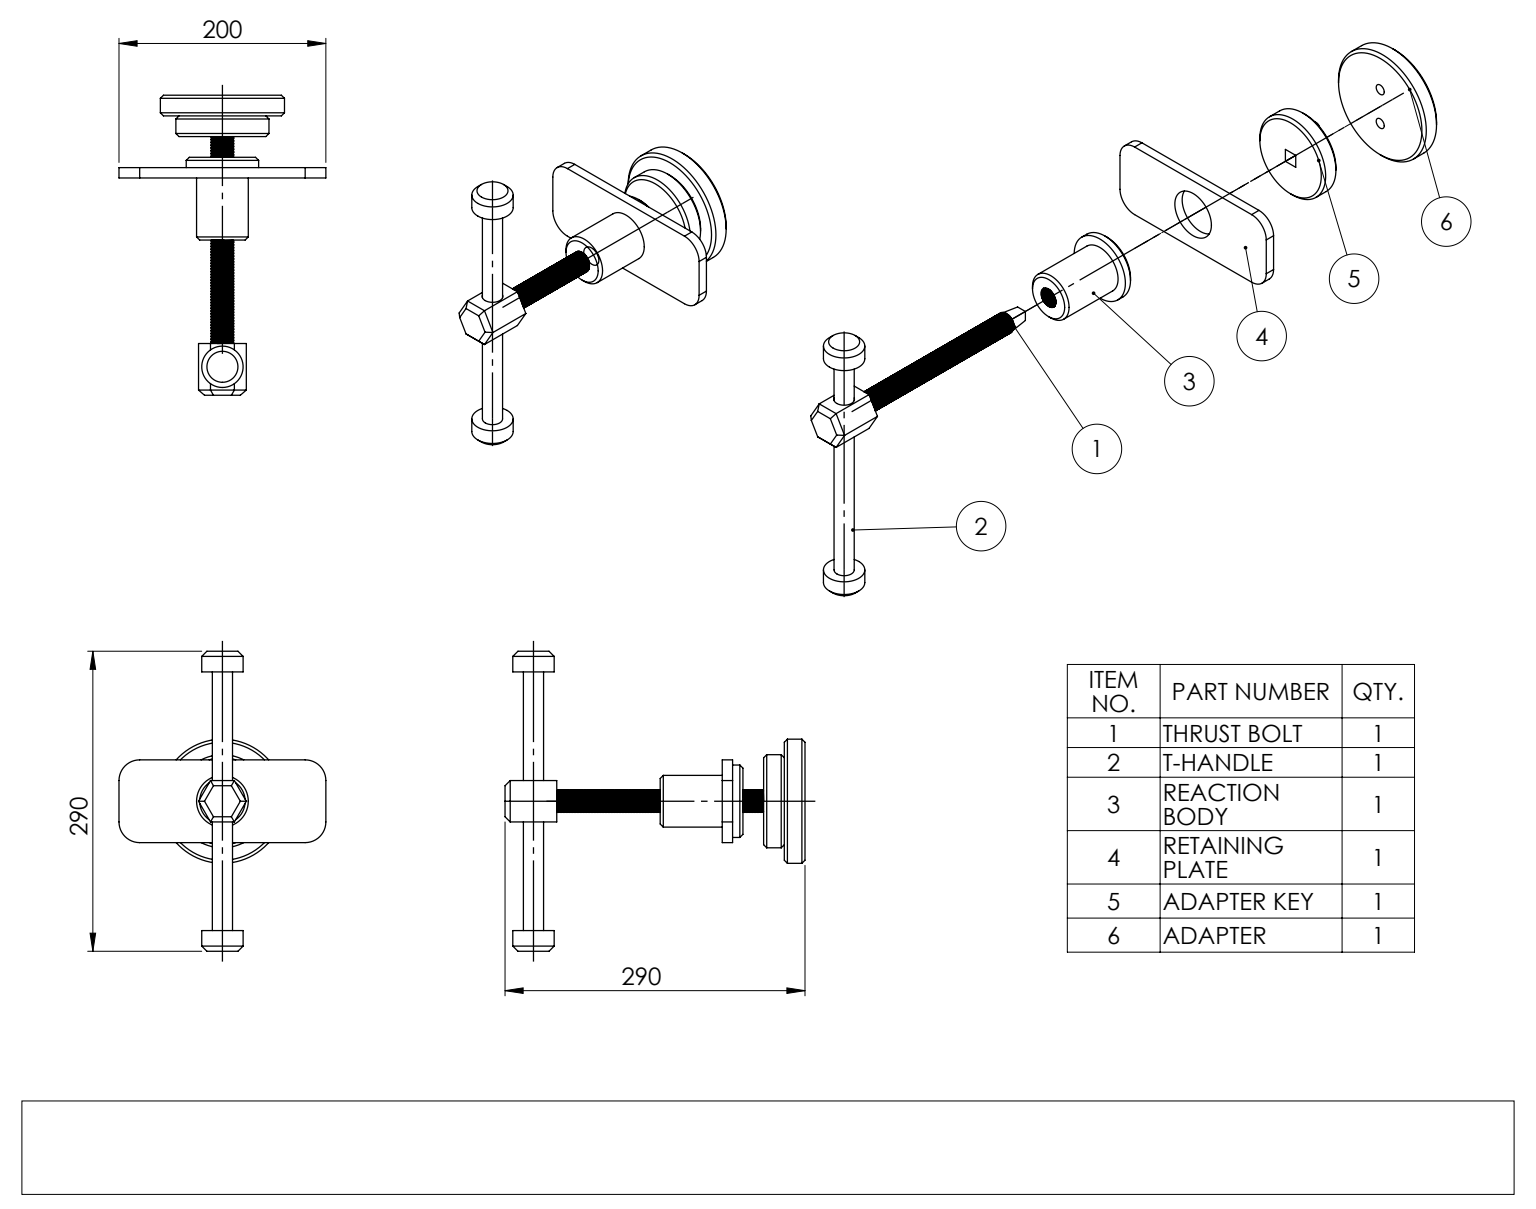
ISO-10303-21;
HEADER;
FILE_DESCRIPTION (('STEP AP203'),
    '1' );
FILE_NAME ('BR-597',
    '2026-09-28T05:57:06',
    ( '' ),
    ( '' ),
    'SwSTEP 2.0',
    'SolidWorks 2026',
    '' );
FILE_SCHEMA (( 'AUTOMOTIVE_DESIGN' ));
ENDSEC;

DATA;
#1 = ORIENTED_EDGE ( 'NONE', *, *, #11918, .T. ) ;
#2 = CARTESIAN_POINT ( 'NONE',  ( 10.81189881249999551, -6.242252689847874514, -42.15625000204836681 ) ) ;
#3 = CALENDAR_DATE ( 2026, 28, 9 ) ;
#4 = CARTESIAN_POINT ( 'NONE',  ( -10.81189881249999729, 1.324075727343319199E-15, -105.5937500020483810 ) ) ;
#5 = CARTESIAN_POINT ( 'NONE',  ( 10.81189881249999729, 6.242252689847867408, -121.4062500020483810 ) ) ;
#6 = VERTEX_POINT ( 'NONE', #18708 ) ;
#7 = DIRECTION ( 'NONE',  ( -0.000000000000000000, -0.000000000000000000, -1.000000000000000000 ) ) ;
#8 = CARTESIAN_POINT ( 'NONE',  ( -5.405949406249996869, 9.363379034771805109, -182.5312500020484094 ) ) ;
#9 = CARTESIAN_POINT ( 'NONE',  ( -5.000000000000003553, -8.660254037844383745, -26.49999999999996803 ) ) ;
#10 = DIRECTION ( 'NONE',  ( 0.000000000000000000, 0.000000000000000000, -1.000000000000000000 ) ) ;
#11 = AXIS2_PLACEMENT_3D ( 'NONE', #22333, #25786, #11966 ) ;
#12 = CARTESIAN_POINT ( 'NONE',  ( -2.293366432827344421E-15, -12.48450537969573659, -130.7187500020483810 ) ) ;
#13 = CARTESIAN_POINT ( 'NONE',  ( 10.81189881249999729, 0.000000000000000000, -100.3437500020483810 ) ) ;
#14 = CARTESIAN_POINT ( 'NONE',  ( -9.999999999999998224, 1.224646799147353059E-15, -200.0000000000000000 ) ) ;
#15 = CARTESIAN_POINT ( 'NONE',  ( 10.81189881249999551, -6.242252689847874514, -106.6562500020483952 ) ) ;
#16 = CARTESIAN_POINT ( 'NONE',  ( 5.000000000000000000, 8.660254037844385522, -194.1250000040967905 ) ) ;
#17 = CARTESIAN_POINT ( 'NONE',  ( -10.81189881249999729, 6.242252689847871849, -113.2187500020483810 ) ) ;
#18 = CARTESIAN_POINT ( 'NONE',  ( -2.293366432827344421E-15, -12.48450537969573659, -186.4062500020484094 ) ) ;
#19 = CARTESIAN_POINT ( 'NONE',  ( 9.999999999999998224, 0.000000000000000000, -46.99999999999998579 ) ) ;
#20 = CYLINDRICAL_SURFACE ( 'NONE', #32104, 9.999999999999998224 ) ;
#21 = CARTESIAN_POINT ( 'NONE',  ( 5.000000000000000000, 8.660254037844385522, -142.7500000000000000 ) ) ;
#22 = CARTESIAN_POINT ( 'NONE',  ( 4.999999999999992006, -8.660254037844389075, -2.249999999999974243 ) ) ;
#23 = CARTESIAN_POINT ( 'NONE',  ( 5.405949406249999534, 9.363379034771803333, -58.09375000204835970 ) ) ;
#24 = CARTESIAN_POINT ( 'NONE',  ( 7.644554776091147741E-16, 12.48450537969573659, -50.46875000204835970 ) ) ;
#25 = CARTESIAN_POINT ( 'NONE',  ( -9.999999999999998224, 5.773502691896259087, -178.7500000040967905 ) ) ;
#26 = CARTESIAN_POINT ( 'NONE',  ( 10.81189881249999551, -6.242252689847874514, -15.15625000204837036 ) ) ;
#27 = CARTESIAN_POINT ( 'NONE',  ( 10.81189881249999551, -6.242252689847874514, -29.96875000204834905 ) ) ;
#28 = CARTESIAN_POINT ( 'NONE',  ( 5.000000000000000000, 8.660254037844385522, -117.2500000000000000 ) ) ;
#29 = CARTESIAN_POINT ( 'NONE',  ( 5.405949406249992428, -9.363379034771808662, -141.0937500020483810 ) ) ;
#30 = CARTESIAN_POINT ( 'NONE',  ( 7.070501591499377789E-16, 11.54700538379251284, -105.1249999999999858 ) ) ;
#31 = CARTESIAN_POINT ( 'NONE',  ( -2.293366432827344421E-15, -12.48450537969573659, -37.90625000204836681 ) ) ;
#32 =( BOUNDED_CURVE ( )  B_SPLINE_CURVE ( 2, ( #493, #39950, #13606, #30683, #37364, #10382, #33502 ),
 .UNSPECIFIED., .F., .F. ) 
 B_SPLINE_CURVE_WITH_KNOTS ( ( 3, 2, 2, 3 ),
 ( 0.2462686567164180107, 0.2475124378109453960, 0.2487562189054727535, 0.2500000000000001110 ),
 .UNSPECIFIED. ) 
 CURVE ( )  GEOMETRIC_REPRESENTATION_ITEM ( )  RATIONAL_B_SPLINE_CURVE ( ( 0.9999999999999880096, 0.8660254037844506980, 1.000000000000000000, 0.8660254037844387076, 1.000000000000000000, 0.8660254037844267172, 1.000000000000011990 ) ) 
 REPRESENTATION_ITEM ( '' )  );
#33 = CARTESIAN_POINT ( 'NONE',  ( -5.000000000000003553, -8.660254037844383745, -27.99999999999996803 ) ) ;
#34 = CARTESIAN_POINT ( 'NONE',  ( 10.00000000000000000, 5.773502691896255534, -67.87500000000000000 ) ) ;
#35 = CARTESIAN_POINT ( 'NONE',  ( 10.81189881249999729, 0.000000000000000000, -133.5312500020484094 ) ) ;
#36 = CARTESIAN_POINT ( 'NONE',  ( 10.81189881249999729, 6.242252689847867408, -113.9062500020483952 ) ) ;
#37 = ORIENTED_EDGE ( 'NONE', *, *, #14781, .T. ) ;
#38 = CARTESIAN_POINT ( 'NONE',  ( -5.000000000000003553, -8.660254037844383745, -128.5000000000000000 ) ) ;
#39 = CARTESIAN_POINT ( 'NONE',  ( 10.00000000000000000, 5.773502691896255534, -105.7500000040967905 ) ) ;
#40 = DIRECTION ( 'NONE',  ( -0.000000000000000000, -0.000000000000000000, 1.000000000000000000 ) ) ;
#41 = CARTESIAN_POINT ( 'NONE',  ( -5.405949406250003975, -9.363379034771801557, -67.84375000204836681 ) ) ;
#42 = ORIENTED_EDGE ( 'NONE', *, *, #41503, .T. ) ;
#43 = CARTESIAN_POINT ( 'NONE',  ( 5.000000000000000000, 8.660254037844385522, -30.24999999999997158 ) ) ;
#44 = CARTESIAN_POINT ( 'NONE',  ( 5.000000000000000000, 8.660254037844385522, -18.62500000409675494 ) ) ;
#45 = CARTESIAN_POINT ( 'NONE',  ( -10.81189881249999729, 6.242252689847871849, -45.90625000204838102 ) ) ;
#46 = CARTESIAN_POINT ( 'NONE',  ( 5.000000000000000000, 8.660254037844385522, -111.6250000040967763 ) ) ;
#47 = CARTESIAN_POINT ( 'NONE',  ( 4.999999999999992006, -8.660254037844389075, -37.12500000409676915 ) ) ;
#48 = CARTESIAN_POINT ( 'NONE',  ( 0.000000000000000000, 0.000000000000000000, -200.0000000000000000 ) ) ;
#49 = CARTESIAN_POINT ( 'NONE',  ( -5.405949406250003975, -9.363379034771801557, -140.0312500020484094 ) ) ;
#50 = CARTESIAN_POINT ( 'NONE',  ( -5.405949406250003975, -9.363379034771801557, -140.0312500020484094 ) ) ;
#51 = CARTESIAN_POINT ( 'NONE',  ( -2.121150477449813534E-15, -11.54700538379251284, -123.8749999999999858 ) ) ;
#52 = EDGE_LOOP ( 'NONE', ( #2862, #11579, #9941, #38309 ) ) ;
#53 = ORIENTED_EDGE ( 'NONE', *, *, #4042, .F. ) ;
#54 = ADVANCED_FACE ( 'NONE', ( #19135 ), #5555, .T. ) ;
#55 = EDGE_LOOP ( 'NONE', ( #10881, #42328, #28621, #40784 ) ) ;
#56 = EDGE_CURVE ( 'NONE', #16041, #19819, #26737, .T. ) ;
#57 = DIRECTION ( 'NONE',  ( -0.000000000000000000, -0.000000000000000000, 1.000000000000000000 ) ) ;
#58 = CARTESIAN_POINT ( 'NONE',  ( -2.293366432827344421E-15, -12.48450537969573659, -177.2187500020484094 ) ) ;
#59 = CARTESIAN_POINT ( 'NONE',  ( -10.81189881249999729, 1.324075727343319199E-15, -23.09375000204835615 ) ) ;
#60 = CARTESIAN_POINT ( 'NONE',  ( -5.000000000000003553, -8.660254037844383745, -128.8750000040967905 ) ) ;
#61 = CARTESIAN_POINT ( 'NONE',  ( 5.405949406249992428, -9.363379034771808662, -157.5937500020483810 ) ) ;
#62 = CARTESIAN_POINT ( 'NONE',  ( 5.405949406249999534, 9.363379034771803333, -146.5937500020483810 ) ) ;
#63 = CARTESIAN_POINT ( 'NONE',  ( 9.999999999999998224, 0.000000000000000000, -173.3750000040968189 ) ) ;
#64 = CARTESIAN_POINT ( 'NONE',  ( -2.293366432827344421E-15, -12.48450537969573659, -127.7187500020483668 ) ) ;
#65 = CARTESIAN_POINT ( 'NONE',  ( -5.405949406249996869, 9.363379034771805109, -136.0312500020484094 ) ) ;
#66 = CARTESIAN_POINT ( 'NONE',  ( 5.405949406249999534, 9.363379034771803333, -16.09375000204835260 ) ) ;
#67 = CARTESIAN_POINT ( 'NONE',  ( -10.81189881249999729, -6.242252689847864744, -138.4687500020483810 ) ) ;
#68 = CARTESIAN_POINT ( 'NONE',  ( 9.877642915644548438, -4.410630136379726451, -179.9999999999999716 ) ) ;
#69 =( BOUNDED_CURVE ( )  B_SPLINE_CURVE ( 2, ( #4574, #21398, #14476, #34370, #4786, #36947, #20536 ),
 .UNSPECIFIED., .F., .F. ) 
 B_SPLINE_CURVE_WITH_KNOTS ( ( 3, 2, 2, 3 ),
 ( 0.1455223880597014963, 0.1467661691542288538, 0.1480099502487562391, 0.1492537313432835966 ),
 .UNSPECIFIED. ) 
 CURVE ( )  GEOMETRIC_REPRESENTATION_ITEM ( )  RATIONAL_B_SPLINE_CURVE ( ( 1.000000000000000000, 0.8660254037844387076, 1.000000000000000000, 0.8660254037844387076, 1.000000000000000000, 0.8660254037844357100, 1.000000000000003109 ) ) 
 REPRESENTATION_ITEM ( '' )  );
#70 = CARTESIAN_POINT ( 'NONE',  ( 10.00000000000051159, -5.773502691895965988, -102.6249999999999858 ) ) ;
#71 = CARTESIAN_POINT ( 'NONE',  ( 7.070501591499377789E-16, 11.54700538379251284, -165.1249999999999716 ) ) ;
#72 = CARTESIAN_POINT ( 'NONE',  ( -2.121150477449813534E-15, -11.54700538379251284, -17.37499999999997158 ) ) ;
#73 = CARTESIAN_POINT ( 'NONE',  ( -5.405949406249996869, 9.363379034771805109, -72.84375000204838102 ) ) ;
#74 = CARTESIAN_POINT ( 'NONE',  ( -5.405949406250003975, -9.363379034771801557, -39.53125000204838102 ) ) ;
#75 = CARTESIAN_POINT ( 'NONE',  ( 10.81189881249999551, -6.242252689847874514, -53.96875000204837391 ) ) ;
#76 = CARTESIAN_POINT ( 'NONE',  ( -2.121150477449813534E-15, -11.54700538379251284, -16.25000000409675849 ) ) ;
#77 = CARTESIAN_POINT ( 'NONE',  ( -2.293366432827344421E-15, -12.48450537969573659, -159.2187500020483810 ) ) ;
#78 = VECTOR ( 'NONE', #7244, 1000.000000000000000 ) ;
#79 = CARTESIAN_POINT ( 'NONE',  ( -5.000000000000003553, -8.660254037844383745, -130.0000000000000000 ) ) ;
#80 = CARTESIAN_POINT ( 'NONE',  ( 7.644554776091147741E-16, 12.48450537969573659, -137.6562500020484094 ) ) ;
#81 = CARTESIAN_POINT ( 'NONE',  ( 0.000000000000000000, 0.000000000000000000, -99.99999999999998579 ) ) ;
#82 = CARTESIAN_POINT ( 'NONE',  ( -4.999999999999996447, 8.660254037844387298, -112.8750000040967763 ) ) ;
#83 = CARTESIAN_POINT ( 'NONE',  ( 7.070501591499377789E-16, 11.54700538379251284, -90.12499999999997158 ) ) ;
#84 = ORIENTED_EDGE ( 'NONE', *, *, #34120, .T. ) ;
#85 =( BOUNDED_CURVE ( )  B_SPLINE_CURVE ( 2, ( #33505, #9757, #39954, #703, #26171, #36305, #278 ),
 .UNSPECIFIED., .F., .F. ) 
 B_SPLINE_CURVE_WITH_KNOTS ( ( 3, 2, 2, 3 ),
 ( 0.9440298507462689948, 0.9452736318407963800, 0.9465174129353237653, 0.9477611940298510396 ),
 .UNSPECIFIED. ) 
 CURVE ( )  GEOMETRIC_REPRESENTATION_ITEM ( )  RATIONAL_B_SPLINE_CURVE ( ( 0.9999999999999641398, 0.8660254037844745678, 1.000000000000000000, 0.8660254037844387076, 1.000000000000000000, 0.8660254037844028474, 1.000000000000035971 ) ) 
 REPRESENTATION_ITEM ( '' )  );
#86 = CARTESIAN_POINT ( 'NONE',  ( 5.405949406249992428, -9.363379034771808662, -112.7812500020483952 ) ) ;
#87 = CARTESIAN_POINT ( 'NONE',  ( 9.999999999999998224, 0.000000000000000000, -129.8750000040967905 ) ) ;
#88 = DIRECTION ( 'NONE',  ( -0.000000000000000000, -0.000000000000000000, -1.000000000000000000 ) ) ;
#89 = CARTESIAN_POINT ( 'NONE',  ( -10.81189881249999729, 1.324075727343319199E-15, -171.7812500020484094 ) ) ;
#90 = CARTESIAN_POINT ( 'NONE',  ( 5.000000000000000000, 8.660254037844385522, -42.62500000409677625 ) ) ;
#91 = CARTESIAN_POINT ( 'NONE',  ( -1.040834085586084257E-14, -125.0000000000000000, 12.74999999999998934 ) ) ;
#92 = CARTESIAN_POINT ( 'NONE',  ( -10.81189881249999729, 6.242252689847871849, -62.40625000204838813 ) ) ;
#93 = CARTESIAN_POINT ( 'NONE',  ( 7.070501591499376803E-16, 11.54700538379251284, -101.0000000040967905 ) ) ;
#94 = CARTESIAN_POINT ( 'NONE',  ( -10.81189881249999729, 1.324075727343319199E-15, -164.2812500020484094 ) ) ;
#95 = CARTESIAN_POINT ( 'NONE',  ( 5.405949406249999534, 9.363379034771803333, -134.5937500020483810 ) ) ;
#96 = DIRECTION ( 'NONE',  ( -0.000000000000000000, -0.000000000000000000, 1.000000000000000000 ) ) ;
#97 = CARTESIAN_POINT ( 'NONE',  ( -9.999999999999998224, 1.224646799147353059E-15, -196.2500000000000000 ) ) ;
#98 = ORIENTED_EDGE ( 'NONE', *, *, #19816, .T. ) ;
#99 = DIRECTION ( 'NONE',  ( -0.000000000000000000, -0.000000000000000000, -1.000000000000000000 ) ) ;
#100 = VECTOR ( 'NONE', #1628, 1000.000000000000000 ) ;
#101 = LOCAL_TIME ( 11, 57, 6.000000000000000000, #23512 ) ;
#103 = ORIENTED_EDGE ( 'NONE', *, *, #9830, .F. ) ;
#102 = CARTESIAN_POINT ( 'NONE',  ( 5.405949406249999534, 9.363379034771803333, -70.28125000204838102 ) ) ;
#104 =( NAMED_UNIT ( * ) PLANE_ANGLE_UNIT ( ) SI_UNIT ( $, .RADIAN. ) );
#105 = EDGE_CURVE ( 'NONE', #39394, #30784, #41849, .T. ) ;
#107 = VERTEX_POINT ( 'NONE', #25626 ) ;
#106 = CARTESIAN_POINT ( 'NONE',  ( -2.293366432827344421E-15, -12.48450537969573659, -121.7187500020483952 ) ) ;
#108 = ORIENTED_EDGE ( 'NONE', *, *, #20529, .T. ) ;
#109 = EDGE_CURVE ( 'NONE', #35866, #23028, #3547, .T. ) ;
#110 = CARTESIAN_POINT ( 'NONE',  ( 10.81189881249999551, -6.242252689847874514, -23.96875000204836681 ) ) ;
#111 = CARTESIAN_POINT ( 'NONE',  ( 10.81189881249999551, -6.242252689847874514, -197.9687500020484094 ) ) ;
#112 = AXIS2_PLACEMENT_3D ( 'NONE', #13766, #17434, #17222 ) ;
#114 = ADVANCED_FACE ( 'NONE', ( #26883 ), #29920, .T. ) ;
#113 = CARTESIAN_POINT ( 'NONE',  ( 10.81189881249999907, 6.242252689847868297, -50.71875000204835970 ) ) ;
#115 = FACE_OUTER_BOUND ( 'NONE', #1522, .T. ) ;
#116 = CARTESIAN_POINT ( 'NONE',  ( -9.999999999999998224, 1.224646799147353059E-15, -26.74999999999996803 ) ) ;
#117 = CARTESIAN_POINT ( 'NONE',  ( -5.405949406249996869, 9.363379034771805109, -182.3437500020483810 ) ) ;
#118 = CARTESIAN_POINT ( 'NONE',  ( 10.81189881249999729, 0.000000000000000000, -166.3437500020484094 ) ) ;
#119 = CC_DESIGN_PERSON_AND_ORGANIZATION_ASSIGNMENT ( #41852, #12290, ( #9061 ) ) ;
#120 = CARTESIAN_POINT ( 'NONE',  ( -10.81189881249999907, -6.242252689847864744, -147.4687500020484094 ) ) ;
#121 = CARTESIAN_POINT ( 'NONE',  ( -5.405949406249996869, 9.363379034771805109, -162.8437500020484094 ) ) ;
#122 = DIRECTION ( 'NONE',  ( -1.000000000000000000, 0.000000000000000000, 0.000000000000000000 ) ) ;
#123 = FACE_OUTER_BOUND ( 'NONE', #11010, .T. ) ;
#124 = CARTESIAN_POINT ( 'NONE',  ( -9.999999999999998224, 1.224646799147353059E-15, -188.7500000000000000 ) ) ;
#125 = CARTESIAN_POINT ( 'NONE',  ( 5.405949406249992428, -9.363379034771808662, -99.09375000204838102 ) ) ;
#126 = FACE_OUTER_BOUND ( 'NONE', #13645, .T. ) ;
#127 = CARTESIAN_POINT ( 'NONE',  ( -5.405949406250003975, -9.363379034771801557, -63.53125000204837391 ) ) ;
#128 = CARTESIAN_POINT ( 'NONE',  ( 10.81189881249999907, 6.242252689847868297, -184.2187500020483810 ) ) ;
#129 = CARTESIAN_POINT ( 'NONE',  ( 7.644554776091147741E-16, 12.48450537969573659, -164.6562500020484094 ) ) ;
#130 = CARTESIAN_POINT ( 'NONE',  ( 5.405949406249992428, -9.363379034771808662, -51.28125000204835970 ) ) ;
#131 = CARTESIAN_POINT ( 'NONE',  ( -9.999999999999998224, 1.224646799147353059E-15, -136.6250000040967620 ) ) ;
#132 = CARTESIAN_POINT ( 'NONE',  ( -9.999999999999998224, 1.224646799147353059E-15, -118.2500000000000000 ) ) ;
#133 = AXIS2_PLACEMENT_3D ( 'NONE', #27318, #14555, #30777 ) ;
#134 = VERTEX_POINT ( 'NONE', #10468 ) ;
#135 = CARTESIAN_POINT ( 'NONE',  ( -5.405949406249996869, 9.363379034771805109, -142.0312500020483810 ) ) ;
#136 = CARTESIAN_POINT ( 'NONE',  ( -10.81189881249999729, 6.242252689847871849, -152.4062500020483810 ) ) ;
#137 = ADVANCED_FACE ( 'NONE', ( #29707 ), #23658, .T. ) ;
#138 = SECURITY_CLASSIFICATION ( '', '', #9442 ) ;
#139 = CARTESIAN_POINT ( 'NONE',  ( -10.81189881249999729, 1.324075727343319199E-15, -195.7812500020484094 ) ) ;
#140 = LINE ( 'NONE', #33368, #22679 ) ;
#141 = CARTESIAN_POINT ( 'NONE',  ( -5.405949406249996869, 9.363379034771805109, -90.84375000204838102 ) ) ;
#142 = ORIENTED_EDGE ( 'NONE', *, *, #37948, .T. ) ;
#143 = CARTESIAN_POINT ( 'NONE',  ( -4.999999999999996447, 8.660254037844387298, -58.49999999999997158 ) ) ;
#144 = CARTESIAN_POINT ( 'NONE',  ( -10.81189881249999729, 1.324075727343319199E-15, -186.5937500020483810 ) ) ;
#145 = CARTESIAN_POINT ( 'NONE',  ( -5.000000000000003553, -8.660254037844383745, -62.87500000409676204 ) ) ;
#146 = CARTESIAN_POINT ( 'NONE',  ( 7.070501591499376803E-16, 11.54700538379251284, -102.1250000000000000 ) ) ;
#147 = CARTESIAN_POINT ( 'NONE',  ( 9.999999999999998224, 0.000000000000000000, -144.5000000000000000 ) ) ;
#148 = CARTESIAN_POINT ( 'NONE',  ( 10.81189881249999551, -6.242252689847874514, -81.15625000204839523 ) ) ;
#149 = CARTESIAN_POINT ( 'NONE',  ( -10.81189881249999729, -6.242252689847864744, -62.15625000204838813 ) ) ;
#150 = CARTESIAN_POINT ( 'NONE',  ( 5.000000000000000000, 8.660254037844385522, -57.62500000409676204 ) ) ;
#151 = CARTESIAN_POINT ( 'NONE',  ( -10.81189881249999729, 6.242252689847871849, -17.21875000204836681 ) ) ;
#152 = CARTESIAN_POINT ( 'NONE',  ( 9.999999999999998224, 0.000000000000000000, -200.0000000000000000 ) ) ;
#153 = CARTESIAN_POINT ( 'NONE',  ( -10.81189881249999907, -6.242252689847864744, -188.1562500020484094 ) ) ;
#154 = CARTESIAN_POINT ( 'NONE',  ( -10.81189881249999729, 6.242252689847871849, -11.40625000204836859 ) ) ;
#155 = CARTESIAN_POINT ( 'NONE',  ( 7.644554776091147741E-16, 12.48450537969573659, -0.9687500020483524876 ) ) ;
#156 = DIRECTION ( 'NONE',  ( -0.000000000000000000, -0.000000000000000000, -1.000000000000000000 ) ) ;
#157 =( BOUNDED_CURVE ( )  B_SPLINE_CURVE ( 2, ( #19226, #13579, #9933, #13155, #20069, #32416, #9303 ),
 .UNSPECIFIED., .F., .F. ) 
 B_SPLINE_CURVE_WITH_KNOTS ( ( 3, 2, 2, 3 ),
 ( 0.3955223880597015795, 0.3967661691542289648, 0.3980099502487563501, 0.3992537313432836799 ),
 .UNSPECIFIED. ) 
 CURVE ( )  GEOMETRIC_REPRESENTATION_ITEM ( )  RATIONAL_B_SPLINE_CURVE ( ( 0.9999999999999880096, 0.8660254037844506980, 1.000000000000000000, 0.8660254037844387076, 1.000000000000000000, 0.8660254037844267172, 1.000000000000011990 ) ) 
 REPRESENTATION_ITEM ( '' )  );
#158 = CARTESIAN_POINT ( 'NONE',  ( 9.999999999999998224, 1.224646799147353059E-15, -99.99999999999998579 ) ) ;
#159 = DIRECTION ( 'NONE',  ( -1.000000000000000000, 0.000000000000000000, 0.000000000000000000 ) ) ;
#160 = CARTESIAN_POINT ( 'NONE',  ( -10.00000000000000000, -5.773502691896251982, -167.6249999999999716 ) ) ;
#161 = CARTESIAN_POINT ( 'NONE',  ( 0.000000000000000000, 0.000000000000000000, -99.99999999999998579 ) ) ;
#163 = ORIENTED_EDGE ( 'NONE', *, *, #36914, .F. ) ;
#162 = CARTESIAN_POINT ( 'NONE',  ( -2.293366432827344421E-15, -12.48450537969573659, -94.90625000204838102 ) ) ;
#164 = CYLINDRICAL_SURFACE ( 'NONE', #41388, 9.999999999999998224 ) ;
#166 = ORIENTED_EDGE ( 'NONE', *, *, #11173, .F. ) ;
#165 = CARTESIAN_POINT ( 'NONE',  ( 10.81189881249999729, 6.242252689847867408, -101.7187500020483810 ) ) ;
#167 = ORIENTED_EDGE ( 'NONE', *, *, #19593, .F. ) ;
#168 = AXIS2_PLACEMENT_3D ( 'NONE', #1708, #40738, #1276 ) ;
#169 = CARTESIAN_POINT ( 'NONE',  ( 10.81189881249999729, 0.000000000000000000, -31.34375000204836681 ) ) ;
#170 = CARTESIAN_POINT ( 'NONE',  ( 10.81189881249999551, -6.242252689847874514, -22.65625000204837391 ) ) ;
#171 = CALENDAR_DATE ( 2026, 28, 9 ) ;
#172 = CARTESIAN_POINT ( 'NONE',  ( 5.405949406249999534, 9.363379034771803333, -71.59375000204836681 ) ) ;
#173 = CARTESIAN_POINT ( 'NONE',  ( 0.000000000000000000, 0.000000000000000000, -200.0000000000000000 ) ) ;
#174 = CARTESIAN_POINT ( 'NONE',  ( 5.405949406249992428, -9.363379034771808662, -192.0937500020484094 ) ) ;
#175 = CARTESIAN_POINT ( 'NONE',  ( -2.293366432827344421E-15, -12.48450537969573659, -150.2187500020483810 ) ) ;
#176 = CARTESIAN_POINT ( 'NONE',  ( 5.000000000000000000, 8.660254037844385522, -99.24999999999998579 ) ) ;
#177 = LINE ( 'NONE', #29948, #5403 ) ;
#178 = CARTESIAN_POINT ( 'NONE',  ( 5.405949406249999534, 9.363379034771803333, -149.7812500020483810 ) ) ;
#179 = CARTESIAN_POINT ( 'NONE',  ( -10.00000000000000000, -5.773502691896251982, -4.096743805827756695E-09 ) ) ;
#180 = VECTOR ( 'NONE', #38036, 1000.000000000000000 ) ;
#181 = CARTESIAN_POINT ( 'NONE',  ( -10.00000000000154188, 5.773502691895366468, -49.75000000409671230 ) ) ;
#182 = ADVANCED_FACE ( 'NONE', ( #33380 ), #3374, .T. ) ;
#183 = CARTESIAN_POINT ( 'NONE',  ( -10.81189881249999907, -6.242252689847864744, -123.4687500020483810 ) ) ;
#184 = DIRECTION ( 'NONE',  ( -0.000000000000000000, -0.000000000000000000, 1.000000000000000000 ) ) ;
#185 = CARTESIAN_POINT ( 'NONE',  ( 5.405949406249999534, 9.363379034771803333, -91.28125000204838102 ) ) ;
#186 = CARTESIAN_POINT ( 'NONE',  ( 5.405949406249999534, 9.363379034771803333, -106.0937500020483810 ) ) ;
#187 = CARTESIAN_POINT ( 'NONE',  ( 5.405949406249999534, 9.363379034771803333, -74.59375000204838102 ) ) ;
#188 = CARTESIAN_POINT ( 'NONE',  ( -10.81189881249999729, 1.324075727343319199E-15, -83.28125000204838102 ) ) ;
#189 = CARTESIAN_POINT ( 'NONE',  ( 10.00000000000000000, 5.773502691896255534, -161.2500000040967905 ) ) ;
#190 = CARTESIAN_POINT ( 'NONE',  ( -10.81189881249999729, -6.242252689847864744, -162.6562500020483810 ) ) ;
#191 = CARTESIAN_POINT ( 'NONE',  ( -5.405949406249996869, 9.363379034771805109, -181.0312500020483810 ) ) ;
#192 = CARTESIAN_POINT ( 'NONE',  ( -4.999999999999996447, 8.660254037844387298, -159.3750000040967905 ) ) ;
#193 = DIRECTION ( 'NONE',  ( -1.000000000000000000, 0.000000000000000000, 0.000000000000000000 ) ) ;
#194 = CARTESIAN_POINT ( 'NONE',  ( -5.405949406250003975, -9.363379034771801557, -9.343750002048345493 ) ) ;
#195 = FACE_OUTER_BOUND ( 'NONE', #14094, .T. ) ;
#196 = CARTESIAN_POINT ( 'NONE',  ( -10.81189881249999729, 1.324075727343319199E-15, -113.0937500020483810 ) ) ;
#197 = CARTESIAN_POINT ( 'NONE',  ( 10.00000000000000000, 5.773502691896255534, -81.37499999999998579 ) ) ;
#198 = CARTESIAN_POINT ( 'NONE',  ( 10.81189881249999729, 0.000000000000000000, -13.53125000204835615 ) ) ;
#199 = CARTESIAN_POINT ( 'NONE',  ( -9.999999999999998224, 5.773502691896259087, -91.75000000409677625 ) ) ;
#200 = CYLINDRICAL_SURFACE ( 'NONE', #38257, 25.00000000000000000 ) ;
#201 = CARTESIAN_POINT ( 'NONE',  ( 5.405949406249999534, 9.363379034771803333, -112.2812500020483952 ) ) ;
#202 = CARTESIAN_POINT ( 'NONE',  ( -2.293366432827344421E-15, -12.48450537969573659, -84.40625000204838102 ) ) ;
#203 = ORIENTED_EDGE ( 'NONE', *, *, #41316, .F. ) ;
#204 =( BOUNDED_CURVE ( )  B_SPLINE_CURVE ( 2, ( #13200, #12782, #19064, #9770, #9143, #32665, #29001 ),
 .UNSPECIFIED., .F., .F. ) 
 B_SPLINE_CURVE_WITH_KNOTS ( ( 3, 2, 2, 3 ),
 ( 0.5373134328358210032, 0.5385572139303483885, 0.5398009950248757738, 0.5410447761194030480 ),
 .UNSPECIFIED. ) 
 CURVE ( )  GEOMETRIC_REPRESENTATION_ITEM ( )  RATIONAL_B_SPLINE_CURVE ( ( 0.9999999999999880096, 0.8660254037844506980, 1.000000000000000000, 0.8660254037844387076, 1.000000000000000000, 0.8660254037844267172, 1.000000000000011990 ) ) 
 REPRESENTATION_ITEM ( '' )  );
#205 = CARTESIAN_POINT ( 'NONE',  ( 9.999999999999996447, -5.773502691896262640, -83.50000000409676204 ) ) ;
#206 = CARTESIAN_POINT ( 'NONE',  ( 9.999999999999742428, 5.773502691896404748, -134.2500000040967905 ) ) ;
#207 = CARTESIAN_POINT ( 'NONE',  ( -10.81189881249999729, 1.324075727343319199E-15, -44.09375000204837391 ) ) ;
#208 = ORIENTED_EDGE ( 'NONE', *, *, #27661, .F. ) ;
#209 = CARTESIAN_POINT ( 'NONE',  ( 5.000000000000000000, 8.660254037844385522, -7.749999999999978684 ) ) ;
#210 = CARTESIAN_POINT ( 'NONE',  ( -5.000000000000003553, -8.660254037844383745, -142.0000000000000000 ) ) ;
#211 = CARTESIAN_POINT ( 'NONE',  ( -9.999999999999998224, 1.224646799147353059E-15, -200.0000000000000000 ) ) ;
#212 = CARTESIAN_POINT ( 'NONE',  ( 9.999999999999996447, -5.773502691896262640, -10.00000000409676026 ) ) ;
#213 = VECTOR ( 'NONE', #33847, 1000.000000000000000 ) ;
#214 = CARTESIAN_POINT ( 'NONE',  ( 10.00000000000000000, 5.773502691896255534, -189.3750000000000000 ) ) ;
#215 = CARTESIAN_POINT ( 'NONE',  ( 9.999999999999998224, 0.000000000000000000, -123.5000000000000000 ) ) ;
#217 = ORIENTED_EDGE ( 'NONE', *, *, #1701, .T. ) ;
#216 = CARTESIAN_POINT ( 'NONE',  ( 5.405949406249992428, -9.363379034771808662, -115.7812500020483952 ) ) ;
#218 = ORIENTED_EDGE ( 'NONE', *, *, #5122, .T. ) ;
#219 = CARTESIAN_POINT ( 'NONE',  ( -5.405949406249996869, 9.363379034771805109, -47.53125000204838813 ) ) ;
#220 = PERSON_AND_ORGANIZATION_ROLE ( 'design_owner' ) ;
#221 = CARTESIAN_POINT ( 'NONE',  ( -10.81189881249999907, -6.242252689847864744, -91.96875000204838102 ) ) ;
#222 = CARTESIAN_POINT ( 'NONE',  ( -10.81189881249999729, -6.242252689847864744, -120.6562500020483810 ) ) ;
#223 = VERTEX_POINT ( 'NONE', #23443 ) ;
#224 = CARTESIAN_POINT ( 'NONE',  ( -9.999999999999998224, 1.224646799147353059E-15, -112.2499999999999858 ) ) ;
#225 = CARTESIAN_POINT ( 'NONE',  ( 4.999999999999992006, -8.660254037844389075, -116.2499999999999858 ) ) ;
#226 = CARTESIAN_POINT ( 'NONE',  ( 10.81189881249999907, 6.242252689847868297, -182.9062500020484094 ) ) ;
#227 = DIRECTION ( 'NONE',  ( 0.000000000000000000, -0.000000000000000000, 1.000000000000000000 ) ) ;
#228 = CARTESIAN_POINT ( 'NONE',  ( -10.81189881249999729, 6.242252689847871849, -129.7187500020483810 ) ) ;
#229 = CARTESIAN_POINT ( 'NONE',  ( -5.405949406250003975, -9.363379034771801557, -102.3437500020483810 ) ) ;
#230 = CYLINDRICAL_SURFACE ( 'NONE', #27006, 9.999999999999998224 ) ;
#231 = CARTESIAN_POINT ( 'NONE',  ( 10.81189881249999729, 0.000000000000000000, -105.0312500020483810 ) ) ;
#232 = CARTESIAN_POINT ( 'NONE',  ( 5.000000000000000000, 8.660254037844385522, -189.6250000040967905 ) ) ;
#233 = CARTESIAN_POINT ( 'NONE',  ( -5.405949406250003975, -9.363379034771801557, -115.8437500020483810 ) ) ;
#234 = CARTESIAN_POINT ( 'NONE',  ( -2.293366432827344421E-15, -12.48450537969573659, -189.4062500020484094 ) ) ;
#235 = CARTESIAN_POINT ( 'NONE',  ( 0.000000000000000000, 0.000000000000000000, -170.0000000000000000 ) ) ;
#236 = CARTESIAN_POINT ( 'NONE',  ( 57.00000000000002132, 7.164183775012018789E-15, -220.0000000000000000 ) ) ;
#237 = CARTESIAN_POINT ( 'NONE',  ( -9.999999999999998224, 1.224646799147353059E-15, -134.7499999999999716 ) ) ;
#238 = CARTESIAN_POINT ( 'NONE',  ( -4.999999999999996447, 8.660254037844387298, -7.499999999999978684 ) ) ;
#239 = CARTESIAN_POINT ( 'NONE',  ( 5.405949406249999534, 9.363379034771803333, -64.09375000204836681 ) ) ;
#240 = CARTESIAN_POINT ( 'NONE',  ( 5.405949406249992428, -9.363379034771808662, -51.09375000204835260 ) ) ;
#241 = CARTESIAN_POINT ( 'NONE',  ( -10.00000000000000000, -5.773502691896251982, -181.5000000040967905 ) ) ;
#242 = CARTESIAN_POINT ( 'NONE',  ( 10.81189881249999729, 0.000000000000000000, -18.03125000204835970 ) ) ;
#243 = CARTESIAN_POINT ( 'NONE',  ( 5.405949406249999534, 9.363379034771803333, -31.09375000204836326 ) ) ;
#244 = CARTESIAN_POINT ( 'NONE',  ( -5.000000000000003553, -8.660254037844383745, -124.3750000040967763 ) ) ;
#245 = CARTESIAN_POINT ( 'NONE',  ( 10.81189881249999907, 6.242252689847868297, -134.7187500020484094 ) ) ;
#246 = CARTESIAN_POINT ( 'NONE',  ( 9.999999999999998224, 0.000000000000000000, -108.4999999999999858 ) ) ;
#247 = CARTESIAN_POINT ( 'NONE',  ( 10.81189881249999729, 0.000000000000000000, -40.53125000204838102 ) ) ;
#248 = FACE_OUTER_BOUND ( 'NONE', #19771, .T. ) ;
#249 = CARTESIAN_POINT ( 'NONE',  ( 9.999999999999996447, -5.773502691896262640, -63.62499999999999289 ) ) ;
#250 = CARTESIAN_POINT ( 'NONE',  ( 5.405949406249999534, 9.363379034771803333, -136.2812500020483810 ) ) ;
#251 = CARTESIAN_POINT ( 'NONE',  ( 5.405949406249999534, 9.363379034771803333, -112.2812500020483952 ) ) ;
#252 = EDGE_CURVE ( 'NONE', #311, #38192, #33161, .T. ) ;
#253 = ORIENTED_EDGE ( 'NONE', *, *, #28926, .T. ) ;
#254 = CARTESIAN_POINT ( 'NONE',  ( -10.00000000000051337, 5.773502691895962435, -142.3750000000000000 ) ) ;
#255 = CARTESIAN_POINT ( 'NONE',  ( -9.999999999999998224, 5.773502691896259087, -105.2500000040967763 ) ) ;
#256 = CARTESIAN_POINT ( 'NONE',  ( -2.121150477449813534E-15, -11.54700538379251284, -146.3749999999999716 ) ) ;
#257 = CARTESIAN_POINT ( 'NONE',  ( 10.81189881249999551, -6.242252689847874514, -67.46875000204838102 ) ) ;
#258 = VERTEX_POINT ( 'NONE', #36387 ) ;
#259 = CARTESIAN_POINT ( 'NONE',  ( -4.999999999999996447, 8.660254037844387298, -35.99999999999997868 ) ) ;
#260 = CARTESIAN_POINT ( 'NONE',  ( -5.000000000000003553, -8.660254037844383745, -20.87500000409675494 ) ) ;
#261 = CARTESIAN_POINT ( 'NONE',  ( -10.81189881249999729, 6.242252689847871849, -39.90625000204835970 ) ) ;
#262 = CARTESIAN_POINT ( 'NONE',  ( 9.999999999999998224, 0.000000000000000000, -35.37500000409676915 ) ) ;
#263 = CARTESIAN_POINT ( 'NONE',  ( -10.00000000000000000, -5.773502691896251982, -39.00000000409676204 ) ) ;
#264 = LINE ( 'NONE', #16194, #5231 ) ;
#265 = CARTESIAN_POINT ( 'NONE',  ( 5.405949406249992428, -9.363379034771808662, -145.7812500020483810 ) ) ;
#266 = CARTESIAN_POINT ( 'NONE',  ( -2.121150477449813534E-15, -11.54700538379251284, -110.3749999999999858 ) ) ;
#267 = EDGE_LOOP ( 'NONE', ( #11226, #4653, #4074, #29262 ) ) ;
#268 = ORIENTED_EDGE ( 'NONE', *, *, #28886, .F. ) ;
#269 = EDGE_CURVE ( 'NONE', #8961, #22977, #32528, .T. ) ;
#270 = VERTEX_POINT ( 'NONE', #36591 ) ;
#271 = DIRECTION ( 'NONE',  ( -0.000000000000000000, -0.000000000000000000, 1.000000000000000000 ) ) ;
#272 = CARTESIAN_POINT ( 'NONE',  ( 7.644554776091147741E-16, 12.48450537969573659, -170.4687500020483810 ) ) ;
#273 = CARTESIAN_POINT ( 'NONE',  ( -10.81189881249999907, -6.242252689847864744, -21.46875000204836681 ) ) ;
#274 = CARTESIAN_POINT ( 'NONE',  ( 9.999999999999227285, 5.773502691896701400, -111.7500000040967478 ) ) ;
#275 = CARTESIAN_POINT ( 'NONE',  ( -10.81189881249999729, 1.324075727343319199E-15, -153.5937500020483810 ) ) ;
#276 = CARTESIAN_POINT ( 'NONE',  ( 10.81189881249999907, 6.242252689847868297, -143.7187500020483810 ) ) ;
#277 =( BOUNDED_CURVE ( )  B_SPLINE_CURVE ( 2, ( #35244, #34601, #35030, #41688, #5459, #14928, #5032 ),
 .UNSPECIFIED., .F., .F. ) 
 B_SPLINE_CURVE_WITH_KNOTS ( ( 3, 2, 2, 3 ),
 ( 0.4962686567164180107, 0.4975124378109453960, 0.4987562189054727257, 0.5000000000000001110 ),
 .UNSPECIFIED. ) 
 CURVE ( )  GEOMETRIC_REPRESENTATION_ITEM ( )  RATIONAL_B_SPLINE_CURVE ( ( 0.9999999999999880096, 0.8660254037844506980, 1.000000000000000000, 0.8660254037844387076, 1.000000000000000000, 0.8660254037844267172, 1.000000000000011990 ) ) 
 REPRESENTATION_ITEM ( '' )  );
#278 = CARTESIAN_POINT ( 'NONE',  ( 9.999999999999998224, 0.000000000000000000, -8.375000004096744277 ) ) ;
#279 = CARTESIAN_POINT ( 'NONE',  ( -10.81189881249999729, 6.242252689847871849, -125.2187500020483810 ) ) ;
#280 = CARTESIAN_POINT ( 'NONE',  ( 7.644554776091147741E-16, 12.48450537969573659, -128.6562500020483810 ) ) ;
#281 = CARTESIAN_POINT ( 'NONE',  ( -10.81189881249999729, 6.242252689847871849, -6.718750002048347270 ) ) ;
#282 = CARTESIAN_POINT ( 'NONE',  ( 10.81189881249999551, -6.242252689847874514, -139.4687500020483810 ) ) ;
#283 = CARTESIAN_POINT ( 'NONE',  ( 10.64016988090102700, -2.046480638857292256, -180.0000000000000000 ) ) ;
#284 = CARTESIAN_POINT ( 'NONE',  ( 7.070501591499376803E-16, 11.54700538379251284, -120.1249999999999858 ) ) ;
#285 = CARTESIAN_POINT ( 'NONE',  ( 7.070501591499377789E-16, 11.54700538379251284, -159.1250000000000000 ) ) ;
#286 = CARTESIAN_POINT ( 'NONE',  ( -10.81189881249999729, 1.324075727343319199E-15, -0.7812500020483725827 ) ) ;
#287 = CARTESIAN_POINT ( 'NONE',  ( -5.405949406250003975, -9.363379034771801557, -70.84375000204836681 ) ) ;
#288 = CARTESIAN_POINT ( 'NONE',  ( -10.81189881249999907, -6.242252689847864744, -44.15625000204838102 ) ) ;
#289 = CARTESIAN_POINT ( 'NONE',  ( -5.405949406249996869, 9.363379034771805109, -51.84375000204835260 ) ) ;
#290 = CARTESIAN_POINT ( 'NONE',  ( -1.040834085586084257E-14, -20.00000000000000355, 32.49999999999999289 ) ) ;
#291 = CARTESIAN_POINT ( 'NONE',  ( 10.81189881249999551, -6.242252689847874514, -158.9687500020484094 ) ) ;
#292 = CARTESIAN_POINT ( 'NONE',  ( 7.070501591499377789E-16, 11.54700538379251284, -127.6249999999999858 ) ) ;
#293 = CARTESIAN_POINT ( 'NONE',  ( -5.405949406250003975, -9.363379034771801557, -138.5312500020484094 ) ) ;
#294 = CARTESIAN_POINT ( 'NONE',  ( 9.999999999999998224, 0.000000000000000000, -150.5000000000000000 ) ) ;
#295 = CARTESIAN_POINT ( 'NONE',  ( 9.999999999999996447, -5.773502691896262640, -118.0000000040967905 ) ) ;
#296 = CARTESIAN_POINT ( 'NONE',  ( -9.999999999999998224, 5.773502691896259087, -92.87500000000000000 ) ) ;
#297 = ORIENTED_EDGE ( 'NONE', *, *, #13005, .T. ) ;
#298 = CARTESIAN_POINT ( 'NONE',  ( -2.293366432827344421E-15, -12.48450537969573659, -112.9062500020483952 ) ) ;
#299 = CARTESIAN_POINT ( 'NONE',  ( 10.00000000000000000, 5.773502691896255534, -128.2500000040967620 ) ) ;
#300 = LINE ( 'NONE', #39765, #14626 ) ;
#301 = CARTESIAN_POINT ( 'NONE',  ( -10.81189881249999729, 6.242252689847871849, -162.9062500020484094 ) ) ;
#302 = CARTESIAN_POINT ( 'NONE',  ( -10.00000000000000000, -5.773502691896251982, -45.00000000409676204 ) ) ;
#303 = EDGE_CURVE ( 'NONE', #6776, #24567, #9100, .T. ) ;
#304 = CARTESIAN_POINT ( 'NONE',  ( 9.999999999999998224, 0.000000000000000000, -155.3750000040967905 ) ) ;
#305 = CARTESIAN_POINT ( 'NONE',  ( 5.405949406249999534, 9.363379034771803333, -50.78125000204835970 ) ) ;
#306 = CARTESIAN_POINT ( 'NONE',  ( 9.999999999999479527, 5.773502691896553074, -73.87499999999994316 ) ) ;
#307 = CARTESIAN_POINT ( 'NONE',  ( -5.405949406249996869, 9.363379034771805109, -161.5312500020484094 ) ) ;
#308 = CARTESIAN_POINT ( 'NONE',  ( 5.405949406249992428, -9.363379034771808662, -136.5937500020483810 ) ) ;
#309 = CARTESIAN_POINT ( 'NONE',  ( -9.999999999999998224, 1.224646799147353059E-15, -100.2499999999999858 ) ) ;
#310 = CARTESIAN_POINT ( 'NONE',  ( -5.000000000000003553, -8.660254037844383745, -196.0000000000000000 ) ) ;
#311 = VERTEX_POINT ( 'NONE', #39824 ) ;
#312 = CARTESIAN_POINT ( 'NONE',  ( -4.999999999999996447, 8.660254037844387298, -130.8750000040967905 ) ) ;
#314 = ORIENTED_EDGE ( 'NONE', *, *, #31517, .F. ) ;
#313 = CARTESIAN_POINT ( 'NONE',  ( 5.405949406249992428, -9.363379034771808662, -70.78125000204838102 ) ) ;
#315 = PERSON_AND_ORGANIZATION ( #11915, #17965 ) ;
#317 = VERTEX_POINT ( 'NONE', #16084 ) ;
#316 = CARTESIAN_POINT ( 'NONE',  ( -5.405949406249996869, 9.363379034771805109, -117.8437500020483810 ) ) ;
#318 = VERTEX_POINT ( 'NONE', #29279 ) ;
#319 = CARTESIAN_POINT ( 'NONE',  ( 10.81189881249999551, -6.242252689847874514, -17.96875000204837036 ) ) ;
#320 =( BOUNDED_CURVE ( )  B_SPLINE_CURVE ( 2, ( #6511, #29389, #19660, #35453, #2432, #8903, #15567 ),
 .UNSPECIFIED., .F., .F. ) 
 B_SPLINE_CURVE_WITH_KNOTS ( ( 3, 2, 2, 3 ),
 ( 0.3955223880597015795, 0.3967661691542289648, 0.3980099502487563501, 0.3992537313432836799 ),
 .UNSPECIFIED. ) 
 CURVE ( )  GEOMETRIC_REPRESENTATION_ITEM ( )  RATIONAL_B_SPLINE_CURVE ( ( 0.9999999999999880096, 0.8660254037844506980, 1.000000000000000000, 0.8660254037844387076, 1.000000000000000000, 0.8660254037844267172, 1.000000000000011990 ) ) 
 REPRESENTATION_ITEM ( '' )  );
#321 = CARTESIAN_POINT ( 'NONE',  ( 5.405949406249999534, 9.363379034771803333, -196.0937500020484094 ) ) ;
#322 = CARTESIAN_POINT ( 'NONE',  ( -10.81189881249999907, -6.242252689847864744, -45.46875000204837391 ) ) ;
#323 = CARTESIAN_POINT ( 'NONE',  ( 0.000000000000000000, 0.000000000000000000, -200.0000000000000000 ) ) ;
#324 = DIRECTION ( 'NONE',  ( 1.000000000000000000, 0.000000000000000000, 0.000000000000000000 ) ) ;
#325 = CARTESIAN_POINT ( 'NONE',  ( -10.81189881249999729, -6.242252689847864744, -183.4687500020484094 ) ) ;
#326 = CARTESIAN_POINT ( 'NONE',  ( 10.81189881249999907, 6.242252689847868297, -170.7187500020483810 ) ) ;
#327 = CARTESIAN_POINT ( 'NONE',  ( -5.405949406249996869, 9.363379034771805109, -146.3437500020483810 ) ) ;
#328 = CARTESIAN_POINT ( 'NONE',  ( 5.405949406249999534, 9.363379034771803333, -163.0937500020484094 ) ) ;
#329 = CARTESIAN_POINT ( 'NONE',  ( -9.999999999999998224, 1.224646799147353059E-15, -105.1250000040967763 ) ) ;
#330 =( BOUNDED_CURVE ( )  B_SPLINE_CURVE ( 2, ( #4756, #1316, #14448, #8439, #17905, #11862, #34553 ),
 .UNSPECIFIED., .F., .F. ) 
 B_SPLINE_CURVE_WITH_KNOTS ( ( 3, 2, 2, 3 ),
 ( 0.1567164179104477695, 0.1579601990049751270, 0.1592039800995025123, 0.1604477611940298698 ),
 .UNSPECIFIED. ) 
 CURVE ( )  GEOMETRIC_REPRESENTATION_ITEM ( )  RATIONAL_B_SPLINE_CURVE ( ( 1.000000000000000000, 0.8660254037844387076, 1.000000000000000000, 0.8660254037844387076, 1.000000000000000000, 0.8660254037844357100, 1.000000000000003109 ) ) 
 REPRESENTATION_ITEM ( '' )  );
#331 = FACE_OUTER_BOUND ( 'NONE', #10477, .T. ) ;
#332 = CARTESIAN_POINT ( 'NONE',  ( -5.000000000000003553, -8.660254037844383745, -188.5000000000000000 ) ) ;
#333 = CARTESIAN_POINT ( 'NONE',  ( -10.81189881249999729, 6.242252689847871849, -96.71875000204838102 ) ) ;
#334 = CARTESIAN_POINT ( 'NONE',  ( -5.405949406250003975, -9.363379034771801557, -68.03125000204838102 ) ) ;
#335 = CYLINDRICAL_SURFACE ( 'NONE', #35072, 9.999999999999998224 ) ;
#336 = CARTESIAN_POINT ( 'NONE',  ( 7.644554776091147741E-16, 12.48450537969573659, -183.9687500020484094 ) ) ;
#337 = CARTESIAN_POINT ( 'NONE',  ( -10.81189881249999907, -6.242252689847864744, -119.1562500020484237 ) ) ;
#338 = CARTESIAN_POINT ( 'NONE',  ( 7.644554776091147741E-16, 12.48450537969573659, -163.1562500020483810 ) ) ;
#339 = CARTESIAN_POINT ( 'NONE',  ( 7.644554776091147741E-16, 12.48450537969573659, -50.65625000204837391 ) ) ;
#340 = CARTESIAN_POINT ( 'NONE',  ( 5.000000000000000000, 8.660254037844385522, -137.1250000040967620 ) ) ;
#341 = CARTESIAN_POINT ( 'NONE',  ( 5.000000000000000000, 8.660254037844385522, -112.7499999999999858 ) ) ;
#342 = VERTEX_POINT ( 'NONE', #10257 ) ;
#343 = AXIS2_PLACEMENT_3D ( 'NONE', #16719, #354, #20184 ) ;
#344 = CARTESIAN_POINT ( 'NONE',  ( 7.644554776091147741E-16, 12.48450537969573659, -137.6562500020484094 ) ) ;
#345 = CARTESIAN_POINT ( 'NONE',  ( -10.81189881249999729, 1.324075727343319199E-15, -152.2812500020484094 ) ) ;
#346 = CARTESIAN_POINT ( 'NONE',  ( -10.81189881249999729, 6.242252689847871849, -189.9062500020484379 ) ) ;
#347 = CARTESIAN_POINT ( 'NONE',  ( -9.999999999999998224, 1.224646799147353059E-15, -125.7499999999999716 ) ) ;
#348 = CARTESIAN_POINT ( 'NONE',  ( 10.81189881249999907, 6.242252689847868297, -82.21875000204836681 ) ) ;
#349 = ORIENTED_EDGE ( 'NONE', *, *, #20808, .F. ) ;
#350 = CARTESIAN_POINT ( 'NONE',  ( 9.999999999999998224, 0.000000000000000000, -57.49999999999996447 ) ) ;
#351 = CARTESIAN_POINT ( 'NONE',  ( -2.293366432827344421E-15, -12.48450537969573659, -181.7187500020484094 ) ) ;
#352 = CARTESIAN_POINT ( 'NONE',  ( -5.000000000000003553, -8.660254037844383745, -67.37500000409676204 ) ) ;
#353 = EDGE_CURVE ( 'NONE', #4966, #40396, #23982, .T. ) ;
#354 = DIRECTION ( 'NONE',  ( -0.000000000000000000, -0.000000000000000000, 1.000000000000000000 ) ) ;
#355 = CARTESIAN_POINT ( 'NONE',  ( 9.999999999999998224, 0.000000000000000000, -71.37500000409677625 ) ) ;
#356 = EDGE_CURVE ( 'NONE', #32390, #11765, #10047, .T. ) ;
#357 = CARTESIAN_POINT ( 'NONE',  ( -5.405949406250003975, -9.363379034771801557, -77.03125000204838102 ) ) ;
#358 = CARTESIAN_POINT ( 'NONE',  ( -5.405949406249996869, 9.363379034771805109, -61.03125000204837391 ) ) ;
#359 = ADVANCED_FACE ( 'NONE', ( #16509 ), #6406, .T. ) ;
#360 = CARTESIAN_POINT ( 'NONE',  ( -4.999999999999996447, 8.660254037844387298, -60.37500000409676204 ) ) ;
#361 = CARTESIAN_POINT ( 'NONE',  ( 10.81189881249999907, 6.242252689847868297, -8.718750002048359704 ) ) ;
#362 = DIRECTION ( 'NONE',  ( -0.000000000000000000, -0.000000000000000000, 1.000000000000000000 ) ) ;
#363 = CARTESIAN_POINT ( 'NONE',  ( 10.81189881249999729, 0.000000000000000000, -184.5312500020484094 ) ) ;
#364 = CARTESIAN_POINT ( 'NONE',  ( -10.81189881249999729, 6.242252689847871849, -9.906250002048366810 ) ) ;
#365 = CARTESIAN_POINT ( 'NONE',  ( 5.405949406249999534, 9.363379034771803333, -1.093750002048365921 ) ) ;
#366 = CARTESIAN_POINT ( 'NONE',  ( 9.999999999999998224, 0.000000000000000000, -147.8750000040967905 ) ) ;
#367 = CARTESIAN_POINT ( 'NONE',  ( 4.999999999999992006, -8.660254037844389075, -45.74999999999998579 ) ) ;
#368 = CC_DESIGN_PERSON_AND_ORGANIZATION_ASSIGNMENT ( #31056, #21758, ( #36620 ) ) ;
#369 = CARTESIAN_POINT ( 'NONE',  ( -5.000000000000003553, -8.660254037844383745, -134.8750000040967905 ) ) ;
#370 = CARTESIAN_POINT ( 'NONE',  ( 7.070501591499377789E-16, 11.54700538379251284, -168.1250000000000000 ) ) ;
#371 = CARTESIAN_POINT ( 'NONE',  ( -9.999999999999742428, -5.773502691896402084, -122.6249999999999858 ) ) ;
#373 = ORIENTED_EDGE ( 'NONE', *, *, #16628, .T. ) ;
#372 = CARTESIAN_POINT ( 'NONE',  ( 7.644554776091147741E-16, 12.48450537969573659, -92.65625000204839523 ) ) ;
#374 = CARTESIAN_POINT ( 'NONE',  ( -9.999999999999998224, 1.224646799147353059E-15, -160.6250000040967905 ) ) ;
#375 = EDGE_CURVE ( 'NONE', #30674, #33916, #10463, .T. ) ;
#377 = ORIENTED_EDGE ( 'NONE', *, *, #20105, .T. ) ;
#376 = CARTESIAN_POINT ( 'NONE',  ( -5.405949406250003975, -9.363379034771801557, -100.8437500020483810 ) ) ;
#378 = ORIENTED_EDGE ( 'NONE', *, *, #33115, .F. ) ;
#379 = CARTESIAN_POINT ( 'NONE',  ( -5.405949406250003975, -9.363379034771801557, -36.34375000204836681 ) ) ;
#380 = VECTOR ( 'NONE', #39658, 1000.000000000000000 ) ;
#381 = CARTESIAN_POINT ( 'NONE',  ( 10.81189881249999729, 0.000000000000000000, -24.03125000204836681 ) ) ;
#382 = EDGE_CURVE ( 'NONE', #28565, #29057, #16244, .T. ) ;
#383 = CARTESIAN_POINT ( 'NONE',  ( 10.81189881249999551, -6.242252689847874514, -70.46875000204840944 ) ) ;
#384 = LINE ( 'NONE', #32964, #19456 ) ;
#385 = EDGE_CURVE ( 'NONE', #1917, #4764, #24732, .T. ) ;
#386 = CARTESIAN_POINT ( 'NONE',  ( 10.81189881249999907, 6.242252689847868297, -193.2187500020484094 ) ) ;
#387 = CARTESIAN_POINT ( 'NONE',  ( 10.81189881249999729, 0.000000000000000000, -149.8437500020483810 ) ) ;
#388 = CARTESIAN_POINT ( 'NONE',  ( 5.000000000000000000, 8.660254037844385522, -132.6250000040967620 ) ) ;
#389 = DIRECTION ( 'NONE',  ( -0.000000000000000000, -0.000000000000000000, 1.000000000000000000 ) ) ;
#390 = CARTESIAN_POINT ( 'NONE',  ( 10.81189881249999729, 0.000000000000000000, -145.5312500020483810 ) ) ;
#391 = CARTESIAN_POINT ( 'NONE',  ( 7.070501591499377789E-16, 11.54700538379251284, -2.000000004096753159 ) ) ;
#392 = CARTESIAN_POINT ( 'NONE',  ( 5.405949406249992428, -9.363379034771808662, -124.5937500020483952 ) ) ;
#393 = FACE_OUTER_BOUND ( 'NONE', #36030, .T. ) ;
#394 = CARTESIAN_POINT ( 'NONE',  ( 10.81189881249999551, -6.242252689847874514, -93.15625000204838102 ) ) ;
#395 = CARTESIAN_POINT ( 'NONE',  ( 10.81189881249999729, 6.242252689847867408, -109.2187500020483810 ) ) ;
#396 = CARTESIAN_POINT ( 'NONE',  ( 10.81189881249999907, 6.242252689847868297, -73.21875000204836681 ) ) ;
#397 = CARTESIAN_POINT ( 'NONE',  ( -10.81189881249999729, 1.324075727343319199E-15, -75.78125000204838102 ) ) ;
#398 = CARTESIAN_POINT ( 'NONE',  ( 9.999999999999998224, 0.000000000000000000, -165.8750000040967905 ) ) ;
#399 = DIRECTION ( 'NONE',  ( -1.000000000000000000, 0.000000000000000000, 0.000000000000000000 ) ) ;
#400 = CARTESIAN_POINT ( 'NONE',  ( -10.81189881249999729, 1.324075727343319199E-15, -156.7812500020484094 ) ) ;
#401 = CARTESIAN_POINT ( 'NONE',  ( -2.293366432827344421E-15, -12.48450537969573659, -168.4062500020483810 ) ) ;
#402 = DIRECTION ( 'NONE',  ( -0.000000000000000000, -0.000000000000000000, -1.000000000000000000 ) ) ;
#403 = CARTESIAN_POINT ( 'NONE',  ( -10.81189881249999729, 6.242252689847871849, -0.7187500020483517105 ) ) ;
#404 = CARTESIAN_POINT ( 'NONE',  ( -5.000000000000003553, -8.660254037844383745, -108.9999999999999858 ) ) ;
#405 = CARTESIAN_POINT ( 'NONE',  ( 10.81189881249999551, -6.242252689847874514, -107.9687500020483810 ) ) ;
#406 = CARTESIAN_POINT ( 'NONE',  ( -5.000000000000003553, -8.660254037844383745, -84.99999999999997158 ) ) ;
#407 = CARTESIAN_POINT ( 'NONE',  ( 10.81189881249999907, 6.242252689847868297, -13.40625000204837036 ) ) ;
#408 = CARTESIAN_POINT ( 'NONE',  ( -4.999999999999996447, 8.660254037844387298, -90.37500000409677625 ) ) ;
#409 = VECTOR ( 'NONE', #32686, 1000.000000000000000 ) ;
#410 =( BOUNDED_CURVE ( )  B_SPLINE_CURVE ( 2, ( #7723, #30182, #3850, #7503, #30606, #17408, #620 ),
 .UNSPECIFIED., .F., .F. ) 
 B_SPLINE_CURVE_WITH_KNOTS ( ( 3, 2, 2, 3 ),
 ( 0.1529850746268656692, 0.1542288557213930267, 0.1554726368159203842, 0.1567164179104477695 ),
 .UNSPECIFIED. ) 
 CURVE ( )  GEOMETRIC_REPRESENTATION_ITEM ( )  RATIONAL_B_SPLINE_CURVE ( ( 1.000000000000000000, 0.8660254037844387076, 1.000000000000000000, 0.8660254037844387076, 1.000000000000000000, 0.8660254037844387076, 1.000000000000000000 ) ) 
 REPRESENTATION_ITEM ( '' )  );
#411 = CARTESIAN_POINT ( 'NONE',  ( -4.999999999999996447, 8.660254037844387298, -115.4999999999999858 ) ) ;
#412 = CARTESIAN_POINT ( 'NONE',  ( 10.81189881249999729, 0.000000000000000000, -109.5312500020483810 ) ) ;
#413 = CARTESIAN_POINT ( 'NONE',  ( -10.81189881249999729, 6.242252689847871849, -84.90625000204838102 ) ) ;
#414 = VERTEX_POINT ( 'NONE', #34229 ) ;
#415 = ADVANCED_FACE ( 'NONE', ( #31205 ), #992, .F. ) ;
#416 = CARTESIAN_POINT ( 'NONE',  ( -9.999999999999998224, 1.224646799147353059E-15, -87.12500000409677625 ) ) ;
#417 = CARTESIAN_POINT ( 'NONE',  ( 9.999999999999998224, 0.000000000000000000, -48.49999999999998579 ) ) ;
#418 = CARTESIAN_POINT ( 'NONE',  ( 10.81189881249999907, 6.242252689847868297, -41.71875000204835970 ) ) ;
#419 = VERTEX_POINT ( 'NONE', #17362 ) ;
#420 = CARTESIAN_POINT ( 'NONE',  ( 4.999999999999992006, -8.660254037844389075, -6.749999999999978684 ) ) ;
#421 = CARTESIAN_POINT ( 'NONE',  ( -2.121150477449813534E-15, -11.54700538379251284, -141.8750000000000000 ) ) ;
#422 = CARTESIAN_POINT ( 'NONE',  ( 9.999999999999998224, 0.000000000000000000, -140.0000000000000000 ) ) ;
#423 = CARTESIAN_POINT ( 'NONE',  ( 4.999999999999992006, -8.660254037844389075, -13.12500000409674783 ) ) ;
#424 = CARTESIAN_POINT ( 'NONE',  ( 4.999999999999992006, -8.660254037844389075, -194.2500000000000000 ) ) ;
#425 = CARTESIAN_POINT ( 'NONE',  ( 7.070501591499376803E-16, 11.54700538379251284, -96.12500000000000000 ) ) ;
#427 = ORIENTED_EDGE ( 'NONE', *, *, #34188, .T. ) ;
#426 = CARTESIAN_POINT ( 'NONE',  ( -5.405949406250003975, -9.363379034771801557, -117.5312500020483952 ) ) ;
#428 = CARTESIAN_POINT ( 'NONE',  ( 9.999999999999998224, 0.000000000000000000, -13.99999999999995737 ) ) ;
#429 = AXIS2_PLACEMENT_3D ( 'NONE', #40358, #23353, #23565 ) ;
#430 = ORIENTED_EDGE ( 'NONE', *, *, #34123, .T. ) ;
#431 = EDGE_CURVE ( 'NONE', #17742, #13704, #21254, .T. ) ;
#432 = AXIS2_PLACEMENT_3D ( 'NONE', #22811, #9638, #19552 ) ;
#433 = CARTESIAN_POINT ( 'NONE',  ( 7.644554776091147741E-16, 12.48450537969573659, -49.15625000204837391 ) ) ;
#434 = COORDINATED_UNIVERSAL_TIME_OFFSET ( 6, 0, .AHEAD. ) ;
#435 = CARTESIAN_POINT ( 'NONE',  ( -10.81189881249999729, 6.242252689847871849, -96.71875000204838102 ) ) ;
#436 = CARTESIAN_POINT ( 'NONE',  ( 5.405949406249992428, -9.363379034771808662, -121.7812500020483952 ) ) ;
#437 = VERTEX_POINT ( 'NONE', #1633 ) ;
#438 = AXIS2_PLACEMENT_3D ( 'NONE', #20570, #30100, #539 ) ;
#439 = CARTESIAN_POINT ( 'NONE',  ( -10.00000000000154188, 5.773502691895366468, -51.25000000409671941 ) ) ;
#440 = CARTESIAN_POINT ( 'NONE',  ( 4.999999999999992006, -8.660254037844389075, -125.6250000040967620 ) ) ;
#441 = CARTESIAN_POINT ( 'NONE',  ( -5.405949406250003975, -9.363379034771801557, -171.5312500020484094 ) ) ;
#442 = CARTESIAN_POINT ( 'NONE',  ( -10.00000000000038547, 5.773502691896036154, -154.7500000040967905 ) ) ;
#443 = CARTESIAN_POINT ( 'NONE',  ( -10.81189881249999729, 6.242252689847871849, -135.7187500020483810 ) ) ;
#444 = CARTESIAN_POINT ( 'NONE',  ( 5.405949406249999534, 9.363379034771803333, -92.59375000204838102 ) ) ;
#445 = CARTESIAN_POINT ( 'NONE',  ( -5.000000000000003553, -8.660254037844383745, -44.49999999999998579 ) ) ;
#446 = CARTESIAN_POINT ( 'NONE',  ( 10.81189881249999907, 6.242252689847868297, -103.4062500020483952 ) ) ;
#447 = CARTESIAN_POINT ( 'NONE',  ( -5.000000000000003553, -8.660254037844383745, -184.3750000040967905 ) ) ;
#448 = CARTESIAN_POINT ( 'NONE',  ( -10.81189881249999729, 6.242252689847871849, -116.2187500020483810 ) ) ;
#449 = CARTESIAN_POINT ( 'NONE',  ( -10.81189881249999729, -6.242252689847864744, -174.6562500020484094 ) ) ;
#450 =( BOUNDED_CURVE ( )  B_SPLINE_CURVE ( 2, ( #33037, #22265, #38870, #35646, #2628, #12315, #3257 ),
 .UNSPECIFIED., .F., .F. ) 
 B_SPLINE_CURVE_WITH_KNOTS ( ( 3, 2, 2, 3 ),
 ( 0.2462686567164180107, 0.2475124378109453960, 0.2487562189054727535, 0.2500000000000001110 ),
 .UNSPECIFIED. ) 
 CURVE ( )  GEOMETRIC_REPRESENTATION_ITEM ( )  RATIONAL_B_SPLINE_CURVE ( ( 0.9999999999999880096, 0.8660254037844506980, 1.000000000000000000, 0.8660254037844387076, 1.000000000000000000, 0.8660254037844267172, 1.000000000000011990 ) ) 
 REPRESENTATION_ITEM ( '' )  );
#451 = CARTESIAN_POINT ( 'NONE',  ( 5.000000000000000000, 8.660254037844385522, -3.249999999999975131 ) ) ;
#452 = CARTESIAN_POINT ( 'NONE',  ( 9.999999999999676703, 5.773502691896441164, -185.2500000040967620 ) ) ;
#453 = CARTESIAN_POINT ( 'NONE',  ( 5.000000000000000000, 8.660254037844385522, -7.749999999999978684 ) ) ;
#454 = CARTESIAN_POINT ( 'NONE',  ( 7.644554776091147741E-16, 12.48450537969573659, -59.46875000204837391 ) ) ;
#455 = CARTESIAN_POINT ( 'NONE',  ( 10.81189881249999729, 0.000000000000000000, -40.34375000204837391 ) ) ;
#456 = CARTESIAN_POINT ( 'NONE',  ( 10.00000000000000000, 5.773502691896255534, -180.7500000040968189 ) ) ;
#457 = CARTESIAN_POINT ( 'NONE',  ( 10.81189881249999729, 0.000000000000000000, -19.53125000204835970 ) ) ;
#458 = CARTESIAN_POINT ( 'NONE',  ( -5.405949406249996869, 9.363379034771805109, -30.84375000204836326 ) ) ;
#459 = DIRECTION ( 'NONE',  ( -0.000000000000000000, -0.000000000000000000, -1.000000000000000000 ) ) ;
#460 = CARTESIAN_POINT ( 'NONE',  ( 7.644554776091147741E-16, 12.48450537969573659, -140.4687500020483810 ) ) ;
#461 = CARTESIAN_POINT ( 'NONE',  ( 4.999999999999992006, -8.660254037844389075, -105.7499999999999858 ) ) ;
#462 = CARTESIAN_POINT ( 'NONE',  ( -5.405949406250003975, -9.363379034771801557, -38.03125000204838102 ) ) ;
#463 = CARTESIAN_POINT ( 'NONE',  ( -5.000000000000003553, -8.660254037844383745, -148.0000000000000000 ) ) ;
#464 = AXIS2_PLACEMENT_3D ( 'NONE', #4502, #8399, #24809 ) ;
#465 = CARTESIAN_POINT ( 'NONE',  ( 5.000000000000000000, 8.660254037844385522, -57.24999999999996447 ) ) ;
#466 = CARTESIAN_POINT ( 'NONE',  ( -10.81189881249999729, 6.242252689847871849, -128.4062500020484094 ) ) ;
#467 = CARTESIAN_POINT ( 'NONE',  ( 7.644554776091147741E-16, 12.48450537969573659, -110.6562500020483810 ) ) ;
#468 = VERTEX_POINT ( 'NONE', #30351 ) ;
#469 = FACE_OUTER_BOUND ( 'NONE', #25673, .T. ) ;
#470 = CARTESIAN_POINT ( 'NONE',  ( 7.070501591499377789E-16, 11.54700538379251284, -105.5000000040967763 ) ) ;
#471 = CARTESIAN_POINT ( 'NONE',  ( -1.040834085586084257E-14, -125.0000000000000000, 22.49999999999999289 ) ) ;
#472 = CARTESIAN_POINT ( 'NONE',  ( 5.405949406249999534, 9.363379034771803333, -70.09375000204836681 ) ) ;
#473 = ORIENTED_EDGE ( 'NONE', *, *, #25999, .F. ) ;
#474 = CARTESIAN_POINT ( 'NONE',  ( -9.999999999999998224, 1.224646799147353059E-15, -32.74999999999997158 ) ) ;
#475 = CARTESIAN_POINT ( 'NONE',  ( 7.070501591499377789E-16, 11.54700538379251284, -21.50000000409676559 ) ) ;
#476 = CARTESIAN_POINT ( 'NONE',  ( -2.293366432827344421E-15, -12.48450537969573659, -42.40625000204837391 ) ) ;
#477 = DIRECTION ( 'NONE',  ( -0.000000000000000000, -0.000000000000000000, 1.000000000000000000 ) ) ;
#478 = CARTESIAN_POINT ( 'NONE',  ( -4.999999999999996447, 8.660254037844387298, -37.87500000409676915 ) ) ;
#479 = CARTESIAN_POINT ( 'NONE',  ( 7.070501591499376803E-16, 11.54700538379251284, -57.50000000409677625 ) ) ;
#480 = EDGE_CURVE ( 'NONE', #37390, #31108, #781, .T. ) ;
#481 = CARTESIAN_POINT ( 'NONE',  ( -5.405949406249996869, 9.363379034771805109, -145.0312500020483810 ) ) ;
#482 = CARTESIAN_POINT ( 'NONE',  ( -2.121150477449813534E-15, -11.54700538379251284, -15.87499999999997868 ) ) ;
#483 = ORIENTED_EDGE ( 'NONE', *, *, #39890, .F. ) ;
#484 = ORIENTED_EDGE ( 'NONE', *, *, #2776, .T. ) ;
#485 = CARTESIAN_POINT ( 'NONE',  ( 9.999999999999998224, 0.000000000000000000, -114.4999999999999858 ) ) ;
#486 = EDGE_CURVE ( 'NONE', #18454, #8390, #35575, .T. ) ;
#487 = CYLINDRICAL_SURFACE ( 'NONE', #21478, 9.999999999999998224 ) ;
#488 = CARTESIAN_POINT ( 'NONE',  ( 10.81189881249999551, -6.242252689847874514, -176.9687500020483810 ) ) ;
#489 = APPROVAL_PERSON_ORGANIZATION ( #33603, #2230, #3391 ) ;
#490 = CARTESIAN_POINT ( 'NONE',  ( 7.644554776091147741E-16, 12.48450537969573659, -196.1562500020484379 ) ) ;
#491 = CARTESIAN_POINT ( 'NONE',  ( -5.405949406249996869, 9.363379034771805109, -26.34375000204835970 ) ) ;
#492 = CARTESIAN_POINT ( 'NONE',  ( 10.00000000000000000, 5.773502691896255534, -170.2500000040967905 ) ) ;
#493 = CARTESIAN_POINT ( 'NONE',  ( 9.999999999999998224, 0.000000000000000000, -150.5000000000000000 ) ) ;
#494 = CARTESIAN_POINT ( 'NONE',  ( -5.405949406249996869, 9.363379034771805109, -158.3437500020483810 ) ) ;
#495 = CARTESIAN_POINT ( 'NONE',  ( 10.81189881249999907, 6.242252689847868297, -133.2187500020483810 ) ) ;
#496 = CARTESIAN_POINT ( 'NONE',  ( -2.121150477449813534E-15, -11.54700538379251284, -88.25000000409677625 ) ) ;
#497 = CARTESIAN_POINT ( 'NONE',  ( 5.405949406249999534, 9.363379034771803333, -127.0937500020483668 ) ) ;
#498 = CARTESIAN_POINT ( 'NONE',  ( -10.00000000000000000, -5.773502691896251982, -193.5000000040967905 ) ) ;
#499 = CARTESIAN_POINT ( 'NONE',  ( 5.405949406249992428, -9.363379034771808662, -135.2812500020483810 ) ) ;
#500 = CARTESIAN_POINT ( 'NONE',  ( 5.405949406249999534, 9.363379034771803333, -10.09375000204834549 ) ) ;
#501 = CARTESIAN_POINT ( 'NONE',  ( -10.81189881249999729, 6.242252689847871849, -135.7187500020483810 ) ) ;
#502 = CARTESIAN_POINT ( 'NONE',  ( -2.121150477449813534E-15, -11.54700538379251284, -129.8750000000000000 ) ) ;
#503 = CARTESIAN_POINT ( 'NONE',  ( 10.00000000000051159, -5.773502691895965988, -178.0000000040967336 ) ) ;
#504 = CARTESIAN_POINT ( 'NONE',  ( 10.00000000000000000, 5.773502691896255534, -154.8750000000000000 ) ) ;
#505 = CARTESIAN_POINT ( 'NONE',  ( -10.81189881249999729, 1.324075727343319199E-15, -86.09375000204836681 ) ) ;
#506 = CARTESIAN_POINT ( 'NONE',  ( -5.405949406249996869, 9.363379034771805109, -74.34375000204838102 ) ) ;
#507 = CARTESIAN_POINT ( 'NONE',  ( -5.405949406250003975, -9.363379034771801557, -41.03125000204838102 ) ) ;
#508 = CARTESIAN_POINT ( 'NONE',  ( -5.405949406249996869, 9.363379034771805109, -56.34375000204835970 ) ) ;
#509 = CARTESIAN_POINT ( 'NONE',  ( -9.999999999999998224, 1.224646799147353059E-15, -142.2500000000000000 ) ) ;
#510 = CARTESIAN_POINT ( 'NONE',  ( -10.81189881249999729, 6.242252689847871849, -165.7187500020483810 ) ) ;
#511 = CARTESIAN_POINT ( 'NONE',  ( -10.00000000000000000, -5.773502691896251982, -130.1250000000000000 ) ) ;
#512 = CARTESIAN_POINT ( 'NONE',  ( 7.644554776091147741E-16, 12.48450537969573659, -140.6562500020484094 ) ) ;
#513 = CARTESIAN_POINT ( 'NONE',  ( 0.000000000000000000, 0.000000000000000000, -200.0000000000000000 ) ) ;
#514 = CARTESIAN_POINT ( 'NONE',  ( 5.000000000000000000, 8.660254037844385522, -87.24999999999998579 ) ) ;
#515 = CARTESIAN_POINT ( 'NONE',  ( 5.405949406249992428, -9.363379034771808662, -18.28125000204835970 ) ) ;
#516 = VERTEX_POINT ( 'NONE', #4861 ) ;
#517 = CARTESIAN_POINT ( 'NONE',  ( 5.405949406249992428, -9.363379034771808662, -111.2812500020483810 ) ) ;
#518 = CARTESIAN_POINT ( 'NONE',  ( 9.999999999999998224, 0.000000000000000000, -135.8750000040967905 ) ) ;
#519 = CARTESIAN_POINT ( 'NONE',  ( -10.00000000000019185, -5.773502691896140071, -178.1249999999999432 ) ) ;
#520 = CARTESIAN_POINT ( 'NONE',  ( -10.81189881249999907, -6.242252689847864744, -167.1562500020483810 ) ) ;
#521 = CARTESIAN_POINT ( 'NONE',  ( 7.070501591499377789E-16, 11.54700538379251284, -44.00000000409676204 ) ) ;
#522 = CARTESIAN_POINT ( 'NONE',  ( 7.644554776091147741E-16, 12.48450537969573659, -49.15625000204837391 ) ) ;
#523 = EDGE_CURVE ( 'NONE', #21106, #26311, #40206, .T. ) ;
#524 = CARTESIAN_POINT ( 'NONE',  ( 5.405949406249999534, 9.363379034771803333, -164.7812500020484094 ) ) ;
#525 = CARTESIAN_POINT ( 'NONE',  ( -2.293366432827344421E-15, -12.48450537969573659, -135.2187500020483810 ) ) ;
#526 = CARTESIAN_POINT ( 'NONE',  ( 0.000000000000000000, 5.321294541346989426, -219.9999999999999716 ) ) ;
#527 = EDGE_LOOP ( 'NONE', ( #24852, #22930, #27645, #38076 ) ) ;
#528 = CARTESIAN_POINT ( 'NONE',  ( 7.070501591499376803E-16, 11.54700538379251284, -131.0000000040967905 ) ) ;
#530 = VERTEX_POINT ( 'NONE', #27313 ) ;
#529 = CARTESIAN_POINT ( 'NONE',  ( -10.81189881249999907, -6.242252689847864744, -62.15625000204838102 ) ) ;
#532 = ORIENTED_EDGE ( 'NONE', *, *, #29928, .F. ) ;
#531 = CARTESIAN_POINT ( 'NONE',  ( 5.405949406249992428, -9.363379034771808662, -115.5937500020483810 ) ) ;
#533 =( BOUNDED_CURVE ( )  B_SPLINE_CURVE ( 2, ( #18878, #5294, #15199, #35083, #38941, #2694, #21690 ),
 .UNSPECIFIED., .F., .F. ) 
 B_SPLINE_CURVE_WITH_KNOTS ( ( 3, 2, 2, 3 ),
 ( 0.02611940298507465369, 0.02736318407960201815, 0.02860696517412938261, 0.02985074626865674360 ),
 .UNSPECIFIED. ) 
 CURVE ( )  GEOMETRIC_REPRESENTATION_ITEM ( )  RATIONAL_B_SPLINE_CURVE ( ( 0.9999999999999970024, 0.8660254037844417052, 1.000000000000000000, 0.8660254037844387076, 1.000000000000000000, 0.8660254037844357100, 1.000000000000003109 ) ) 
 REPRESENTATION_ITEM ( '' )  );
#534 = CARTESIAN_POINT ( 'NONE',  ( 5.405949406249999534, 9.363379034771803333, -25.09375000204835970 ) ) ;
#535 = CARTESIAN_POINT ( 'NONE',  ( -5.405949406250003975, -9.363379034771801557, -195.3437500020484094 ) ) ;
#536 = CARTESIAN_POINT ( 'NONE',  ( 10.81189881249999729, 0.000000000000000000, -49.34375000204838102 ) ) ;
#537 = DIRECTION ( 'NONE',  ( -0.000000000000000000, -0.000000000000000000, 1.000000000000000000 ) ) ;
#538 = EDGE_CURVE ( 'NONE', #35065, #39621, #32792, .T. ) ;
#539 = DIRECTION ( 'NONE',  ( -1.000000000000000000, 0.000000000000000000, 0.000000000000000000 ) ) ;
#540 = CARTESIAN_POINT ( 'NONE',  ( 7.644554776091147741E-16, 12.48450537969573659, -176.4687500020484094 ) ) ;
#541 = CARTESIAN_POINT ( 'NONE',  ( -2.293366432827344421E-15, -12.48450537969573659, -169.7187500020483810 ) ) ;
#542 = CARTESIAN_POINT ( 'NONE',  ( -10.81189881249999907, -6.242252689847864744, -153.4687500020484094 ) ) ;
#543 = CARTESIAN_POINT ( 'NONE',  ( 7.644554776091147741E-16, 12.48450537969573659, -164.4687500020483810 ) ) ;
#544 = CARTESIAN_POINT ( 'NONE',  ( -5.000000000000003553, -8.660254037844383745, -104.8750000040967763 ) ) ;
#545 = CARTESIAN_POINT ( 'NONE',  ( 9.999999999999998224, 0.000000000000000000, -188.3750000040967905 ) ) ;
#546 = CARTESIAN_POINT ( 'NONE',  ( -4.999999999999996447, 8.660254037844387298, -183.0000000000000000 ) ) ;
#547 = CARTESIAN_POINT ( 'NONE',  ( 5.405949406249992428, -9.363379034771808662, -97.59375000204838102 ) ) ;
#548 = CARTESIAN_POINT ( 'NONE',  ( 5.405949406249999534, 9.363379034771803333, -65.78125000204838102 ) ) ;
#549 = CARTESIAN_POINT ( 'NONE',  ( 9.999999999999998224, 0.000000000000000000, -168.8750000040967905 ) ) ;
#550 = CARTESIAN_POINT ( 'NONE',  ( -10.81189881249999729, 6.242252689847871849, -188.2187500020483810 ) ) ;
#551 = CARTESIAN_POINT ( 'NONE',  ( -5.405949406250003975, -9.363379034771801557, -125.0312500020483952 ) ) ;
#552 = CARTESIAN_POINT ( 'NONE',  ( -2.293366432827344421E-15, -12.48450537969573659, -159.4062500020483810 ) ) ;
#553 = CARTESIAN_POINT ( 'NONE',  ( -10.81189881249999729, 6.242252689847871849, -51.90625000204837391 ) ) ;
#554 = CARTESIAN_POINT ( 'NONE',  ( 9.999999999999998224, 0.000000000000000000, -138.8750000040968189 ) ) ;
#555 = CARTESIAN_POINT ( 'NONE',  ( -2.121150477449813534E-15, -11.54700538379251284, -114.8749999999999716 ) ) ;
#556 = ORIENTED_EDGE ( 'NONE', *, *, #24143, .F. ) ;
#557 = CARTESIAN_POINT ( 'NONE',  ( 10.81189881249999551, -6.242252689847874514, -136.6562500020484094 ) ) ;
#558 = CARTESIAN_POINT ( 'NONE',  ( -5.405949406250003975, -9.363379034771801557, -144.5312500020483810 ) ) ;
#559 = CARTESIAN_POINT ( 'NONE',  ( -10.81189881249999729, 1.324075727343319199E-15, -188.2812500020484094 ) ) ;
#560 = CARTESIAN_POINT ( 'NONE',  ( -10.81189881249999729, 1.324075727343319199E-15, -80.09375000204838102 ) ) ;
#561 = AXIS2_PLACEMENT_3D ( 'NONE', #36619, #6430, #2984 ) ;
#562 = ORIENTED_EDGE ( 'NONE', *, *, #35604, .T. ) ;
#563 = CARTESIAN_POINT ( 'NONE',  ( -9.999999999999998224, 5.773502691896259087, -53.87499999999996447 ) ) ;
#564 = CARTESIAN_POINT ( 'NONE',  ( 5.405949406249992428, -9.363379034771808662, -181.5937500020483810 ) ) ;
#565 = CARTESIAN_POINT ( 'NONE',  ( 7.070501591499377789E-16, 11.54700538379251284, -68.00000000409679046 ) ) ;
#566 = CIRCLE ( 'NONE', #35714, 20.00000000000000000 ) ;
#567 = CARTESIAN_POINT ( 'NONE',  ( 7.070501591499376803E-16, 11.54700538379251284, -179.0000000040967905 ) ) ;
#568 = CARTESIAN_POINT ( 'NONE',  ( -5.405949406249996869, 9.363379034771805109, -77.53125000204838102 ) ) ;
#569 = CARTESIAN_POINT ( 'NONE',  ( 5.405949406249992428, -9.363379034771808662, -58.78125000204836681 ) ) ;
#570 =( BOUNDED_CURVE ( )  B_SPLINE_CURVE ( 2, ( #24153, #28024, #1483, #40729, #41154, #21541, #1270 ),
 .UNSPECIFIED., .F., .F. ) 
 B_SPLINE_CURVE_WITH_KNOTS ( ( 3, 2, 2, 3 ),
 ( 0.2201492537313433639, 0.2213930348258707215, 0.2226368159203980790, 0.2238805970149254365 ),
 .UNSPECIFIED. ) 
 CURVE ( )  GEOMETRIC_REPRESENTATION_ITEM ( )  RATIONAL_B_SPLINE_CURVE ( ( 0.9999999999999910072, 0.8660254037844477004, 1.000000000000000000, 0.8660254037844387076, 1.000000000000000000, 0.8660254037844327124, 1.000000000000005995 ) ) 
 REPRESENTATION_ITEM ( '' )  );
#571 = CARTESIAN_POINT ( 'NONE',  ( -9.999999999999998224, 5.773502691896259087, -49.75000000409676915 ) ) ;
#572 = CARTESIAN_POINT ( 'NONE',  ( 10.81189881249999551, -6.242252689847874514, -8.968750002048359704 ) ) ;
#573 = DIRECTION ( 'NONE',  ( 1.000000000000000000, 0.000000000000000000, 0.000000000000000000 ) ) ;
#574 = CARTESIAN_POINT ( 'NONE',  ( -5.405949406250003975, -9.363379034771801557, -182.0312500020483810 ) ) ;
#575 = CARTESIAN_POINT ( 'NONE',  ( 10.81189881249999729, 0.000000000000000000, -4.531250002048375691 ) ) ;
#576 = CARTESIAN_POINT ( 'NONE',  ( 5.000000000000000000, 8.660254037844385522, -85.74999999999998579 ) ) ;
#577 = CARTESIAN_POINT ( 'NONE',  ( 7.320508151741852210, -7.320508031779506375, -100.0669873003032393 ) ) ;
#578 = CARTESIAN_POINT ( 'NONE',  ( -9.999999999999227285, -5.773502691896698735, -103.5000000040967336 ) ) ;
#579 = DIRECTION ( 'NONE',  ( -0.000000000000000000, -0.000000000000000000, 1.000000000000000000 ) ) ;
#580 =( BOUNDED_CURVE ( )  B_SPLINE_CURVE ( 2, ( #41162, #856, #11601, #23943, #21549, #20896, #11392 ),
 .UNSPECIFIED., .F., .F. ) 
 B_SPLINE_CURVE_WITH_KNOTS ( ( 3, 2, 2, 3 ),
 ( 0.4253731343283583266, 0.4266169154228856564, 0.4278606965174130417, 0.4291044776119404269 ),
 .UNSPECIFIED. ) 
 CURVE ( )  GEOMETRIC_REPRESENTATION_ITEM ( )  RATIONAL_B_SPLINE_CURVE ( ( 0.9999999999999880096, 0.8660254037844506980, 1.000000000000000000, 0.8660254037844387076, 1.000000000000000000, 0.8660254037844267172, 1.000000000000011990 ) ) 
 REPRESENTATION_ITEM ( '' )  );
#581 = CARTESIAN_POINT ( 'NONE',  ( -9.999999999999998224, 1.224646799147353059E-15, -146.7500000000000000 ) ) ;
#583 = ORIENTED_EDGE ( 'NONE', *, *, #23598, .F. ) ;
#582 = CARTESIAN_POINT ( 'NONE',  ( -10.81189881249999729, 6.242252689847871849, -92.40625000204838102 ) ) ;
#584 = CARTESIAN_POINT ( 'NONE',  ( -4.999999999999996447, 8.660254037844387298, -24.37500000409675849 ) ) ;
#586 = ORIENTED_EDGE ( 'NONE', *, *, #41768, .F. ) ;
#585 = CARTESIAN_POINT ( 'NONE',  ( 3.516324526667281347, 10.45435446766629894, -100.0500568239963002 ) ) ;
#587 = VERTEX_POINT ( 'NONE', #37224 ) ;
#588 = CARTESIAN_POINT ( 'NONE',  ( -10.81189881249999729, 6.242252689847871849, -23.21875000204836326 ) ) ;
#589 = CARTESIAN_POINT ( 'NONE',  ( -10.81189881249999729, 6.242252689847871849, -21.90625000204837036 ) ) ;
#590 =( BOUNDED_CURVE ( )  B_SPLINE_CURVE ( 2, ( #31404, #18430, #8519, #21672, #31619, #26918, #41073 ),
 .UNSPECIFIED., .F., .F. ) 
 B_SPLINE_CURVE_WITH_KNOTS ( ( 3, 2, 2, 3 ),
 ( 0.02985074626865674360, 0.03109452736318411153, 0.03233830845771147600, 0.03358208955223884046 ),
 .UNSPECIFIED. ) 
 CURVE ( )  GEOMETRIC_REPRESENTATION_ITEM ( )  RATIONAL_B_SPLINE_CURVE ( ( 0.9999999999999970024, 0.8660254037844417052, 1.000000000000000000, 0.8660254037844387076, 1.000000000000000000, 0.8660254037844349329, 1.000000000000003775 ) ) 
 REPRESENTATION_ITEM ( '' )  );
#591 = DATE_TIME_ROLE ( 'classification_date' ) ;
#592 = CARTESIAN_POINT ( 'NONE',  ( -10.81189881249999907, -6.242252689847864744, -70.96875000204840944 ) ) ;
#593 = CARTESIAN_POINT ( 'NONE',  ( -10.00000000000012790, -5.773502691896178263, -174.0000000040968473 ) ) ;
#594 = ADVANCED_FACE ( 'NONE', ( #20609 ), #33795, .T. ) ;
#595 = CARTESIAN_POINT ( 'NONE',  ( 4.999999999999992006, -8.660254037844389075, -45.74999999999998579 ) ) ;
#596 = CARTESIAN_POINT ( 'NONE',  ( 5.405949406249999534, 9.363379034771803333, -196.0937500020484094 ) ) ;
#597 = CARTESIAN_POINT ( 'NONE',  ( 5.405949406249999534, 9.363379034771803333, -148.0937500020483810 ) ) ;
#598 = EDGE_CURVE ( 'NONE', #33430, #41855, #8103, .T. ) ;
#599 = CARTESIAN_POINT ( 'NONE',  ( -10.00000000000076916, 5.773502691895813221, -132.2500000040967620 ) ) ;
#600 = FACE_OUTER_BOUND ( 'NONE', #38499, .T. ) ;
#601 = CARTESIAN_POINT ( 'NONE',  ( 7.644554776091147741E-16, 12.48450537969573659, -149.6562500020484094 ) ) ;
#602 = CARTESIAN_POINT ( 'NONE',  ( -2.121150477449813534E-15, -11.54700538379251284, -2.750000004096756712 ) ) ;
#603 = LINE ( 'NONE', #13718, #29480 ) ;
#604 = CARTESIAN_POINT ( 'NONE',  ( 5.405949406249999534, 9.363379034771803333, -124.0937500020483952 ) ) ;
#605 = DIRECTION ( 'NONE',  ( -0.000000000000000000, -0.000000000000000000, 1.000000000000000000 ) ) ;
#606 = CARTESIAN_POINT ( 'NONE',  ( 5.405949406249999534, 9.363379034771803333, -94.28125000204838102 ) ) ;
#607 = CARTESIAN_POINT ( 'NONE',  ( 10.81189881249999729, 6.242252689847867408, -100.2187500020483810 ) ) ;
#608 = CARTESIAN_POINT ( 'NONE',  ( -10.81189881249999729, 6.242252689847871849, -72.71875000204835260 ) ) ;
#609 = CARTESIAN_POINT ( 'NONE',  ( -5.405949406249996869, 9.363379034771805109, -73.03125000204838102 ) ) ;
#610 = CARTESIAN_POINT ( 'NONE',  ( 10.00000000000000000, 5.773502691896255534, -165.7500000040967905 ) ) ;
#611 = CARTESIAN_POINT ( 'NONE',  ( 5.405949406249992428, -9.363379034771808662, -159.2812500020484094 ) ) ;
#612 = CARTESIAN_POINT ( 'NONE',  ( 5.405949406249999534, 9.363379034771803333, -170.7812500020484094 ) ) ;
#613 = DIRECTION ( 'NONE',  ( -0.000000000000000000, -0.000000000000000000, 1.000000000000000000 ) ) ;
#614 = DIRECTION ( 'NONE',  ( -0.000000000000000000, -0.000000000000000000, -1.000000000000000000 ) ) ;
#615 = CARTESIAN_POINT ( 'NONE',  ( -2.121150477449813534E-15, -11.54700538379251284, -149.3750000000000000 ) ) ;
#616 = CARTESIAN_POINT ( 'NONE',  ( 10.81189881249999729, 0.000000000000000000, -107.8437500020483810 ) ) ;
#617 = CARTESIAN_POINT ( 'NONE',  ( -4.999999999999996447, 8.660254037844387298, -79.49999999999998579 ) ) ;
#618 = CARTESIAN_POINT ( 'NONE',  ( -10.81189881249999729, 1.324075727343319199E-15, -8.281250002048350822 ) ) ;
#619 = CARTESIAN_POINT ( 'NONE',  ( 9.999999999999998224, 0.000000000000000000, -93.87500000409677625 ) ) ;
#620 = CARTESIAN_POINT ( 'NONE',  ( 9.999999999999998224, 0.000000000000000000, -168.5000000000000000 ) ) ;
#621 = CARTESIAN_POINT ( 'NONE',  ( 10.81189881249999729, 0.000000000000000000, -99.03125000204839523 ) ) ;
#622 = CARTESIAN_POINT ( 'NONE',  ( 7.644554776091147741E-16, 12.48450537969573659, -83.65625000204838102 ) ) ;
#623 = CARTESIAN_POINT ( 'NONE',  ( 7.070501591499377789E-16, 11.54700538379251284, -75.50000000409677625 ) ) ;
#624 = CARTESIAN_POINT ( 'NONE',  ( 9.999999999999998224, 0.000000000000000000, -146.3750000040967905 ) ) ;
#625 = CARTESIAN_POINT ( 'NONE',  ( 10.81189881249999907, 6.242252689847868297, -32.71875000204835260 ) ) ;
#626 = EDGE_LOOP ( 'NONE', ( #27970, #9734, #5629, #32320 ) ) ;
#627 = CARTESIAN_POINT ( 'NONE',  ( -9.999999999999998224, 5.773502691896259087, -10.37499999999995381 ) ) ;
#628 = CARTESIAN_POINT ( 'NONE',  ( 5.405949406249999534, 9.363379034771803333, -31.28125000204837036 ) ) ;
#629 = CARTESIAN_POINT ( 'NONE',  ( -4.999999999999996447, 8.660254037844387298, -147.0000000000000000 ) ) ;
#630 = CARTESIAN_POINT ( 'NONE',  ( -9.999999999999998224, 1.224646799147353059E-15, -139.2499999999999716 ) ) ;
#631 = EDGE_CURVE ( 'NONE', #26632, #15830, #7962, .T. ) ;
#632 = VECTOR ( 'NONE', #19479, 1000.000000000000000 ) ;
#633 = CARTESIAN_POINT ( 'NONE',  ( -9.999999999999998224, 1.224646799147353059E-15, -13.62500000409674961 ) ) ;
#634 = CARTESIAN_POINT ( 'NONE',  ( -9.999999999999998224, 5.773502691896259087, -188.8750000000000568 ) ) ;
#635 = CARTESIAN_POINT ( 'NONE',  ( 7.070501591499376803E-16, 11.54700538379251284, -123.1249999999999858 ) ) ;
#637 = ORIENTED_EDGE ( 'NONE', *, *, #8821, .T. ) ;
#636 = CARTESIAN_POINT ( 'NONE',  ( -5.405949406249996869, 9.363379034771805109, -118.0312500020483952 ) ) ;
#638 = CARTESIAN_POINT ( 'NONE',  ( 4.999999999999992006, -8.660254037844389075, -74.62500000409677625 ) ) ;
#639 = ORIENTED_EDGE ( 'NONE', *, *, #8724, .T. ) ;
#640 = ORIENTED_EDGE ( 'NONE', *, *, #901, .F. ) ;
#641 = CARTESIAN_POINT ( 'NONE',  ( 7.644554776091147741E-16, 12.48450537969573659, -43.15625000204838102 ) ) ;
#642 = SHAPE_DEFINITION_REPRESENTATION ( #7327, #6779 ) ;
#643 = CARTESIAN_POINT ( 'NONE',  ( -10.81189881249999907, -6.242252689847864744, -94.96875000204838102 ) ) ;
#644 = CARTESIAN_POINT ( 'NONE',  ( 10.81189881249999729, 0.000000000000000000, -120.0312500020483952 ) ) ;
#646 = ORIENTED_EDGE ( 'NONE', *, *, #5501, .F. ) ;
#645 = EDGE_CURVE ( 'NONE', #15029, #36871, #9699, .T. ) ;
#647 = CARTESIAN_POINT ( 'NONE',  ( -9.999999999999998224, 1.224646799147353059E-15, -133.2499999999999716 ) ) ;
#648 = CARTESIAN_POINT ( 'NONE',  ( 10.81189881249999729, 0.000000000000000000, -193.3437500020484094 ) ) ;
#649 = ADVANCED_FACE ( 'NONE', ( #25782 ), #8323, .T. ) ;
#650 = CARTESIAN_POINT ( 'NONE',  ( 7.644554776091147741E-16, 12.48450537969573659, -169.1562500020484094 ) ) ;
#651 = EDGE_CURVE ( 'NONE', #26892, #19714, #35826, .T. ) ;
#652 = CARTESIAN_POINT ( 'NONE',  ( -5.405949406249996869, 9.363379034771805109, -129.8437500020484094 ) ) ;
#653 =( BOUNDED_CURVE ( )  B_SPLINE_CURVE ( 2, ( #37800, #31773, #34793, #28743, #41870, #5213, #18149 ),
 .UNSPECIFIED., .F., .F. ) 
 B_SPLINE_CURVE_WITH_KNOTS ( ( 3, 2, 2, 3 ),
 ( 0.9328358208955226383, 0.9340796019900500236, 0.9353233830845774088, 0.9365671641791047941 ),
 .UNSPECIFIED. ) 
 CURVE ( )  GEOMETRIC_REPRESENTATION_ITEM ( )  RATIONAL_B_SPLINE_CURVE ( ( 0.9999999999999761302, 0.8660254037844625774, 1.000000000000000000, 0.8660254037844387076, 1.000000000000000000, 0.8660254037844028474, 1.000000000000035971 ) ) 
 REPRESENTATION_ITEM ( '' )  );
#654 = CC_DESIGN_DATE_AND_TIME_ASSIGNMENT ( #34558, #4987, ( #8303 ) ) ;
#655 = CARTESIAN_POINT ( 'NONE',  ( 5.405949406249992428, -9.363379034771808662, -93.09375000204838102 ) ) ;
#656 = CARTESIAN_POINT ( 'NONE',  ( -4.999999999999996447, 8.660254037844387298, -154.5000000000000000 ) ) ;
#657 = CARTESIAN_POINT ( 'NONE',  ( -5.405949406250003975, -9.363379034771801557, -98.03125000204839523 ) ) ;
#658 = CARTESIAN_POINT ( 'NONE',  ( 4.999999999999992006, -8.660254037844389075, -187.1250000040967905 ) ) ;
#659 = CARTESIAN_POINT ( 'NONE',  ( 5.405949406249999534, 9.363379034771803333, -110.5937500020483810 ) ) ;
#660 = CARTESIAN_POINT ( 'NONE',  ( -2.293366432827344421E-15, -12.48450537969573659, -178.9062500020484379 ) ) ;
#661 = CARTESIAN_POINT ( 'NONE',  ( 9.999999999999998224, 0.000000000000000000, -200.0000000000000000 ) ) ;
#662 = CARTESIAN_POINT ( 'NONE',  ( 10.81189881249999729, 0.000000000000000000, -178.5312500020483810 ) ) ;
#663 = CARTESIAN_POINT ( 'NONE',  ( 7.644554776091147741E-16, 12.48450537969573659, -196.1562500020484379 ) ) ;
#664 = CARTESIAN_POINT ( 'NONE',  ( -5.405949406249996869, 9.363379034771805109, -63.84375000204836681 ) ) ;
#665 = VECTOR ( 'NONE', #4017, 1000.000000000000000 ) ;
#666 = CARTESIAN_POINT ( 'NONE',  ( 10.81189881249999551, -6.242252689847874514, -44.96875000204836681 ) ) ;
#667 = CARTESIAN_POINT ( 'NONE',  ( 9.999999999999998224, 0.000000000000000000, -173.3750000040968189 ) ) ;
#668 = CARTESIAN_POINT ( 'NONE',  ( 5.405949406249999534, 9.363379034771803333, -19.28125000204835970 ) ) ;
#669 = CARTESIAN_POINT ( 'NONE',  ( -5.405949406249996869, 9.363379034771805109, -21.84375000204835615 ) ) ;
#670 = DIRECTION ( 'NONE',  ( 1.000000000000000000, 0.000000000000000000, 0.000000000000000000 ) ) ;
#671 = CARTESIAN_POINT ( 'NONE',  ( -2.293366432827344421E-15, -12.48450537969573659, -126.2187500020483952 ) ) ;
#672 = CARTESIAN_POINT ( 'NONE',  ( 4.999999999999992006, -8.660254037844389075, -107.2499999999999858 ) ) ;
#673 = CARTESIAN_POINT ( 'NONE',  ( -10.81189881249999729, 6.242252689847871849, -29.40625000204835260 ) ) ;
#674 = CARTESIAN_POINT ( 'NONE',  ( 6.964452268037472749, 6.964452268037473637, -201.2186212422413689 ) ) ;
#675 = CARTESIAN_POINT ( 'NONE',  ( 7.070501591499377789E-16, 11.54700538379251284, -55.62499999999998579 ) ) ;
#676 = CARTESIAN_POINT ( 'NONE',  ( -5.405949406250003975, -9.363379034771801557, -123.5312500020483952 ) ) ;
#677 = CARTESIAN_POINT ( 'NONE',  ( -5.405949406249996869, 9.363379034771805109, -109.0312500020483810 ) ) ;
#678 = ADVANCED_FACE ( 'NONE', ( #5078 ), #28601, .T. ) ;
#679 = ORIENTED_EDGE ( 'NONE', *, *, #9216, .T. ) ;
#680 = CARTESIAN_POINT ( 'NONE',  ( -4.999999999999996447, 8.660254037844387298, -160.5000000000000000 ) ) ;
#681 = CARTESIAN_POINT ( 'NONE',  ( 4.999999999999992006, -8.660254037844389075, -104.6250000040967763 ) ) ;
#682 = CARTESIAN_POINT ( 'NONE',  ( 9.999999999999872102, 5.773502691896329253, -162.3750000000000000 ) ) ;
#683 = CARTESIAN_POINT ( 'NONE',  ( -5.405949406250003975, -9.363379034771801557, -60.34375000204835970 ) ) ;
#684 = VERTEX_POINT ( 'NONE', #25360 ) ;
#685 = CARTESIAN_POINT ( 'NONE',  ( -5.000000000000003553, -8.660254037844383745, -32.49999999999997158 ) ) ;
#686 = CARTESIAN_POINT ( 'NONE',  ( 5.405949406249992428, -9.363379034771808662, -36.28125000204837391 ) ) ;
#687 = CARTESIAN_POINT ( 'NONE',  ( 4.999999999999992006, -8.660254037844389075, -38.62500000409676915 ) ) ;
#688 = CARTESIAN_POINT ( 'NONE',  ( -10.00000000000102496, 5.773502691895664007, -57.25000000409674072 ) ) ;
#689 = CARTESIAN_POINT ( 'NONE',  ( -10.81189881249999729, 6.242252689847871849, -144.9062500020484094 ) ) ;
#690 = CARTESIAN_POINT ( 'NONE',  ( -4.999999999999996447, 8.660254037844387298, -166.8750000040967905 ) ) ;
#691 = EDGE_LOOP ( 'NONE', ( #4059, #17804, #37681, #25112 ) ) ;
#692 = VECTOR ( 'NONE', #41320, 1000.000000000000227 ) ;
#693 = ORIENTED_EDGE ( 'NONE', *, *, #35509, .F. ) ;
#694 = DIRECTION ( 'NONE',  ( -0.000000000000000000, -0.000000000000000000, -1.000000000000000000 ) ) ;
#695 = CYLINDRICAL_SURFACE ( 'NONE', #38038, 9.999999999999998224 ) ;
#696 =( BOUNDED_CURVE ( )  B_SPLINE_CURVE ( 2, ( #32919, #42190, #13037, #42399, #26231, #3352, #25810 ),
 .UNSPECIFIED., .F., .F. ) 
 B_SPLINE_CURVE_WITH_KNOTS ( ( 3, 2, 2, 3 ),
 ( 0.3320895522388061516, 0.3333333333333334259, 0.3345771144278607556, 0.3358208955223880854 ),
 .UNSPECIFIED. ) 
 CURVE ( )  GEOMETRIC_REPRESENTATION_ITEM ( )  RATIONAL_B_SPLINE_CURVE ( ( 0.9999999999999820144, 0.8660254037844566932, 1.000000000000000000, 0.8660254037844387076, 1.000000000000000000, 0.8660254037844387076, 1.000000000000000000 ) ) 
 REPRESENTATION_ITEM ( '' )  );
#697 = CARTESIAN_POINT ( 'NONE',  ( -10.81189881249999729, 6.242252689847871849, -164.2187500020483810 ) ) ;
#698 = CARTESIAN_POINT ( 'NONE',  ( 10.81189881249999729, 0.000000000000000000, -198.0312500020484094 ) ) ;
#699 = CARTESIAN_POINT ( 'NONE',  ( 5.405949406249999534, 9.363379034771803333, -16.09375000204835260 ) ) ;
#700 = CARTESIAN_POINT ( 'NONE',  ( -12.99038105676667598, 7.500000000000051514, 49.99999999999998579 ) ) ;
#701 = CARTESIAN_POINT ( 'NONE',  ( -10.81189881249999729, 6.242252689847871849, -158.2187500020483810 ) ) ;
#702 = CARTESIAN_POINT ( 'NONE',  ( -5.405949406249996869, 9.363379034771805109, -138.8437500020484094 ) ) ;
#703 = CARTESIAN_POINT ( 'NONE',  ( -2.121150477449813534E-15, -11.54700538379251284, -8.750000004096753159 ) ) ;
#704 = CARTESIAN_POINT ( 'NONE',  ( 10.81189881249999551, -6.242252689847874514, -115.4687500020483810 ) ) ;
#705 = CARTESIAN_POINT ( 'NONE',  ( 9.999999999999998224, 0.000000000000000000, -192.8750000040967905 ) ) ;
#706 = CARTESIAN_POINT ( 'NONE',  ( -5.405949406249996869, 9.363379034771805109, -127.0312500020483952 ) ) ;
#707 = CARTESIAN_POINT ( 'NONE',  ( -5.405949406250003975, -9.363379034771801557, -12.34375000204834905 ) ) ;
#708 = CARTESIAN_POINT ( 'NONE',  ( 10.81189881249999729, 6.242252689847867408, -136.2187500020483810 ) ) ;
#709 = CARTESIAN_POINT ( 'NONE',  ( 5.000000000000000000, 8.660254037844385522, -163.7500000000000000 ) ) ;
#710 = CARTESIAN_POINT ( 'NONE',  ( -9.999999999999998224, 1.224646799147353059E-15, -178.6250000040968189 ) ) ;
#711 = CARTESIAN_POINT ( 'NONE',  ( -4.999999999999996447, 8.660254037844387298, -151.5000000000000000 ) ) ;
#712 = CARTESIAN_POINT ( 'NONE',  ( -9.999999999999998224, 1.224646799147353059E-15, -19.24999999999996092 ) ) ;
#713 = EDGE_CURVE ( 'NONE', #35715, #25539, #16503, .T. ) ;
#714 = CARTESIAN_POINT ( 'NONE',  ( 10.81189881249999729, 0.000000000000000000, -82.34375000204836681 ) ) ;
#715 = CARTESIAN_POINT ( 'NONE',  ( -5.405949406250003975, -9.363379034771801557, -63.34375000204836681 ) ) ;
#716 = CARTESIAN_POINT ( 'NONE',  ( -9.999999999999998224, 1.224646799147353059E-15, -35.74999999999997868 ) ) ;
#717 = CARTESIAN_POINT ( 'NONE',  ( -5.405949406249996869, 9.363379034771805109, -44.53125000204838102 ) ) ;
#718 = CARTESIAN_POINT ( 'NONE',  ( 10.81189881249999729, 0.000000000000000000, -44.84375000204837391 ) ) ;
#719 = CYLINDRICAL_SURFACE ( 'NONE', #31650, 9.999999999999998224 ) ;
#720 = CARTESIAN_POINT ( 'NONE',  ( -10.81189881249999729, 1.324075727343319199E-15, -156.5937500020483810 ) ) ;
#721 = CARTESIAN_POINT ( 'NONE',  ( -10.00000000000000000, -5.773502691896251982, -131.6250000000000000 ) ) ;
#722 = CARTESIAN_POINT ( 'NONE',  ( 10.81189881249999729, 0.000000000000000000, -138.0312500020484094 ) ) ;
#723 = FACE_OUTER_BOUND ( 'NONE', #41523, .T. ) ;
#724 = CARTESIAN_POINT ( 'NONE',  ( 4.999999999999992006, -8.660254037844389075, -84.74999999999997158 ) ) ;
#725 = CARTESIAN_POINT ( 'NONE',  ( 5.405949406249999534, 9.363379034771803333, -17.78125000204835970 ) ) ;
#726 = ORIENTED_EDGE ( 'NONE', *, *, #22094, .T. ) ;
#727 = CARTESIAN_POINT ( 'NONE',  ( 5.405949406249992428, -9.363379034771808662, -108.2812500020483810 ) ) ;
#728 = CARTESIAN_POINT ( 'NONE',  ( 5.000000000000000000, 8.660254037844385522, -134.1250000040967620 ) ) ;
#729 = CARTESIAN_POINT ( 'NONE',  ( -9.999999999999998224, 1.224646799147353059E-15, -115.6250000040967905 ) ) ;
#730 = AXIS2_PLACEMENT_3D ( 'NONE', #35139, #34718, #14823 ) ;
#731 = CARTESIAN_POINT ( 'NONE',  ( 9.999999999999996447, -5.773502691896262640, -44.50000000409676915 ) ) ;
#732 = DIRECTION ( 'NONE',  ( -0.000000000000000000, -0.000000000000000000, -1.000000000000000000 ) ) ;
#733 = CARTESIAN_POINT ( 'NONE',  ( -2.293366432827344421E-15, -12.48450537969573659, -49.90625000204838102 ) ) ;
#734 = CARTESIAN_POINT ( 'NONE',  ( -10.81189881249999907, -6.242252689847864744, -152.1562500020484094 ) ) ;
#735 = CARTESIAN_POINT ( 'NONE',  ( -5.405949406250003975, -9.363379034771801557, -133.8437500020484094 ) ) ;
#736 = CARTESIAN_POINT ( 'NONE',  ( 9.999999999999479527, 5.773502691896553074, -150.3750000000000000 ) ) ;
#737 = ORIENTED_EDGE ( 'NONE', *, *, #16143, .T. ) ;
#738 = LINE ( 'NONE', #34393, #39657 ) ;
#740 = VERTEX_POINT ( 'NONE', #18224 ) ;
#739 = CARTESIAN_POINT ( 'NONE',  ( -2.293366432827344421E-15, -12.48450537969573659, -63.40625000204838102 ) ) ;
#741 = PERSON_AND_ORGANIZATION ( #11915, #17965 ) ;
#743 = ORIENTED_EDGE ( 'NONE', *, *, #17051, .T. ) ;
#742 = CARTESIAN_POINT ( 'NONE',  ( 7.644554776091147741E-16, 12.48450537969573659, -114.9687500020483668 ) ) ;
#744 = CARTESIAN_POINT ( 'NONE',  ( 7.644554776091147741E-16, 12.48450537969573659, -18.96875000204837391 ) ) ;
#745 = CARTESIAN_POINT ( 'NONE',  ( 5.405949406249999534, 9.363379034771803333, -188.5937500020483810 ) ) ;
#746 = CARTESIAN_POINT ( 'NONE',  ( 5.405949406249999534, 9.363379034771803333, -46.09375000204838102 ) ) ;
#747 = CARTESIAN_POINT ( 'NONE',  ( 9.999999999998456346, 5.773502691897149042, -62.25000000409676204 ) ) ;
#748 = FACE_OUTER_BOUND ( 'NONE', #30201, .T. ) ;
#749 = AXIS2_PLACEMENT_3D ( 'NONE', #21637, #18173, #15569 ) ;
#750 = CARTESIAN_POINT ( 'NONE',  ( -10.81189881249999729, -6.242252689847864744, -180.4687500020484094 ) ) ;
#751 = CARTESIAN_POINT ( 'NONE',  ( -5.405949406250003975, -9.363379034771801557, -163.8437500020484094 ) ) ;
#752 = CARTESIAN_POINT ( 'NONE',  ( 7.644554776091147741E-16, 12.48450537969573659, -143.4687500020483810 ) ) ;
#753 = CARTESIAN_POINT ( 'NONE',  ( 5.405949406249992428, -9.363379034771808662, -163.5937500020484094 ) ) ;
#754 = CYLINDRICAL_SURFACE ( 'NONE', #21930, 9.999999999999998224 ) ;
#755 = DIRECTION ( 'NONE',  ( -0.000000000000000000, -0.000000000000000000, -1.000000000000000000 ) ) ;
#756 = CARTESIAN_POINT ( 'NONE',  ( -5.000000000000003553, -8.660254037844383745, -182.5000000000000000 ) ) ;
#757 = CARTESIAN_POINT ( 'NONE',  ( -10.81189881249999729, 1.324075727343319199E-15, -92.09375000204838102 ) ) ;
#758 = CARTESIAN_POINT ( 'NONE',  ( -2.293366432827344421E-15, -12.48450537969573659, -69.40625000204838102 ) ) ;
#759 = CARTESIAN_POINT ( 'NONE',  ( -10.81189881249999907, -6.242252689847864744, -175.9687500020483526 ) ) ;
#760 = CARTESIAN_POINT ( 'NONE',  ( -5.405949406250003975, -9.363379034771801557, -122.0312500020483952 ) ) ;
#761 = CARTESIAN_POINT ( 'NONE',  ( 10.81189881249999551, -6.242252689847874514, -162.1562500020484094 ) ) ;
#762 = CARTESIAN_POINT ( 'NONE',  ( 10.81189881249999907, 6.242252689847868297, -52.40625000204838102 ) ) ;
#763 = CARTESIAN_POINT ( 'NONE',  ( -9.999999999999998224, 5.773502691896259087, -136.7500000040967905 ) ) ;
#764 = CARTESIAN_POINT ( 'NONE',  ( -5.000000000000003553, -8.660254037844383745, -104.4999999999999858 ) ) ;
#765 = ORIENTED_EDGE ( 'NONE', *, *, #1965, .F. ) ;
#766 = CARTESIAN_POINT ( 'NONE',  ( 5.405949406249992428, -9.363379034771808662, -138.2812500020483810 ) ) ;
#767 = CARTESIAN_POINT ( 'NONE',  ( -10.81189881249999907, -6.242252689847864744, -150.6562500020484094 ) ) ;
#768 = CARTESIAN_POINT ( 'NONE',  ( -5.405949406250003975, -9.363379034771801557, -188.0312500020484094 ) ) ;
#769 = CARTESIAN_POINT ( 'NONE',  ( -10.81189881249999729, 6.242252689847871849, -84.71875000204836681 ) ) ;
#770 = ORIENTED_EDGE ( 'NONE', *, *, #21485, .F. ) ;
#771 = CARTESIAN_POINT ( 'NONE',  ( -9.999999999999998224, 1.224646799147353059E-15, -52.24999999999996447 ) ) ;
#772 = CARTESIAN_POINT ( 'NONE',  ( -5.405949406250003975, -9.363379034771801557, -181.8437500020483810 ) ) ;
#773 = CARTESIAN_POINT ( 'NONE',  ( 9.999999999999996447, -5.773502691896262640, -62.50000000409677625 ) ) ;
#774 = DIRECTION ( 'NONE',  ( 1.000000000000000000, 0.000000000000000000, 0.000000000000000000 ) ) ;
#775 = CARTESIAN_POINT ( 'NONE',  ( 5.000000000000000000, 8.660254037844385522, -179.1250000040968189 ) ) ;
#776 = CARTESIAN_POINT ( 'NONE',  ( 7.644554776091147741E-16, 12.48450537969573659, -76.15625000204839523 ) ) ;
#777 = CARTESIAN_POINT ( 'NONE',  ( 7.644554776091147741E-16, 12.48450537969573659, -56.65625000204837391 ) ) ;
#778 = ADVANCED_FACE ( 'NONE', ( #8529 ), #41731, .T. ) ;
#779 = CARTESIAN_POINT ( 'NONE',  ( 10.00000000000000000, 5.773502691896255534, -51.75000000409676204 ) ) ;
#780 = CARTESIAN_POINT ( 'NONE',  ( -10.81189881249999729, 1.324075727343319199E-15, -8.093750002048343717 ) ) ;
#781 = LINE ( 'NONE', #14330, #22809 ) ;
#782 = CARTESIAN_POINT ( 'NONE',  ( -2.293366432827344421E-15, -12.48450537969573659, -174.4062500020483810 ) ) ;
#783 = APPROVAL_PERSON_ORGANIZATION ( #33118, #10370, #6361 ) ;
#784 = CARTESIAN_POINT ( 'NONE',  ( -10.81189881249999907, -6.242252689847864744, -6.656250002048364145 ) ) ;
#785 = DIRECTION ( 'NONE',  ( -0.000000000000000000, -0.000000000000000000, 1.000000000000000000 ) ) ;
#786 = DIRECTION ( 'NONE',  ( 1.000000000000000000, 4.506943796211477094E-16, 0.000000000000000000 ) ) ;
#787 = CARTESIAN_POINT ( 'NONE',  ( 9.999999999999998224, 0.000000000000000000, -102.8750000040967763 ) ) ;
#788 = FACE_OUTER_BOUND ( 'NONE', #14986, .T. ) ;
#789 = LINE ( 'NONE', #29930, #38601 ) ;
#791 = ORIENTED_EDGE ( 'NONE', *, *, #21137, .T. ) ;
#790 = CARTESIAN_POINT ( 'NONE',  ( 5.405949406249992428, -9.363379034771808662, -85.78125000204838102 ) ) ;
#792 = CYLINDRICAL_SURFACE ( 'NONE', #42070, 9.999999999999998224 ) ;
#794 = ORIENTED_EDGE ( 'NONE', *, *, #33571, .F. ) ;
#793 = DIRECTION ( 'NONE',  ( 0.000000000000000000, 0.000000000000000000, -1.000000000000000000 ) ) ;
#795 = VERTEX_POINT ( 'NONE', #5721 ) ;
#796 = CARTESIAN_POINT ( 'NONE',  ( 10.81189881249999551, -6.242252689847874514, -26.96875000204837747 ) ) ;
#797 = CARTESIAN_POINT ( 'NONE',  ( 5.405949406249999534, 9.363379034771803333, -20.78125000204836326 ) ) ;
#798 = APPROVAL_ROLE ( '' ) ;
#799 = CARTESIAN_POINT ( 'NONE',  ( -10.81189881249999729, 6.242252689847871849, -69.71875000204838102 ) ) ;
#800 = CARTESIAN_POINT ( 'NONE',  ( -9.999999999999742428, -5.773502691896402084, -122.6249999999999858 ) ) ;
#801 = CARTESIAN_POINT ( 'NONE',  ( 7.070501591499377789E-16, 11.54700538379251284, -43.62499999999996447 ) ) ;
#802 = CARTESIAN_POINT ( 'NONE',  ( -10.81189881249999729, 1.324075727343319199E-15, -183.5937500020483810 ) ) ;
#803 = AXIS2_PLACEMENT_3D ( 'NONE', #35661, #19239, #32428 ) ;
#804 = CARTESIAN_POINT ( 'NONE',  ( -9.999999999999998224, 1.224646799147353059E-15, -178.6250000040968189 ) ) ;
#805 = CARTESIAN_POINT ( 'NONE',  ( -10.00000000000051337, 5.773502691895962435, -98.87499999999997158 ) ) ;
#806 = CARTESIAN_POINT ( 'NONE',  ( -9.999999999999998224, 1.224646799147353059E-15, -95.74999999999998579 ) ) ;
#807 = CARTESIAN_POINT ( 'NONE',  ( 9.999999999999996447, -5.773502691896262640, -1.000000004096748496 ) ) ;
#808 = LINE ( 'NONE', #1232, #21898 ) ;
#809 = CC_DESIGN_APPROVAL ( #26222, ( #22864 ) ) ;
#810 = CARTESIAN_POINT ( 'NONE',  ( 5.405949406249999534, 9.363379034771803333, -118.0937500020483810 ) ) ;
#811 = CARTESIAN_POINT ( 'NONE',  ( -9.999999999999998224, 1.224646799147353059E-15, -109.2499999999999858 ) ) ;
#812 = CARTESIAN_POINT ( 'NONE',  ( 5.405949406249999534, 9.363379034771803333, -89.78125000204838102 ) ) ;
#813 = CARTESIAN_POINT ( 'NONE',  ( 5.405949406249992428, -9.363379034771808662, -97.59375000204838102 ) ) ;
#814 = CARTESIAN_POINT ( 'NONE',  ( -2.293366432827344421E-15, -12.48450537969573659, -66.21875000204838102 ) ) ;
#815 = CARTESIAN_POINT ( 'NONE',  ( -2.293366432827344421E-15, -12.48450537969573659, -78.40625000204838102 ) ) ;
#816 = CARTESIAN_POINT ( 'NONE',  ( 9.999999999999998224, 0.000000000000000000, -159.8750000040967905 ) ) ;
#817 =( BOUNDED_CURVE ( )  B_SPLINE_CURVE ( 2, ( #10105, #39880, #23929, #23502, #17205, #20245, #37073 ),
 .UNSPECIFIED., .F., .F. ) 
 B_SPLINE_CURVE_WITH_KNOTS ( ( 3, 2, 2, 3 ),
 ( 0.9141791044776121922, 0.9154228855721395774, 0.9166666666666669627, 0.9179104477611943480 ),
 .UNSPECIFIED. ) 
 CURVE ( )  GEOMETRIC_REPRESENTATION_ITEM ( )  RATIONAL_B_SPLINE_CURVE ( ( 0.9999999999999761302, 0.8660254037844625774, 1.000000000000000000, 0.8660254037844387076, 1.000000000000000000, 0.8660254037844028474, 1.000000000000035971 ) ) 
 REPRESENTATION_ITEM ( '' )  );
#818 = CARTESIAN_POINT ( 'NONE',  ( -10.81189881249999729, -6.242252689847864744, -158.1562500020484094 ) ) ;
#819 = CARTESIAN_POINT ( 'NONE',  ( -10.81189881249999729, 6.242252689847871849, -170.4062500020484094 ) ) ;
#820 = VECTOR ( 'NONE', #41436, 1000.000000000000000 ) ;
#821 = PLANE ( 'NONE',  #20595 ) ;
#822 = CARTESIAN_POINT ( 'NONE',  ( -9.999999999999998224, 1.224646799147353059E-15, -149.7500000000000000 ) ) ;
#823 = CARTESIAN_POINT ( 'NONE',  ( -5.405949406249996869, 9.363379034771805109, -102.8437500020483810 ) ) ;
#824 = DIRECTION ( 'NONE',  ( -0.000000000000000000, -0.000000000000000000, -1.000000000000000000 ) ) ;
#825 = CARTESIAN_POINT ( 'NONE',  ( -5.000000000000003553, -8.660254037844383745, -77.49999999999998579 ) ) ;
#826 = CARTESIAN_POINT ( 'NONE',  ( -5.405949406250003975, -9.363379034771801557, -3.531250002048374803 ) ) ;
#827 = CARTESIAN_POINT ( 'NONE',  ( -9.999999999999998224, 1.224646799147353059E-15, -93.12500000409677625 ) ) ;
#828 = CARTESIAN_POINT ( 'NONE',  ( 10.81189881249999551, -6.242252689847874514, -100.6562500020483952 ) ) ;
#829 = CARTESIAN_POINT ( 'NONE',  ( 5.405949406249999534, 9.363379034771803333, -86.78125000204838102 ) ) ;
#830 =( BOUNDED_CURVE ( )  B_SPLINE_CURVE ( 2, ( #36833, #13512, #36415, #10287, #3833, #30164, #23686 ),
 .UNSPECIFIED., .F., .F. ) 
 B_SPLINE_CURVE_WITH_KNOTS ( ( 3, 2, 2, 3 ),
 ( 0.2910447761194031036, 0.2922885572139304333, 0.2935323383084578186, 0.2947761194029852039 ),
 .UNSPECIFIED. ) 
 CURVE ( )  GEOMETRIC_REPRESENTATION_ITEM ( )  RATIONAL_B_SPLINE_CURVE ( ( 0.9999999999999880096, 0.8660254037844506980, 1.000000000000000000, 0.8660254037844387076, 1.000000000000000000, 0.8660254037844267172, 1.000000000000011990 ) ) 
 REPRESENTATION_ITEM ( '' )  );
#831 = CARTESIAN_POINT ( 'NONE',  ( -5.000000000000003553, -8.660254037844383745, -77.87500000409677625 ) ) ;
#832 = CARTESIAN_POINT ( 'NONE',  ( 10.81189881249999907, 6.242252689847868297, -37.21875000204835260 ) ) ;
#833 = ORIENTED_EDGE ( 'NONE', *, *, #26459, .F. ) ;
#834 = CARTESIAN_POINT ( 'NONE',  ( 9.999999999999996447, -5.773502691896262640, -11.12499999999995737 ) ) ;
#835 = CARTESIAN_POINT ( 'NONE',  ( 10.81189881249999907, 6.242252689847868297, -25.40625000204838102 ) ) ;
#836 = EDGE_CURVE ( 'NONE', #16464, #23854, #11860, .T. ) ;
#837 = CARTESIAN_POINT ( 'NONE',  ( 9.999999999999996447, -5.773502691896262640, -147.6250000000000000 ) ) ;
#838 = CARTESIAN_POINT ( 'NONE',  ( 9.999999999999998224, 0.000000000000000000, -200.0000000000000000 ) ) ;
#839 = CARTESIAN_POINT ( 'NONE',  ( 9.999999999999996447, -5.773502691896262640, -5.500000004096755823 ) ) ;
#840 = CARTESIAN_POINT ( 'NONE',  ( 7.644554776091147741E-16, 12.48450537969573659, -134.6562500020483810 ) ) ;
#841 = AXIS2_PLACEMENT_3D ( 'NONE', #9008, #5137, #34714 ) ;
#842 = CARTESIAN_POINT ( 'NONE',  ( -2.121150477449813534E-15, -11.54700538379251284, -188.3750000000000284 ) ) ;
#843 = DIRECTION ( 'NONE',  ( -1.000000000000000000, -4.506943796211477094E-16, 0.000000000000000000 ) ) ;
#844 = APPLICATION_CONTEXT ( 'configuration controlled 3d designs of mechanical parts and assemblies' ) ;
#846 = EDGE_LOOP ( 'NONE', ( #39244, #16924, #7522, #35832 ) ) ;
#845 = CARTESIAN_POINT ( 'NONE',  ( 10.81189881249999907, 6.242252689847868297, -113.9062500020483952 ) ) ;
#847 = CARTESIAN_POINT ( 'NONE',  ( -4.999999999999996447, 8.660254037844387298, -36.37500000409676915 ) ) ;
#848 = VERTEX_POINT ( 'NONE', #12170 ) ;
#849 = ORIENTED_EDGE ( 'NONE', *, *, #18345, .F. ) ;
#850 = CARTESIAN_POINT ( 'NONE',  ( 5.405949406249999534, 9.363379034771803333, -49.28125000204838813 ) ) ;
#851 = MECHANICAL_CONTEXT ( 'NONE', #29772, 'mechanical' ) ;
#852 = VECTOR ( 'NONE', #22630, 1000.000000000000000 ) ;
#853 = CARTESIAN_POINT ( 'NONE',  ( -5.405949406250003975, -9.363379034771801557, -93.34375000204838102 ) ) ;
#854 = CARTESIAN_POINT ( 'NONE',  ( 10.81189881249999729, 6.242252689847867408, -122.9062500020483810 ) ) ;
#855 = ORIENTED_EDGE ( 'NONE', *, *, #34933, .F. ) ;
#856 = CARTESIAN_POINT ( 'NONE',  ( 9.999999999999479527, 5.773502691896553074, -114.3749999999999716 ) ) ;
#857 = CARTESIAN_POINT ( 'NONE',  ( 5.405949406249999534, 9.363379034771803333, -194.5937500020484094 ) ) ;
#858 = CARTESIAN_POINT ( 'NONE',  ( -5.405949406250003975, -9.363379034771801557, -176.0312500020483810 ) ) ;
#859 = CARTESIAN_POINT ( 'NONE',  ( -2.121150477449813534E-15, -11.54700538379251284, -68.37499999999998579 ) ) ;
#860 = CARTESIAN_POINT ( 'NONE',  ( -10.81189881249999729, 1.324075727343319199E-15, -128.0937500020483810 ) ) ;
#861 = CARTESIAN_POINT ( 'NONE',  ( 10.81189881249999907, 6.242252689847868297, -92.71875000204836681 ) ) ;
#862 = CYLINDRICAL_SURFACE ( 'NONE', #31845, 9.999999999999998224 ) ;
#863 = CARTESIAN_POINT ( 'NONE',  ( 5.405949406249992428, -9.363379034771808662, -102.2812500020483952 ) ) ;
#864 = CARTESIAN_POINT ( 'NONE',  ( 7.070501591499377789E-16, 11.54700538379251284, -188.0000000040967905 ) ) ;
#865 = CARTESIAN_POINT ( 'NONE',  ( 10.81189881249999551, -6.242252689847874514, -109.4687500020483952 ) ) ;
#866 = CARTESIAN_POINT ( 'NONE',  ( 5.405949406249992428, -9.363379034771808662, -180.2812500020484094 ) ) ;
#867 = CARTESIAN_POINT ( 'NONE',  ( 80.00000000000002842, 19.99999999999999289, -160.0000000000000000 ) ) ;
#868 = DIRECTION ( 'NONE',  ( 0.000000000000000000, 0.000000000000000000, -1.000000000000000000 ) ) ;
#869 = CARTESIAN_POINT ( 'NONE',  ( 5.405949406249992428, -9.363379034771808662, -193.7812500020484094 ) ) ;
#870 = CARTESIAN_POINT ( 'NONE',  ( -10.81189881249999729, 1.324075727343319199E-15, -50.09375000204835260 ) ) ;
#871 = CARTESIAN_POINT ( 'NONE',  ( 10.81189881249999551, -6.242252689847874514, -41.96875000204835970 ) ) ;
#872 = CARTESIAN_POINT ( 'NONE',  ( -2.121150477449813534E-15, -11.54700538379251284, -173.7500000040968189 ) ) ;
#873 = CARTESIAN_POINT ( 'NONE',  ( 10.81189881249999729, 0.000000000000000000, -12.03125000204835438 ) ) ;
#874 = CARTESIAN_POINT ( 'NONE',  ( -5.405949406250003975, -9.363379034771801557, -19.84375000204835615 ) ) ;
#875 = FACE_OUTER_BOUND ( 'NONE', #15728, .T. ) ;
#876 = CARTESIAN_POINT ( 'NONE',  ( -10.81189881249999907, -6.242252689847864744, -133.9687500020483810 ) ) ;
#877 = CARTESIAN_POINT ( 'NONE',  ( 4.999999999999992006, -8.660254037844389075, -102.7500000000000000 ) ) ;
#878 = CARTESIAN_POINT ( 'NONE',  ( -10.81189881249999729, 1.324075727343319199E-15, -32.28125000204837391 ) ) ;
#879 = CARTESIAN_POINT ( 'NONE',  ( -5.000000000000003553, -8.660254037844383745, -57.99999999999997158 ) ) ;
#880 = CARTESIAN_POINT ( 'NONE',  ( -10.81189881249999907, -6.242252689847864744, -123.6562500020484094 ) ) ;
#881 = CARTESIAN_POINT ( 'NONE',  ( -5.405949406249996869, 9.363379034771805109, -106.0312500020483810 ) ) ;
#882 = ORIENTED_EDGE ( 'NONE', *, *, #22628, .F. ) ;
#883 = CARTESIAN_POINT ( 'NONE',  ( 4.999999999999992006, -8.660254037844389075, -6.749999999999978684 ) ) ;
#884 = CARTESIAN_POINT ( 'NONE',  ( 7.070501591499377789E-16, 11.54700538379251284, -104.0000000040967763 ) ) ;
#885 = CARTESIAN_POINT ( 'NONE',  ( 10.00000000000011013, -5.773502691896197803, -194.5000000040968189 ) ) ;
#886 = CARTESIAN_POINT ( 'NONE',  ( -2.293366432827344421E-15, -12.48450537969573659, -61.71875000204837391 ) ) ;
#887 = ORIENTED_EDGE ( 'NONE', *, *, #16169, .T. ) ;
#888 = CARTESIAN_POINT ( 'NONE',  ( -9.999999999999998224, 5.773502691896259087, -29.87499999999994671 ) ) ;
#889 = EDGE_CURVE ( 'NONE', #21756, #21702, #32549, .T. ) ;
#890 = CARTESIAN_POINT ( 'NONE',  ( 7.644554776091147741E-16, 12.48450537969573659, -35.65625000204835260 ) ) ;
#891 = CARTESIAN_POINT ( 'NONE',  ( -2.121150477449813534E-15, -11.54700538379251284, -90.87500000000000000 ) ) ;
#892 = CARTESIAN_POINT ( 'NONE',  ( 7.070501591499377789E-16, 11.54700538379251284, -30.50000000409674783 ) ) ;
#893 = ADVANCED_FACE ( 'NONE', ( #38728 ), #31847, .F. ) ;
#894 = ADVANCED_FACE ( 'NONE', ( #15403, #36540 ), #12798, .F. ) ;
#895 = CYLINDRICAL_SURFACE ( 'NONE', #29343, 9.999999999999998224 ) ;
#896 = CARTESIAN_POINT ( 'NONE',  ( -5.405949406250003975, -9.363379034771801557, -138.5312500020484094 ) ) ;
#897 = CC_DESIGN_DATE_AND_TIME_ASSIGNMENT ( #7744, #24158, ( #18005 ) ) ;
#898 = CARTESIAN_POINT ( 'NONE',  ( -4.999999999999996447, 8.660254037844387298, -174.3750000040968189 ) ) ;
#899 = ORIENTED_EDGE ( 'NONE', *, *, #28328, .T. ) ;
#900 = VERTEX_POINT ( 'NONE', #13639 ) ;
#901 = EDGE_CURVE ( 'NONE', #35538, #22217, #21188, .T. ) ;
#902 =( BOUNDED_CURVE ( )  B_SPLINE_CURVE ( 2, ( #15846, #28631, #22560, #29046, #28420, #31441, #38756 ),
 .UNSPECIFIED., .F., .F. ) 
 B_SPLINE_CURVE_WITH_KNOTS ( ( 3, 2, 2, 3 ),
 ( 0.3619402985074628432, 0.3631840796019901729, 0.3644278606965175027, 0.3656716417910448325 ),
 .UNSPECIFIED. ) 
 CURVE ( )  GEOMETRIC_REPRESENTATION_ITEM ( )  RATIONAL_B_SPLINE_CURVE ( ( 0.9999999999999820144, 0.8660254037844566932, 1.000000000000000000, 0.8660254037844387076, 1.000000000000000000, 0.8660254037844327124, 1.000000000000005995 ) ) 
 REPRESENTATION_ITEM ( '' )  );
#903 = CARTESIAN_POINT ( 'NONE',  ( 9.999999999999998224, 0.000000000000000000, -105.8750000040967763 ) ) ;
#904 = CARTESIAN_POINT ( 'NONE',  ( -10.81189881249999907, -6.242252689847864744, -163.9687500020484094 ) ) ;
#905 = ADVANCED_FACE ( 'NONE', ( #38935 ), #13216, .T. ) ;
#906 = CARTESIAN_POINT ( 'NONE',  ( 5.405949406249992428, -9.363379034771808662, -198.2812500020484094 ) ) ;
#907 = CARTESIAN_POINT ( 'NONE',  ( -2.293366432827344421E-15, -12.48450537969573659, -16.71875000204836326 ) ) ;
#908 = DIRECTION ( 'NONE',  ( 1.000000000000000000, 0.000000000000000000, 0.000000000000000000 ) ) ;
#909 = CARTESIAN_POINT ( 'NONE',  ( -5.405949406250003975, -9.363379034771801557, -144.3437500020483810 ) ) ;
#910 = CARTESIAN_POINT ( 'NONE',  ( 5.405949406249992428, -9.363379034771808662, -141.0937500020483810 ) ) ;
#911 = CARTESIAN_POINT ( 'NONE',  ( 10.81189881249999729, 0.000000000000000000, -109.5312500020483810 ) ) ;
#912 = CARTESIAN_POINT ( 'NONE',  ( 10.81189881249999551, -6.242252689847874514, -118.4687500020483810 ) ) ;
#913 = CARTESIAN_POINT ( 'NONE',  ( 5.000000000000000000, 8.660254037844385522, -195.6250000040967905 ) ) ;
#914 = CARTESIAN_POINT ( 'NONE',  ( 10.81189881249999907, 6.242252689847868297, -121.4062500020483810 ) ) ;
#915 = CARTESIAN_POINT ( 'NONE',  ( -10.81189881249999907, -6.242252689847864744, -13.96875000204836681 ) ) ;
#916 = CARTESIAN_POINT ( 'NONE',  ( 5.405949406249999534, 9.363379034771803333, -131.5937500020483810 ) ) ;
#917 = DIRECTION ( 'NONE',  ( 0.000000000000000000, 0.000000000000000000, -1.000000000000000000 ) ) ;
#918 = CARTESIAN_POINT ( 'NONE',  ( 10.00000000000051159, -5.773502691895965988, -96.62499999999998579 ) ) ;
#919 = CARTESIAN_POINT ( 'NONE',  ( 5.000000000000000000, 8.660254037844385522, -154.7500000000000000 ) ) ;
#920 = CARTESIAN_POINT ( 'NONE',  ( 7.070501591499377789E-16, 11.54700538379251284, -19.62499999999997513 ) ) ;
#921 = CARTESIAN_POINT ( 'NONE',  ( -10.81189881249999729, -6.242252689847864744, -84.46875000204836681 ) ) ;
#922 = CARTESIAN_POINT ( 'NONE',  ( 10.81189881249999551, -6.242252689847874514, -64.46875000204838102 ) ) ;
#923 = CARTESIAN_POINT ( 'NONE',  ( 10.81189881249999907, 6.242252689847868297, -37.40625000204836681 ) ) ;
#924 = CARTESIAN_POINT ( 'NONE',  ( -10.81189881249999907, -6.242252689847864744, -43.96875000204835970 ) ) ;
#925 = DIRECTION ( 'NONE',  ( 1.000000000000000000, 0.000000000000000000, 0.000000000000000000 ) ) ;
#926 = CARTESIAN_POINT ( 'NONE',  ( -10.81189881249999729, 6.242252689847871849, -153.7187500020483526 ) ) ;
#927 = CARTESIAN_POINT ( 'NONE',  ( -2.121150477449813534E-15, -11.54700538379251284, -128.3750000000000000 ) ) ;
#928 = CARTESIAN_POINT ( 'NONE',  ( 5.405949406249992428, -9.363379034771808662, -127.7812500020483810 ) ) ;
#929 = EDGE_CURVE ( 'NONE', #29237, #40403, #1924, .T. ) ;
#930 = CARTESIAN_POINT ( 'NONE',  ( 6.220436543609608293, 8.439850853362262484, -179.9999999999998863 ) ) ;
#931 = CARTESIAN_POINT ( 'NONE',  ( 4.999999999999992006, -8.660254037844389075, -86.24999999999998579 ) ) ;
#932 = CARTESIAN_POINT ( 'NONE',  ( -5.405949406249996869, 9.363379034771805109, -22.03125000204836326 ) ) ;
#933 = VERTEX_POINT ( 'NONE', #36122 ) ;
#934 = CARTESIAN_POINT ( 'NONE',  ( -10.81189881249999729, 6.242252689847871849, -110.4062500020483810 ) ) ;
#935 = CARTESIAN_POINT ( 'NONE',  ( 10.00000000000000000, 5.773502691896255534, -125.2500000040967905 ) ) ;
#936 = CARTESIAN_POINT ( 'NONE',  ( -4.999999999999996447, 8.660254037844387298, -38.99999999999997868 ) ) ;
#937 = CARTESIAN_POINT ( 'NONE',  ( -10.00000000000000000, -5.773502691896251982, -33.00000000409676204 ) ) ;
#938 = CARTESIAN_POINT ( 'NONE',  ( 9.999999999999998224, 0.000000000000000000, -129.8750000040967905 ) ) ;
#939 = CARTESIAN_POINT ( 'NONE',  ( -2.293366432827344421E-15, -12.48450537969573659, -55.90625000204838102 ) ) ;
#940 = CARTESIAN_POINT ( 'NONE',  ( 9.999999999999998224, 0.000000000000000000, -146.0000000000000000 ) ) ;
#941 = CARTESIAN_POINT ( 'NONE',  ( -2.293366432827344421E-15, -12.48450537969573659, -151.9062500020483810 ) ) ;
#942 = CARTESIAN_POINT ( 'NONE',  ( -5.405949406250003975, -9.363379034771801557, -136.8437500020484094 ) ) ;
#943 = CARTESIAN_POINT ( 'NONE',  ( -9.999999999999998224, 1.224646799147353059E-15, -199.2500000000000000 ) ) ;
#944 = ORIENTED_EDGE ( 'NONE', *, *, #33581, .T. ) ;
#945 = CYLINDRICAL_SURFACE ( 'NONE', #32114, 9.999999999999998224 ) ;
#946 = ORIENTED_EDGE ( 'NONE', *, *, #37567, .T. ) ;
#947 =( BOUNDED_CURVE ( )  B_SPLINE_CURVE ( 2, ( #24537, #27764, #27336, #11550, #27982, #24759, #4887 ),
 .UNSPECIFIED., .F., .F. ) 
 B_SPLINE_CURVE_WITH_KNOTS ( ( 3, 2, 2, 3 ),
 ( 0.07835820895522395413, 0.07960199004975131165, 0.08084577114427868305, 0.08208955223880604057 ),
 .UNSPECIFIED. ) 
 CURVE ( )  GEOMETRIC_REPRESENTATION_ITEM ( )  RATIONAL_B_SPLINE_CURVE ( ( 0.9999999999999924505, 0.8660254037844461461, 1.000000000000000000, 0.8660254037844387076, 1.000000000000000000, 0.8660254037844312691, 1.000000000000007550 ) ) 
 REPRESENTATION_ITEM ( '' )  );
#948 = EDGE_CURVE ( 'NONE', #41544, #2239, #13723, .T. ) ;
#949 = ORIENTED_EDGE ( 'NONE', *, *, #14043, .F. ) ;
#950 = COORDINATED_UNIVERSAL_TIME_OFFSET ( 6, 0, .AHEAD. ) ;
#952 = ORIENTED_EDGE ( 'NONE', *, *, #12475, .F. ) ;
#951 = CARTESIAN_POINT ( 'NONE',  ( -2.293366432827344421E-15, -12.48450537969573659, -109.7187500020483668 ) ) ;
#953 = CARTESIAN_POINT ( 'NONE',  ( -5.000000000000002665, 20.00000000000000000, -235.0000000000000000 ) ) ;
#954 = CARTESIAN_POINT ( 'NONE',  ( 10.81189881249999729, 0.000000000000000000, -193.3437500020484094 ) ) ;
#955 = CARTESIAN_POINT ( 'NONE',  ( 10.81189881249999907, 6.242252689847868297, -35.71875000204835970 ) ) ;
#956 = FACE_OUTER_BOUND ( 'NONE', #6211, .T. ) ;
#957 = CARTESIAN_POINT ( 'NONE',  ( -9.999999999998456346, -5.773502691897145489, -10.50000000409672296 ) ) ;
#958 = CARTESIAN_POINT ( 'NONE',  ( -5.405949406249996869, 9.363379034771805109, -183.8437500020483810 ) ) ;
#959 = CARTESIAN_POINT ( 'NONE',  ( 10.81189881249999551, -6.242252689847874514, -158.9687500020484094 ) ) ;
#960 = LINE ( 'NONE', #1170, #21072 ) ;
#961 = CARTESIAN_POINT ( 'NONE',  ( -2.293366432827344421E-15, -12.48450537969573659, -142.7187500020484094 ) ) ;
#962 = CARTESIAN_POINT ( 'NONE',  ( -10.81189881249999729, 1.324075727343319199E-15, -150.5937500020483810 ) ) ;
#963 = CARTESIAN_POINT ( 'NONE',  ( -4.999999999999996447, 8.660254037844387298, -86.99999999999998579 ) ) ;
#964 = DIRECTION ( 'NONE',  ( -0.000000000000000000, -0.000000000000000000, 1.000000000000000000 ) ) ;
#965 = CARTESIAN_POINT ( 'NONE',  ( -4.999999999999996447, 8.660254037844387298, -181.5000000000000000 ) ) ;
#966 = CARTESIAN_POINT ( 'NONE',  ( 7.644554776091147741E-16, 12.48450537969573659, -87.96875000204838102 ) ) ;
#967 = CARTESIAN_POINT ( 'NONE',  ( -2.275517850991317657E-15, -20.00000000000000000, -235.0000000000000000 ) ) ;
#968 = CARTESIAN_POINT ( 'NONE',  ( -2.293366432827344421E-15, -12.48450537969573659, -66.40625000204838102 ) ) ;
#969 = CARTESIAN_POINT ( 'NONE',  ( 7.070501591499376803E-16, 11.54700538379251284, -168.5000000040967620 ) ) ;
#970 = CARTESIAN_POINT ( 'NONE',  ( -10.81189881249999729, 1.324075727343319199E-15, -182.0937500020483810 ) ) ;
#971 = CARTESIAN_POINT ( 'NONE',  ( 7.644554776091147741E-16, 12.48450537969573659, -121.1562500020483952 ) ) ;
#972 = CARTESIAN_POINT ( 'NONE',  ( -10.81189881249999729, 6.242252689847871849, -158.4062500020483810 ) ) ;
#973 = CARTESIAN_POINT ( 'NONE',  ( 10.81189881249999729, 0.000000000000000000, -49.53125000204838813 ) ) ;
#974 = CARTESIAN_POINT ( 'NONE',  ( -9.999999999999998224, 5.773502691896259087, -132.2500000040967905 ) ) ;
#975 = CARTESIAN_POINT ( 'NONE',  ( -10.00000000000000000, -5.773502691896251982, -110.6249999999999858 ) ) ;
#976 = ORIENTED_EDGE ( 'NONE', *, *, #7502, .F. ) ;
#977 = CARTESIAN_POINT ( 'NONE',  ( -10.81189881249999729, 6.242252689847871849, -132.9062500020483810 ) ) ;
#978 = CARTESIAN_POINT ( 'NONE',  ( 7.070501591499377789E-16, 11.54700538379251284, -146.0000000040967905 ) ) ;
#979 = CARTESIAN_POINT ( 'NONE',  ( -10.81189881249999729, 6.242252689847871849, -147.9062500020483810 ) ) ;
#980 = CARTESIAN_POINT ( 'NONE',  ( -2.293366432827344421E-15, -12.48450537969573659, -184.9062500020484094 ) ) ;
#981 = CARTESIAN_POINT ( 'NONE',  ( 5.405949406249992428, -9.363379034771808662, -85.59375000204836681 ) ) ;
#982 = VERTEX_POINT ( 'NONE', #26410 ) ;
#983 = CARTESIAN_POINT ( 'NONE',  ( 5.000000000000000000, 8.660254037844385522, -48.24999999999998579 ) ) ;
#984 = CARTESIAN_POINT ( 'NONE',  ( -10.81189881249999729, 6.242252689847871849, -180.7187500020483810 ) ) ;
#985 = CARTESIAN_POINT ( 'NONE',  ( 9.999999999999998224, 0.000000000000000000, -56.37500000409676204 ) ) ;
#986 = CARTESIAN_POINT ( 'NONE',  ( -5.000000000000003553, -8.660254037844383745, -179.5000000000000000 ) ) ;
#987 = CARTESIAN_POINT ( 'NONE',  ( -5.000000000000003553, -8.660254037844383745, -158.5000000000000000 ) ) ;
#988 = CARTESIAN_POINT ( 'NONE',  ( 7.644554776091147741E-16, 12.48450537969573659, -74.65625000204838102 ) ) ;
#989 = CARTESIAN_POINT ( 'NONE',  ( 7.644554776091147741E-16, 12.48450537969573659, -62.65625000204838813 ) ) ;
#990 = CARTESIAN_POINT ( 'NONE',  ( 5.000000000000000000, 8.660254037844385522, -51.62500000409675494 ) ) ;
#991 = CARTESIAN_POINT ( 'NONE',  ( -10.81189881249999729, 6.242252689847871849, -12.71875000204836326 ) ) ;
#992 = CYLINDRICAL_SURFACE ( 'NONE', #29713, 9.999999999999998224 ) ;
#993 = CARTESIAN_POINT ( 'NONE',  ( 10.81189881249999551, -6.242252689847874514, -177.1562500020484094 ) ) ;
#994 = CARTESIAN_POINT ( 'NONE',  ( -10.81189881249999729, 1.324075727343319199E-15, -6.781250002048377468 ) ) ;
#995 = LINE ( 'NONE', #11531, #18049 ) ;
#996 = DIRECTION ( 'NONE',  ( 0.000000000000000000, -0.08715574274765837404, -0.9961946980917455452 ) ) ;
#997 = CARTESIAN_POINT ( 'NONE',  ( 5.000000000000000000, 8.660254037844385522, -154.7500000000000000 ) ) ;
#998 = CYLINDRICAL_SURFACE ( 'NONE', #23130, 24.99999999999999645 ) ;
#999 = CARTESIAN_POINT ( 'NONE',  ( -5.000000000000003553, -8.660254037844383745, -122.5000000000000000 ) ) ;
#1000 = EDGE_CURVE ( 'NONE', #28982, #14499, #28136, .T. ) ;
#1002 = VERTEX_POINT ( 'NONE', #35708 ) ;
#1001 = CARTESIAN_POINT ( 'NONE',  ( 5.405949406249992428, -9.363379034771808662, -84.28125000204838102 ) ) ;
#1003 =( LENGTH_UNIT ( ) NAMED_UNIT ( * ) SI_UNIT ( .MILLI., .METRE. ) );
#1005 = EDGE_LOOP ( 'NONE', ( #25428, #30555, #16181, #13108 ) ) ;
#1004 = CARTESIAN_POINT ( 'NONE',  ( -4.999999999999996447, 8.660254037844387298, -80.99999999999998579 ) ) ;
#1006 = ORIENTED_EDGE ( 'NONE', *, *, #30835, .F. ) ;
#1007 = CARTESIAN_POINT ( 'NONE',  ( 5.405949406249992428, -9.363379034771808662, -34.59375000204836681 ) ) ;
#1008 = CARTESIAN_POINT ( 'NONE',  ( -10.81189881249999729, 1.324075727343319199E-15, -27.59375000204836326 ) ) ;
#1009 = CARTESIAN_POINT ( 'NONE',  ( -5.405949406249996869, 9.363379034771805109, -13.03125000204835615 ) ) ;
#1010 = CARTESIAN_POINT ( 'NONE',  ( -2.293366432827344421E-15, -12.48450537969573659, -63.21875000204839523 ) ) ;
#1011 = CARTESIAN_POINT ( 'NONE',  ( 9.999999999999996447, -5.773502691896262640, -42.62499999999997158 ) ) ;
#1012 = CARTESIAN_POINT ( 'NONE',  ( -5.405949406249996869, 9.363379034771805109, -183.8437500020483810 ) ) ;
#1013 = CARTESIAN_POINT ( 'NONE',  ( 10.81189881249999551, -6.242252689847874514, -163.4687500020483810 ) ) ;
#1014 = EDGE_CURVE ( 'NONE', #18719, #21484, #32476, .T. ) ;
#1015 = CARTESIAN_POINT ( 'NONE',  ( 7.070501591499376803E-16, 11.54700538379251284, -175.6250000000000000 ) ) ;
#1016 = CARTESIAN_POINT ( 'NONE',  ( 9.999999999999998224, 0.000000000000000000, -200.0000000000000000 ) ) ;
#1017 = CARTESIAN_POINT ( 'NONE',  ( 4.999999999999992006, -8.660254037844389075, -20.62500000409675494 ) ) ;
#1018 = CARTESIAN_POINT ( 'NONE',  ( 9.999999999999998224, 0.000000000000000000, -200.0000000000000000 ) ) ;
#1019 = CARTESIAN_POINT ( 'NONE',  ( 10.81189881249999729, 0.000000000000000000, -116.8437500020483810 ) ) ;
#1020 = CARTESIAN_POINT ( 'NONE',  ( 0.000000000000000000, 0.000000000000000000, -200.0000000000000000 ) ) ;
#1021 = CARTESIAN_POINT ( 'NONE',  ( 10.81189881249999551, -6.242252689847874514, -88.65625000204838102 ) ) ;
#1022 = CARTESIAN_POINT ( 'NONE',  ( -5.405949406249996869, 9.363379034771805109, -99.84375000204838102 ) ) ;
#1023 = CARTESIAN_POINT ( 'NONE',  ( -10.81189881249999907, -6.242252689847864744, -70.96875000204838102 ) ) ;
#1024 = CARTESIAN_POINT ( 'NONE',  ( -10.81189881249999907, -6.242252689847864744, -80.15625000204839523 ) ) ;
#1025 = CARTESIAN_POINT ( 'NONE',  ( -9.999999999999998224, 1.224646799147353059E-15, -156.1250000040967905 ) ) ;
#1026 = CARTESIAN_POINT ( 'NONE',  ( -10.00000000000000000, -5.773502691896251982, -133.1250000000000000 ) ) ;
#1027 = CARTESIAN_POINT ( 'NONE',  ( -5.405949406250003975, -9.363379034771801557, -156.5312500020484094 ) ) ;
#1028 = CARTESIAN_POINT ( 'NONE',  ( -10.81189881249999907, -6.242252689847864744, -174.6562500020483810 ) ) ;
#1029 = CYLINDRICAL_SURFACE ( 'NONE', #35783, 9.999999999999998224 ) ;
#1030 = CARTESIAN_POINT ( 'NONE',  ( -5.405949406249996869, 9.363379034771805109, -105.8437500020483810 ) ) ;
#1031 = CARTESIAN_POINT ( 'NONE',  ( 9.999999999999998224, 0.000000000000000000, -146.0000000000000000 ) ) ;
#1032 = CARTESIAN_POINT ( 'NONE',  ( 9.999999999999996447, -5.773502691896262640, -75.62499999999998579 ) ) ;
#1033 = CARTESIAN_POINT ( 'NONE',  ( -2.293366432827344421E-15, -12.48450537969573659, -4.906250002048362369 ) ) ;
#1034 = CARTESIAN_POINT ( 'NONE',  ( 5.000000000000000000, 8.660254037844385522, -87.62500000409677625 ) ) ;
#1035 = CARTESIAN_POINT ( 'NONE',  ( 10.81189881249999729, 0.000000000000000000, -100.5312500020483952 ) ) ;
#1036 = CARTESIAN_POINT ( 'NONE',  ( -2.293366432827344421E-15, -12.48450537969573659, -79.90625000204838102 ) ) ;
#1037 = CARTESIAN_POINT ( 'NONE',  ( 7.070501591499377789E-16, 11.54700538379251284, -72.50000000409676204 ) ) ;
#1038 = CARTESIAN_POINT ( 'NONE',  ( -9.999999999999998224, 1.224646799147353059E-15, -200.0000000000000000 ) ) ;
#1039 = CARTESIAN_POINT ( 'NONE',  ( 10.81189881249999907, 6.242252689847868297, -31.21875000204835260 ) ) ;
#1040 = ORIENTED_EDGE ( 'NONE', *, *, #22283, .F. ) ;
#1041 = CARTESIAN_POINT ( 'NONE',  ( -2.121150477449813534E-15, -11.54700538379251284, -3.874999999999953815 ) ) ;
#1042 = CARTESIAN_POINT ( 'NONE',  ( -10.81189881249999729, 6.242252689847871849, -29.40625000204835260 ) ) ;
#1043 = CARTESIAN_POINT ( 'NONE',  ( -10.81189881249999729, 6.242252689847871849, -12.71875000204837569 ) ) ;
#1044 = CYLINDRICAL_SURFACE ( 'NONE', #33100, 9.999999999999998224 ) ;
#1045 = CARTESIAN_POINT ( 'NONE',  ( 5.000000000000000000, 8.660254037844385522, -0.6250000040967651493 ) ) ;
#1046 = CARTESIAN_POINT ( 'NONE',  ( -5.405949406250003975, -9.363379034771801557, -128.0312500020484094 ) ) ;
#1047 = EDGE_CURVE ( 'NONE', #8327, #13549, #2902, .T. ) ;
#1048 = CARTESIAN_POINT ( 'NONE',  ( 10.00000000000000000, 5.773502691896255534, -183.3750000000000000 ) ) ;
#1049 = DIRECTION ( 'NONE',  ( -1.000000000000000000, 0.000000000000000000, 0.000000000000000000 ) ) ;
#1051 = ORIENTED_EDGE ( 'NONE', *, *, #12971, .T. ) ;
#1050 = CARTESIAN_POINT ( 'NONE',  ( 7.644554776091147741E-16, 12.48450537969573659, -113.6562500020483952 ) ) ;
#1052 = CARTESIAN_POINT ( 'NONE',  ( 0.000000000000000000, 0.000000000000000000, -180.0000000000000000 ) ) ;
#1053 = VERTEX_POINT ( 'NONE', #42366 ) ;
#1054 = VERTEX_POINT ( 'NONE', #16453 ) ;
#1055 = CARTESIAN_POINT ( 'NONE',  ( -10.81189881249999729, 6.242252689847871849, -39.90625000204835970 ) ) ;
#1056 = PERSON_AND_ORGANIZATION_ROLE ( 'design_supplier' ) ;
#1057 = CARTESIAN_POINT ( 'NONE',  ( -2.293366432827344421E-15, -12.48450537969573659, -91.71875000204838102 ) ) ;
#1058 = CARTESIAN_POINT ( 'NONE',  ( 0.000000000000000000, 0.000000000000000000, -200.0000000000000000 ) ) ;
#1059 = CARTESIAN_POINT ( 'NONE',  ( -9.999999999999998224, 1.224646799147353059E-15, -200.0000000000000000 ) ) ;
#1060 = VECTOR ( 'NONE', #37117, 1000.000000000000000 ) ;
#1061 = FACE_OUTER_BOUND ( 'NONE', #23770, .T. ) ;
#1062 =( BOUNDED_SURFACE ( )  B_SPLINE_SURFACE ( 1, 2, ( 
 ( #28852, #5971, #23214, #2527, #42619, #26242, #6592, #13048, #16280, #39391, #22790, #19749, #42199, #35952, #29477, #23005, #15652, #16072, #32515, #9618, #12840, #18911, #3151, #2729, #16495, #26446, #41988, #32929, #3362, #29693, #139, #13260, #19534, #39598, #29061, #12417, #6393, #25611, #32094, #32718, #9195, #38974, #22365, #12625, #19122, #9410, #22574, #25819, #35753, #10032, #6181, #32307, #15861, #19320, #2944, #1193, #7660, #39810, #37213, #40026, #10665, #19962, #27300, #20177, #10242, #3787, #20381, #20596, #4206, #33572, #16712, #16921, #3994, #7442, #33999, #24072, #20813, #346, #17138, #30122, #30339, #27516, #4420, #36793, #36578, #17560, #30760, #26660, #24293, #13468, #559, #26871, #768, #14316, #23430, #11090, #10456, #13680, #33367, #23647, #17349, #40436, #7231, #40648, #13894, #27087, #40230, #6807, #33148, #7025, #3578, #23859, #37007, #29907, #10879, #33783, #30553, #980, #14098, #8520, #34856, #21457, #4634, #4850, #8312, #38079, #21890, #11952, #8736, #30977, #34641, #34430, #5067, #15398, #35069, #24721, #24500, #5496, #18646, #14536, #12164, #1406, #17993, #14752, #18215, #31840, #40866, #41726, #27947, #31193, #21244, #41074, #5278, #27730, #28595, #31405, #11737, #15184, #17780, #1623, #2054, #2277, #21028, #11519, #37437, #21673, #37867, #1840, #28381, #7880, #41522, #34218, #11307, #25143, #14966, #37653, #8093, #28164, #41299, #24936, #18431, #31620, #38290, #8947, #6347, #32677, #12997, #19491, #22744, #3106, #29222, #26194, #5924, #42361, #35910, #16234, #22110, #22531, #38930, #32472, #19276, #25356, #9570, #9155, #22961, #32886, #35284, #29434, #42576, #39342, #9781, #36116, #25987, #6549, #35498, #5717, #12794, #18869, #29646, #16026, #32049, #2683, #89, #19075, #28809, #15818, #29014, #32256, #42153, #2896, #38504, #19703, #22323, #3316, #16448, #2478, #15607, #41941, #12374, #25570, #38722, #39138, #12584, #25777, #9362, #35704, #6133, #18116, #4535, #19913, #33319, #31311, #36536, #16662, #3744, #16874, #23386, #30079, #34330, #520, #37767, #37341, #14219, #10200, #8212, #14659, #3526, #1526, #27419, #17677, #26405, #4748, #26617, #29863, #6977, #40555, #27632, #11212, #10999, #23165, #20131, #24193, #14440, #40981, #31093, #27848, #6759, #7787, #20931, #34113, #34544, #11424, #30872, #301, #24619, #21361, #33102, #13211, #13421, #1307, #40771, #24412, #4970, #39766, #39555, #37553, #7991, #21144, #17894, #9986, #36328, #18975, #2169, #25261, #15507, #41192, #1954, #2380, #38617, #14869, #15080, #35396, #8848, #28280, #41417, #28712, #25472, #41838, #9054, #22221, #12276, #5398, #24838, #37985, #8429, #18336, #38195, #11633, #34760, #2590, #28066, #18762, #5820, #32160, #31951, #35181, #15719, #12067, #1743, #18550, #21582, #5182, #31525, #8639, #11853, #25052, #21794, #34974, #31740, #15304, #28501, #41631, #38406, #22006, #5607, #12960, #19453, #25741, #35246, #42536, #22924, #19244, #5461, #18611, #9322, #32221, #2647, #9116, #15360, #35666, #31804, #2235, #12549, #38894, #25320, #28558, #35875, #32011, #26156, #19037, #22287, #22491, #22072, #12334, #6307, #38682, #12129, #41901, #15571, #35458, #5883, #15779, #32643, #9535, #6097, #5678, #15990, #42115, #28977, #2859, #3070, #25533, #41690, #32434, #39306, #2436, #29187, #22706, #16196, #18827, #38466, #29396, #42326, #28772, #8908, #9743, #12752, #25948, #39097, #36498, #265, #23765, #16623, #33060, #3487, #23560, #481, #689, #10578, #10795, #26788, #6723, #29826, #32852, #36079, #26999, #26578, #39728, #6934, #13808, #20089, #10163, #29606, #33697, #36294, #7146, #7362, #13386, #39937, #16835, #16407, #23346, #36920, #10369, #36707, #30036, #33281, #14013, #17052, #20299, #19664, #26368, #13175, #3706, #40150, #3916, #50, #17264, #3280, #4123, #23129, #13596, #33490, #30251, #20511, #39521, #27207, #30468, #896, #40352, #9950, #6515, #19876, #37994, #7572, #34126, #5191, #24632, #4546, #20941, #31321, #8440, #1753, #21591, #34770, #14881, #37562, #17477, #30672, #1102, #24202, #27641, #33915, #40563, #28288, #20726, #4981, #28076, #11645, #18125, #21370, #41205, #27858, #24847, #17687, #40991, #34554, #18347, #4334, #21153, #8004, #31103, #17906, #23984, #8221, #7797, #31534, #1963, #14227, #15092, #41427, #37126, #27429, #11008, #37777, #37351, #30882, #1317, #11434, #14449, #40782, #14670, #11223, #24422, #34340, #4757, #1535, #31959, #2388, #22018, #15516, #32381, #28721, #35823, #35404, #41846, #8859, #6254, #12286, #25481, #28509, #25891, #15727, #25061, #2806, #25270, #15313, #35189, #38627, #25686, #9267, #9063, #21804, #5620, #22232, #12494, #39045, #29135, #9482, #5410, #5829, #18771, #18983, #32591, #22651, #32170, #41640, #19401, #3016, #31750, #29339, #18560, #2599, #28927, #42064, #16139, #12075, #11863, #38839, #22435, #38416, #35614, #2179, #38203, #6042, #19192, #15937, #42270, #12696, #8648, #34983, #39467, #9901, #29984, #6882, #7098, #17001, #17210, #33228, #13118, #23077, #39257, #42481, #33439, #33006, #3435, #36235, #16783, #10320, #3866, #26103, #39674, #13335, #20034, #36448, #12907, #26732, #26317, #40099, #7308, #9690, #30200, #636, #20250, #13752, #23506, #426, #36656, #6667, #22866, #3657, #36029, #4071, #13548, #6466, #19818, #19608, #16571, #3227, #29773, #216, #26525, #10110, #26942, #23286, #23714, #39886, #10531, #36867, #20459, #33647, #32788, #16350, #29550, #31849, #845, #8169, #1050, #33858, #27375, #1268, #1481, #27806, #14393, #40300, #40510, #27589, #31050, #14824, #4926, #1698, #23934, #40727, #10955, #11170, #8388, #28022, #17636, #17424, #41152, #11590, #7521, #5143, #37077, #24151, #7738, #24367, #24798, #4283, #34719, #20885, #37292, #14174, #34071, #40937, #20672, #21539, #37509, #4703, #21317, #10743, #4493, #37726, #37943, #13964, #30830, #30412, #14617, #7952, #21102, #30621, #27159, #34289, #11380, #17854, #24578, #34506, #18076, #31270, #21960, #28238, #5781, #18291, #35775, #25427, #38571, #38154, #41373, #5994, #2128, #38997, #31912, #35140, #9013, #34930, #25220, #19143, #8803, #25012, #12026, #28460, #5565, #18718, #15468, #32331, #22388, #22181, #5351, #28878, #12234, #2339, #15677, #2757, #38365, #31478, #28669, #9433, #15260, #42011, #35566, #15882, #18506, #11809, #29084, #41798, #31696, #8597, #25841, #35352, #12440, #41593, #18935, #32119, #42221, #2550, #25634, #38793, #9219, #12650, #22598, #1911, #15041, #21751, #19555, #3178, #2966, #6207, #6617, #19983, #16093, #22816, #13494, #19770, #39417, #42432, #3811, #6415, #33172, #20199, #16304, #39620, #29718, #29287, #29500, #23453, #23236, #10058, #162, #9850, #26891, #29932, #36396, #32538, #39206, #26055, #32953, #26682, #16733, #12861, #30143, #9643, #16945, #35977, #16520, #3604, #372, #23027, #582, #32740, #42642, #13070, #36179, #26265, #13285, #26471, #13699, #33388, #6827, #39834, #3383, #10267, #36601, #7048, #40045, #10476, #23667, #19351, #41094, #20406, #17800, #1426, #24521, #30997, #17158, #4015, #11326, #10687, #17370, #11110, #4652, #27749, #33594, #34018, #7681, #1214, #30780, #36815, #21046, #20616, #34450, #1641, #30359, #40884, #37672, #14559, #8112, #21264, #37456, #4869, #4229, #790, #40670, #13913, #11535, #27537, #27108, #14119, #7255, #30571, #40251, #27321, #40456, #1001, #10903, #18017, #24092, #31215, #17581, #37233, #33805, #14769, #20833, #4440, #23880, #27965, #24313, #37030, #7467, #14339, #7899, #34238, #38308, #38516, #22124, #8750, #34662, #34873, #21905, #25370, #9165, #41953, #38735, #18232, #35085, #21692, #5510, #2696, #22335, #11967, #11754, #35511, #5938, #1859, #42166, #31422, #5296, #2072, #18660, #19086, #28183, #29027, #15203, #18451, #8540, #28402, #35299, #14985, #15829, #31858, #41743, #2492, #5086, #31638, #32061, #32272, #8332, #41540, #24741, #8960, #25163, #2290, #15620, #37887, #28823, #21479, #41317, #15413, #28609, #12178, #5729, #18881, #12386, #25582, #24955, #38097, #23179, #6561, #3118, #9998, #13432, #6359, #30092, #19503, #3756, #39152, #36339, #29874, #16676, #42373, #22543, #23397, #32688, #26000, #6149, #20146, #39356, #6771, #9582, #13015, #16247, #313, #35921, #22758, #29447, #102, #19717, #19928, #26628, #12595, #3330, #42589, #26205, #9376, #25787, #9795, #26415, #35716, #29233, #33116, #22973, #36129, #19290, #10212, #12807, #39566, #39778, #32897, #16463, #29660, #32483, #13227, #36547, #3541, #6992, #33330, #16888, #38943, #2909, #16040, #26839, #33540, #20351, #27862, #8444, #11650, #36761, #25065, #39990, #11867, #30304, #11439, #41210, #37999, #17910, #38208, #23616, #17104, #3964, #31107, #739, #8225, #24636, #8654, #15096, #21373, #13861, #21807, #18566, #14886, #529, #13648, #4986, #40995, #37781, #4761, #10423, #31325, #7195, #27057, #34557, #18129, #40201, #10632, #31539, #23817, #34988, #14675, #1540, #1757, #36974, #8010, #1970, #34344, #21157, #28082, #5416, #24850, #21595, #34774, #5195, #18351, #28292, #41431, #15317, #41851, #12912, #32385, #12289, #28725, #39049, #3020, #9488, #29344, #16146, #22655, #2603, #25275, #38421, #8863, #31965, #35408, #41645, #5625, #36033, #28513, #12700, #35828, #19405, #25896, #12081, #22025, #6258, #18776, #25485, #6046, #42277, #32596, #35196, #28932, #15731, #38844, #25693, #31754, #15941, #15521, #42485, #39261, #2392, #26108, #9694, #22871, #6470, #2183, #2810, #38633, #9069, #22236, #35618, #5833, #18988, #22440, #32174, #42068, #12498, #9271, #19196, #29138, #10114, #29778, #23294, #40104, #39680, #850, #433, #36452, #16576, #13969, #6886, #20038, #36241, #33654, #23511, #32797, #10535, #33010, #23081, #219, #33233, #33444, #17008, #3660, #29555, #13339, #16788, #20256, #4077, #36872, #17215, #13122, #29987, #26531, #13552, #40306, #30420, #26739, #6674, #27164, #10748, #39471, #37083, #26321, #39893, #10324, #36660, #23939, #19825, #19612, #7102, #3871, #3439, #30205, #641, #13760, #26947, #23721, #7314, #3231, #20465, #16356, #2, #9905, #7527, #34511, #34076, #5148, #15047, #4290, #11597, #24804, #28030, #37949, #31276, #8175, #18081, #17642, #33863, #11388, #1055, #11815, #40942, #14181, #27594, #25017, #30836, #10959, #40734, #11176, #1273, #24372, #41157, #37516, #31484, #31055, #7957, #4498, #1918, #21107, #34294, #24157, #21544, #24584, #20678, #8394, #20892, #37299, #14400, #4710, #21323, #4931, #17860, #17430, #1486, #14624, #1705, #34724, #18297, #28244, #27380, #27812, #37731, #14829, #41378, #30626, #40516, #7743, #6213, #9440, #15266, #12867, #2133, #18725, #15473, #35358, #19358, #41598, #42440, #28674, #31916, #21965, #41803, #35572, #28466, #16100, #18941, #12445, #15888, #5357, #35147, #2762, #22605, #21757, #5571, #32544, #38798, #2346, #12239, #29090, #35781, #42230, #2972, #29293, #12656, #9020, #31702, #12031, #25224, #38370, #25434, #18514, #8809, #38159, #34936, #19148, #25850, #39004, #32337, #38577, #22185, #8603, #5786, #32124, #2556, #15682, #28884, #42018, #25642, #9225, #22394, #5999, #32749, #6625, #3390, #23243, #36821, #29507, #30367, #16527, #19777, #9858, #29725, #23461, #3185, #4021, #6835, #381, #3819, #35986, #23034, #33395, #40053, #9650, #36188, #7262, #26689, #32962, #170, #16953, #10484, #30151, #23674, #20414, #589, #39626, #19562, #16312, #42650, #26272, #13292, #6422, #13077, #797, #22823, #7056, #13707, #26898, #20206, #39425, #26479, #33602, #10065, #36402, #13501, #36608, #17165, #19989, #33180, #3611, #16740, #29940, #26062, #10274, #39842, #39213, #21489, #10694, #18026, #31221, #34457, #1648, #37679, #14567, #24529, #24102, #40257, #17809, #7473, #18240, #4659, #20622, #34026, #31430, #37241, #17378, #4448, #17589, #7688, #30788, #4878, #1222, #37895, #37464, #14347, #10911, #8339, #27545, #40679, #30578, #27974, #31005, #27115, #14778, #27329, #1009, #20843, #11118, #27756, #11335, #24320, #23889, #7907, #21055, #40892, #41101, #11543, #24749, #33812, #34245, #1434, #8119, #34671, #21271, #5094, #13921, #37037, #4236, #14128, #40463, #15835, #22343, #15422, #38105, #8549, #21700, #2079, #5517, #11763, #18458, #6156, #28191, #25588, #9172, #32279, #38743, #24964, #34882, #19096, #31646, #25172, #18889, #12394, #35519, #41325, #41751, #28619, #8966, #38524, #1867, #28830, #28409, #42174, #9386, #5305, #5948, #2704, #29035, #12601, #25795, #2503, #38951, #11977, #15210, #5736, #41547, #19297, #35306, #38316, #21912, #14993, #8757, #35092, #18668, #31865, #2297, #12186, #22551, #25377, #35726, #22131, #32069, #15627, #41961, #6568, #32904, #6367, #3762, #36347, #2918, #10218, #3126, #35927, #29454, #3338, #3550, #29881, #16470, #42383, #42597, #29668, #33123, #16895, #6999 ),
 ( #7204, #13022, #19510, #9801, #22980, #26214, #36136, #23404, #19724, #13654, #13234, #111, #39364, #26845, #26422, #39573, #32695, #30097, #6778, #16048, #36553, #16254, #10006, #23186, #19935, #16685, #321, #13440, #12815, #26635, #39785, #20151, #535, #33341, #39997, #26008, #10430, #23622, #36767, #32491, #29240, #39159, #9590, #22765, #34398, #40208, #37839, #27063, #954, #40407, #17532, #31164, #23828, #24693, #10852, #14072, #4179, #24043, #17748, #10638, #41046, #1163, #37410, #40839, #30311, #17323, #27700, #4818, #3971, #30526, #1595, #21000, #27267, #37184, #11278, #17964, #24473, #14723, #27915, #37622, #33973, #13867, #36981, #7417, #20567, #7631, #745, #33758, #20357, #17111, #1377, #8065, #21214, #14506, #20784, #4392, #11489, #30733, #14287, #7852, #30944, #33546, #27487, #40622, #11062, #24263, #34190, #4608, #35253, #34827, #5890, #15788, #5040, #12342, #25541, #28780, #38690, #32018, #8917, #18185, #5251, #15579, #22295, #34614, #18403, #32229, #22080, #31592, #2024, #41911, #35467, #9123, #19047, #2655, #28985, #21862, #1811, #14938, #28138, #8493, #11924, #31377, #24904, #12555, #41270, #2446, #42123, #25749, #8280, #11708, #38053, #21428, #21646, #15154, #25329, #18838, #28352, #41488, #5468, #35042, #15367, #2247, #25117, #5688, #38261, #8708, #18617, #31814, #28568, #41698, #12136, #38474, #19884, #39527, #6730, #6315, #22500, #58, #32441, #488, #29613, #2867, #16202, #13602, #19462, #42332, #29403, #42545, #32648, #12968, #16632, #26165, #20096, #19671, #39313, #35881, #33290, #9751, #22932, #12763, #10170, #13182, #9332, #29834, #9542, #25957, #3076, #36086, #9958, #36300, #6521, #6105, #32858, #3287, #23136, #23355, #13393, #36506, #15998, #16417, #26375, #33068, #16843, #6944, #3493, #39103, #3715, #30042, #29193, #38903, #22715, #272, #26585, #39735, #35675, #19250, #31112, #17271, #20517, #10585, #4130, #24211, #3923, #4767, #7582, #1110, #4556, #30679, #39946, #17696, #40156, #30258, #23773, #40360, #40573, #37361, #10801, #36713, #36927, #23991, #27437, #11231, #1327, #40790, #20306, #37134, #7370, #20735, #17916, #24430, #14020, #13816, #37573, #8016, #17060, #1546, #33498, #33705, #30476, #33922, #21162, #697, #26796, #904, #27212, #4346, #17486, #7804, #27008, #10377, #14236, #11016, #30890, #7154, #20952, #34135, #34349, #23567, #14458, #27649, #15324, #24855, #11656, #22032, #28732, #35204, #12296, #41859, #5634, #28300, #8231, #21381, #34564, #14892, #18357, #24643, #31332, #18997, #41000, #38428, #18783, #2399, #8870, #37787, #4993, #31971, #1762, #38006, #31762, #25283, #15529, #11444, #11875, #41437, #21814, #8661, #14679, #41652, #41217, #25493, #22244, #18136, #38641, #9077, #35415, #5840, #32181, #28522, #27866, #8451, #28090, #18575, #21601, #34781, #5423, #5201, #31546, #1978, #15103, #25071, #38215, #34995, #2191, #12089, #3825, #26485, #23679, #33185, #39631, #3395, #36826, #10071, #23248, #35626, #26903, #7268, #4027, #10279, #2609, #15739, #39846, #3617, #16744, #36408, #25701, #23466, #28939, #42076, #26694, #36613, #6053, #22449, #10490, #175, #12506, #29944, #387, #7061, #29729, #6841, #20421, #19994, #32968, #13505, #20211, #33400, #16961, #30157, #33609, #38851, #597, #13296, #13714, #40059, #9278, #19204, #16532, #34925, #16456, #5346, #32892, #25007, #9577, #16240, #3113, #28233, #8382, #9789, #18501, #11805, #34713, #6555, #25216, #39146, #38149, #41588, #31690, #29441, #21745, #8592, #2123, #29229, #6141, #6353, #42582, #41146, #32478, #15253, #28454, #37937, #11584, #12020, #12800, #21532, #15035, #19498, #38937, #9368, #5136, #39348, #41368, #25995, #13007, #22538, #2904, #35710, #18283, #19284, #26200, #16033, #42368, #22751, #35917, #19711, #32683, #22968, #24791, #31472, #1905, #36124, #3322, #40196, #23171, #10839, #26412, #40394, #16670, #39985, #27052, #23813, #3749, #24034, #9992, #3534, #33110, #16883, #29867, #36755, #10416, #37173, #942, #7190, #308, #20139, #39772, #33325, #7409, #6983, #7621, #23609, #30086, #26624, #20774, #525, #13641, #13427, #14061, #33537, #95, #20556, #10206, #23392, #36542, #26833, #735, #10626, #20345, #39561, #3959, #17098, #30298, #27254, #4167, #33963, #36334, #13855, #36966, #33746, #4384, #29654, #17312, #30516, #13218, #6765, #19921, #35032, #24250, #40827, #37612, #14715, #28342, #20991, #21853, #8056, #11269, #1366, #21203, #14930, #37400, #38254, #41038, #34603, #38044, #27475, #14497, #24895, #31583, #1151, #27690, #41480, #18176, #24465, #34389, #8486, #2015, #21639, #15146, #11913, #34819, #31154, #11054, #7843, #34178, #17736, #4807, #40611, #4597, #17523, #14274, #41259, #5242, #18395, #11699, #30930, #17955, #25107, #1587, #27904, #5034, #28128, #8700, #11481, #24683, #37829, #8272, #21418, #30724, #1802, #31368, #26003, #19931, #36764, #39359, #39569, #19720, #7200, #39780, #3544, #42376, #6362, #35923, #106, #23400, #26631, #9585, #39993, #12810, #26842, #3121, #26418, #13435, #13017, #16680, #23182, #36550, #33334, #33543, #6774, #29450, #26209, #39154, #16043, #16466, #29877, #22761, #32691, #6995, #29662, #6563, #19506, #13651, #16250, #316, #30094, #9797, #33119, #10001, #42592, #22976, #10215, #20354, #36132, #36342, #32900, #29236, #20148, #3759, #3333, #13230, #16891, #531, #10426, #23619, #40204, #28515, #742, #15319, #33754, #14282, #1374, #40835, #20781, #41647, #27060, #20564, #7414, #33969, #4176, #11059, #27484, #12083, #18569, #24258, #17320, #25278, #22027, #17744, #3968, #17107, #7849, #30731, #1160, #7627, #13864, #34184, #30307, #10635, #37407, #20997, #23821, #36977, #34990, #30523, #38423, #17529, #4389, #4605, #951, #10849, #5418, #37180, #14069, #40402, #27262, #40619, #30938, #14503, #31756, #8657, #27697, #24041, #11869, #25067, #38210, #21809, #2186, #8865, #9907, #42071, #26323, #18990, #3022, #9696, #39263, #22238, #2394, #3233, #28934, #5835, #28727, #4, #19198, #32598, #32176, #35620, #12501, #22875, #15734, #2605, #38636, #9273, #9071, #42279, #2812, #13125, #6472, #12702, #35410, #29557, #35198, #6262, #5628, #18778, #39051, #32388, #15944, #38846, #15523, #22657, #31967, #41854, #25898, #9490, #12291, #25487, #36035, #25695, #39474, #6048, #22442, #35830, #29140, #19408, #19614, #16148, #29346, #42487, #12914, #26110, #32799, #16358, #10750, #27166, #30207, #39682, #33656, #17010, #13554, #20468, #23941, #16790, #40518, #29990, #14183, #6888, #4079, #40308, #37086, #10116, #33012, #33866, #435, #36454, #16578, #30628, #7104, #17217, #20041, #23514, #26741, #7529, #3662, #33236, #39895, #10537, #643, #30422, #20680, #23083, #13762, #10326, #36663, #19827, #36243, #20259, #36874, #3441, #23296, #853, #33446, #3874, #29781, #4292, #26950, #7316, #17432, #40106, #23723, #13971, #221, #13342, #1057, #27382, #6676, #26533, #14627, #31704, #34727, #41159, #37302, #1275, #30838, #37733, #18299, #21547, #4500, #34938, #7746, #21760, #40737, #21325, #8397, #5150, #27814, #5359, #34078, #27597, #34513, #18516, #25019, #31278, #11179, #2135, #28469, #24806, #10962, #24159, #14831, #8177, #4934, #40944, #20894, #11599, #17644, #14402, #18084, #1707, #24374, #37518, #41380, #7959, #15269, #24586, #11390, #28032, #21109, #17862, #11818, #1491, #34296, #4712, #31057, #37951, #31486, #1920, #38161, #15049, #28246, #8606, #9443, #35573, #32126, #39006, #42442, #35361, #16313, #5788, #32750, #25436, #22607, #16102, #2975, #28676, #8811, #9652, #18942, #12242, #35149, #6424, #25643, #35784, #38578, #42020, #2559, #29295, #22188, #9022, #15684, #29093, #6002, #6215, #12869, #41599, #32339, #28887, #12447, #38373, #12033, #38800, #12658, #21967, #15475, #19361, #9227, #22396, #5573, #39215, #41806, #25852, #26064, #19150, #2765, #15890, #18727, #31919, #42232, #19565, #32546, #22825, #35989, #3186, #25226, #2348, #13078, #19779, #6628, #13502, #36822, #40055, #23035, #10696, #26274, #40259, #16529, #39843, #26899, #23675, #3614, #23890, #9861, #3392, #32963, #16742, #29726, #36609, #26482, #16956, #7057, #7264, #4023, #4237, #20207, #172, #39628, #39427, #29509, #29941, #592, #36190, #13293, #20416, #383, #19991, #10067, #27117, #23245, #13710, #799, #36404, #33396, #10276, #6838, #33182, #3820, #7474, #26690, #23462, #30153, #20625, #10486, #33604, #17167, #30369, #13923, #37038, #33813, #42653, #10912, #41326, #14129, #28193, #4449, #27757, #14779, #11544, #34247, #11764, #40464, #34027, #20844, #4660, #17590, #24530, #40893, #24965, #31431, #37680, #30789, #38106, #34883, #31223, #17379, #30579, #21272, #1435, #14568, #21056, #27330, #4879, #1010, #24104, #8120, #34459, #37243, #7689, #5095, #1223, #8550, #31006, #17810, #18027, #14348, #24321, #18241, #7908, #27547, #11119, #40680, #11336, #1649, #27975, #1868, #21490, #41102, #37465, #24750, #37897, #8340, #34672, #14994, #21701, #22766, #12187, #39160, #31866, #15837, #22552, #9387, #35093, #15211, #16050, #41752, #18669, #41548, #12817, #32070, #2705, #2298, #5737, #25378, #35727, #28620, #15423, #25589, #5519, #42384, #5306, #19098, #18459, #31647, #9173, #2504, #15628, #8967, #28410, #35520, #2081, #11978, #12395, #38744, #25174, #38317, #6157, #38525, #26009, #18890, #22133, #22344, #21913, #35307, #19298, #28831, #8758, #41962, #5949, #32280, #29036, #42175, #32492, #2919, #12602, #25796, #38952, #29241, #9591, #33342, #36768, #29670, #10639, #113, #27064, #19725, #3763, #10432, #39999, #22981, #3127, #3972, #13235, #39786, #536, #7205, #13655, #33547, #20358, #26846, #6780, #29455, #42598, #13024, #36137, #39574, #16255, #9802, #40209, #19511, #16896, #23623, #17112, #30098, #26216, #39365, #30312, #6569, #16471, #10219, #746, #13868, #32696, #33125, #19936, #322, #29882, #35928, #20152, #32905, #3339, #6368, #13441, #26423, #10008, #23187, #36348, #3552, #36554, #16686, #26636, #23405, #7001, #17325, #28139, #14508, #30527, #1164, #41272, #4393, #27269, #14288, #27488, #33974, #40623, #1596, #11064, #5041, #4609, #24265, #20786, #18186, #37411, #7853, #21001, #21215, #24694, #17533, #23830, #30734, #14939, #7633, #34399, #41047, #27916, #10853, #33759, #34191, #37185, #1812, #17749, #31378, #30945, #4819, #1378, #27702, #40840, #11490, #11279, #24474, #37624, #8066, #17966, #31166, #37840, #36982, #14724, #8281, #21430, #20568, #7418, #34615, #4180, #955, #40408, #14073, #24044, #2249, #5252, #9333, #11925, #25542, #25750, #21863, #2447, #35255, #34828, #21647, #15580, #32442, #35043, #5690, #15368, #2869, #35468, #41912, #38054, #2025, #31593, #38475, #19048, #22296, #18404, #35676, #8494, #22501, #41490, #22081, #9125, #5891, #28569, #6106, #15155, #28353, #25118, #41699, #38262, #18839, #32019, #19252, #38904, #28781, #8709, #15999, #29194, #38692, #11709, #24906, #12343, #8919, #32230, #12137, #5470, #2656, #18618, #31816, #15790, #28986, #25330, #42125, #12557, #26167, #20308, #13184, #16418, #33069, #16203, #6522, #491, #32859, #6317, #36087, #9753, #29615, #3289, #39528, #30044, #3717, #6731, #29406, #10171, #36301, #39314, #22934, #29836, #19886, #6945, #16846, #17062, #3494, #12969, #19672, #39104, #42333, #59, #13394, #9543, #42546, #20098, #26377, #9959, #35882, #39948, #23137, #26586, #13604, #16634, #273, #39737, #22717, #19464, #23356, #33501, #36508, #33291, #26798, #3925, #10380, #23569, #25958, #32649, #3077, #36716, #7156, #12764, #23776, #11446, #27011, #41002, #17273, #40576, #27651, #24432, #4348, #24646, #10588, #4132, #33707, #17489, #30478, #37363, #11019, #37789, #1548, #7806, #907, #8233, #4997, #1329, #30260, #699, #34139, #14238, #27439, #33924, #40158, #17698, #13818, #36929, #20954, #4558, #7373, #20519, #17918, #14022, #21383, #1112, #30682, #30892, #27216, #37136, #31115, #20737, #40362, #23994, #10803, #24212, #14461, #40792, #14681, #34351, #11233, #7584, #37575, #8020, #21164, #4769, #27868, #34566, #35629, #25073, #9280, #1981, #28734, #35417, #22246, #5204, #28092, #21816, #31548, #38853, #5425, #25703, #2193, #15531, #15105, #18577, #38218, #5842, #41439, #12509, #18138, #31973, #31334, #1765, #22034, #15326, #28524, #34997, #41219, #5636, #14894, #11658, #25285, #38430, #38008, #24857, #18999, #28302, #22451, #31764, #41655, #8872, #34783, #8663, #32183, #12092, #8453, #11877, #35206, #18785, #2401, #41861, #2611, #15741, #12298, #18359, #25495, #38645, #9079, #28941, #42078, #21604, #24110, #12919, #40469, #32605, #17174, #23896, #10701, #35835, #15950, #9703, #19415, #27335, #36041, #14135, #32807, #4028, #3029, #6477, #26114, #37043, #29353, #16156, #42492, #36827, #13133, #13927, #7481, #6055, #39480, #39268, #22882, #2818 ) ),
 .UNSPECIFIED., .F., .F., .F. ) 
 B_SPLINE_SURFACE_WITH_KNOTS ( ( 2, 2 ),
 ( 3, 2, 2, 2, 2, 2, 2, 2, 2, 2, 2, 2, 2, 2, 2, 2, 2, 2, 2, 2, 2, 2, 2, 2, 2, 2, 2, 2, 2, 2, 2, 2, 2, 2, 2, 2, 2, 2, 2, 2, 2, 2, 2, 2, 2, 2, 2, 2, 2, 2, 2, 2, 2, 2, 2, 2, 2, 2, 2, 2, 2, 2, 2, 2, 2, 2, 2, 2, 2, 2, 2, 2, 2, 2, 2, 2, 2, 2, 2, 2, 2, 2, 2, 2, 2, 2, 2, 2, 2, 2, 2, 2, 2, 2, 2, 2, 2, 2, 2, 2, 2, 2, 2, 2, 2, 2, 2, 2, 2, 2, 2, 2, 2, 2, 2, 2, 2, 2, 2, 2, 2, 2, 2, 2, 2, 2, 2, 2, 2, 2, 2, 2, 2, 2, 2, 2, 2, 2, 2, 2, 2, 2, 2, 2, 2, 2, 2, 2, 2, 2, 2, 2, 2, 2, 2, 2, 2, 2, 2, 2, 2, 2, 2, 2, 2, 2, 2, 2, 2, 2, 2, 2, 2, 2, 2, 2, 2, 2, 2, 2, 2, 2, 2, 2, 2, 2, 2, 2, 2, 2, 2, 2, 2, 2, 2, 2, 2, 2, 2, 2, 2, 2, 2, 2, 2, 2, 2, 2, 2, 2, 2, 2, 2, 2, 2, 2, 2, 2, 2, 2, 2, 2, 2, 2, 2, 2, 2, 2, 2, 2, 2, 2, 2, 2, 2, 2, 2, 2, 2, 2, 2, 2, 2, 2, 2, 2, 2, 2, 2, 2, 2, 2, 2, 2, 2, 2, 2, 2, 2, 2, 2, 2, 2, 2, 2, 2, 2, 2, 2, 2, 2, 2, 2, 2, 2, 2, 2, 2, 2, 2, 2, 2, 2, 2, 2, 2, 2, 2, 2, 2, 2, 2, 2, 2, 2, 2, 2, 2, 2, 2, 2, 2, 2, 2, 2, 2, 2, 2, 2, 2, 2, 2, 2, 2, 2, 2, 2, 2, 2, 2, 2, 2, 2, 2, 2, 2, 2, 2, 2, 2, 2, 2, 2, 2, 2, 2, 2, 2, 2, 2, 2, 2, 2, 2, 2, 2, 2, 2, 2, 2, 2, 2, 2, 2, 2, 2, 2, 2, 2, 2, 2, 2, 2, 2, 2, 2, 2, 2, 2, 2, 2, 2, 2, 2, 2, 2, 2, 2, 2, 2, 2, 2, 2, 2, 2, 2, 2, 2, 2, 2, 2, 2, 2, 2, 2, 2, 2, 2, 2, 2, 2, 2, 2, 2, 2, 2, 2, 2, 2, 2, 2, 2, 2, 2, 2, 2, 2, 2, 2, 2, 2, 2, 2, 2, 2, 2, 2, 2, 2, 2, 2, 2, 2, 2, 2, 2, 2, 2, 2, 2, 2, 2, 2, 2, 2, 2, 2, 2, 2, 2, 2, 2, 2, 2, 2, 2, 2, 2, 2, 2, 2, 2, 2, 2, 2, 2, 2, 2, 2, 2, 2, 2, 2, 2, 2, 2, 2, 2, 2, 2, 2, 2, 2, 2, 2, 2, 2, 2, 2, 2, 2, 2, 2, 2, 2, 2, 2, 2, 2, 2, 2, 2, 2, 2, 2, 2, 2, 2, 2, 2, 2, 2, 2, 2, 2, 2, 2, 2, 2, 2, 2, 2, 2, 2, 2, 2, 2, 2, 2, 2, 2, 2, 2, 2, 2, 2, 2, 2, 2, 2, 2, 2, 2, 2, 2, 2, 2, 2, 2, 2, 2, 2, 2, 2, 2, 2, 2, 2, 2, 2, 2, 2, 2, 2, 2, 2, 2, 2, 2, 2, 2, 2, 2, 2, 2, 2, 2, 2, 2, 2, 2, 2, 2, 2, 2, 2, 2, 2, 2, 2, 2, 2, 2, 2, 2, 2, 2, 2, 2, 2, 2, 2, 2, 2, 2, 2, 2, 2, 2, 2, 2, 2, 2, 2, 2, 2, 2, 2, 2, 2, 2, 2, 2, 2, 2, 2, 2, 2, 2, 2, 2, 2, 2, 2, 2, 2, 2, 2, 2, 2, 2, 2, 2, 2, 2, 2, 2, 2, 2, 2, 2, 2, 2, 2, 2, 2, 2, 2, 2, 2, 2, 2, 2, 2, 2, 2, 2, 2, 2, 2, 2, 2, 2, 2, 2, 2, 2, 2, 2, 2, 2, 2, 2, 2, 2, 2, 2, 2, 2, 2, 2, 2, 2, 2, 2, 2, 2, 2, 2, 2, 2, 2, 2, 2, 2, 2, 2, 2, 2, 2, 2, 2, 2, 2, 2, 2, 2, 2, 2, 2, 2, 2, 2, 2, 2, 2, 2, 2, 2, 2, 2, 2, 2, 2, 2, 2, 2, 2, 2, 2, 2, 2, 2, 2, 2, 2, 2, 2, 2, 2, 2, 2, 2, 2, 2, 2, 2, 2, 2, 2, 2, 2, 2, 2, 2, 2, 2, 2, 2, 2, 2, 2, 2, 2, 2, 2, 2, 2, 2, 2, 2, 2, 2, 2, 2, 2, 2, 2, 2, 2, 2, 2, 2, 2, 2, 2, 2, 2, 2, 2, 3 ),
 ( 0.000000000000000000, 1.000000000000000000 ),
 ( 0.000000000000000000, 0.001243781094527363160, 0.002487562189054726321, 0.003731343283582089481, 0.004975124378109452641, 0.006218905472636816235, 0.007462686567164178962, 0.008706467661691542556, 0.009950248756218905283, 0.01119402985074626801, 0.01243781094527363247, 0.01368159203980099520, 0.01492537313432835792, 0.01616915422885572065, 0.01741293532338308511, 0.01865671641791044610, 0.01990049751243781057, 0.02114427860696517503, 0.02238805970149253602, 0.02363184079601990048, 0.02487562189054726494, 0.02611940298507462593, 0.02736318407960199039, 0.02860696517412935486, 0.02985074626865671585, 0.03109452736318408031, 0.03233830845771144130, 0.03358208955223880576, 0.03482587064676617022, 0.03606965174129353469, 0.03731343283582089221, 0.03855721393034825667, 0.03980099502487562113, 0.04104477611940298559, 0.04228855721393035005, 0.04353233830845771452, 0.04477611940298507204, 0.04601990049751243650, 0.04726368159203980096, 0.04850746268656716542, 0.04975124378109452988, 0.05099502487562188741, 0.05223880597014925187, 0.05348258706467661633, 0.05472636815920398079, 0.05597014925373134525, 0.05721393034825870971, 0.05845771144278606724, 0.05970149253731343170, 0.06094527363184079616, 0.06218905472636816062, 0.06343283582089552508, 0.06467661691542288260, 0.06592039800995025400, 0.06716417910447761153, 0.06840796019900496905, 0.06965174129353234045, 0.07089552238805969797, 0.07213930348258706937, 0.07338308457711442689, 0.07462686567164178442, 0.07587064676616915582, 0.07711442786069651334, 0.07835820895522388474, 0.07960199004975124226, 0.08084577114427861366, 0.08208955223880597118, 0.08333333333333332871, 0.08457711442786070011, 0.08582089552238805763, 0.08706467661691542903, 0.08830845771144278655, 0.08955223880597014408, 0.09079601990049751548, 0.09203980099502487300, 0.09328358208955224440, 0.09452736318407960192, 0.09577114427860695944, 0.09701492537313433084, 0.09825870646766168837, 0.09950248756218905977, 0.1007462686567164173, 0.1019900497512437748, 0.1032338308457711462, 0.1044776119402985037, 0.1057213930348258751, 0.1069651741293532327, 0.1082089552238805902, 0.1094527363184079616, 0.1106965174129353191, 0.1119402985074626905, 0.1131840796019900480, 0.1144278606965174194, 0.1156716417910447769, 0.1169154228855721345, 0.1181592039800995059, 0.1194029850746268634, 0.1206467661691542348, 0.1218905472636815923, 0.1231343283582089498, 0.1243781094527363212, 0.1256218905472636926, 0.1268656716417910502, 0.1281094527363184077, 0.1293532338308457652, 0.1305970149253731227, 0.1318407960199005080, 0.1330845771144278655, 0.1343283582089552231, 0.1355721393034825806, 0.1368159203980099381, 0.1380597014925373234, 0.1393034825870646809, 0.1405472636815920384, 0.1417910447761193959, 0.1430348258706467535, 0.1442786069651741387, 0.1455223880597014963, 0.1467661691542288538, 0.1480099502487562113, 0.1492537313432835688, 0.1504975124378109541, 0.1517412935323383116, 0.1529850746268656692, 0.1542288557213930267, 0.1554726368159203842, 0.1567164179104477695, 0.1579601990049751270, 0.1592039800995024845, 0.1604477611940298420, 0.1616915422885572273, 0.1629353233830845848, 0.1641791044776119424, 0.1654228855721392999, 0.1666666666666666574, 0.1679104477611940427, 0.1691542288557214002, 0.1703980099502487577, 0.1716417910447761153, 0.1728855721393034728, 0.1741293532338308581, 0.1753731343283582156, 0.1766169154228855731, 0.1778606965174129306, 0.1791044776119402882, 0.1803482587064676734, 0.1815920398009950310, 0.1828358208955223885, 0.1840796019900497460, 0.1853233830845771035, 0.1865671641791044888, 0.1878109452736318463, 0.1890547263681592038, 0.1902985074626865614, 0.1915422885572139189, 0.1927860696517413042, 0.1940298507462686617, 0.1952736318407960192, 0.1965174129353233767, 0.1977611940298507343, 0.1990049751243781195, 0.2002487562189054771, 0.2014925373134328346, 0.2027363184079601921, 0.2039800995024875496, 0.2052238805970149349, 0.2064676616915422924, 0.2077114427860696499, 0.2089552238805970075, 0.2101990049751243650, 0.2114427860696517503, 0.2126865671641791078, 0.2139303482587064653, 0.2151741293532338228, 0.2164179104477611804, 0.2176616915422885656, 0.2189054726368159232, 0.2201492537313432807, 0.2213930348258706382, 0.2226368159203980235, 0.2238805970149253810, 0.2251243781094527385, 0.2263681592039800961, 0.2276119402985074536, 0.2288557213930348389, 0.2300995024875621964, 0.2313432835820895539, 0.2325870646766169114, 0.2338308457711442689, 0.2350746268656716542, 0.2363184079601990117, 0.2375621890547263693, 0.2388059701492537268, 0.2400497512437810843, 0.2412935323383084696, 0.2425373134328358271, 0.2437810945273631846, 0.2450248756218905422, 0.2462686567164178997, 0.2475124378109452850, 0.2487562189054726425, 0.2500000000000000000, 0.2512437810945273853, 0.2524875621890547150, 0.2537313432835821003, 0.2549751243781094301, 0.2562189054726368154, 0.2574626865671642006, 0.2587064676616915304, 0.2599502487562189157, 0.2611940298507462455, 0.2624378109452736307, 0.2636815920398010160, 0.2649253731343283458, 0.2661691542288557311, 0.2674129353233830608, 0.2686567164179104461, 0.2699004975124378314, 0.2711442786069651611, 0.2723880597014925464, 0.2736318407960198762, 0.2748756218905472615, 0.2761194029850746468, 0.2773631840796019765, 0.2786069651741293618, 0.2798507462686566916, 0.2810945273631840768, 0.2823383084577114621, 0.2835820895522387919, 0.2848258706467661772, 0.2860696517412935069, 0.2873134328358208922, 0.2885572139303482775, 0.2898009950248756073, 0.2910447761194029925, 0.2922885572139303223, 0.2935323383084577076, 0.2947761194029850929, 0.2960199004975124226, 0.2972636815920398079, 0.2985074626865671377, 0.2997512437810945229, 0.3009950248756219082, 0.3022388059701492380, 0.3034825870646766233, 0.3047263681592039530, 0.3059701492537313383, 0.3072139303482587236, 0.3084577114427860534, 0.3097014925373134386, 0.3109452736318407684, 0.3121890547263681537, 0.3134328358208955390, 0.3146766169154228687, 0.3159203980099502540, 0.3171641791044776393, 0.3184079601990049690, 0.3196517412935323543, 0.3208955223880596841, 0.3221393034825870694, 0.3233830845771144546, 0.3246268656716417844, 0.3258706467661691697, 0.3271144278606964995, 0.3283582089552238847, 0.3296019900497512700, 0.3308457711442785998, 0.3320895522388059851, 0.3333333333333333148, 0.3345771144278607001, 0.3358208955223880854, 0.3370646766169154152, 0.3383084577114428004, 0.3395522388059701302, 0.3407960199004975155, 0.3420398009950249008, 0.3432835820895522305, 0.3445273631840796158, 0.3457711442786069456, 0.3470149253731343308, 0.3482587064676617161, 0.3495024875621890459, 0.3507462686567164312, 0.3519900497512437609, 0.3532338308457711462, 0.3544776119402985315, 0.3557213930348258613, 0.3569651741293532465, 0.3582089552238805763, 0.3594527363184079616, 0.3606965174129353469, 0.3619402985074626766, 0.3631840796019900619, 0.3644278606965173917, 0.3656716417910447769, 0.3669154228855721622, 0.3681592039800994920, 0.3694029850746268773, 0.3706467661691542070, 0.3718905472636815923, 0.3731343283582089776, 0.3743781094527363074, 0.3756218905472636926, 0.3768656716417910224, 0.3781094527363184077, 0.3793532338308457930, 0.3805970149253731227, 0.3818407960199005080, 0.3830845771144278378, 0.3843283582089552231, 0.3855721393034826083, 0.3868159203980099381, 0.3880597014925373234, 0.3893034825870646531, 0.3905472636815920384, 0.3917910447761194237, 0.3930348258706467535, 0.3942786069651741387, 0.3955223880597014685, 0.3967661691542288538, 0.3980099502487562391, 0.3992537313432835688, 0.4004975124378109541, 0.4017412935323382839, 0.4029850746268656692, 0.4042288557213930544, 0.4054726368159203842, 0.4067164179104477695, 0.4079601990049750992, 0.4092039800995024845, 0.4104477611940298698, 0.4116915422885571996, 0.4129353233830845848, 0.4141791044776119146, 0.4154228855721392999, 0.4166666666666666852, 0.4179104477611940149, 0.4191542288557214002, 0.4203980099502487300, 0.4216417910447761153, 0.4228855721393035005, 0.4241293532338308303, 0.4253731343283582156, 0.4266169154228855454, 0.4278606965174129306, 0.4291044776119403159, 0.4303482587064676457, 0.4315920398009950310, 0.4328358208955223607, 0.4340796019900497460, 0.4353233830845771313, 0.4365671641791044610, 0.4378109452736318463, 0.4390547263681592316, 0.4402985074626865614, 0.4415422885572139466, 0.4427860696517412764, 0.4440298507462686617, 0.4452736318407960470, 0.4465174129353233767, 0.4477611940298507620, 0.4490049751243780918, 0.4502487562189054771, 0.4514925373134328623, 0.4527363184079601921, 0.4539800995024875774, 0.4552238805970149071, 0.4564676616915422924, 0.4577114427860696777, 0.4589552238805970075, 0.4601990049751243927, 0.4614427860696517225, 0.4626865671641791078, 0.4639303482587064931, 0.4651741293532338228, 0.4664179104477612081, 0.4676616915422885379, 0.4689054726368159232, 0.4701492537313433084, 0.4713930348258706382, 0.4726368159203980235, 0.4738805970149253532, 0.4751243781094527385, 0.4763681592039801238, 0.4776119402985074536, 0.4788557213930348389, 0.4800995024875621686, 0.4813432835820895539, 0.4825870646766169392, 0.4838308457711442689, 0.4850746268656716542, 0.4863184079601989840, 0.4875621890547263693, 0.4888059701492537545, 0.4900497512437810843, 0.4912935323383084696, 0.4925373134328357994, 0.4937810945273631846, 0.4950248756218905699, 0.4962686567164178997, 0.4975124378109452850, 0.4987562189054726147, 0.5000000000000000000, 0.5012437810945273853, 0.5024875621890547706, 0.5037313432835820448, 0.5049751243781094301, 0.5062189054726368154, 0.5074626865671642006, 0.5087064676616915859, 0.5099502487562188602, 0.5111940298507462455, 0.5124378109452736307, 0.5136815920398010160, 0.5149253731343284013, 0.5161691542288556755, 0.5174129353233830608, 0.5186567164179104461, 0.5199004975124378314, 0.5211442786069652167, 0.5223880597014924909, 0.5236318407960198762, 0.5248756218905472615, 0.5261194029850746468, 0.5273631840796020320, 0.5286069651741293063, 0.5298507462686566916, 0.5310945273631840768, 0.5323383084577114621, 0.5335820895522388474, 0.5348258706467661217, 0.5360696517412935069, 0.5373134328358208922, 0.5385572139303482775, 0.5398009950248756628, 0.5410447761194029370, 0.5422885572139303223, 0.5435323383084577076, 0.5447761194029850929, 0.5460199004975124781, 0.5472636815920397524, 0.5485074626865671377, 0.5497512437810945229, 0.5509950248756219082, 0.5522388059701492935, 0.5534825870646765678, 0.5547263681592039530, 0.5559701492537313383, 0.5572139303482587236, 0.5584577114427861089, 0.5597014925373133831, 0.5609452736318407684, 0.5621890547263681537, 0.5634328358208955390, 0.5646766169154229242, 0.5659203980099501985, 0.5671641791044775838, 0.5684079601990049690, 0.5696517412935323543, 0.5708955223880597396, 0.5721393034825870139, 0.5733830845771143991, 0.5746268656716417844, 0.5758706467661691697, 0.5771144278606965550, 0.5783582089552238292, 0.5796019900497512145, 0.5808457711442785998, 0.5820895522388059851, 0.5833333333333333703, 0.5845771144278606446, 0.5858208955223880299, 0.5870646766169154152, 0.5883084577114428004, 0.5895522388059701857, 0.5907960199004974600, 0.5920398009950248452, 0.5932835820895522305, 0.5945273631840796158, 0.5957711442786070011, 0.5970149253731342753, 0.5982587064676616606, 0.5995024875621890459, 0.6007462686567164312, 0.6019900497512438164, 0.6032338308457710907, 0.6044776119402984760, 0.6057213930348258613, 0.6069651741293532465, 0.6082089552238806318, 0.6094527363184079061, 0.6106965174129352913, 0.6119402985074626766, 0.6131840796019900619, 0.6144278606965174472, 0.6156716417910447214, 0.6169154228855721067, 0.6181592039800994920, 0.6194029850746268773, 0.6206467661691542625, 0.6218905472636815368, 0.6231343283582089221, 0.6243781094527363074, 0.6256218905472636926, 0.6268656716417910779, 0.6281094527363184632, 0.6293532338308457375, 0.6305970149253731227, 0.6318407960199005080, 0.6330845771144278933, 0.6343283582089552786, 0.6355721393034825528, 0.6368159203980099381, 0.6380597014925373234, 0.6393034825870647087, 0.6405472636815920939, 0.6417910447761193682, 0.6430348258706467535, 0.6442786069651741387, 0.6455223880597015240, 0.6467661691542289093, 0.6480099502487561836, 0.6492537313432835688, 0.6504975124378109541, 0.6517412935323383394, 0.6529850746268657247, 0.6542288557213929989, 0.6554726368159203842, 0.6567164179104477695, 0.6579601990049751548, 0.6592039800995025400, 0.6604477611940298143, 0.6616915422885571996, 0.6629353233830845848, 0.6641791044776119701, 0.6654228855721393554, 0.6666666666666666297, 0.6679104477611940149, 0.6691542288557214002, 0.6703980099502487855, 0.6716417910447761708, 0.6728855721393034450, 0.6741293532338308303, 0.6753731343283582156, 0.6766169154228856009, 0.6778606965174129861, 0.6791044776119402604, 0.6803482587064676457, 0.6815920398009950310, 0.6828358208955224162, 0.6840796019900498015, 0.6853233830845770758, 0.6865671641791044610, 0.6878109452736318463, 0.6890547263681592316, 0.6902985074626866169, 0.6915422885572138911, 0.6927860696517412764, 0.6940298507462686617, 0.6952736318407960470, 0.6965174129353234322, 0.6977611940298507065, 0.6990049751243780918, 0.7002487562189054771, 0.7014925373134328623, 0.7027363184079602476, 0.7039800995024875219, 0.7052238805970149071, 0.7064676616915422924, 0.7077114427860696777, 0.7089552238805970630, 0.7101990049751243372, 0.7114427860696517225, 0.7126865671641791078, 0.7139303482587064931, 0.7151741293532338783, 0.7164179104477611526, 0.7176616915422885379, 0.7189054726368159232, 0.7201492537313433084, 0.7213930348258706937, 0.7226368159203979680, 0.7238805970149253532, 0.7251243781094527385, 0.7263681592039801238, 0.7276119402985075091, 0.7288557213930347833, 0.7300995024875621686, 0.7313432835820895539, 0.7325870646766169392, 0.7338308457711443245, 0.7350746268656715987, 0.7363184079601989840, 0.7375621890547263693, 0.7388059701492537545, 0.7400497512437811398, 0.7412935323383084141, 0.7425373134328357994, 0.7437810945273631846, 0.7450248756218905699, 0.7462686567164179552, 0.7475124378109452294, 0.7487562189054726147, 0.7500000000000000000, 0.7512437810945273853, 0.7524875621890547706, 0.7537313432835820448, 0.7549751243781094301, 0.7562189054726368154, 0.7574626865671642006, 0.7587064676616915859, 0.7599502487562188602, 0.7611940298507462455, 0.7624378109452736307, 0.7636815920398010160, 0.7649253731343284013, 0.7661691542288556755, 0.7674129353233830608, 0.7686567164179104461, 0.7699004975124378314, 0.7711442786069652167, 0.7723880597014924909, 0.7736318407960198762, 0.7748756218905472615, 0.7761194029850746468, 0.7773631840796020320, 0.7786069651741293063, 0.7798507462686566916, 0.7810945273631840768, 0.7823383084577114621, 0.7835820895522388474, 0.7848258706467661217, 0.7860696517412935069, 0.7873134328358208922, 0.7885572139303482775, 0.7898009950248756628, 0.7910447761194029370, 0.7922885572139303223, 0.7935323383084577076, 0.7947761194029850929, 0.7960199004975124781, 0.7972636815920397524, 0.7985074626865671377, 0.7997512437810945229, 0.8009950248756219082, 0.8022388059701492935, 0.8034825870646765678, 0.8047263681592039530, 0.8059701492537313383, 0.8072139303482587236, 0.8084577114427861089, 0.8097014925373133831, 0.8109452736318407684, 0.8121890547263681537, 0.8134328358208955390, 0.8146766169154229242, 0.8159203980099501985, 0.8171641791044775838, 0.8184079601990049690, 0.8196517412935323543, 0.8208955223880597396, 0.8221393034825870139, 0.8233830845771143991, 0.8246268656716417844, 0.8258706467661691697, 0.8271144278606965550, 0.8283582089552238292, 0.8296019900497512145, 0.8308457711442785998, 0.8320895522388059851, 0.8333333333333333703, 0.8345771144278606446, 0.8358208955223880299, 0.8370646766169154152, 0.8383084577114428004, 0.8395522388059701857, 0.8407960199004974600, 0.8420398009950248452, 0.8432835820895522305, 0.8445273631840796158, 0.8457711442786070011, 0.8470149253731342753, 0.8482587064676616606, 0.8495024875621890459, 0.8507462686567164312, 0.8519900497512438164, 0.8532338308457710907, 0.8544776119402984760, 0.8557213930348258613, 0.8569651741293532465, 0.8582089552238806318, 0.8594527363184079061, 0.8606965174129352913, 0.8619402985074626766, 0.8631840796019900619, 0.8644278606965174472, 0.8656716417910447214, 0.8669154228855721067, 0.8681592039800994920, 0.8694029850746268773, 0.8706467661691542625, 0.8718905472636815368, 0.8731343283582089221, 0.8743781094527363074, 0.8756218905472636926, 0.8768656716417910779, 0.8781094527363184632, 0.8793532338308457375, 0.8805970149253731227, 0.8818407960199005080, 0.8830845771144278933, 0.8843283582089552786, 0.8855721393034825528, 0.8868159203980099381, 0.8880597014925373234, 0.8893034825870647087, 0.8905472636815920939, 0.8917910447761193682, 0.8930348258706467535, 0.8942786069651741387, 0.8955223880597015240, 0.8967661691542289093, 0.8980099502487561836, 0.8992537313432835688, 0.9004975124378109541, 0.9017412935323383394, 0.9029850746268657247, 0.9042288557213929989, 0.9054726368159203842, 0.9067164179104477695, 0.9079601990049751548, 0.9092039800995025400, 0.9104477611940298143, 0.9116915422885571996, 0.9129353233830845848, 0.9141791044776119701, 0.9154228855721393554, 0.9166666666666666297, 0.9179104477611940149, 0.9191542288557214002, 0.9203980099502487855, 0.9216417910447761708, 0.9228855721393034450, 0.9241293532338308303, 0.9253731343283582156, 0.9266169154228856009, 0.9278606965174129861, 0.9291044776119402604, 0.9303482587064676457, 0.9315920398009950310, 0.9328358208955224162, 0.9340796019900498015, 0.9353233830845770758, 0.9365671641791044610, 0.9378109452736318463, 0.9390547263681592316, 0.9402985074626866169, 0.9415422885572138911, 0.9427860696517412764, 0.9440298507462686617, 0.9452736318407960470, 0.9465174129353234322, 0.9477611940298507065, 0.9490049751243780918, 0.9502487562189054771, 0.9514925373134328623, 0.9527363184079602476, 0.9539800995024875219, 0.9552238805970149071, 0.9564676616915422924, 0.9577114427860696777, 0.9589552238805970630, 0.9601990049751243372, 0.9614427860696517225, 0.9626865671641791078, 0.9639303482587064931, 0.9651741293532338783, 0.9664179104477611526, 0.9676616915422885379, 0.9689054726368159232, 0.9701492537313433084, 0.9713930348258706937, 0.9726368159203979680, 0.9738805970149253532, 0.9751243781094527385, 0.9763681592039801238, 0.9776119402985075091, 0.9788557213930347833, 0.9800995024875621686, 0.9813432835820895539, 0.9825870646766169392, 0.9838308457711443245, 0.9850746268656715987, 0.9863184079601989840, 0.9875621890547263693, 0.9888059701492537545, 0.9900497512437811398, 0.9912935323383084141, 0.9925373134328357994, 0.9937810945273631846, 0.9950248756218905699 ),
 .UNSPECIFIED. ) 
 GEOMETRIC_REPRESENTATION_ITEM ( )  RATIONAL_B_SPLINE_SURFACE ( (
 ( 1.000000000000000000, 0.8660254037844387076, 1.000000000000000000, 0.8660254037844387076, 1.000000000000000000, 0.8660254037844387076, 1.000000000000000000, 0.8660254037844387076, 1.000000000000000000, 0.8660254037844387076, 1.000000000000000000, 0.8660254037844387076, 1.000000000000000000, 0.8660254037844387076, 1.000000000000000000, 0.8660254037844387076, 1.000000000000000000, 0.8660254037844387076, 1.000000000000000000, 0.8660254037844387076, 1.000000000000000000, 0.8660254037844387076, 1.000000000000000000, 0.8660254037844387076, 1.000000000000000000, 0.8660254037844387076, 1.000000000000000000, 0.8660254037844387076, 1.000000000000000000, 0.8660254037844387076, 1.000000000000000000, 0.8660254037844387076, 1.000000000000000000, 0.8660254037844387076, 1.000000000000000000, 0.8660254037844387076, 1.000000000000000000, 0.8660254037844387076, 1.000000000000000000, 0.8660254037844387076, 1.000000000000000000, 0.8660254037844387076, 1.000000000000000000, 0.8660254037844387076, 1.000000000000000000, 0.8660254037844387076, 1.000000000000000000, 0.8660254037844387076, 1.000000000000000000, 0.8660254037844387076, 1.000000000000000000, 0.8660254037844387076, 1.000000000000000000, 0.8660254037844387076, 1.000000000000000000, 0.8660254037844387076, 1.000000000000000000, 0.8660254037844387076, 1.000000000000000000, 0.8660254037844387076, 1.000000000000000000, 0.8660254037844387076, 1.000000000000000000, 0.8660254037844387076, 1.000000000000000000, 0.8660254037844387076, 1.000000000000000000, 0.8660254037844387076, 1.000000000000000000, 0.8660254037844387076, 1.000000000000000000, 0.8660254037844387076, 1.000000000000000000, 0.8660254037844387076, 1.000000000000000000, 0.8660254037844387076, 1.000000000000000000, 0.8660254037844387076, 1.000000000000000000, 0.8660254037844387076, 1.000000000000000000, 0.8660254037844387076, 1.000000000000000000, 0.8660254037844387076, 1.000000000000000000, 0.8660254037844387076, 1.000000000000000000, 0.8660254037844387076, 1.000000000000000000, 0.8660254037844387076, 1.000000000000000000, 0.8660254037844387076, 1.000000000000000000, 0.8660254037844387076, 1.000000000000000000, 0.8660254037844387076, 1.000000000000000000, 0.8660254037844387076, 1.000000000000000000, 0.8660254037844387076, 1.000000000000000000, 0.8660254037844387076, 1.000000000000000000, 0.8660254037844387076, 1.000000000000000000, 0.8660254037844387076, 1.000000000000000000, 0.8660254037844387076, 1.000000000000000000, 0.8660254037844387076, 1.000000000000000000, 0.8660254037844387076, 1.000000000000000000, 0.8660254037844387076, 1.000000000000000000, 0.8660254037844387076, 1.000000000000000000, 0.8660254037844387076, 1.000000000000000000, 0.8660254037844387076, 1.000000000000000000, 0.8660254037844387076, 1.000000000000000000, 0.8660254037844387076, 1.000000000000000000, 0.8660254037844387076, 1.000000000000000000, 0.8660254037844387076, 1.000000000000000000, 0.8660254037844387076, 1.000000000000000000, 0.8660254037844387076, 1.000000000000000000, 0.8660254037844387076, 1.000000000000000000, 0.8660254037844387076, 1.000000000000000000, 0.8660254037844387076, 1.000000000000000000, 0.8660254037844387076, 1.000000000000000000, 0.8660254037844387076, 1.000000000000000000, 0.8660254037844387076, 1.000000000000000000, 0.8660254037844387076, 1.000000000000000000, 0.8660254037844387076, 1.000000000000000000, 0.8660254037844387076, 1.000000000000000000, 0.8660254037844387076, 1.000000000000000000, 0.8660254037844387076, 1.000000000000000000, 0.8660254037844387076, 1.000000000000000000, 0.8660254037844387076, 1.000000000000000000, 0.8660254037844387076, 1.000000000000000000, 0.8660254037844387076, 1.000000000000000000, 0.8660254037844387076, 1.000000000000000000, 0.8660254037844387076, 1.000000000000000000, 0.8660254037844387076, 1.000000000000000000, 0.8660254037844387076, 1.000000000000000000, 0.8660254037844387076, 1.000000000000000000, 0.8660254037844387076, 1.000000000000000000, 0.8660254037844387076, 1.000000000000000000, 0.8660254037844387076, 1.000000000000000000, 0.8660254037844387076, 1.000000000000000000, 0.8660254037844387076, 1.000000000000000000, 0.8660254037844387076, 1.000000000000000000, 0.8660254037844387076, 1.000000000000000000, 0.8660254037844387076, 1.000000000000000000, 0.8660254037844387076, 1.000000000000000000, 0.8660254037844387076, 1.000000000000000000, 0.8660254037844387076, 1.000000000000000000, 0.8660254037844387076, 1.000000000000000000, 0.8660254037844387076, 1.000000000000000000, 0.8660254037844387076, 1.000000000000000000, 0.8660254037844387076, 1.000000000000000000, 0.8660254037844387076, 1.000000000000000000, 0.8660254037844387076, 1.000000000000000000, 0.8660254037844387076, 1.000000000000000000, 0.8660254037844387076, 1.000000000000000000, 0.8660254037844387076, 1.000000000000000000, 0.8660254037844387076, 1.000000000000000000, 0.8660254037844387076, 1.000000000000000000, 0.8660254037844387076, 1.000000000000000000, 0.8660254037844387076, 1.000000000000000000, 0.8660254037844387076, 1.000000000000000000, 0.8660254037844387076, 1.000000000000000000, 0.8660254037844387076, 1.000000000000000000, 0.8660254037844387076, 1.000000000000000000, 0.8660254037844387076, 1.000000000000000000, 0.8660254037844387076, 1.000000000000000000, 0.8660254037844387076, 1.000000000000000000, 0.8660254037844387076, 1.000000000000000000, 0.8660254037844387076, 1.000000000000000000, 0.8660254037844387076, 1.000000000000000000, 0.8660254037844387076, 1.000000000000000000, 0.8660254037844387076, 1.000000000000000000, 0.8660254037844387076, 1.000000000000000000, 0.8660254037844387076, 1.000000000000000000, 0.8660254037844387076, 1.000000000000000000, 0.8660254037844387076, 1.000000000000000000, 0.8660254037844387076, 1.000000000000000000, 0.8660254037844387076, 1.000000000000000000, 0.8660254037844387076, 1.000000000000000000, 0.8660254037844387076, 1.000000000000000000, 0.8660254037844387076, 1.000000000000000000, 0.8660254037844387076, 1.000000000000000000, 0.8660254037844387076, 1.000000000000000000, 0.8660254037844387076, 1.000000000000000000, 0.8660254037844387076, 1.000000000000000000, 0.8660254037844387076, 1.000000000000000000, 0.8660254037844387076, 1.000000000000000000, 0.8660254037844387076, 1.000000000000000000, 0.8660254037844387076, 1.000000000000000000, 0.8660254037844387076, 1.000000000000000000, 0.8660254037844387076, 1.000000000000000000, 0.8660254037844387076, 1.000000000000000000, 0.8660254037844387076, 1.000000000000000000, 0.8660254037844387076, 1.000000000000000000, 0.8660254037844387076, 1.000000000000000000, 0.8660254037844387076, 1.000000000000000000, 0.8660254037844387076, 1.000000000000000000, 0.8660254037844387076, 1.000000000000000000, 0.8660254037844387076, 1.000000000000000000, 0.8660254037844387076, 1.000000000000000000, 0.8660254037844387076, 1.000000000000000000, 0.8660254037844387076, 1.000000000000000000, 0.8660254037844387076, 1.000000000000000000, 0.8660254037844387076, 1.000000000000000000, 0.8660254037844387076, 1.000000000000000000, 0.8660254037844387076, 1.000000000000000000, 0.8660254037844387076, 1.000000000000000000, 0.8660254037844387076, 1.000000000000000000, 0.8660254037844387076, 1.000000000000000000, 0.8660254037844387076, 1.000000000000000000, 0.8660254037844387076, 1.000000000000000000, 0.8660254037844387076, 1.000000000000000000, 0.8660254037844387076, 1.000000000000000000, 0.8660254037844387076, 1.000000000000000000, 0.8660254037844387076, 1.000000000000000000, 0.8660254037844387076, 1.000000000000000000, 0.8660254037844387076, 1.000000000000000000, 0.8660254037844387076, 1.000000000000000000, 0.8660254037844387076, 1.000000000000000000, 0.8660254037844387076, 1.000000000000000000, 0.8660254037844387076, 1.000000000000000000, 0.8660254037844387076, 1.000000000000000000, 0.8660254037844387076, 1.000000000000000000, 0.8660254037844387076, 1.000000000000000000, 0.8660254037844387076, 1.000000000000000000, 0.8660254037844387076, 1.000000000000000000, 0.8660254037844387076, 1.000000000000000000, 0.8660254037844387076, 1.000000000000000000, 0.8660254037844387076, 1.000000000000000000, 0.8660254037844387076, 1.000000000000000000, 0.8660254037844387076, 1.000000000000000000, 0.8660254037844387076, 1.000000000000000000, 0.8660254037844387076, 1.000000000000000000, 0.8660254037844387076, 1.000000000000000000, 0.8660254037844387076, 1.000000000000000000, 0.8660254037844387076, 1.000000000000000000, 0.8660254037844387076, 1.000000000000000000, 0.8660254037844387076, 1.000000000000000000, 0.8660254037844387076, 1.000000000000000000, 0.8660254037844387076, 1.000000000000000000, 0.8660254037844387076, 1.000000000000000000, 0.8660254037844387076, 1.000000000000000000, 0.8660254037844387076, 1.000000000000000000, 0.8660254037844387076, 1.000000000000000000, 0.8660254037844387076, 1.000000000000000000, 0.8660254037844387076, 1.000000000000000000, 0.8660254037844387076, 1.000000000000000000, 0.8660254037844387076, 1.000000000000000000, 0.8660254037844387076, 1.000000000000000000, 0.8660254037844387076, 1.000000000000000000, 0.8660254037844387076, 1.000000000000000000, 0.8660254037844387076, 1.000000000000000000, 0.8660254037844387076, 1.000000000000000000, 0.8660254037844387076, 1.000000000000000000, 0.8660254037844387076, 1.000000000000000000, 0.8660254037844387076, 1.000000000000000000, 0.8660254037844387076, 1.000000000000000000, 0.8660254037844387076, 1.000000000000000000, 0.8660254037844387076, 1.000000000000000000, 0.8660254037844387076, 1.000000000000000000, 0.8660254037844387076, 1.000000000000000000, 0.8660254037844387076, 1.000000000000000000, 0.8660254037844387076, 1.000000000000000000, 0.8660254037844387076, 1.000000000000000000, 0.8660254037844387076, 1.000000000000000000, 0.8660254037844387076, 1.000000000000000000, 0.8660254037844387076, 1.000000000000000000, 0.8660254037844387076, 1.000000000000000000, 0.8660254037844387076, 1.000000000000000000, 0.8660254037844387076, 1.000000000000000000, 0.8660254037844387076, 1.000000000000000000, 0.8660254037844387076, 1.000000000000000000, 0.8660254037844387076, 1.000000000000000000, 0.8660254037844387076, 1.000000000000000000, 0.8660254037844387076, 1.000000000000000000, 0.8660254037844387076, 1.000000000000000000, 0.8660254037844387076, 1.000000000000000000, 0.8660254037844387076, 1.000000000000000000, 0.8660254037844387076, 1.000000000000000000, 0.8660254037844387076, 1.000000000000000000, 0.8660254037844387076, 1.000000000000000000, 0.8660254037844387076, 1.000000000000000000, 0.8660254037844387076, 1.000000000000000000, 0.8660254037844387076, 1.000000000000000000, 0.8660254037844387076, 1.000000000000000000, 0.8660254037844387076, 1.000000000000000000, 0.8660254037844387076, 1.000000000000000000, 0.8660254037844387076, 1.000000000000000000, 0.8660254037844387076, 1.000000000000000000, 0.8660254037844387076, 1.000000000000000000, 0.8660254037844387076, 1.000000000000000000, 0.8660254037844387076, 1.000000000000000000, 0.8660254037844387076, 1.000000000000000000, 0.8660254037844387076, 1.000000000000000000, 0.8660254037844387076, 1.000000000000000000, 0.8660254037844387076, 1.000000000000000000, 0.8660254037844387076, 1.000000000000000000, 0.8660254037844387076, 1.000000000000000000, 0.8660254037844387076, 1.000000000000000000, 0.8660254037844387076, 1.000000000000000000, 0.8660254037844387076, 1.000000000000000000, 0.8660254037844387076, 1.000000000000000000, 0.8660254037844387076, 1.000000000000000000, 0.8660254037844387076, 1.000000000000000000, 0.8660254037844387076, 1.000000000000000000, 0.8660254037844387076, 1.000000000000000000, 0.8660254037844387076, 1.000000000000000000, 0.8660254037844387076, 1.000000000000000000, 0.8660254037844387076, 1.000000000000000000, 0.8660254037844387076, 1.000000000000000000, 0.8660254037844387076, 1.000000000000000000, 0.8660254037844387076, 1.000000000000000000, 0.8660254037844387076, 1.000000000000000000, 0.8660254037844387076, 1.000000000000000000, 0.8660254037844387076, 1.000000000000000000, 0.8660254037844387076, 1.000000000000000000, 0.8660254037844387076, 1.000000000000000000, 0.8660254037844387076, 1.000000000000000000, 0.8660254037844387076, 1.000000000000000000, 0.8660254037844387076, 1.000000000000000000, 0.8660254037844387076, 1.000000000000000000, 0.8660254037844387076, 1.000000000000000000, 0.8660254037844387076, 1.000000000000000000, 0.8660254037844387076, 1.000000000000000000, 0.8660254037844387076, 1.000000000000000000, 0.8660254037844387076, 1.000000000000000000, 0.8660254037844387076, 1.000000000000000000, 0.8660254037844387076, 1.000000000000000000, 0.8660254037844387076, 1.000000000000000000, 0.8660254037844387076, 1.000000000000000000, 0.8660254037844387076, 1.000000000000000000, 0.8660254037844387076, 1.000000000000000000, 0.8660254037844387076, 1.000000000000000000, 0.8660254037844387076, 1.000000000000000000, 0.8660254037844387076, 1.000000000000000000, 0.8660254037844387076, 1.000000000000000000, 0.8660254037844387076, 1.000000000000000000, 0.8660254037844387076, 1.000000000000000000, 0.8660254037844387076, 1.000000000000000000, 0.8660254037844387076, 1.000000000000000000, 0.8660254037844387076, 1.000000000000000000, 0.8660254037844387076, 1.000000000000000000, 0.8660254037844387076, 1.000000000000000000, 0.8660254037844387076, 1.000000000000000000, 0.8660254037844387076, 1.000000000000000000, 0.8660254037844387076, 1.000000000000000000, 0.8660254037844387076, 1.000000000000000000, 0.8660254037844387076, 1.000000000000000000, 0.8660254037844387076, 1.000000000000000000, 0.8660254037844387076, 1.000000000000000000, 0.8660254037844387076, 1.000000000000000000, 0.8660254037844387076, 1.000000000000000000, 0.8660254037844387076, 1.000000000000000000, 0.8660254037844387076, 1.000000000000000000, 0.8660254037844387076, 1.000000000000000000, 0.8660254037844387076, 1.000000000000000000, 0.8660254037844387076, 1.000000000000000000, 0.8660254037844387076, 1.000000000000000000, 0.8660254037844387076, 1.000000000000000000, 0.8660254037844387076, 1.000000000000000000, 0.8660254037844387076, 1.000000000000000000, 0.8660254037844387076, 1.000000000000000000, 0.8660254037844387076, 1.000000000000000000, 0.8660254037844387076, 1.000000000000000000, 0.8660254037844387076, 1.000000000000000000, 0.8660254037844387076, 1.000000000000000000, 0.8660254037844387076, 1.000000000000000000, 0.8660254037844387076, 1.000000000000000000, 0.8660254037844387076, 1.000000000000000000, 0.8660254037844387076, 1.000000000000000000, 0.8660254037844387076, 1.000000000000000000, 0.8660254037844387076, 1.000000000000000000, 0.8660254037844387076, 1.000000000000000000, 0.8660254037844387076, 1.000000000000000000, 0.8660254037844387076, 1.000000000000000000, 0.8660254037844387076, 1.000000000000000000, 0.8660254037844387076, 1.000000000000000000, 0.8660254037844387076, 1.000000000000000000, 0.8660254037844387076, 1.000000000000000000, 0.8660254037844387076, 1.000000000000000000, 0.8660254037844387076, 1.000000000000000000, 0.8660254037844387076, 1.000000000000000000, 0.8660254037844387076, 1.000000000000000000, 0.8660254037844387076, 1.000000000000000000, 0.8660254037844387076, 1.000000000000000000, 0.8660254037844387076, 1.000000000000000000, 0.8660254037844387076, 1.000000000000000000, 0.8660254037844387076, 1.000000000000000000, 0.8660254037844387076, 1.000000000000000000, 0.8660254037844387076, 1.000000000000000000, 0.8660254037844387076, 1.000000000000000000, 0.8660254037844387076, 1.000000000000000000, 0.8660254037844387076, 1.000000000000000000, 0.8660254037844387076, 1.000000000000000000, 0.8660254037844387076, 1.000000000000000000, 0.8660254037844387076, 1.000000000000000000, 0.8660254037844387076, 1.000000000000000000, 0.8660254037844387076, 1.000000000000000000, 0.8660254037844387076, 1.000000000000000000, 0.8660254037844387076, 1.000000000000000000, 0.8660254037844387076, 1.000000000000000000, 0.8660254037844387076, 1.000000000000000000, 0.8660254037844387076, 1.000000000000000000, 0.8660254037844387076, 1.000000000000000000, 0.8660254037844387076, 1.000000000000000000, 0.8660254037844387076, 1.000000000000000000, 0.8660254037844387076, 1.000000000000000000, 0.8660254037844387076, 1.000000000000000000, 0.8660254037844387076, 1.000000000000000000, 0.8660254037844387076, 1.000000000000000000, 0.8660254037844387076, 1.000000000000000000, 0.8660254037844387076, 1.000000000000000000, 0.8660254037844387076, 1.000000000000000000, 0.8660254037844387076, 1.000000000000000000, 0.8660254037844387076, 1.000000000000000000, 0.8660254037844387076, 1.000000000000000000, 0.8660254037844387076, 1.000000000000000000, 0.8660254037844387076, 1.000000000000000000, 0.8660254037844387076, 1.000000000000000000, 0.8660254037844387076, 1.000000000000000000, 0.8660254037844387076, 1.000000000000000000, 0.8660254037844387076, 1.000000000000000000, 0.8660254037844387076, 1.000000000000000000, 0.8660254037844387076, 1.000000000000000000, 0.8660254037844387076, 1.000000000000000000, 0.8660254037844387076, 1.000000000000000000, 0.8660254037844387076, 1.000000000000000000, 0.8660254037844387076, 1.000000000000000000, 0.8660254037844387076, 1.000000000000000000, 0.8660254037844387076, 1.000000000000000000, 0.8660254037844387076, 1.000000000000000000, 0.8660254037844387076, 1.000000000000000000, 0.8660254037844387076, 1.000000000000000000, 0.8660254037844387076, 1.000000000000000000, 0.8660254037844387076, 1.000000000000000000, 0.8660254037844387076, 1.000000000000000000, 0.8660254037844387076, 1.000000000000000000, 0.8660254037844387076, 1.000000000000000000, 0.8660254037844387076, 1.000000000000000000, 0.8660254037844387076, 1.000000000000000000, 0.8660254037844387076, 1.000000000000000000, 0.8660254037844387076, 1.000000000000000000, 0.8660254037844387076, 1.000000000000000000, 0.8660254037844387076, 1.000000000000000000, 0.8660254037844387076, 1.000000000000000000, 0.8660254037844387076, 1.000000000000000000, 0.8660254037844387076, 1.000000000000000000, 0.8660254037844387076, 1.000000000000000000, 0.8660254037844387076, 1.000000000000000000, 0.8660254037844387076, 1.000000000000000000, 0.8660254037844387076, 1.000000000000000000, 0.8660254037844387076, 1.000000000000000000, 0.8660254037844387076, 1.000000000000000000, 0.8660254037844387076, 1.000000000000000000, 0.8660254037844387076, 1.000000000000000000, 0.8660254037844387076, 1.000000000000000000, 0.8660254037844387076, 1.000000000000000000, 0.8660254037844387076, 1.000000000000000000, 0.8660254037844387076, 1.000000000000000000, 0.8660254037844387076, 1.000000000000000000, 0.8660254037844387076, 1.000000000000000000, 0.8660254037844387076, 1.000000000000000000, 0.8660254037844387076, 1.000000000000000000, 0.8660254037844387076, 1.000000000000000000, 0.8660254037844387076, 1.000000000000000000, 0.8660254037844387076, 1.000000000000000000, 0.8660254037844387076, 1.000000000000000000, 0.8660254037844387076, 1.000000000000000000, 0.8660254037844387076, 1.000000000000000000, 0.8660254037844387076, 1.000000000000000000, 0.8660254037844387076, 1.000000000000000000, 0.8660254037844387076, 1.000000000000000000, 0.8660254037844387076, 1.000000000000000000, 0.8660254037844387076, 1.000000000000000000, 0.8660254037844387076, 1.000000000000000000, 0.8660254037844387076, 1.000000000000000000, 0.8660254037844387076, 1.000000000000000000, 0.8660254037844387076, 1.000000000000000000, 0.8660254037844387076, 1.000000000000000000, 0.8660254037844387076, 1.000000000000000000, 0.8660254037844387076, 1.000000000000000000, 0.8660254037844387076, 1.000000000000000000, 0.8660254037844387076, 1.000000000000000000, 0.8660254037844387076, 1.000000000000000000, 0.8660254037844387076, 1.000000000000000000, 0.8660254037844387076, 1.000000000000000000, 0.8660254037844387076, 1.000000000000000000, 0.8660254037844387076, 1.000000000000000000, 0.8660254037844387076, 1.000000000000000000, 0.8660254037844387076, 1.000000000000000000, 0.8660254037844387076, 1.000000000000000000, 0.8660254037844387076, 1.000000000000000000, 0.8660254037844387076, 1.000000000000000000, 0.8660254037844387076, 1.000000000000000000, 0.8660254037844387076, 1.000000000000000000, 0.8660254037844387076, 1.000000000000000000, 0.8660254037844387076, 1.000000000000000000, 0.8660254037844387076, 1.000000000000000000, 0.8660254037844387076, 1.000000000000000000, 0.8660254037844387076, 1.000000000000000000, 0.8660254037844387076, 1.000000000000000000, 0.8660254037844387076, 1.000000000000000000, 0.8660254037844387076, 1.000000000000000000, 0.8660254037844387076, 1.000000000000000000, 0.8660254037844387076, 1.000000000000000000, 0.8660254037844387076, 1.000000000000000000, 0.8660254037844387076, 1.000000000000000000, 0.8660254037844387076, 1.000000000000000000, 0.8660254037844387076, 1.000000000000000000, 0.8660254037844387076, 1.000000000000000000, 0.8660254037844387076, 1.000000000000000000, 0.8660254037844387076, 1.000000000000000000, 0.8660254037844387076, 1.000000000000000000, 0.8660254037844387076, 1.000000000000000000, 0.8660254037844387076, 1.000000000000000000, 0.8660254037844387076, 1.000000000000000000, 0.8660254037844387076, 1.000000000000000000, 0.8660254037844387076, 1.000000000000000000, 0.8660254037844387076, 1.000000000000000000, 0.8660254037844387076, 1.000000000000000000, 0.8660254037844387076, 1.000000000000000000, 0.8660254037844387076, 1.000000000000000000, 0.8660254037844387076, 1.000000000000000000, 0.8660254037844387076, 1.000000000000000000, 0.8660254037844387076, 1.000000000000000000, 0.8660254037844387076, 1.000000000000000000, 0.8660254037844387076, 1.000000000000000000, 0.8660254037844387076, 1.000000000000000000, 0.8660254037844387076, 1.000000000000000000, 0.8660254037844387076, 1.000000000000000000, 0.8660254037844387076, 1.000000000000000000, 0.8660254037844387076, 1.000000000000000000, 0.8660254037844387076, 1.000000000000000000, 0.8660254037844387076, 1.000000000000000000, 0.8660254037844387076, 1.000000000000000000, 0.8660254037844387076, 1.000000000000000000, 0.8660254037844387076, 1.000000000000000000, 0.8660254037844387076, 1.000000000000000000, 0.8660254037844387076, 1.000000000000000000, 0.8660254037844387076, 1.000000000000000000, 0.8660254037844387076, 1.000000000000000000, 0.8660254037844387076, 1.000000000000000000, 0.8660254037844387076, 1.000000000000000000, 0.8660254037844387076, 1.000000000000000000, 0.8660254037844387076, 1.000000000000000000, 0.8660254037844387076, 1.000000000000000000, 0.8660254037844387076, 1.000000000000000000, 0.8660254037844387076, 1.000000000000000000, 0.8660254037844387076, 1.000000000000000000, 0.8660254037844387076, 1.000000000000000000, 0.8660254037844387076, 1.000000000000000000, 0.8660254037844387076, 1.000000000000000000, 0.8660254037844387076, 1.000000000000000000, 0.8660254037844387076, 1.000000000000000000, 0.8660254037844387076, 1.000000000000000000, 0.8660254037844387076, 1.000000000000000000, 0.8660254037844387076, 1.000000000000000000, 0.8660254037844387076, 1.000000000000000000, 0.8660254037844387076, 1.000000000000000000, 0.8660254037844387076, 1.000000000000000000, 0.8660254037844387076, 1.000000000000000000, 0.8660254037844387076, 1.000000000000000000, 0.8660254037844387076, 1.000000000000000000, 0.8660254037844387076, 1.000000000000000000, 0.8660254037844387076, 1.000000000000000000, 0.8660254037844387076, 1.000000000000000000, 0.8660254037844387076, 1.000000000000000000, 0.8660254037844387076, 1.000000000000000000, 0.8660254037844387076, 1.000000000000000000, 0.8660254037844387076, 1.000000000000000000, 0.8660254037844387076, 1.000000000000000000, 0.8660254037844387076, 1.000000000000000000, 0.8660254037844387076, 1.000000000000000000, 0.8660254037844387076, 1.000000000000000000, 0.8660254037844387076, 1.000000000000000000, 0.8660254037844387076, 1.000000000000000000, 0.8660254037844387076, 1.000000000000000000, 0.8660254037844387076, 1.000000000000000000, 0.8660254037844387076, 1.000000000000000000, 0.8660254037844387076, 1.000000000000000000, 0.8660254037844387076, 1.000000000000000000, 0.8660254037844387076, 1.000000000000000000, 0.8660254037844387076, 1.000000000000000000, 0.8660254037844387076, 1.000000000000000000, 0.8660254037844387076, 1.000000000000000000, 0.8660254037844387076, 1.000000000000000000, 0.8660254037844387076, 1.000000000000000000, 0.8660254037844387076, 1.000000000000000000, 0.8660254037844387076, 1.000000000000000000, 0.8660254037844387076, 1.000000000000000000, 0.8660254037844387076, 1.000000000000000000, 0.8660254037844387076, 1.000000000000000000, 0.8660254037844387076, 1.000000000000000000, 0.8660254037844387076, 1.000000000000000000, 0.8660254037844387076, 1.000000000000000000, 0.8660254037844387076, 1.000000000000000000, 0.8660254037844387076, 1.000000000000000000, 0.8660254037844387076, 1.000000000000000000, 0.8660254037844387076, 1.000000000000000000, 0.8660254037844387076, 1.000000000000000000, 0.8660254037844387076, 1.000000000000000000, 0.8660254037844387076, 1.000000000000000000, 0.8660254037844387076, 1.000000000000000000, 0.8660254037844387076, 1.000000000000000000, 0.8660254037844387076, 1.000000000000000000, 0.8660254037844387076, 1.000000000000000000, 0.8660254037844387076, 1.000000000000000000, 0.8660254037844387076, 1.000000000000000000, 0.8660254037844387076, 1.000000000000000000, 0.8660254037844387076, 1.000000000000000000, 0.8660254037844387076, 1.000000000000000000, 0.8660254037844387076, 1.000000000000000000, 0.8660254037844387076, 1.000000000000000000, 0.8660254037844387076, 1.000000000000000000, 0.8660254037844387076, 1.000000000000000000, 0.8660254037844387076, 1.000000000000000000, 0.8660254037844387076, 1.000000000000000000, 0.8660254037844387076, 1.000000000000000000, 0.8660254037844387076, 1.000000000000000000, 0.8660254037844387076, 1.000000000000000000, 0.8660254037844387076, 1.000000000000000000, 0.8660254037844387076, 1.000000000000000000, 0.8660254037844387076, 1.000000000000000000, 0.8660254037844387076, 1.000000000000000000, 0.8660254037844387076, 1.000000000000000000, 0.8660254037844387076, 1.000000000000000000, 0.8660254037844387076, 1.000000000000000000, 0.8660254037844387076, 1.000000000000000000, 0.8660254037844387076, 1.000000000000000000, 0.8660254037844387076, 1.000000000000000000, 0.8660254037844387076, 1.000000000000000000, 0.8660254037844387076, 1.000000000000000000, 0.8660254037844387076, 1.000000000000000000, 0.8660254037844387076, 1.000000000000000000, 0.8660254037844387076, 1.000000000000000000, 0.8660254037844387076, 1.000000000000000000, 0.8660254037844387076, 1.000000000000000000, 0.8660254037844387076, 1.000000000000000000, 0.8660254037844387076, 1.000000000000000000, 0.8660254037844387076, 1.000000000000000000, 0.8660254037844387076, 1.000000000000000000, 0.8660254037844387076, 1.000000000000000000, 0.8660254037844387076, 1.000000000000000000, 0.8660254037844387076, 1.000000000000000000, 0.8660254037844387076, 1.000000000000000000, 0.8660254037844387076, 1.000000000000000000, 0.8660254037844387076, 1.000000000000000000, 0.8660254037844387076, 1.000000000000000000, 0.8660254037844387076, 1.000000000000000000, 0.8660254037844387076, 1.000000000000000000, 0.8660254037844387076, 1.000000000000000000, 0.8660254037844387076, 1.000000000000000000, 0.8660254037844387076, 1.000000000000000000, 0.8660254037844387076, 1.000000000000000000, 0.8660254037844387076, 1.000000000000000000, 0.8660254037844387076, 1.000000000000000000, 0.8660254037844387076, 1.000000000000000000, 0.8660254037844387076, 1.000000000000000000, 0.8660254037844387076, 1.000000000000000000, 0.8660254037844387076, 1.000000000000000000, 0.8660254037844387076, 1.000000000000000000, 0.8660254037844387076, 1.000000000000000000, 0.8660254037844387076, 1.000000000000000000, 0.8660254037844387076, 1.000000000000000000, 0.8660254037844387076, 1.000000000000000000, 0.8660254037844387076, 1.000000000000000000, 0.8660254037844387076, 1.000000000000000000, 0.8660254037844387076, 1.000000000000000000, 0.8660254037844387076, 1.000000000000000000, 0.8660254037844387076, 1.000000000000000000, 0.8660254037844387076, 1.000000000000000000, 0.8660254037844387076, 1.000000000000000000, 0.8660254037844387076, 1.000000000000000000, 0.8660254037844387076, 1.000000000000000000, 0.8660254037844387076, 1.000000000000000000, 0.8660254037844387076, 1.000000000000000000, 0.8660254037844387076, 1.000000000000000000, 0.8660254037844387076, 1.000000000000000000, 0.8660254037844387076, 1.000000000000000000, 0.8660254037844387076, 1.000000000000000000, 0.8660254037844387076, 1.000000000000000000, 0.8660254037844387076, 1.000000000000000000, 0.8660254037844387076, 1.000000000000000000, 0.8660254037844387076, 1.000000000000000000, 0.8660254037844387076, 1.000000000000000000, 0.8660254037844387076, 1.000000000000000000, 0.8660254037844387076, 1.000000000000000000, 0.8660254037844387076, 1.000000000000000000, 0.8660254037844387076, 1.000000000000000000, 0.8660254037844387076, 1.000000000000000000, 0.8660254037844387076, 1.000000000000000000, 0.8660254037844387076, 1.000000000000000000, 0.8660254037844387076, 1.000000000000000000, 0.8660254037844387076, 1.000000000000000000, 0.8660254037844387076, 1.000000000000000000, 0.8660254037844387076, 1.000000000000000000, 0.8660254037844387076, 1.000000000000000000, 0.8660254037844387076, 1.000000000000000000, 0.8660254037844387076, 1.000000000000000000, 0.8660254037844387076, 1.000000000000000000, 0.8660254037844387076, 1.000000000000000000, 0.8660254037844387076, 1.000000000000000000, 0.8660254037844387076, 1.000000000000000000, 0.8660254037844387076, 1.000000000000000000, 0.8660254037844387076, 1.000000000000000000, 0.8660254037844387076, 1.000000000000000000, 0.8660254037844387076, 1.000000000000000000, 0.8660254037844387076, 1.000000000000000000, 0.8660254037844387076, 1.000000000000000000, 0.8660254037844387076, 1.000000000000000000, 0.8660254037844387076, 1.000000000000000000, 0.8660254037844387076, 1.000000000000000000, 0.8660254037844387076, 1.000000000000000000, 0.8660254037844387076, 1.000000000000000000, 0.8660254037844387076, 1.000000000000000000, 0.8660254037844387076, 1.000000000000000000, 0.8660254037844387076, 1.000000000000000000, 0.8660254037844387076, 1.000000000000000000, 0.8660254037844387076, 1.000000000000000000, 0.8660254037844387076, 1.000000000000000000, 0.8660254037844387076, 1.000000000000000000, 0.8660254037844387076, 1.000000000000000000, 0.8660254037844387076, 1.000000000000000000, 0.8660254037844387076, 1.000000000000000000, 0.8660254037844387076, 1.000000000000000000, 0.8660254037844387076, 1.000000000000000000, 0.8660254037844387076, 1.000000000000000000, 0.8660254037844387076, 1.000000000000000000, 0.8660254037844387076, 1.000000000000000000, 0.8660254037844387076, 1.000000000000000000, 0.8660254037844387076, 1.000000000000000000, 0.8660254037844387076, 1.000000000000000000, 0.8660254037844387076, 1.000000000000000000, 0.8660254037844387076, 1.000000000000000000, 0.8660254037844387076, 1.000000000000000000, 0.8660254037844387076, 1.000000000000000000, 0.8660254037844387076, 1.000000000000000000, 0.8660254037844387076, 1.000000000000000000, 0.8660254037844387076, 1.000000000000000000, 0.8660254037844387076, 1.000000000000000000, 0.8660254037844387076, 1.000000000000000000, 0.8660254037844387076, 1.000000000000000000, 0.8660254037844387076, 1.000000000000000000, 0.8660254037844387076, 1.000000000000000000, 0.8660254037844387076, 1.000000000000000000, 0.8660254037844387076, 1.000000000000000000, 0.8660254037844387076, 1.000000000000000000, 0.8660254037844387076, 1.000000000000000000, 0.8660254037844387076, 1.000000000000000000, 0.8660254037844387076, 1.000000000000000000, 0.8660254037844387076, 1.000000000000000000, 0.8660254037844387076, 1.000000000000000000, 0.8660254037844387076, 1.000000000000000000, 0.8660254037844387076, 1.000000000000000000, 0.8660254037844387076, 1.000000000000000000, 0.8660254037844387076, 1.000000000000000000, 0.8660254037844387076, 1.000000000000000000, 0.8660254037844387076, 1.000000000000000000, 0.8660254037844387076, 1.000000000000000000, 0.8660254037844387076, 1.000000000000000000, 0.8660254037844387076, 1.000000000000000000, 0.8660254037844387076, 1.000000000000000000, 0.8660254037844387076, 1.000000000000000000, 0.8660254037844387076, 1.000000000000000000, 0.8660254037844387076, 1.000000000000000000, 0.8660254037844387076, 1.000000000000000000, 0.8660254037844387076, 1.000000000000000000, 0.8660254037844387076, 1.000000000000000000, 0.8660254037844387076, 1.000000000000000000, 0.8660254037844387076, 1.000000000000000000, 0.8660254037844387076, 1.000000000000000000, 0.8660254037844387076, 1.000000000000000000, 0.8660254037844387076, 1.000000000000000000, 0.8660254037844387076, 1.000000000000000000, 0.8660254037844387076, 1.000000000000000000, 0.8660254037844387076, 1.000000000000000000, 0.8660254037844387076, 1.000000000000000000, 0.8660254037844387076, 1.000000000000000000, 0.8660254037844387076, 1.000000000000000000, 0.8660254037844387076, 1.000000000000000000, 0.8660254037844387076, 1.000000000000000000, 0.8660254037844387076, 1.000000000000000000, 0.8660254037844387076, 1.000000000000000000, 0.8660254037844387076, 1.000000000000000000, 0.8660254037844387076, 1.000000000000000000, 0.8660254037844387076, 1.000000000000000000, 0.8660254037844387076, 1.000000000000000000, 0.8660254037844387076, 1.000000000000000000, 0.8660254037844387076, 1.000000000000000000, 0.8660254037844387076, 1.000000000000000000, 0.8660254037844387076, 1.000000000000000000, 0.8660254037844387076, 1.000000000000000000, 0.8660254037844387076, 1.000000000000000000, 0.8660254037844387076, 1.000000000000000000, 0.8660254037844387076, 1.000000000000000000, 0.8660254037844387076, 1.000000000000000000, 0.8660254037844387076, 1.000000000000000000, 0.8660254037844387076, 1.000000000000000000, 0.8660254037844387076, 1.000000000000000000, 0.8660254037844387076, 1.000000000000000000, 0.8660254037844387076, 1.000000000000000000, 0.8660254037844387076, 1.000000000000000000, 0.8660254037844387076, 1.000000000000000000, 0.8660254037844387076, 1.000000000000000000, 0.8660254037844387076, 1.000000000000000000, 0.8660254037844387076, 1.000000000000000000, 0.8660254037844387076, 1.000000000000000000, 0.8660254037844387076, 1.000000000000000000, 0.8660254037844387076, 1.000000000000000000, 0.8660254037844387076, 1.000000000000000000, 0.8660254037844387076, 1.000000000000000000, 0.8660254037844387076, 1.000000000000000000, 0.8660254037844387076, 1.000000000000000000, 0.8660254037844387076, 1.000000000000000000, 0.8660254037844387076, 1.000000000000000000, 0.8660254037844387076, 1.000000000000000000, 0.8660254037844387076, 1.000000000000000000, 0.8660254037844387076, 1.000000000000000000, 0.8660254037844387076, 1.000000000000000000, 0.8660254037844387076, 1.000000000000000000, 0.8660254037844387076, 1.000000000000000000, 0.8660254037844387076, 1.000000000000000000, 0.8660254037844387076, 1.000000000000000000, 0.8660254037844387076, 1.000000000000000000, 0.8660254037844387076, 1.000000000000000000, 0.8660254037844387076, 1.000000000000000000, 0.8660254037844387076, 1.000000000000000000, 0.8660254037844387076, 1.000000000000000000, 0.8660254037844387076, 1.000000000000000000, 0.8660254037844387076, 1.000000000000000000, 0.8660254037844387076, 1.000000000000000000, 0.8660254037844387076, 1.000000000000000000, 0.8660254037844387076, 1.000000000000000000, 0.8660254037844387076, 1.000000000000000000, 0.8660254037844387076, 1.000000000000000000, 0.8660254037844387076, 1.000000000000000000, 0.8660254037844387076, 1.000000000000000000, 0.8660254037844387076, 1.000000000000000000, 0.8660254037844387076, 1.000000000000000000, 0.8660254037844387076, 1.000000000000000000, 0.8660254037844387076, 1.000000000000000000, 0.8660254037844387076, 1.000000000000000000, 0.8660254037844387076, 1.000000000000000000, 0.8660254037844387076, 1.000000000000000000, 0.8660254037844387076, 1.000000000000000000, 0.8660254037844387076, 1.000000000000000000, 0.8660254037844387076, 1.000000000000000000, 0.8660254037844387076, 1.000000000000000000, 0.8660254037844387076, 1.000000000000000000, 0.8660254037844387076, 1.000000000000000000),
 ( 1.000000000000000000, 0.8660254037844387076, 1.000000000000000000, 0.8660254037844387076, 1.000000000000000000, 0.8660254037844387076, 1.000000000000000000, 0.8660254037844387076, 1.000000000000000000, 0.8660254037844387076, 1.000000000000000000, 0.8660254037844387076, 1.000000000000000000, 0.8660254037844387076, 1.000000000000000000, 0.8660254037844387076, 1.000000000000000000, 0.8660254037844387076, 1.000000000000000000, 0.8660254037844387076, 1.000000000000000000, 0.8660254037844387076, 1.000000000000000000, 0.8660254037844387076, 1.000000000000000000, 0.8660254037844387076, 1.000000000000000000, 0.8660254037844387076, 1.000000000000000000, 0.8660254037844387076, 1.000000000000000000, 0.8660254037844387076, 1.000000000000000000, 0.8660254037844387076, 1.000000000000000000, 0.8660254037844387076, 1.000000000000000000, 0.8660254037844387076, 1.000000000000000000, 0.8660254037844387076, 1.000000000000000000, 0.8660254037844387076, 1.000000000000000000, 0.8660254037844387076, 1.000000000000000000, 0.8660254037844387076, 1.000000000000000000, 0.8660254037844387076, 1.000000000000000000, 0.8660254037844387076, 1.000000000000000000, 0.8660254037844387076, 1.000000000000000000, 0.8660254037844387076, 1.000000000000000000, 0.8660254037844387076, 1.000000000000000000, 0.8660254037844387076, 1.000000000000000000, 0.8660254037844387076, 1.000000000000000000, 0.8660254037844387076, 1.000000000000000000, 0.8660254037844387076, 1.000000000000000000, 0.8660254037844387076, 1.000000000000000000, 0.8660254037844387076, 1.000000000000000000, 0.8660254037844387076, 1.000000000000000000, 0.8660254037844387076, 1.000000000000000000, 0.8660254037844387076, 1.000000000000000000, 0.8660254037844387076, 1.000000000000000000, 0.8660254037844387076, 1.000000000000000000, 0.8660254037844387076, 1.000000000000000000, 0.8660254037844387076, 1.000000000000000000, 0.8660254037844387076, 1.000000000000000000, 0.8660254037844387076, 1.000000000000000000, 0.8660254037844387076, 1.000000000000000000, 0.8660254037844387076, 1.000000000000000000, 0.8660254037844387076, 1.000000000000000000, 0.8660254037844387076, 1.000000000000000000, 0.8660254037844387076, 1.000000000000000000, 0.8660254037844387076, 1.000000000000000000, 0.8660254037844387076, 1.000000000000000000, 0.8660254037844387076, 1.000000000000000000, 0.8660254037844387076, 1.000000000000000000, 0.8660254037844387076, 1.000000000000000000, 0.8660254037844387076, 1.000000000000000000, 0.8660254037844387076, 1.000000000000000000, 0.8660254037844387076, 1.000000000000000000, 0.8660254037844387076, 1.000000000000000000, 0.8660254037844387076, 1.000000000000000000, 0.8660254037844387076, 1.000000000000000000, 0.8660254037844387076, 1.000000000000000000, 0.8660254037844387076, 1.000000000000000000, 0.8660254037844387076, 1.000000000000000000, 0.8660254037844387076, 1.000000000000000000, 0.8660254037844387076, 1.000000000000000000, 0.8660254037844387076, 1.000000000000000000, 0.8660254037844387076, 1.000000000000000000, 0.8660254037844387076, 1.000000000000000000, 0.8660254037844387076, 1.000000000000000000, 0.8660254037844387076, 1.000000000000000000, 0.8660254037844387076, 1.000000000000000000, 0.8660254037844387076, 1.000000000000000000, 0.8660254037844387076, 1.000000000000000000, 0.8660254037844387076, 1.000000000000000000, 0.8660254037844387076, 1.000000000000000000, 0.8660254037844387076, 1.000000000000000000, 0.8660254037844387076, 1.000000000000000000, 0.8660254037844387076, 1.000000000000000000, 0.8660254037844387076, 1.000000000000000000, 0.8660254037844387076, 1.000000000000000000, 0.8660254037844387076, 1.000000000000000000, 0.8660254037844387076, 1.000000000000000000, 0.8660254037844387076, 1.000000000000000000, 0.8660254037844387076, 1.000000000000000000, 0.8660254037844387076, 1.000000000000000000, 0.8660254037844387076, 1.000000000000000000, 0.8660254037844387076, 1.000000000000000000, 0.8660254037844387076, 1.000000000000000000, 0.8660254037844387076, 1.000000000000000000, 0.8660254037844387076, 1.000000000000000000, 0.8660254037844387076, 1.000000000000000000, 0.8660254037844387076, 1.000000000000000000, 0.8660254037844387076, 1.000000000000000000, 0.8660254037844387076, 1.000000000000000000, 0.8660254037844387076, 1.000000000000000000, 0.8660254037844387076, 1.000000000000000000, 0.8660254037844387076, 1.000000000000000000, 0.8660254037844387076, 1.000000000000000000, 0.8660254037844387076, 1.000000000000000000, 0.8660254037844387076, 1.000000000000000000, 0.8660254037844387076, 1.000000000000000000, 0.8660254037844387076, 1.000000000000000000, 0.8660254037844387076, 1.000000000000000000, 0.8660254037844387076, 1.000000000000000000, 0.8660254037844387076, 1.000000000000000000, 0.8660254037844387076, 1.000000000000000000, 0.8660254037844387076, 1.000000000000000000, 0.8660254037844387076, 1.000000000000000000, 0.8660254037844387076, 1.000000000000000000, 0.8660254037844387076, 1.000000000000000000, 0.8660254037844387076, 1.000000000000000000, 0.8660254037844387076, 1.000000000000000000, 0.8660254037844387076, 1.000000000000000000, 0.8660254037844387076, 1.000000000000000000, 0.8660254037844387076, 1.000000000000000000, 0.8660254037844387076, 1.000000000000000000, 0.8660254037844387076, 1.000000000000000000, 0.8660254037844387076, 1.000000000000000000, 0.8660254037844387076, 1.000000000000000000, 0.8660254037844387076, 1.000000000000000000, 0.8660254037844387076, 1.000000000000000000, 0.8660254037844387076, 1.000000000000000000, 0.8660254037844387076, 1.000000000000000000, 0.8660254037844387076, 1.000000000000000000, 0.8660254037844387076, 1.000000000000000000, 0.8660254037844387076, 1.000000000000000000, 0.8660254037844387076, 1.000000000000000000, 0.8660254037844387076, 1.000000000000000000, 0.8660254037844387076, 1.000000000000000000, 0.8660254037844387076, 1.000000000000000000, 0.8660254037844387076, 1.000000000000000000, 0.8660254037844387076, 1.000000000000000000, 0.8660254037844387076, 1.000000000000000000, 0.8660254037844387076, 1.000000000000000000, 0.8660254037844387076, 1.000000000000000000, 0.8660254037844387076, 1.000000000000000000, 0.8660254037844387076, 1.000000000000000000, 0.8660254037844387076, 1.000000000000000000, 0.8660254037844387076, 1.000000000000000000, 0.8660254037844387076, 1.000000000000000000, 0.8660254037844387076, 1.000000000000000000, 0.8660254037844387076, 1.000000000000000000, 0.8660254037844387076, 1.000000000000000000, 0.8660254037844387076, 1.000000000000000000, 0.8660254037844387076, 1.000000000000000000, 0.8660254037844387076, 1.000000000000000000, 0.8660254037844387076, 1.000000000000000000, 0.8660254037844387076, 1.000000000000000000, 0.8660254037844387076, 1.000000000000000000, 0.8660254037844387076, 1.000000000000000000, 0.8660254037844387076, 1.000000000000000000, 0.8660254037844387076, 1.000000000000000000, 0.8660254037844387076, 1.000000000000000000, 0.8660254037844387076, 1.000000000000000000, 0.8660254037844387076, 1.000000000000000000, 0.8660254037844387076, 1.000000000000000000, 0.8660254037844387076, 1.000000000000000000, 0.8660254037844387076, 1.000000000000000000, 0.8660254037844387076, 1.000000000000000000, 0.8660254037844387076, 1.000000000000000000, 0.8660254037844387076, 1.000000000000000000, 0.8660254037844387076, 1.000000000000000000, 0.8660254037844387076, 1.000000000000000000, 0.8660254037844387076, 1.000000000000000000, 0.8660254037844387076, 1.000000000000000000, 0.8660254037844387076, 1.000000000000000000, 0.8660254037844387076, 1.000000000000000000, 0.8660254037844387076, 1.000000000000000000, 0.8660254037844387076, 1.000000000000000000, 0.8660254037844387076, 1.000000000000000000, 0.8660254037844387076, 1.000000000000000000, 0.8660254037844387076, 1.000000000000000000, 0.8660254037844387076, 1.000000000000000000, 0.8660254037844387076, 1.000000000000000000, 0.8660254037844387076, 1.000000000000000000, 0.8660254037844387076, 1.000000000000000000, 0.8660254037844387076, 1.000000000000000000, 0.8660254037844387076, 1.000000000000000000, 0.8660254037844387076, 1.000000000000000000, 0.8660254037844387076, 1.000000000000000000, 0.8660254037844387076, 1.000000000000000000, 0.8660254037844387076, 1.000000000000000000, 0.8660254037844387076, 1.000000000000000000, 0.8660254037844387076, 1.000000000000000000, 0.8660254037844387076, 1.000000000000000000, 0.8660254037844387076, 1.000000000000000000, 0.8660254037844387076, 1.000000000000000000, 0.8660254037844387076, 1.000000000000000000, 0.8660254037844387076, 1.000000000000000000, 0.8660254037844387076, 1.000000000000000000, 0.8660254037844387076, 1.000000000000000000, 0.8660254037844387076, 1.000000000000000000, 0.8660254037844387076, 1.000000000000000000, 0.8660254037844387076, 1.000000000000000000, 0.8660254037844387076, 1.000000000000000000, 0.8660254037844387076, 1.000000000000000000, 0.8660254037844387076, 1.000000000000000000, 0.8660254037844387076, 1.000000000000000000, 0.8660254037844387076, 1.000000000000000000, 0.8660254037844387076, 1.000000000000000000, 0.8660254037844387076, 1.000000000000000000, 0.8660254037844387076, 1.000000000000000000, 0.8660254037844387076, 1.000000000000000000, 0.8660254037844387076, 1.000000000000000000, 0.8660254037844387076, 1.000000000000000000, 0.8660254037844387076, 1.000000000000000000, 0.8660254037844387076, 1.000000000000000000, 0.8660254037844387076, 1.000000000000000000, 0.8660254037844387076, 1.000000000000000000, 0.8660254037844387076, 1.000000000000000000, 0.8660254037844387076, 1.000000000000000000, 0.8660254037844387076, 1.000000000000000000, 0.8660254037844387076, 1.000000000000000000, 0.8660254037844387076, 1.000000000000000000, 0.8660254037844387076, 1.000000000000000000, 0.8660254037844387076, 1.000000000000000000, 0.8660254037844387076, 1.000000000000000000, 0.8660254037844387076, 1.000000000000000000, 0.8660254037844387076, 1.000000000000000000, 0.8660254037844387076, 1.000000000000000000, 0.8660254037844387076, 1.000000000000000000, 0.8660254037844387076, 1.000000000000000000, 0.8660254037844387076, 1.000000000000000000, 0.8660254037844387076, 1.000000000000000000, 0.8660254037844387076, 1.000000000000000000, 0.8660254037844387076, 1.000000000000000000, 0.8660254037844387076, 1.000000000000000000, 0.8660254037844387076, 1.000000000000000000, 0.8660254037844387076, 1.000000000000000000, 0.8660254037844387076, 1.000000000000000000, 0.8660254037844387076, 1.000000000000000000, 0.8660254037844387076, 1.000000000000000000, 0.8660254037844387076, 1.000000000000000000, 0.8660254037844387076, 1.000000000000000000, 0.8660254037844387076, 1.000000000000000000, 0.8660254037844387076, 1.000000000000000000, 0.8660254037844387076, 1.000000000000000000, 0.8660254037844387076, 1.000000000000000000, 0.8660254037844387076, 1.000000000000000000, 0.8660254037844387076, 1.000000000000000000, 0.8660254037844387076, 1.000000000000000000, 0.8660254037844387076, 1.000000000000000000, 0.8660254037844387076, 1.000000000000000000, 0.8660254037844387076, 1.000000000000000000, 0.8660254037844387076, 1.000000000000000000, 0.8660254037844387076, 1.000000000000000000, 0.8660254037844387076, 1.000000000000000000, 0.8660254037844387076, 1.000000000000000000, 0.8660254037844387076, 1.000000000000000000, 0.8660254037844387076, 1.000000000000000000, 0.8660254037844387076, 1.000000000000000000, 0.8660254037844387076, 1.000000000000000000, 0.8660254037844387076, 1.000000000000000000, 0.8660254037844387076, 1.000000000000000000, 0.8660254037844387076, 1.000000000000000000, 0.8660254037844387076, 1.000000000000000000, 0.8660254037844387076, 1.000000000000000000, 0.8660254037844387076, 1.000000000000000000, 0.8660254037844387076, 1.000000000000000000, 0.8660254037844387076, 1.000000000000000000, 0.8660254037844387076, 1.000000000000000000, 0.8660254037844387076, 1.000000000000000000, 0.8660254037844387076, 1.000000000000000000, 0.8660254037844387076, 1.000000000000000000, 0.8660254037844387076, 1.000000000000000000, 0.8660254037844387076, 1.000000000000000000, 0.8660254037844387076, 1.000000000000000000, 0.8660254037844387076, 1.000000000000000000, 0.8660254037844387076, 1.000000000000000000, 0.8660254037844387076, 1.000000000000000000, 0.8660254037844387076, 1.000000000000000000, 0.8660254037844387076, 1.000000000000000000, 0.8660254037844387076, 1.000000000000000000, 0.8660254037844387076, 1.000000000000000000, 0.8660254037844387076, 1.000000000000000000, 0.8660254037844387076, 1.000000000000000000, 0.8660254037844387076, 1.000000000000000000, 0.8660254037844387076, 1.000000000000000000, 0.8660254037844387076, 1.000000000000000000, 0.8660254037844387076, 1.000000000000000000, 0.8660254037844387076, 1.000000000000000000, 0.8660254037844387076, 1.000000000000000000, 0.8660254037844387076, 1.000000000000000000, 0.8660254037844387076, 1.000000000000000000, 0.8660254037844387076, 1.000000000000000000, 0.8660254037844387076, 1.000000000000000000, 0.8660254037844387076, 1.000000000000000000, 0.8660254037844387076, 1.000000000000000000, 0.8660254037844387076, 1.000000000000000000, 0.8660254037844387076, 1.000000000000000000, 0.8660254037844387076, 1.000000000000000000, 0.8660254037844387076, 1.000000000000000000, 0.8660254037844387076, 1.000000000000000000, 0.8660254037844387076, 1.000000000000000000, 0.8660254037844387076, 1.000000000000000000, 0.8660254037844387076, 1.000000000000000000, 0.8660254037844387076, 1.000000000000000000, 0.8660254037844387076, 1.000000000000000000, 0.8660254037844387076, 1.000000000000000000, 0.8660254037844387076, 1.000000000000000000, 0.8660254037844387076, 1.000000000000000000, 0.8660254037844387076, 1.000000000000000000, 0.8660254037844387076, 1.000000000000000000, 0.8660254037844387076, 1.000000000000000000, 0.8660254037844387076, 1.000000000000000000, 0.8660254037844387076, 1.000000000000000000, 0.8660254037844387076, 1.000000000000000000, 0.8660254037844387076, 1.000000000000000000, 0.8660254037844387076, 1.000000000000000000, 0.8660254037844387076, 1.000000000000000000, 0.8660254037844387076, 1.000000000000000000, 0.8660254037844387076, 1.000000000000000000, 0.8660254037844387076, 1.000000000000000000, 0.8660254037844387076, 1.000000000000000000, 0.8660254037844387076, 1.000000000000000000, 0.8660254037844387076, 1.000000000000000000, 0.8660254037844387076, 1.000000000000000000, 0.8660254037844387076, 1.000000000000000000, 0.8660254037844387076, 1.000000000000000000, 0.8660254037844387076, 1.000000000000000000, 0.8660254037844387076, 1.000000000000000000, 0.8660254037844387076, 1.000000000000000000, 0.8660254037844387076, 1.000000000000000000, 0.8660254037844387076, 1.000000000000000000, 0.8660254037844387076, 1.000000000000000000, 0.8660254037844387076, 1.000000000000000000, 0.8660254037844387076, 1.000000000000000000, 0.8660254037844387076, 1.000000000000000000, 0.8660254037844387076, 1.000000000000000000, 0.8660254037844387076, 1.000000000000000000, 0.8660254037844387076, 1.000000000000000000, 0.8660254037844387076, 1.000000000000000000, 0.8660254037844387076, 1.000000000000000000, 0.8660254037844387076, 1.000000000000000000, 0.8660254037844387076, 1.000000000000000000, 0.8660254037844387076, 1.000000000000000000, 0.8660254037844387076, 1.000000000000000000, 0.8660254037844387076, 1.000000000000000000, 0.8660254037844387076, 1.000000000000000000, 0.8660254037844387076, 1.000000000000000000, 0.8660254037844387076, 1.000000000000000000, 0.8660254037844387076, 1.000000000000000000, 0.8660254037844387076, 1.000000000000000000, 0.8660254037844387076, 1.000000000000000000, 0.8660254037844387076, 1.000000000000000000, 0.8660254037844387076, 1.000000000000000000, 0.8660254037844387076, 1.000000000000000000, 0.8660254037844387076, 1.000000000000000000, 0.8660254037844387076, 1.000000000000000000, 0.8660254037844387076, 1.000000000000000000, 0.8660254037844387076, 1.000000000000000000, 0.8660254037844387076, 1.000000000000000000, 0.8660254037844387076, 1.000000000000000000, 0.8660254037844387076, 1.000000000000000000, 0.8660254037844387076, 1.000000000000000000, 0.8660254037844387076, 1.000000000000000000, 0.8660254037844387076, 1.000000000000000000, 0.8660254037844387076, 1.000000000000000000, 0.8660254037844387076, 1.000000000000000000, 0.8660254037844387076, 1.000000000000000000, 0.8660254037844387076, 1.000000000000000000, 0.8660254037844387076, 1.000000000000000000, 0.8660254037844387076, 1.000000000000000000, 0.8660254037844387076, 1.000000000000000000, 0.8660254037844387076, 1.000000000000000000, 0.8660254037844387076, 1.000000000000000000, 0.8660254037844387076, 1.000000000000000000, 0.8660254037844387076, 1.000000000000000000, 0.8660254037844387076, 1.000000000000000000, 0.8660254037844387076, 1.000000000000000000, 0.8660254037844387076, 1.000000000000000000, 0.8660254037844387076, 1.000000000000000000, 0.8660254037844387076, 1.000000000000000000, 0.8660254037844387076, 1.000000000000000000, 0.8660254037844387076, 1.000000000000000000, 0.8660254037844387076, 1.000000000000000000, 0.8660254037844387076, 1.000000000000000000, 0.8660254037844387076, 1.000000000000000000, 0.8660254037844387076, 1.000000000000000000, 0.8660254037844387076, 1.000000000000000000, 0.8660254037844387076, 1.000000000000000000, 0.8660254037844387076, 1.000000000000000000, 0.8660254037844387076, 1.000000000000000000, 0.8660254037844387076, 1.000000000000000000, 0.8660254037844387076, 1.000000000000000000, 0.8660254037844387076, 1.000000000000000000, 0.8660254037844387076, 1.000000000000000000, 0.8660254037844387076, 1.000000000000000000, 0.8660254037844387076, 1.000000000000000000, 0.8660254037844387076, 1.000000000000000000, 0.8660254037844387076, 1.000000000000000000, 0.8660254037844387076, 1.000000000000000000, 0.8660254037844387076, 1.000000000000000000, 0.8660254037844387076, 1.000000000000000000, 0.8660254037844387076, 1.000000000000000000, 0.8660254037844387076, 1.000000000000000000, 0.8660254037844387076, 1.000000000000000000, 0.8660254037844387076, 1.000000000000000000, 0.8660254037844387076, 1.000000000000000000, 0.8660254037844387076, 1.000000000000000000, 0.8660254037844387076, 1.000000000000000000, 0.8660254037844387076, 1.000000000000000000, 0.8660254037844387076, 1.000000000000000000, 0.8660254037844387076, 1.000000000000000000, 0.8660254037844387076, 1.000000000000000000, 0.8660254037844387076, 1.000000000000000000, 0.8660254037844387076, 1.000000000000000000, 0.8660254037844387076, 1.000000000000000000, 0.8660254037844387076, 1.000000000000000000, 0.8660254037844387076, 1.000000000000000000, 0.8660254037844387076, 1.000000000000000000, 0.8660254037844387076, 1.000000000000000000, 0.8660254037844387076, 1.000000000000000000, 0.8660254037844387076, 1.000000000000000000, 0.8660254037844387076, 1.000000000000000000, 0.8660254037844387076, 1.000000000000000000, 0.8660254037844387076, 1.000000000000000000, 0.8660254037844387076, 1.000000000000000000, 0.8660254037844387076, 1.000000000000000000, 0.8660254037844387076, 1.000000000000000000, 0.8660254037844387076, 1.000000000000000000, 0.8660254037844387076, 1.000000000000000000, 0.8660254037844387076, 1.000000000000000000, 0.8660254037844387076, 1.000000000000000000, 0.8660254037844387076, 1.000000000000000000, 0.8660254037844387076, 1.000000000000000000, 0.8660254037844387076, 1.000000000000000000, 0.8660254037844387076, 1.000000000000000000, 0.8660254037844387076, 1.000000000000000000, 0.8660254037844387076, 1.000000000000000000, 0.8660254037844387076, 1.000000000000000000, 0.8660254037844387076, 1.000000000000000000, 0.8660254037844387076, 1.000000000000000000, 0.8660254037844387076, 1.000000000000000000, 0.8660254037844387076, 1.000000000000000000, 0.8660254037844387076, 1.000000000000000000, 0.8660254037844387076, 1.000000000000000000, 0.8660254037844387076, 1.000000000000000000, 0.8660254037844387076, 1.000000000000000000, 0.8660254037844387076, 1.000000000000000000, 0.8660254037844387076, 1.000000000000000000, 0.8660254037844387076, 1.000000000000000000, 0.8660254037844387076, 1.000000000000000000, 0.8660254037844387076, 1.000000000000000000, 0.8660254037844387076, 1.000000000000000000, 0.8660254037844387076, 1.000000000000000000, 0.8660254037844387076, 1.000000000000000000, 0.8660254037844387076, 1.000000000000000000, 0.8660254037844387076, 1.000000000000000000, 0.8660254037844387076, 1.000000000000000000, 0.8660254037844387076, 1.000000000000000000, 0.8660254037844387076, 1.000000000000000000, 0.8660254037844387076, 1.000000000000000000, 0.8660254037844387076, 1.000000000000000000, 0.8660254037844387076, 1.000000000000000000, 0.8660254037844387076, 1.000000000000000000, 0.8660254037844387076, 1.000000000000000000, 0.8660254037844387076, 1.000000000000000000, 0.8660254037844387076, 1.000000000000000000, 0.8660254037844387076, 1.000000000000000000, 0.8660254037844387076, 1.000000000000000000, 0.8660254037844387076, 1.000000000000000000, 0.8660254037844387076, 1.000000000000000000, 0.8660254037844387076, 1.000000000000000000, 0.8660254037844387076, 1.000000000000000000, 0.8660254037844387076, 1.000000000000000000, 0.8660254037844387076, 1.000000000000000000, 0.8660254037844387076, 1.000000000000000000, 0.8660254037844387076, 1.000000000000000000, 0.8660254037844387076, 1.000000000000000000, 0.8660254037844387076, 1.000000000000000000, 0.8660254037844387076, 1.000000000000000000, 0.8660254037844387076, 1.000000000000000000, 0.8660254037844387076, 1.000000000000000000, 0.8660254037844387076, 1.000000000000000000, 0.8660254037844387076, 1.000000000000000000, 0.8660254037844387076, 1.000000000000000000, 0.8660254037844387076, 1.000000000000000000, 0.8660254037844387076, 1.000000000000000000, 0.8660254037844387076, 1.000000000000000000, 0.8660254037844387076, 1.000000000000000000, 0.8660254037844387076, 1.000000000000000000, 0.8660254037844387076, 1.000000000000000000, 0.8660254037844387076, 1.000000000000000000, 0.8660254037844387076, 1.000000000000000000, 0.8660254037844387076, 1.000000000000000000, 0.8660254037844387076, 1.000000000000000000, 0.8660254037844387076, 1.000000000000000000, 0.8660254037844387076, 1.000000000000000000, 0.8660254037844387076, 1.000000000000000000, 0.8660254037844387076, 1.000000000000000000, 0.8660254037844387076, 1.000000000000000000, 0.8660254037844387076, 1.000000000000000000, 0.8660254037844387076, 1.000000000000000000, 0.8660254037844387076, 1.000000000000000000, 0.8660254037844387076, 1.000000000000000000, 0.8660254037844387076, 1.000000000000000000, 0.8660254037844387076, 1.000000000000000000, 0.8660254037844387076, 1.000000000000000000, 0.8660254037844387076, 1.000000000000000000, 0.8660254037844387076, 1.000000000000000000, 0.8660254037844387076, 1.000000000000000000, 0.8660254037844387076, 1.000000000000000000, 0.8660254037844387076, 1.000000000000000000, 0.8660254037844387076, 1.000000000000000000, 0.8660254037844387076, 1.000000000000000000, 0.8660254037844387076, 1.000000000000000000, 0.8660254037844387076, 1.000000000000000000, 0.8660254037844387076, 1.000000000000000000, 0.8660254037844387076, 1.000000000000000000, 0.8660254037844387076, 1.000000000000000000, 0.8660254037844387076, 1.000000000000000000, 0.8660254037844387076, 1.000000000000000000, 0.8660254037844387076, 1.000000000000000000, 0.8660254037844387076, 1.000000000000000000, 0.8660254037844387076, 1.000000000000000000, 0.8660254037844387076, 1.000000000000000000, 0.8660254037844387076, 1.000000000000000000, 0.8660254037844387076, 1.000000000000000000, 0.8660254037844387076, 1.000000000000000000, 0.8660254037844387076, 1.000000000000000000, 0.8660254037844387076, 1.000000000000000000, 0.8660254037844387076, 1.000000000000000000, 0.8660254037844387076, 1.000000000000000000, 0.8660254037844387076, 1.000000000000000000, 0.8660254037844387076, 1.000000000000000000, 0.8660254037844387076, 1.000000000000000000, 0.8660254037844387076, 1.000000000000000000, 0.8660254037844387076, 1.000000000000000000, 0.8660254037844387076, 1.000000000000000000, 0.8660254037844387076, 1.000000000000000000, 0.8660254037844387076, 1.000000000000000000, 0.8660254037844387076, 1.000000000000000000, 0.8660254037844387076, 1.000000000000000000, 0.8660254037844387076, 1.000000000000000000, 0.8660254037844387076, 1.000000000000000000, 0.8660254037844387076, 1.000000000000000000, 0.8660254037844387076, 1.000000000000000000, 0.8660254037844387076, 1.000000000000000000, 0.8660254037844387076, 1.000000000000000000, 0.8660254037844387076, 1.000000000000000000, 0.8660254037844387076, 1.000000000000000000, 0.8660254037844387076, 1.000000000000000000, 0.8660254037844387076, 1.000000000000000000, 0.8660254037844387076, 1.000000000000000000, 0.8660254037844387076, 1.000000000000000000, 0.8660254037844387076, 1.000000000000000000, 0.8660254037844387076, 1.000000000000000000, 0.8660254037844387076, 1.000000000000000000, 0.8660254037844387076, 1.000000000000000000, 0.8660254037844387076, 1.000000000000000000, 0.8660254037844387076, 1.000000000000000000, 0.8660254037844387076, 1.000000000000000000, 0.8660254037844387076, 1.000000000000000000, 0.8660254037844387076, 1.000000000000000000, 0.8660254037844387076, 1.000000000000000000, 0.8660254037844387076, 1.000000000000000000, 0.8660254037844387076, 1.000000000000000000, 0.8660254037844387076, 1.000000000000000000, 0.8660254037844387076, 1.000000000000000000, 0.8660254037844387076, 1.000000000000000000, 0.8660254037844387076, 1.000000000000000000, 0.8660254037844387076, 1.000000000000000000, 0.8660254037844387076, 1.000000000000000000, 0.8660254037844387076, 1.000000000000000000, 0.8660254037844387076, 1.000000000000000000, 0.8660254037844387076, 1.000000000000000000, 0.8660254037844387076, 1.000000000000000000, 0.8660254037844387076, 1.000000000000000000, 0.8660254037844387076, 1.000000000000000000, 0.8660254037844387076, 1.000000000000000000, 0.8660254037844387076, 1.000000000000000000, 0.8660254037844387076, 1.000000000000000000, 0.8660254037844387076, 1.000000000000000000, 0.8660254037844387076, 1.000000000000000000, 0.8660254037844387076, 1.000000000000000000, 0.8660254037844387076, 1.000000000000000000, 0.8660254037844387076, 1.000000000000000000, 0.8660254037844387076, 1.000000000000000000, 0.8660254037844387076, 1.000000000000000000, 0.8660254037844387076, 1.000000000000000000, 0.8660254037844387076, 1.000000000000000000, 0.8660254037844387076, 1.000000000000000000, 0.8660254037844387076, 1.000000000000000000, 0.8660254037844387076, 1.000000000000000000, 0.8660254037844387076, 1.000000000000000000, 0.8660254037844387076, 1.000000000000000000, 0.8660254037844387076, 1.000000000000000000, 0.8660254037844387076, 1.000000000000000000, 0.8660254037844387076, 1.000000000000000000, 0.8660254037844387076, 1.000000000000000000, 0.8660254037844387076, 1.000000000000000000, 0.8660254037844387076, 1.000000000000000000, 0.8660254037844387076, 1.000000000000000000, 0.8660254037844387076, 1.000000000000000000, 0.8660254037844387076, 1.000000000000000000, 0.8660254037844387076, 1.000000000000000000, 0.8660254037844387076, 1.000000000000000000, 0.8660254037844387076, 1.000000000000000000, 0.8660254037844387076, 1.000000000000000000, 0.8660254037844387076, 1.000000000000000000, 0.8660254037844387076, 1.000000000000000000, 0.8660254037844387076, 1.000000000000000000, 0.8660254037844387076, 1.000000000000000000, 0.8660254037844387076, 1.000000000000000000, 0.8660254037844387076, 1.000000000000000000, 0.8660254037844387076, 1.000000000000000000, 0.8660254037844387076, 1.000000000000000000, 0.8660254037844387076, 1.000000000000000000, 0.8660254037844387076, 1.000000000000000000, 0.8660254037844387076, 1.000000000000000000, 0.8660254037844387076, 1.000000000000000000, 0.8660254037844387076, 1.000000000000000000, 0.8660254037844387076, 1.000000000000000000, 0.8660254037844387076, 1.000000000000000000, 0.8660254037844387076, 1.000000000000000000, 0.8660254037844387076, 1.000000000000000000, 0.8660254037844387076, 1.000000000000000000, 0.8660254037844387076, 1.000000000000000000, 0.8660254037844387076, 1.000000000000000000, 0.8660254037844387076, 1.000000000000000000, 0.8660254037844387076, 1.000000000000000000, 0.8660254037844387076, 1.000000000000000000, 0.8660254037844387076, 1.000000000000000000, 0.8660254037844387076, 1.000000000000000000, 0.8660254037844387076, 1.000000000000000000, 0.8660254037844387076, 1.000000000000000000, 0.8660254037844387076, 1.000000000000000000, 0.8660254037844387076, 1.000000000000000000, 0.8660254037844387076, 1.000000000000000000, 0.8660254037844387076, 1.000000000000000000, 0.8660254037844387076, 1.000000000000000000, 0.8660254037844387076, 1.000000000000000000, 0.8660254037844387076, 1.000000000000000000, 0.8660254037844387076, 1.000000000000000000, 0.8660254037844387076, 1.000000000000000000, 0.8660254037844387076, 1.000000000000000000, 0.8660254037844387076, 1.000000000000000000, 0.8660254037844387076, 1.000000000000000000, 0.8660254037844387076, 1.000000000000000000, 0.8660254037844387076, 1.000000000000000000, 0.8660254037844387076, 1.000000000000000000, 0.8660254037844387076, 1.000000000000000000, 0.8660254037844387076, 1.000000000000000000, 0.8660254037844387076, 1.000000000000000000, 0.8660254037844387076, 1.000000000000000000, 0.8660254037844387076, 1.000000000000000000, 0.8660254037844387076, 1.000000000000000000, 0.8660254037844387076, 1.000000000000000000, 0.8660254037844387076, 1.000000000000000000, 0.8660254037844387076, 1.000000000000000000, 0.8660254037844387076, 1.000000000000000000, 0.8660254037844387076, 1.000000000000000000, 0.8660254037844387076, 1.000000000000000000, 0.8660254037844387076, 1.000000000000000000, 0.8660254037844387076, 1.000000000000000000, 0.8660254037844387076, 1.000000000000000000, 0.8660254037844387076, 1.000000000000000000, 0.8660254037844387076, 1.000000000000000000, 0.8660254037844387076, 1.000000000000000000, 0.8660254037844387076, 1.000000000000000000, 0.8660254037844387076, 1.000000000000000000, 0.8660254037844387076, 1.000000000000000000, 0.8660254037844387076, 1.000000000000000000, 0.8660254037844387076, 1.000000000000000000, 0.8660254037844387076, 1.000000000000000000, 0.8660254037844387076, 1.000000000000000000, 0.8660254037844387076, 1.000000000000000000, 0.8660254037844387076, 1.000000000000000000, 0.8660254037844387076, 1.000000000000000000, 0.8660254037844387076, 1.000000000000000000, 0.8660254037844387076, 1.000000000000000000, 0.8660254037844387076, 1.000000000000000000, 0.8660254037844387076, 1.000000000000000000, 0.8660254037844387076, 1.000000000000000000, 0.8660254037844387076, 1.000000000000000000, 0.8660254037844387076, 1.000000000000000000, 0.8660254037844387076, 1.000000000000000000, 0.8660254037844387076, 1.000000000000000000, 0.8660254037844387076, 1.000000000000000000, 0.8660254037844387076, 1.000000000000000000, 0.8660254037844387076, 1.000000000000000000, 0.8660254037844387076, 1.000000000000000000, 0.8660254037844387076, 1.000000000000000000, 0.8660254037844387076, 1.000000000000000000, 0.8660254037844387076, 1.000000000000000000, 0.8660254037844387076, 1.000000000000000000, 0.8660254037844387076, 1.000000000000000000, 0.8660254037844387076, 1.000000000000000000, 0.8660254037844387076, 1.000000000000000000, 0.8660254037844387076, 1.000000000000000000, 0.8660254037844387076, 1.000000000000000000, 0.8660254037844387076, 1.000000000000000000, 0.8660254037844387076, 1.000000000000000000, 0.8660254037844387076, 1.000000000000000000, 0.8660254037844387076, 1.000000000000000000, 0.8660254037844387076, 1.000000000000000000, 0.8660254037844387076, 1.000000000000000000, 0.8660254037844387076, 1.000000000000000000, 0.8660254037844387076, 1.000000000000000000, 0.8660254037844387076, 1.000000000000000000, 0.8660254037844387076, 1.000000000000000000, 0.8660254037844387076, 1.000000000000000000, 0.8660254037844387076, 1.000000000000000000, 0.8660254037844387076, 1.000000000000000000, 0.8660254037844387076, 1.000000000000000000, 0.8660254037844387076, 1.000000000000000000, 0.8660254037844387076, 1.000000000000000000, 0.8660254037844387076, 1.000000000000000000, 0.8660254037844387076, 1.000000000000000000, 0.8660254037844387076, 1.000000000000000000, 0.8660254037844387076, 1.000000000000000000, 0.8660254037844387076, 1.000000000000000000, 0.8660254037844387076, 1.000000000000000000, 0.8660254037844387076, 1.000000000000000000, 0.8660254037844387076, 1.000000000000000000, 0.8660254037844387076, 1.000000000000000000, 0.8660254037844387076, 1.000000000000000000, 0.8660254037844387076, 1.000000000000000000, 0.8660254037844387076, 1.000000000000000000, 0.8660254037844387076, 1.000000000000000000, 0.8660254037844387076, 1.000000000000000000, 0.8660254037844387076, 1.000000000000000000, 0.8660254037844387076, 1.000000000000000000, 0.8660254037844387076, 1.000000000000000000, 0.8660254037844387076, 1.000000000000000000, 0.8660254037844387076, 1.000000000000000000, 0.8660254037844387076, 1.000000000000000000, 0.8660254037844387076, 1.000000000000000000, 0.8660254037844387076, 1.000000000000000000, 0.8660254037844387076, 1.000000000000000000, 0.8660254037844387076, 1.000000000000000000, 0.8660254037844387076, 1.000000000000000000, 0.8660254037844387076, 1.000000000000000000, 0.8660254037844387076, 1.000000000000000000, 0.8660254037844387076, 1.000000000000000000, 0.8660254037844387076, 1.000000000000000000, 0.8660254037844387076, 1.000000000000000000, 0.8660254037844387076, 1.000000000000000000, 0.8660254037844387076, 1.000000000000000000, 0.8660254037844387076, 1.000000000000000000, 0.8660254037844387076, 1.000000000000000000, 0.8660254037844387076, 1.000000000000000000, 0.8660254037844387076, 1.000000000000000000, 0.8660254037844387076, 1.000000000000000000, 0.8660254037844387076, 1.000000000000000000, 0.8660254037844387076, 1.000000000000000000, 0.8660254037844387076, 1.000000000000000000, 0.8660254037844387076, 1.000000000000000000, 0.8660254037844387076, 1.000000000000000000, 0.8660254037844387076, 1.000000000000000000, 0.8660254037844387076, 1.000000000000000000, 0.8660254037844387076, 1.000000000000000000, 0.8660254037844387076, 1.000000000000000000, 0.8660254037844387076, 1.000000000000000000, 0.8660254037844387076, 1.000000000000000000, 0.8660254037844387076, 1.000000000000000000, 0.8660254037844387076, 1.000000000000000000, 0.8660254037844387076, 1.000000000000000000, 0.8660254037844387076, 1.000000000000000000, 0.8660254037844387076, 1.000000000000000000, 0.8660254037844387076, 1.000000000000000000, 0.8660254037844387076, 1.000000000000000000, 0.8660254037844387076, 1.000000000000000000, 0.8660254037844387076, 1.000000000000000000, 0.8660254037844387076, 1.000000000000000000, 0.8660254037844387076, 1.000000000000000000, 0.8660254037844387076, 1.000000000000000000, 0.8660254037844387076, 1.000000000000000000, 0.8660254037844387076, 1.000000000000000000, 0.8660254037844387076, 1.000000000000000000, 0.8660254037844387076, 1.000000000000000000, 0.8660254037844387076, 1.000000000000000000, 0.8660254037844387076, 1.000000000000000000, 0.8660254037844387076, 1.000000000000000000, 0.8660254037844387076, 1.000000000000000000, 0.8660254037844387076, 1.000000000000000000, 0.8660254037844387076, 1.000000000000000000, 0.8660254037844387076, 1.000000000000000000, 0.8660254037844387076, 1.000000000000000000, 0.8660254037844387076, 1.000000000000000000, 0.8660254037844387076, 1.000000000000000000, 0.8660254037844387076, 1.000000000000000000, 0.8660254037844387076, 1.000000000000000000, 0.8660254037844387076, 1.000000000000000000, 0.8660254037844387076, 1.000000000000000000, 0.8660254037844387076, 1.000000000000000000, 0.8660254037844387076, 1.000000000000000000, 0.8660254037844387076, 1.000000000000000000, 0.8660254037844387076, 1.000000000000000000, 0.8660254037844387076, 1.000000000000000000, 0.8660254037844387076, 1.000000000000000000, 0.8660254037844387076, 1.000000000000000000, 0.8660254037844387076, 1.000000000000000000, 0.8660254037844387076, 1.000000000000000000, 0.8660254037844387076, 1.000000000000000000, 0.8660254037844387076, 1.000000000000000000, 0.8660254037844387076, 1.000000000000000000, 0.8660254037844387076, 1.000000000000000000, 0.8660254037844387076, 1.000000000000000000, 0.8660254037844387076, 1.000000000000000000) ) ) 
 REPRESENTATION_ITEM ( '' )  SURFACE ( )  );
#1063 = CARTESIAN_POINT ( 'NONE',  ( -2.293366432827344421E-15, -12.48450537969573659, -169.9062500020483810 ) ) ;
#1064 = CARTESIAN_POINT ( 'NONE',  ( 7.216878364870408014, 17.50000000000005684, 49.99999999999998579 ) ) ;
#1065 = EDGE_CURVE ( 'NONE', #26359, #40867, #25993, .T. ) ;
#1066 = CARTESIAN_POINT ( 'NONE',  ( -10.81189881249999729, -6.242252689847864744, -124.9687500020483810 ) ) ;
#1067 = CARTESIAN_POINT ( 'NONE',  ( -5.405949406249996869, 9.363379034771805109, -93.84375000204838102 ) ) ;
#1068 = CARTESIAN_POINT ( 'NONE',  ( 9.999999999999998224, 0.000000000000000000, -106.9999999999999858 ) ) ;
#1069 = CARTESIAN_POINT ( 'NONE',  ( -5.405949406249996869, 9.363379034771805109, -104.5312500020483810 ) ) ;
#1070 = CARTESIAN_POINT ( 'NONE',  ( 7.070501591499377789E-16, 11.54700538379251284, -183.5000000040968189 ) ) ;
#1071 = CARTESIAN_POINT ( 'NONE',  ( 10.81189881249999729, 6.242252689847867408, -107.7187500020483810 ) ) ;
#1072 = CARTESIAN_POINT ( 'NONE',  ( -5.405949406249996869, 9.363379034771805109, -179.5312500020483810 ) ) ;
#1073 = DIRECTION ( 'NONE',  ( -0.000000000000000000, -0.000000000000000000, 1.000000000000000000 ) ) ;
#1074 = CARTESIAN_POINT ( 'NONE',  ( 10.81189881249999551, -6.242252689847874514, -198.1562500020484379 ) ) ;
#1075 = CARTESIAN_POINT ( 'NONE',  ( 10.81189881249999551, -6.242252689847874514, -55.46875000204837391 ) ) ;
#1076 = CARTESIAN_POINT ( 'NONE',  ( 5.405949406249992428, -9.363379034771808662, -43.59375000204837391 ) ) ;
#1077 = CARTESIAN_POINT ( 'NONE',  ( 5.000000000000000000, 8.660254037844385522, -176.1250000040968189 ) ) ;
#1078 = CARTESIAN_POINT ( 'NONE',  ( 7.644554776091147741E-16, 12.48450537969573659, -11.65625000204835438 ) ) ;
#1079 = CARTESIAN_POINT ( 'NONE',  ( 7.644554776091147741E-16, 12.48450537969573659, -18.96875000204837036 ) ) ;
#1080 = DIRECTION ( 'NONE',  ( -0.000000000000000000, -0.000000000000000000, -1.000000000000000000 ) ) ;
#1081 = CARTESIAN_POINT ( 'NONE',  ( -10.81189881249999729, 6.242252689847871849, -132.7187500020483810 ) ) ;
#1082 = CARTESIAN_POINT ( 'NONE',  ( -4.999999999999996447, 8.660254037844387298, -97.49999999999998579 ) ) ;
#1083 = CARTESIAN_POINT ( 'NONE',  ( 10.81189881249999729, 0.000000000000000000, -31.53125000204837391 ) ) ;
#1084 = CARTESIAN_POINT ( 'NONE',  ( 9.999999999999998224, 0.000000000000000000, -111.8750000040967763 ) ) ;
#1085 = CARTESIAN_POINT ( 'NONE',  ( 10.00000000000102318, -5.773502691895667560, -26.50000000409674783 ) ) ;
#1086 = CARTESIAN_POINT ( 'NONE',  ( -9.999999999999998224, 5.773502691896259087, -61.37499999999998579 ) ) ;
#1087 = CARTESIAN_POINT ( 'NONE',  ( 7.644554776091147741E-16, 12.48450537969573659, -127.1562500020483952 ) ) ;
#1088 = CARTESIAN_POINT ( 'NONE',  ( -10.81189881249999729, 6.242252689847871849, -104.4062500020483810 ) ) ;
#1089 = ORIENTED_EDGE ( 'NONE', *, *, #19593, .T. ) ;
#1090 = CARTESIAN_POINT ( 'NONE',  ( -9.999999999999998224, 0.000000000000000000, -99.99999999999998579 ) ) ;
#1091 = CARTESIAN_POINT ( 'NONE',  ( 4.999999999999992006, -8.660254037844389075, -97.12500000409677625 ) ) ;
#1092 = CARTESIAN_POINT ( 'NONE',  ( 10.00000000000051159, -5.773502691895965988, -151.0000000040967905 ) ) ;
#1093 = CARTESIAN_POINT ( 'NONE',  ( 5.405949406249999534, 9.363379034771803333, -59.59375000204835970 ) ) ;
#1094 = VERTEX_POINT ( 'NONE', #3320 ) ;
#1095 = CARTESIAN_POINT ( 'NONE',  ( 9.999999999999996447, -5.773502691896262640, -23.12499999999998224 ) ) ;
#1096 = CARTESIAN_POINT ( 'NONE',  ( -10.81189881249999729, -6.242252689847864744, -38.15625000204835260 ) ) ;
#1097 = CARTESIAN_POINT ( 'NONE',  ( -2.121150477449813534E-15, -11.54700538379251284, -159.8750000000000000 ) ) ;
#1098 = CARTESIAN_POINT ( 'NONE',  ( -9.999999999999998224, 1.224646799147353059E-15, -200.0000000000000000 ) ) ;
#1099 = CARTESIAN_POINT ( 'NONE',  ( -10.00000000000000000, -5.773502691896251982, -31.50000000409674783 ) ) ;
#1100 = VECTOR ( 'NONE', #32490, 1000.000000000000000 ) ;
#1101 = VECTOR ( 'NONE', #34234, 1000.000000000000114 ) ;
#1102 = CARTESIAN_POINT ( 'NONE',  ( -10.81189881249999729, 6.242252689847871849, -135.9062500020484094 ) ) ;
#1103 = CARTESIAN_POINT ( 'NONE',  ( -9.999999999999998224, 1.224646799147353059E-15, -110.7499999999999858 ) ) ;
#1104 = CARTESIAN_POINT ( 'NONE',  ( -9.999999999999998224, 1.224646799147353059E-15, -129.1250000040967620 ) ) ;
#1105 = ORIENTED_EDGE ( 'NONE', *, *, #20888, .F. ) ;
#1107 = EDGE_LOOP ( 'NONE', ( #37460, #22915, #24371, #22762 ) ) ;
#1106 = ORIENTED_EDGE ( 'NONE', *, *, #39009, .F. ) ;
#1108 = DIRECTION ( 'NONE',  ( -0.000000000000000000, -0.000000000000000000, -1.000000000000000000 ) ) ;
#1109 = CARTESIAN_POINT ( 'NONE',  ( 10.00000000000051159, -5.773502691895965988, -146.5000000040967620 ) ) ;
#1110 = CARTESIAN_POINT ( 'NONE',  ( -10.81189881249999729, 6.242252689847871849, -168.7187500020483810 ) ) ;
#1111 = CARTESIAN_POINT ( 'NONE',  ( 10.81189881249999551, -6.242252689847874514, -198.1562500020484379 ) ) ;
#1112 = CARTESIAN_POINT ( 'NONE',  ( -10.81189881249999729, 1.324075727343319199E-15, -14.09375000204834905 ) ) ;
#1113 = CARTESIAN_POINT ( 'NONE',  ( -9.999999999999872102, -5.773502691896326589, -157.5000000040968189 ) ) ;
#1114 = EDGE_CURVE ( 'NONE', #36127, #7309, #20938, .T. ) ;
#1115 = CARTESIAN_POINT ( 'NONE',  ( 10.81189881249999729, 6.242252689847867408, -148.2187500020484094 ) ) ;
#1116 = CARTESIAN_POINT ( 'NONE',  ( -5.405949406250003975, -9.363379034771801557, -133.8437500020484094 ) ) ;
#1117 = EDGE_CURVE ( 'NONE', #21693, #23210, #25367, .T. ) ;
#1118 = CARTESIAN_POINT ( 'NONE',  ( -10.81189881249999729, 6.242252689847871849, -108.9062500020483810 ) ) ;
#1119 = CARTESIAN_POINT ( 'NONE',  ( -10.81189881249999907, -6.242252689847864744, -118.9687500020483810 ) ) ;
#1120 = CARTESIAN_POINT ( 'NONE',  ( 10.00000000000000000, 5.773502691896255534, -195.7500000040968189 ) ) ;
#1121 = CIRCLE ( 'NONE', #7312, 20.00000000000000355 ) ;
#1122 = CARTESIAN_POINT ( 'NONE',  ( 10.81189881249999729, 0.000000000000000000, -123.0312500020483952 ) ) ;
#1123 = CARTESIAN_POINT ( 'NONE',  ( 5.405949406249999534, 9.363379034771803333, -8.593750002048345493 ) ) ;
#1124 = CARTESIAN_POINT ( 'NONE',  ( 10.81189881249999729, 0.000000000000000000, -127.3437500020483952 ) ) ;
#1125 = CARTESIAN_POINT ( 'NONE',  ( -10.81189881249999729, 6.242252689847871849, -198.9062500020484094 ) ) ;
#1126 = CARTESIAN_POINT ( 'NONE',  ( -9.999999999999941380, -5.773502691896284844, -196.5000000040967905 ) ) ;
#1127 = CARTESIAN_POINT ( 'NONE',  ( -2.121150477449813534E-15, -11.54700538379251284, -158.3750000000000000 ) ) ;
#1128 = CARTESIAN_POINT ( 'NONE',  ( -9.999999999999998224, 1.224646799147353059E-15, -17.74999999999996092 ) ) ;
#1129 = CARTESIAN_POINT ( 'NONE',  ( -2.293366432827344421E-15, -12.48450537969573659, -75.21875000204839523 ) ) ;
#1130 = CARTESIAN_POINT ( 'NONE',  ( -2.293366432827344421E-15, -12.48450537969573659, -61.71875000204838102 ) ) ;
#1131 = CARTESIAN_POINT ( 'NONE',  ( 10.00000000000025402, -5.773502691896113426, -158.5000000040968473 ) ) ;
#1132 = CARTESIAN_POINT ( 'NONE',  ( -5.405949406250003975, -9.363379034771801557, -38.03125000204838102 ) ) ;
#1133 = CARTESIAN_POINT ( 'NONE',  ( -5.405949406249996869, 9.363379034771805109, -42.84375000204837391 ) ) ;
#1134 = CARTESIAN_POINT ( 'NONE',  ( 9.999999999999676703, 5.773502691896441164, -186.3749999999999716 ) ) ;
#1135 = CARTESIAN_POINT ( 'NONE',  ( -10.81189881249999729, 6.242252689847871849, -150.7187500020483810 ) ) ;
#1136 = CARTESIAN_POINT ( 'NONE',  ( -10.00000000000000000, -5.773502691896251982, -121.1250000000000000 ) ) ;
#1137 = CARTESIAN_POINT ( 'NONE',  ( 10.81189881249999551, -6.242252689847874514, -129.1562500020483810 ) ) ;
#1138 = CARTESIAN_POINT ( 'NONE',  ( 7.564846744322244021, 7.391372818874605066, -180.0000000000000284 ) ) ;
#1139 = CARTESIAN_POINT ( 'NONE',  ( -5.000000000000003553, -8.660254037844383745, -83.49999999999997158 ) ) ;
#1140 = CARTESIAN_POINT ( 'NONE',  ( 5.405949406249992428, -9.363379034771808662, -15.28125000204835793 ) ) ;
#1141 = ORIENTED_EDGE ( 'NONE', *, *, #16442, .T. ) ;
#1142 = CARTESIAN_POINT ( 'NONE',  ( -2.293366432827344421E-15, -12.48450537969573659, -105.4062500020483810 ) ) ;
#1143 = CARTESIAN_POINT ( 'NONE',  ( 9.999999999999996447, -5.773502691896262640, -121.0000000040967905 ) ) ;
#1144 = CARTESIAN_POINT ( 'NONE',  ( -9.999999999999998224, 1.224646799147353059E-15, -154.6250000040967905 ) ) ;
#1145 = CARTESIAN_POINT ( 'NONE',  ( 7.070501591499377789E-16, 11.54700538379251284, -30.50000000409674428 ) ) ;
#1146 = EDGE_CURVE ( 'NONE', #1053, #28503, #9337, .T. ) ;
#1147 = DIRECTION ( 'NONE',  ( -0.000000000000000000, -0.000000000000000000, 1.000000000000000000 ) ) ;
#1148 = CARTESIAN_POINT ( 'NONE',  ( -5.405949406250003975, -9.363379034771801557, -53.03125000204836681 ) ) ;
#1149 = CARTESIAN_POINT ( 'NONE',  ( 4.999999999999992006, -8.660254037844389075, -135.7499999999999716 ) ) ;
#1150 = CARTESIAN_POINT ( 'NONE',  ( -10.81189881249999729, 1.324075727343319199E-15, -152.2812500020484094 ) ) ;
#1151 = CARTESIAN_POINT ( 'NONE',  ( 7.644554776091147741E-16, 12.48450537969573659, -128.4687500020483810 ) ) ;
#1152 = CARTESIAN_POINT ( 'NONE',  ( -9.999999999999998224, 1.224646799147353059E-15, -178.6250000040968189 ) ) ;
#1153 = EDGE_CURVE ( 'NONE', #2376, #36659, #12347, .T. ) ;
#1154 = EDGE_CURVE ( 'NONE', #530, #15993, #14272, .T. ) ;
#1155 = ORIENTED_EDGE ( 'NONE', *, *, #36440, .T. ) ;
#1156 =( BOUNDED_CURVE ( )  B_SPLINE_CURVE ( 2, ( #33824, #34256, #7918, #20635, #8132, #1445, #30162 ),
 .UNSPECIFIED., .F., .F. ) 
 B_SPLINE_CURVE_WITH_KNOTS ( ( 3, 2, 2, 3 ),
 ( 0.5410447761194030480, 0.5422885572139304333, 0.5435323383084578186, 0.5447761194029852039 ),
 .UNSPECIFIED. ) 
 CURVE ( )  GEOMETRIC_REPRESENTATION_ITEM ( )  RATIONAL_B_SPLINE_CURVE ( ( 0.9999999999999880096, 0.8660254037844506980, 1.000000000000000000, 0.8660254037844387076, 1.000000000000000000, 0.8660254037844267172, 1.000000000000011990 ) ) 
 REPRESENTATION_ITEM ( '' )  );
#1157 = CARTESIAN_POINT ( 'NONE',  ( -45.00000000000000711, 0.000000000000000000, -203.0000000000000000 ) ) ;
#1158 = ORIENTED_EDGE ( 'NONE', *, *, #32558, .F. ) ;
#1159 = ORIENTED_EDGE ( 'NONE', *, *, #42513, .F. ) ;
#1161 = ORIENTED_EDGE ( 'NONE', *, *, #15645, .F. ) ;
#1160 = CARTESIAN_POINT ( 'NONE',  ( -10.81189881249999729, 6.242252689847871849, -111.7187500020483810 ) ) ;
#1162 = CARTESIAN_POINT ( 'NONE',  ( -9.999999999999998224, 1.224646799147353059E-15, -129.1250000040967620 ) ) ;
#1163 = CARTESIAN_POINT ( 'NONE',  ( 10.81189881249999907, 6.242252689847868297, -191.7187500020484094 ) ) ;
#1164 = CARTESIAN_POINT ( 'NONE',  ( -10.81189881249999729, 6.242252689847871849, -42.71875000204835970 ) ) ;
#1165 = CARTESIAN_POINT ( 'NONE',  ( 8.614196012143711556, -6.533971456633876684, 2.775557561562891351E-14 ) ) ;
#1166 = CARTESIAN_POINT ( 'NONE',  ( -9.999999999999998224, 1.224646799147353059E-15, -186.1250000040967905 ) ) ;
#1167 = EDGE_CURVE ( 'NONE', #36659, #35302, #38582, .T. ) ;
#1168 = CARTESIAN_POINT ( 'NONE',  ( 10.81189881249999729, 0.000000000000000000, -169.3437500020484094 ) ) ;
#1169 = CARTESIAN_POINT ( 'NONE',  ( 10.81189881249999551, -6.242252689847874514, -157.4687500020484094 ) ) ;
#1170 = CARTESIAN_POINT ( 'NONE',  ( -60.00000000000000711, 0.000000000000000000, -223.0000000000000000 ) ) ;
#1171 = CARTESIAN_POINT ( 'NONE',  ( -10.81189881249999729, 1.324075727343319199E-15, -144.5937500020483810 ) ) ;
#1173 = ADVANCED_FACE ( 'NONE', ( #14059 ), #17521, .T. ) ;
#1172 = CARTESIAN_POINT ( 'NONE',  ( -5.405949406249996869, 9.363379034771805109, -155.3437500020483810 ) ) ;
#1174 = CARTESIAN_POINT ( 'NONE',  ( -9.999999999999998224, 1.224646799147353059E-15, -133.6250000040967620 ) ) ;
#1175 = CARTESIAN_POINT ( 'NONE',  ( 10.00000000000025402, -5.773502691896113426, -139.0000000040967905 ) ) ;
#1176 = CARTESIAN_POINT ( 'NONE',  ( -10.00000000000000000, -5.773502691896251982, -178.1250000000000284 ) ) ;
#1177 = EDGE_CURVE ( 'NONE', #32541, #42118, #16755, .T. ) ;
#1178 = CARTESIAN_POINT ( 'NONE',  ( -5.405949406250003975, -9.363379034771801557, -90.34375000204838102 ) ) ;
#1179 = CARTESIAN_POINT ( 'NONE',  ( 5.000000000000000000, 8.660254037844385522, -180.6250000040967905 ) ) ;
#1180 = CARTESIAN_POINT ( 'NONE',  ( -2.293366432827344421E-15, -12.48450537969573659, -61.90625000204838813 ) ) ;
#1181 = CARTESIAN_POINT ( 'NONE',  ( -4.999999999999996447, 8.660254037844387298, -145.8750000040967905 ) ) ;
#1182 = CARTESIAN_POINT ( 'NONE',  ( 10.81189881249999729, 0.000000000000000000, -181.3437500020483810 ) ) ;
#1183 = CARTESIAN_POINT ( 'NONE',  ( 10.81189881249999907, 6.242252689847868297, -121.4062500020483810 ) ) ;
#1184 = CARTESIAN_POINT ( 'NONE',  ( -5.405949406250003975, -9.363379034771801557, -155.0312500020484094 ) ) ;
#1185 = LINE ( 'NONE', #16759, #26838 ) ;
#1186 = CARTESIAN_POINT ( 'NONE',  ( 5.405949406249999534, 9.363379034771803333, -41.78125000204838102 ) ) ;
#1187 = CARTESIAN_POINT ( 'NONE',  ( 9.999999999999998224, 0.000000000000000000, -131.3750000040967905 ) ) ;
#1188 = CARTESIAN_POINT ( 'NONE',  ( 7.070501591499377789E-16, 11.54700538379251284, -103.6249999999999858 ) ) ;
#1189 = ORIENTED_EDGE ( 'NONE', *, *, #11626, .T. ) ;
#1190 = CARTESIAN_POINT ( 'NONE',  ( 10.81189881249999551, -6.242252689847874514, -138.1562500020484094 ) ) ;
#1191 = CARTESIAN_POINT ( 'NONE',  ( 9.999999999999998224, 0.000000000000000000, -150.8750000040967905 ) ) ;
#1192 = CARTESIAN_POINT ( 'NONE',  ( -10.81189881249999729, 6.242252689847871849, -146.4062500020484094 ) ) ;
#1193 = CARTESIAN_POINT ( 'NONE',  ( -10.81189881249999907, -6.242252689847864744, -192.6562500020484094 ) ) ;
#1194 = ORIENTED_EDGE ( 'NONE', *, *, #6940, .T. ) ;
#1195 = CARTESIAN_POINT ( 'NONE',  ( -10.00000000000000000, -5.773502691896251982, -46.12499999999996447 ) ) ;
#1196 = CARTESIAN_POINT ( 'NONE',  ( 5.405949406249999534, 9.363379034771803333, -179.5937500020484094 ) ) ;
#1197 = CARTESIAN_POINT ( 'NONE',  ( -10.00000000000000000, -5.773502691896251982, -61.50000000409677625 ) ) ;
#1198 = PLANE ( 'NONE',  #2272 ) ;
#1199 = CARTESIAN_POINT ( 'NONE',  ( 10.81189881249999551, -6.242252689847874514, -73.65625000204836681 ) ) ;
#1200 = CARTESIAN_POINT ( 'NONE',  ( -2.293366432827344421E-15, -12.48450537969573659, -48.40625000204836681 ) ) ;
#1201 = EDGE_CURVE ( 'NONE', #41907, #40786, #11267, .T. ) ;
#1202 =( BOUNDED_CURVE ( )  B_SPLINE_CURVE ( 2, ( #8969, #22135, #35309, #5739, #19512, #22982, #29456 ),
 .UNSPECIFIED., .F., .F. ) 
 B_SPLINE_CURVE_WITH_KNOTS ( ( 3, 2, 2, 3 ),
 ( 0.4291044776119404269, 0.4303482587064677567, 0.4315920398009951975, 0.4328358208955225273 ),
 .UNSPECIFIED. ) 
 CURVE ( )  GEOMETRIC_REPRESENTATION_ITEM ( )  RATIONAL_B_SPLINE_CURVE ( ( 0.9999999999999880096, 0.8660254037844506980, 1.000000000000000000, 0.8660254037844387076, 1.000000000000000000, 0.8660254037844207220, 1.000000000000017986 ) ) 
 REPRESENTATION_ITEM ( '' )  );
#1203 = CARTESIAN_POINT ( 'NONE',  ( 7.070501591499377789E-16, 11.54700538379251284, -56.00000000409676915 ) ) ;
#1204 = MANIFOLD_SOLID_BREP ( 'Fillet1', #25326 ) ;
#1205 = CARTESIAN_POINT ( 'NONE',  ( -5.405949406250003975, -9.363379034771801557, -13.84375000204834905 ) ) ;
#1206 = CARTESIAN_POINT ( 'NONE',  ( 7.644554776091147741E-16, 12.48450537969573659, -173.6562500020483810 ) ) ;
#1207 = CARTESIAN_POINT ( 'NONE',  ( -5.405949406250003975, -9.363379034771801557, -6.531250002048377468 ) ) ;
#1208 = FACE_OUTER_BOUND ( 'NONE', #31158, .T. ) ;
#1209 = CARTESIAN_POINT ( 'NONE',  ( -9.999999999999998224, 1.224646799147353059E-15, -148.2500000000000000 ) ) ;
#1210 = CARTESIAN_POINT ( 'NONE',  ( 9.999999999999742428, 5.773502691896404748, -154.8749999999999716 ) ) ;
#1211 = CYLINDRICAL_SURFACE ( 'NONE', #38312, 9.999999999999998224 ) ;
#1212 =( BOUNDED_CURVE ( )  B_SPLINE_CURVE ( 2, ( #485, #9385, #10375, #13814, #17269, #27005, #40154 ),
 .UNSPECIFIED., .F., .F. ) 
 B_SPLINE_CURVE_WITH_KNOTS ( ( 3, 2, 2, 3 ),
 ( 0.4253731343283583266, 0.4266169154228856564, 0.4278606965174130417, 0.4291044776119404269 ),
 .UNSPECIFIED. ) 
 CURVE ( )  GEOMETRIC_REPRESENTATION_ITEM ( )  RATIONAL_B_SPLINE_CURVE ( ( 0.9999999999999880096, 0.8660254037844506980, 1.000000000000000000, 0.8660254037844387076, 1.000000000000000000, 0.8660254037844267172, 1.000000000000011990 ) ) 
 REPRESENTATION_ITEM ( '' )  );
#1213 = CARTESIAN_POINT ( 'NONE',  ( 4.999999999999992006, -8.660254037844389075, -20.24999999999996092 ) ) ;
#1215 = EDGE_LOOP ( 'NONE', ( #11227, #37033, #21372, #11979 ) ) ;
#1214 = CARTESIAN_POINT ( 'NONE',  ( -10.81189881249999729, 1.324075727343319199E-15, -87.78125000204838102 ) ) ;
#1216 = SHAPE_REPRESENTATION_RELATIONSHIP ( 'NONE' , 'NONE' ,  #40929, #17102 ) ;
#1218 = ORIENTED_EDGE ( 'NONE', *, *, #3677, .T. ) ;
#1217 = CARTESIAN_POINT ( 'NONE',  ( 9.999999999999998224, 0.000000000000000000, -128.3750000040967905 ) ) ;
#1219 = ORIENTED_EDGE ( 'NONE', *, *, #1586, .T. ) ;
#1220 = CARTESIAN_POINT ( 'NONE',  ( -10.81189881249999729, 1.324075727343319199E-15, -35.09375000204836681 ) ) ;
#1221 = CARTESIAN_POINT ( 'NONE',  ( 10.81189881249999907, 6.242252689847868297, -29.71875000204834194 ) ) ;
#1222 = CARTESIAN_POINT ( 'NONE',  ( 5.405949406249999534, 9.363379034771803333, -14.78125000204835793 ) ) ;
#1223 = CARTESIAN_POINT ( 'NONE',  ( -5.405949406249996869, 9.363379034771805109, -62.34375000204836681 ) ) ;
#1224 = CARTESIAN_POINT ( 'NONE',  ( 9.999999999999998224, 0.000000000000000000, -17.37500000409675138 ) ) ;
#1225 = CARTESIAN_POINT ( 'NONE',  ( -10.00000000000000000, -5.773502691896251982, -47.62499999999997158 ) ) ;
#1226 = CARTESIAN_POINT ( 'NONE',  ( -5.405949406250003975, -9.363379034771801557, -187.8437500020483810 ) ) ;
#1227 = CARTESIAN_POINT ( 'NONE',  ( 7.644554776091147741E-16, 12.48450537969573659, -167.4687500020483810 ) ) ;
#1228 = CARTESIAN_POINT ( 'NONE',  ( -9.999999999999998224, 1.224646799147353059E-15, -43.24999999999998579 ) ) ;
#1229 = CARTESIAN_POINT ( 'NONE',  ( -5.000000000000003553, -8.660254037844383745, -99.99999999999998579 ) ) ;
#1230 = CARTESIAN_POINT ( 'NONE',  ( -10.00000000000051337, 5.773502691895962435, -140.8750000000000000 ) ) ;
#1231 = DIRECTION ( 'NONE',  ( 0.000000000000000000, 0.000000000000000000, -1.000000000000000000 ) ) ;
#1232 = CARTESIAN_POINT ( 'NONE',  ( -9.999999999999998224, 0.000000000000000000, -99.99999999999998579 ) ) ;
#1233 = CARTESIAN_POINT ( 'NONE',  ( 10.81189881249999729, 0.000000000000000000, -115.3437500020483810 ) ) ;
#1234 = CARTESIAN_POINT ( 'NONE',  ( -1.040834085586084257E-14, 145.0000000000000000, 22.49999999999999289 ) ) ;
#1235 = AXIS2_PLACEMENT_3D ( 'NONE', #20101, #3926, #25440 ) ;
#1236 = CARTESIAN_POINT ( 'NONE',  ( -5.405949406250003975, -9.363379034771801557, -81.53125000204839523 ) ) ;
#1237 = CARTESIAN_POINT ( 'NONE',  ( 10.81189881249999551, -6.242252689847874514, -103.4687500020483668 ) ) ;
#1238 = VECTOR ( 'NONE', #42446, 1000.000000000000000 ) ;
#1239 = CARTESIAN_POINT ( 'NONE',  ( -5.405949406249996869, 9.363379034771805109, -71.34375000204836681 ) ) ;
#1240 = CARTESIAN_POINT ( 'NONE',  ( 7.644554776091147741E-16, 12.48450537969573659, -77.65625000204838102 ) ) ;
#1241 = CARTESIAN_POINT ( 'NONE',  ( 9.999999999999996447, -5.773502691896262640, -157.0000000040968189 ) ) ;
#1242 = CARTESIAN_POINT ( 'NONE',  ( -10.00000000000000000, -5.773502691896251982, -128.6250000000000000 ) ) ;
#1243 = CARTESIAN_POINT ( 'NONE',  ( 10.81189881249999551, -6.242252689847874514, -162.1562500020484094 ) ) ;
#1244 = CARTESIAN_POINT ( 'NONE',  ( -5.405949406250003975, -9.363379034771801557, -174.5312500020484094 ) ) ;
#1245 = EDGE_CURVE ( 'NONE', #22331, #11539, #29776, .T. ) ;
#1246 = FACE_BOUND ( 'NONE', #18987, .T. ) ;
#1247 = DIRECTION ( 'NONE',  ( 1.000000000000000000, 0.000000000000000000, 0.000000000000000000 ) ) ;
#1248 = CARTESIAN_POINT ( 'NONE',  ( 10.81189881249999907, 6.242252689847868297, -107.7187500020483810 ) ) ;
#1249 = CARTESIAN_POINT ( 'NONE',  ( 5.000000000000000000, 8.660254037844385522, -120.6250000040967905 ) ) ;
#1250 = CARTESIAN_POINT ( 'NONE',  ( 9.999999999999996447, -5.773502691896262640, -72.62499999999995737 ) ) ;
#1251 = CARTESIAN_POINT ( 'NONE',  ( -5.405949406249996869, 9.363379034771805109, -4.031250002048375691 ) ) ;
#1252 = CARTESIAN_POINT ( 'NONE',  ( 9.999999999999996447, -5.773502691896262640, -82.00000000409676204 ) ) ;
#1253 = DIRECTION ( 'NONE',  ( -0.000000000000000000, -0.000000000000000000, 1.000000000000000000 ) ) ;
#1254 = CARTESIAN_POINT ( 'NONE',  ( 10.81189881249999551, -6.242252689847874514, -103.6562500020483668 ) ) ;
#1255 = CARTESIAN_POINT ( 'NONE',  ( 7.644554776091147741E-16, 12.48450537969573659, -73.15625000204836681 ) ) ;
#1256 = CARTESIAN_POINT ( 'NONE',  ( -10.00000000000000000, -5.773502691896251982, -79.50000000409679046 ) ) ;
#1257 = CARTESIAN_POINT ( 'NONE',  ( 5.000000000000000000, 8.660254037844385522, -118.7500000000000000 ) ) ;
#1258 = CARTESIAN_POINT ( 'NONE',  ( -5.405949406250003975, -9.363379034771801557, -30.34375000204836326 ) ) ;
#1259 = EDGE_LOOP ( 'NONE', ( #38574, #7850, #2382, #2551 ) ) ;
#1260 = CARTESIAN_POINT ( 'NONE',  ( -4.999999999999996447, 8.660254037844387298, 2.775557561562891351E-14 ) ) ;
#1261 = CARTESIAN_POINT ( 'NONE',  ( -5.405949406250003975, -9.363379034771801557, -32.03125000204837391 ) ) ;
#1262 = CARTESIAN_POINT ( 'NONE',  ( -5.405949406250003975, -9.363379034771801557, -15.34375000204835082 ) ) ;
#1263 = CARTESIAN_POINT ( 'NONE',  ( 10.00000000000044764, -5.773502691896004180, -176.5000000040967905 ) ) ;
#1264 = CARTESIAN_POINT ( 'NONE',  ( 9.999999999999998224, 0.000000000000000000, -0.8750000040967653714 ) ) ;
#1265 = CARTESIAN_POINT ( 'NONE',  ( 10.81189881249999551, -6.242252689847874514, -130.6562500020484094 ) ) ;
#1266 = CARTESIAN_POINT ( 'NONE',  ( 9.999999999999996447, -5.773502691896262640, -180.6250000000000284 ) ) ;
#1267 = DIRECTION ( 'NONE',  ( -0.000000000000000000, -0.000000000000000000, 1.000000000000000000 ) ) ;
#1269 = VERTEX_POINT ( 'NONE', #17953 ) ;
#1268 = CARTESIAN_POINT ( 'NONE',  ( -10.81189881249999729, 1.324075727343319199E-15, -113.2812500020483952 ) ) ;
#1270 = CARTESIAN_POINT ( 'NONE',  ( 9.999999999999998224, 0.000000000000000000, -153.8750000040967905 ) ) ;
#1271 = EDGE_LOOP ( 'NONE', ( #25258, #42176, #4809, #27326 ) ) ;
#1272 = ORIENTED_EDGE ( 'NONE', *, *, #2506, .F. ) ;
#1273 = CARTESIAN_POINT ( 'NONE',  ( 7.644554776091147741E-16, 12.48450537969573659, -38.65625000204835260 ) ) ;
#1274 = DATE_AND_TIME ( #24585, #31815 ) ;
#1275 = CARTESIAN_POINT ( 'NONE',  ( -10.81189881249999729, 1.324075727343319199E-15, -90.59375000204838102 ) ) ;
#1276 = DIRECTION ( 'NONE',  ( -1.000000000000000000, 0.000000000000000000, 0.000000000000000000 ) ) ;
#1277 = CARTESIAN_POINT ( 'NONE',  ( 3.018241686408907221, 10.32067256058293481, -99.99999999999997158 ) ) ;
#1278 = LINE ( 'NONE', #14406, #27426 ) ;
#1279 = CARTESIAN_POINT ( 'NONE',  ( 5.405949406249992428, -9.363379034771808662, -172.7812500020484094 ) ) ;
#1280 = CARTESIAN_POINT ( 'NONE',  ( -4.999999999999996447, 8.660254037844387298, -58.49999999999997158 ) ) ;
#1281 = CARTESIAN_POINT ( 'NONE',  ( -5.405949406250003975, -9.363379034771801557, -121.8437500020483952 ) ) ;
#1282 = CARTESIAN_POINT ( 'NONE',  ( 5.405949406249999534, 9.363379034771803333, -91.09375000204838102 ) ) ;
#1283 = CARTESIAN_POINT ( 'NONE',  ( -10.81189881249999729, 1.324075727343319199E-15, -2.281250002048373915 ) ) ;
#1284 = CARTESIAN_POINT ( 'NONE',  ( 0.000000000000000000, 0.000000000000000000, -200.0000000000000000 ) ) ;
#1285 = CARTESIAN_POINT ( 'NONE',  ( 10.81189881249999551, -6.242252689847874514, -100.6562500020483952 ) ) ;
#1286 = CARTESIAN_POINT ( 'NONE',  ( -2.121150477449813534E-15, -11.54700538379251284, -179.7500000040967905 ) ) ;
#1287 = CARTESIAN_POINT ( 'NONE',  ( -10.81189881249999729, 6.242252689847871849, -104.2187500020483810 ) ) ;
#1288 = CARTESIAN_POINT ( 'NONE',  ( -5.405949406249996869, 9.363379034771805109, -176.5312500020483810 ) ) ;
#1289 = CARTESIAN_POINT ( 'NONE',  ( -7.423074889580966840, 12.85714285714296246, 52.14285714285716011 ) ) ;
#1290 = CARTESIAN_POINT ( 'NONE',  ( -10.00000000000076916, 5.773502691895813221, -132.2500000040967620 ) ) ;
#1291 = CARTESIAN_POINT ( 'NONE',  ( 5.405949406249999534, 9.363379034771803333, -199.2812500020484094 ) ) ;
#1292 = CARTESIAN_POINT ( 'NONE',  ( 5.405949406249999534, 9.363379034771803333, -55.09375000204835970 ) ) ;
#1293 = CARTESIAN_POINT ( 'NONE',  ( 4.999999999999992006, -8.660254037844389075, -175.1250000040968189 ) ) ;
#1294 = CARTESIAN_POINT ( 'NONE',  ( -10.81189881249999729, 6.242252689847871849, -11.40625000204835438 ) ) ;
#1295 = CARTESIAN_POINT ( 'NONE',  ( -5.405949406250003975, -9.363379034771801557, -22.84375000204835615 ) ) ;
#1296 = CARTESIAN_POINT ( 'NONE',  ( 10.81189881249999907, 6.242252689847868297, -133.2187500020483810 ) ) ;
#1297 = CARTESIAN_POINT ( 'NONE',  ( -10.00000000000000000, -5.773502691896251982, -95.62499999999998579 ) ) ;
#1298 = CARTESIAN_POINT ( 'NONE',  ( -5.405949406250003975, -9.363379034771801557, -29.03125000204837036 ) ) ;
#1299 = CARTESIAN_POINT ( 'NONE',  ( 7.070501591499377789E-16, 11.54700538379251284, -102.5000000040967763 ) ) ;
#1300 = CARTESIAN_POINT ( 'NONE',  ( 0.000000000000000000, 0.000000000000000000, -200.0000000000000000 ) ) ;
#1301 = CARTESIAN_POINT ( 'NONE',  ( 9.999999999999996447, -5.773502691896262640, -59.12499999999998579 ) ) ;
#1302 = CARTESIAN_POINT ( 'NONE',  ( -2.293366432827344421E-15, -12.48450537969573659, -121.9062500020483952 ) ) ;
#1303 = CARTESIAN_POINT ( 'NONE',  ( -10.81189881249999729, 1.324075727343319199E-15, -107.2812500020483810 ) ) ;
#1304 = ORIENTED_EDGE ( 'NONE', *, *, #385, .T. ) ;
#1305 = LINE ( 'NONE', #40341, #10004 ) ;
#1306 = CARTESIAN_POINT ( 'NONE',  ( 7.070501591499377789E-16, 11.54700538379251284, -98.00000000409677625 ) ) ;
#1307 = CARTESIAN_POINT ( 'NONE',  ( 10.81189881249999551, -6.242252689847874514, -162.1562500020484379 ) ) ;
#1308 = CARTESIAN_POINT ( 'NONE',  ( 7.644554776091147741E-16, 12.48450537969573659, -57.96875000204837391 ) ) ;
#1309 = ORIENTED_EDGE ( 'NONE', *, *, #22453, .T. ) ;
#1310 = CARTESIAN_POINT ( 'NONE',  ( 5.000000000000000000, 8.660254037844385522, -28.74999999999997158 ) ) ;
#1311 = CARTESIAN_POINT ( 'NONE',  ( -5.405949406250003975, -9.363379034771801557, -36.53125000204837391 ) ) ;
#1312 = CARTESIAN_POINT ( 'NONE',  ( -9.999999999999998224, 5.773502691896259087, -163.3750000000000000 ) ) ;
#1313 = EDGE_CURVE ( 'NONE', #37408, #38561, #36933, .T. ) ;
#1314 = CARTESIAN_POINT ( 'NONE',  ( -9.999999999999998224, 1.224646799147353059E-15, -135.1250000040967620 ) ) ;
#1315 = CARTESIAN_POINT ( 'NONE',  ( 10.00000000000000000, 5.773502691896255534, -24.75000000409677270 ) ) ;
#1316 = CARTESIAN_POINT ( 'NONE',  ( 10.00000000000000000, 5.773502691896255534, -168.3750000000000000 ) ) ;
#1317 = CARTESIAN_POINT ( 'NONE',  ( -10.81189881249999907, -6.242252689847864744, -131.1562500020483810 ) ) ;
#1318 = CARTESIAN_POINT ( 'NONE',  ( 9.999999999998969713, 5.773502691896851502, -46.87499999999994316 ) ) ;
#1319 = CARTESIAN_POINT ( 'NONE',  ( 0.000000000000000000, 0.000000000000000000, -200.0000000000000000 ) ) ;
#1320 = ORIENTED_EDGE ( 'NONE', *, *, #37835, .T. ) ;
#1321 =( BOUNDED_CURVE ( )  B_SPLINE_CURVE ( 2, ( #28186, #41956, #11757, #24958, #2496, #12181, #25372 ),
 .UNSPECIFIED., .F., .F. ) 
 B_SPLINE_CURVE_WITH_KNOTS ( ( 3, 2, 2, 3 ),
 ( 0.2947761194029852039, 0.2960199004975125336, 0.2972636815920398634, 0.2985074626865671932 ),
 .UNSPECIFIED. ) 
 CURVE ( )  GEOMETRIC_REPRESENTATION_ITEM ( )  RATIONAL_B_SPLINE_CURVE ( ( 0.9999999999999880096, 0.8660254037844506980, 1.000000000000000000, 0.8660254037844387076, 1.000000000000000000, 0.8660254037844327124, 1.000000000000005995 ) ) 
 REPRESENTATION_ITEM ( '' )  );
#1323 = ORIENTED_EDGE ( 'NONE', *, *, #1691, .F. ) ;
#1322 = ORIENTED_EDGE ( 'NONE', *, *, #12215, .F. ) ;
#1324 = AXIS2_PLACEMENT_3D ( 'NONE', #15425, #28623, #25380 ) ;
#1325 = CYLINDRICAL_SURFACE ( 'NONE', #23143, 9.999999999999998224 ) ;
#1326 = DIRECTION ( 'NONE',  ( 1.000000000000000000, 0.000000000000000000, 0.000000000000000000 ) ) ;
#1327 = CARTESIAN_POINT ( 'NONE',  ( 5.405949406249992428, -9.363379034771808662, -166.5937500020484094 ) ) ;
#1328 = CARTESIAN_POINT ( 'NONE',  ( 10.81189881249999907, 6.242252689847868297, -194.9062500020484379 ) ) ;
#1329 = CARTESIAN_POINT ( 'NONE',  ( 10.81189881249999729, 0.000000000000000000, -16.34375000204835260 ) ) ;
#1330 = VECTOR ( 'NONE', #32095, 1000.000000000000000 ) ;
#1331 = DIRECTION ( 'NONE',  ( 0.000000000000000000, 0.000000000000000000, -1.000000000000000000 ) ) ;
#1332 = CARTESIAN_POINT ( 'NONE',  ( 5.405949406249999534, 9.363379034771803333, -151.0937500020483810 ) ) ;
#1333 = CARTESIAN_POINT ( 'NONE',  ( 5.405949406249999534, 9.363379034771803333, -134.5937500020483810 ) ) ;
#1334 = CARTESIAN_POINT ( 'NONE',  ( 10.81189881249999551, -6.242252689847874514, -109.6562500020483810 ) ) ;
#1335 = CARTESIAN_POINT ( 'NONE',  ( -10.81189881249999907, -6.242252689847864744, -114.4687500020483810 ) ) ;
#1336 = CARTESIAN_POINT ( 'NONE',  ( 9.999999999999998224, 0.000000000000000000, -194.3750000040967905 ) ) ;
#1337 = CARTESIAN_POINT ( 'NONE',  ( 5.405949406249999534, 9.363379034771803333, -127.2812500020483810 ) ) ;
#1338 = CARTESIAN_POINT ( 'NONE',  ( -9.999999999999998224, 1.224646799147353059E-15, -198.1250000040967905 ) ) ;
#1339 = CARTESIAN_POINT ( 'NONE',  ( -10.81189881249999729, -6.242252689847864744, -133.9687500020483810 ) ) ;
#1340 = CARTESIAN_POINT ( 'NONE',  ( -5.000000000000003553, -8.660254037844383745, -166.3750000040967905 ) ) ;
#1341 = AXIS2_PLACEMENT_3D ( 'NONE', #35377, #16116, #22841 ) ;
#1342 = CARTESIAN_POINT ( 'NONE',  ( -2.121150477449813534E-15, -11.54700538379251284, -178.2500000040968189 ) ) ;
#1343 = CARTESIAN_POINT ( 'NONE',  ( -5.000000000000003553, -8.660254037844383745, -143.5000000000000000 ) ) ;
#1344 = CARTESIAN_POINT ( 'NONE',  ( -2.121150477449813534E-15, -11.54700538379251284, -20.37499999999997513 ) ) ;
#1345 = CARTESIAN_POINT ( 'NONE',  ( -5.405949406249996869, 9.363379034771805109, -78.84375000204838102 ) ) ;
#1346 = CARTESIAN_POINT ( 'NONE',  ( -10.81189881249999729, 6.242252689847871849, -68.21875000204838102 ) ) ;
#1347 = DIRECTION ( 'NONE',  ( -1.000000000000000000, 0.000000000000000000, 0.000000000000000000 ) ) ;
#1348 = CARTESIAN_POINT ( 'NONE',  ( 10.81189881249999729, 0.000000000000000000, -31.53125000204837391 ) ) ;
#1349 = CARTESIAN_POINT ( 'NONE',  ( -5.405949406249996869, 9.363379034771805109, -48.84375000204838102 ) ) ;
#1350 = CARTESIAN_POINT ( 'NONE',  ( 10.81189881249999907, 6.242252689847868297, -152.7187500020483810 ) ) ;
#1351 = CARTESIAN_POINT ( 'NONE',  ( -10.00000000000000000, -5.773502691896251982, -122.6250000000000000 ) ) ;
#1352 = CARTESIAN_POINT ( 'NONE',  ( 10.81189881249999729, 6.242252689847867408, -128.9062500020483810 ) ) ;
#1353 = CARTESIAN_POINT ( 'NONE',  ( 3.970414520298676031, 9.602429920229235805, -180.0000000000001705 ) ) ;
#1354 = CARTESIAN_POINT ( 'NONE',  ( 9.999999999999998224, 0.000000000000000000, -79.99999999999998579 ) ) ;
#1355 = CARTESIAN_POINT ( 'NONE',  ( -10.81189881249999729, 6.242252689847871849, -21.90625000204837036 ) ) ;
#1356 = ORIENTED_EDGE ( 'NONE', *, *, #105, .T. ) ;
#1357 = CARTESIAN_POINT ( 'NONE',  ( 10.81189881249999551, -6.242252689847874514, -105.1562500020483810 ) ) ;
#1358 = CARTESIAN_POINT ( 'NONE',  ( 5.000000000000000000, 8.660254037844385522, -128.1250000040967620 ) ) ;
#1359 = CARTESIAN_POINT ( 'NONE',  ( -2.121150477449813534E-15, -11.54700538379251284, -143.7500000040967905 ) ) ;
#1360 = CARTESIAN_POINT ( 'NONE',  ( 9.999999999999998224, 0.000000000000000000, -35.37500000409676915 ) ) ;
#1361 = CARTESIAN_POINT ( 'NONE',  ( 9.999999999999998224, 0.000000000000000000, -61.99999999999997158 ) ) ;
#1362 = CARTESIAN_POINT ( 'NONE',  ( 10.81189881249999907, 6.242252689847868297, -47.90625000204837391 ) ) ;
#1363 = CARTESIAN_POINT ( 'NONE',  ( 5.000000000000000000, 8.660254037844385522, -147.2500000000000000 ) ) ;
#1364 = CARTESIAN_POINT ( 'NONE',  ( -5.405949406249996869, 9.363379034771805109, -157.0312500020484094 ) ) ;
#1365 = AXIS2_PLACEMENT_3D ( 'NONE', #20346, #13856, #29869 ) ;
#1366 = CARTESIAN_POINT ( 'NONE',  ( 7.644554776091147741E-16, 12.48450537969573659, -129.9687500020483810 ) ) ;
#1368 = ADVANCED_FACE ( 'NONE', ( #12127 ), #31366, .T. ) ;
#1367 = DIRECTION ( 'NONE',  ( -0.000000000000000000, -0.000000000000000000, 1.000000000000000000 ) ) ;
#1369 = EDGE_LOOP ( 'NONE', ( #15629, #29218, #26146, #12790 ) ) ;
#1370 = EDGE_CURVE ( 'NONE', #2118, #27376, #40003, .T. ) ;
#1371 = VERTEX_POINT ( 'NONE', #25318 ) ;
#1372 = AXIS2_PLACEMENT_3D ( 'NONE', #81, #29426, #10193 ) ;
#1373 = ORIENTED_EDGE ( 'NONE', *, *, #7404, .F. ) ;
#1375 = ORIENTED_EDGE ( 'NONE', *, *, #12974, .F. ) ;
#1374 = CARTESIAN_POINT ( 'NONE',  ( -10.81189881249999907, -6.242252689847864744, -114.4687500020483810 ) ) ;
#1376 = CARTESIAN_POINT ( 'NONE',  ( 9.999999999999998224, 0.000000000000000000, -200.0000000000000000 ) ) ;
#1377 = CARTESIAN_POINT ( 'NONE',  ( -10.81189881249999729, 1.324075727343319199E-15, -188.0937500020483810 ) ) ;
#1378 = CARTESIAN_POINT ( 'NONE',  ( -10.81189881249999729, 1.324075727343319199E-15, -38.09375000204837391 ) ) ;
#1379 = CARTESIAN_POINT ( 'NONE',  ( -1.290480703760489067, -10.30757810694964327, 1.243155832063081332E-14 ) ) ;
#1380 = CARTESIAN_POINT ( 'NONE',  ( 9.999999999999998224, 0.000000000000000000, -152.3750000040967905 ) ) ;
#1381 = CARTESIAN_POINT ( 'NONE',  ( -10.81189881249999729, -6.242252689847864744, -168.4687500020483526 ) ) ;
#1382 = CARTESIAN_POINT ( 'NONE',  ( -10.81189881249999729, 1.324075727343319199E-15, -164.0937500020484094 ) ) ;
#1383 = LINE ( 'NONE', #34405, #18302 ) ;
#1384 = CARTESIAN_POINT ( 'NONE',  ( -2.293366432827344421E-15, -12.48450537969573659, -145.7187500020484094 ) ) ;
#1385 = CARTESIAN_POINT ( 'NONE',  ( 10.81189881249999729, 0.000000000000000000, -150.0312500020483810 ) ) ;
#1386 = CARTESIAN_POINT ( 'NONE',  ( -5.405949406250003975, -9.363379034771801557, -154.8437500020483810 ) ) ;
#1387 = CARTESIAN_POINT ( 'NONE',  ( 9.999999999999998224, 0.000000000000000000, -52.99999999999996447 ) ) ;
#1388 = CARTESIAN_POINT ( 'NONE',  ( -2.121150477449813534E-15, -11.54700538379251284, -139.2500000040967905 ) ) ;
#1389 = CARTESIAN_POINT ( 'NONE',  ( 4.999999999999992006, -8.660254037844389075, -179.2500000000000284 ) ) ;
#1390 = VECTOR ( 'NONE', #16568, 1000.000000000000000 ) ;
#1391 = CARTESIAN_POINT ( 'NONE',  ( 10.81189881249999729, 0.000000000000000000, -89.84375000204838102 ) ) ;
#1392 = CARTESIAN_POINT ( 'NONE',  ( -2.121150477449813534E-15, -11.54700538379251284, -113.3749999999999858 ) ) ;
#1393 = CARTESIAN_POINT ( 'NONE',  ( -10.81189881249999729, 1.324075727343319199E-15, -57.78125000204836681 ) ) ;
#1394 = DIRECTION ( 'NONE',  ( -0.000000000000000000, -0.000000000000000000, -1.000000000000000000 ) ) ;
#1395 = CARTESIAN_POINT ( 'NONE',  ( 10.81189881249999551, -6.242252689847874514, -181.4687500020484094 ) ) ;
#1396 = CARTESIAN_POINT ( 'NONE',  ( 10.81189881249999729, 0.000000000000000000, -115.5312500020483952 ) ) ;
#1397 = CARTESIAN_POINT ( 'NONE',  ( 10.81189881249999729, 0.000000000000000000, -151.5312500020484094 ) ) ;
#1398 = CYLINDRICAL_SURFACE ( 'NONE', #38576, 9.999999999999998224 ) ;
#1399 = CARTESIAN_POINT ( 'NONE',  ( -10.81189881249999729, 6.242252689847871849, -41.40625000204836681 ) ) ;
#1400 = CARTESIAN_POINT ( 'NONE',  ( -9.999999999999998224, 5.773502691896259087, -126.2500000040967763 ) ) ;
#1401 = CARTESIAN_POINT ( 'NONE',  ( -5.000000000000003553, -8.660254037844383745, -110.4999999999999858 ) ) ;
#1402 = VERTEX_POINT ( 'NONE', #9114 ) ;
#1403 = CARTESIAN_POINT ( 'NONE',  ( -10.81189881249999729, 6.242252689847871849, -129.9062500020483810 ) ) ;
#1404 = CARTESIAN_POINT ( 'NONE',  ( 7.070501591499377789E-16, 11.54700538379251284, -152.0000000040967905 ) ) ;
#1405 = CYLINDRICAL_SURFACE ( 'NONE', #22230, 9.999999999999998224 ) ;
#1406 = CARTESIAN_POINT ( 'NONE',  ( -2.293366432827344421E-15, -12.48450537969573659, -181.9062500020483810 ) ) ;
#1407 = ORIENTED_EDGE ( 'NONE', *, *, #13176, .T. ) ;
#1408 = CARTESIAN_POINT ( 'NONE',  ( 5.000000000000000000, 8.660254037844385522, -51.24999999999996447 ) ) ;
#1409 = CARTESIAN_POINT ( 'NONE',  ( 10.81189881249999729, 0.000000000000000000, -173.8437500020484094 ) ) ;
#1410 = CARTESIAN_POINT ( 'NONE',  ( 7.070501591499377789E-16, 11.54700538379251284, -57.50000000409677625 ) ) ;
#1411 = CYLINDRICAL_SURFACE ( 'NONE', #40297, 9.999999999999998224 ) ;
#1412 =( BOUNDED_CURVE ( )  B_SPLINE_CURVE ( 2, ( #12336, #12550, #41693, #35248, #28560, #34822, #34607 ),
 .UNSPECIFIED., .F., .F. ) 
 B_SPLINE_CURVE_WITH_KNOTS ( ( 3, 2, 2, 3 ),
 ( 0.1231343283582089221, 0.1243781094527362935, 0.1256218905472636649, 0.1268656716417910224 ),
 .UNSPECIFIED. ) 
 CURVE ( )  GEOMETRIC_REPRESENTATION_ITEM ( )  RATIONAL_B_SPLINE_CURVE ( ( 1.000000000000002887, 0.8660254037844355990, 1.000000000000000000, 0.8660254037844387076, 1.000000000000000000, 0.8660254037844417052, 0.9999999999999970024 ) ) 
 REPRESENTATION_ITEM ( '' )  );
#1413 = DIRECTION ( 'NONE',  ( -0.000000000000000000, -0.000000000000000000, 1.000000000000000000 ) ) ;
#1414 = CARTESIAN_POINT ( 'NONE',  ( 7.644554776091147741E-16, 12.48450537969573659, -67.15625000204838102 ) ) ;
#1415 = CARTESIAN_POINT ( 'NONE',  ( -10.81189881249999729, 6.242252689847871849, -51.90625000204837391 ) ) ;
#1416 = CARTESIAN_POINT ( 'NONE',  ( -10.00000000000000000, -5.773502691896251982, -49.50000000409676915 ) ) ;
#1417 = CARTESIAN_POINT ( 'NONE',  ( -5.405949406249996869, 9.363379034771805109, -5.343750002048369474 ) ) ;
#1418 = DIRECTION ( 'NONE',  ( 1.000000000000000000, 0.000000000000000000, 0.000000000000000000 ) ) ;
#1419 = CARTESIAN_POINT ( 'NONE',  ( -5.405949406249996869, 9.363379034771805109, -178.0312500020483810 ) ) ;
#1421 = EDGE_CURVE ( 'NONE', #4387, #32685, #21851, .T. ) ;
#1420 = LINE ( 'NONE', #14554, #21342 ) ;
#1422 = DIRECTION ( 'NONE',  ( -0.000000000000000000, -0.000000000000000000, 1.000000000000000000 ) ) ;
#1423 = CARTESIAN_POINT ( 'NONE',  ( 0.000000000000000000, 0.000000000000000000, -99.99999999999998579 ) ) ;
#1424 = ADVANCED_FACE ( 'NONE', ( #11911 ), #22284, .T. ) ;
#1425 = DIRECTION ( 'NONE',  ( 0.000000000000000000, -1.000000000000000000, 0.000000000000000000 ) ) ;
#1427 = EDGE_LOOP ( 'NONE', ( #33363, #21517, #24368, #7565 ) ) ;
#1426 = CARTESIAN_POINT ( 'NONE',  ( -5.405949406249996869, 9.363379034771805109, -89.53125000204838102 ) ) ;
#1428 = SHAPE_REPRESENTATION_RELATIONSHIP ( 'NONE' , 'NONE' ,  #31964, #34104 ) ;
#1429 = ORIENTED_EDGE ( 'NONE', *, *, #13096, .F. ) ;
#1430 = CC_DESIGN_PERSON_AND_ORGANIZATION_ASSIGNMENT ( #34937, #4711, ( #33910 ) ) ;
#1431 = ORIENTED_EDGE ( 'NONE', *, *, #16931, .T. ) ;
#1432 = CARTESIAN_POINT ( 'NONE',  ( 10.81189881249999729, 0.000000000000000000, -37.34375000204836681 ) ) ;
#1433 = CARTESIAN_POINT ( 'NONE',  ( -2.293366432827344421E-15, -12.48450537969573659, -25.71875000204837391 ) ) ;
#1434 = CARTESIAN_POINT ( 'NONE',  ( -10.81189881249999907, -6.242252689847864744, -11.15625000204838457 ) ) ;
#1435 = CARTESIAN_POINT ( 'NONE',  ( -5.405949406249996869, 9.363379034771805109, -63.84375000204836681 ) ) ;
#1436 = CARTESIAN_POINT ( 'NONE',  ( 9.999999999999998224, 0.000000000000000000, -28.99999999999997158 ) ) ;
#1437 = CARTESIAN_POINT ( 'NONE',  ( -9.999999999999998224, 5.773502691896259087, -44.87499999999997868 ) ) ;
#1438 = CARTESIAN_POINT ( 'NONE',  ( 5.405949406249992428, -9.363379034771808662, -183.0937500020483810 ) ) ;
#1439 = CARTESIAN_POINT ( 'NONE',  ( 5.405949406249999534, 9.363379034771803333, -166.0937500020484094 ) ) ;
#1440 = CARTESIAN_POINT ( 'NONE',  ( 10.81189881249999729, 0.000000000000000000, -176.8437500020483810 ) ) ;
#1441 = FACE_OUTER_BOUND ( 'NONE', #10733, .T. ) ;
#1442 = CARTESIAN_POINT ( 'NONE',  ( 9.999999999999998224, 1.224646799147353059E-15, -99.99999999999998579 ) ) ;
#1443 = CARTESIAN_POINT ( 'NONE',  ( -2.121150477449813534E-15, -11.54700538379251284, -20.75000000409677980 ) ) ;
#1444 = EDGE_CURVE ( 'NONE', #25484, #3061, #25619, .T. ) ;
#1445 = CARTESIAN_POINT ( 'NONE',  ( 10.00000000000051159, -5.773502691895965988, -89.50000000409677625 ) ) ;
#1446 = CARTESIAN_POINT ( 'NONE',  ( 7.644554776091147741E-16, 12.48450537969573659, -110.4687500020483668 ) ) ;
#1447 = DIRECTION ( 'NONE',  ( -0.000000000000000000, -0.000000000000000000, -1.000000000000000000 ) ) ;
#1448 = CARTESIAN_POINT ( 'NONE',  ( 10.81189881249999729, 0.000000000000000000, -84.03125000204838102 ) ) ;
#1449 = CARTESIAN_POINT ( 'NONE',  ( -5.405949406250003975, -9.363379034771801557, -102.3437500020483810 ) ) ;
#1450 = CARTESIAN_POINT ( 'NONE',  ( 10.81189881249999551, -6.242252689847874514, -59.96875000204837391 ) ) ;
#1451 = CARTESIAN_POINT ( 'NONE',  ( -10.81189881249999729, 6.242252689847871849, -69.90625000204839523 ) ) ;
#1452 = CARTESIAN_POINT ( 'NONE',  ( 9.999999999999996447, -5.773502691896262640, -154.0000000040968189 ) ) ;
#1453 = CARTESIAN_POINT ( 'NONE',  ( -9.999999999999998224, 1.224646799147353059E-15, -130.2499999999999716 ) ) ;
#1454 =( BOUNDED_CURVE ( )  B_SPLINE_CURVE ( 2, ( #8593, #18502, #15255, #21956, #5562, #18714, #31907 ),
 .UNSPECIFIED., .F., .F. ) 
 B_SPLINE_CURVE_WITH_KNOTS ( ( 3, 2, 2, 3 ),
 ( 0.03731343283582092690, 0.03855721393034829136, 0.03980099502487565583, 0.04104477611940302029 ),
 .UNSPECIFIED. ) 
 CURVE ( )  GEOMETRIC_REPRESENTATION_ITEM ( )  RATIONAL_B_SPLINE_CURVE ( ( 0.9999999999999963363, 0.8660254037844424824, 1.000000000000000000, 0.8660254037844387076, 1.000000000000000000, 0.8660254037844349329, 1.000000000000003775 ) ) 
 REPRESENTATION_ITEM ( '' )  );
#1455 = CARTESIAN_POINT ( 'NONE',  ( 7.644554776091147741E-16, 12.48450537969573659, -146.6562500020484094 ) ) ;
#1456 = CARTESIAN_POINT ( 'NONE',  ( 10.81189881249999907, 6.242252689847868297, -166.4062500020483810 ) ) ;
#1457 = CC_DESIGN_APPROVAL ( #10370, ( #20040 ) ) ;
#1458 = CARTESIAN_POINT ( 'NONE',  ( -2.121150477449813534E-15, -11.54700538379251284, -174.8750000000000000 ) ) ;
#1459 = DIRECTION ( 'NONE',  ( 1.000000000000000000, 0.000000000000000000, 0.000000000000000000 ) ) ;
#1460 = CARTESIAN_POINT ( 'NONE',  ( 10.81189881249999907, 6.242252689847868297, -100.2187500020483810 ) ) ;
#1461 = CARTESIAN_POINT ( 'NONE',  ( 0.000000000000000000, 0.000000000000000000, -99.99999999999998579 ) ) ;
#1462 = CARTESIAN_POINT ( 'NONE',  ( -9.999999999999998224, 1.224646799147353059E-15, -73.24999999999998579 ) ) ;
#1463 = CARTESIAN_POINT ( 'NONE',  ( 5.405949406249999534, 9.363379034771803333, -193.0937500020484094 ) ) ;
#1464 = CARTESIAN_POINT ( 'NONE',  ( 4.999999999999992006, -8.660254037844389075, -80.62500000409677625 ) ) ;
#1465 = CARTESIAN_POINT ( 'NONE',  ( 5.339643252401987006, -9.254418622957800267, -180.0000000000000000 ) ) ;
#1466 = CARTESIAN_POINT ( 'NONE',  ( -10.81189881249999729, 6.242252689847871849, -98.40625000204838102 ) ) ;
#1467 = CARTESIAN_POINT ( 'NONE',  ( -2.293366432827344421E-15, -12.48450537969573659, -72.40625000204836681 ) ) ;
#1468 =( BOUNDED_CURVE ( )  B_SPLINE_CURVE ( 2, ( #18781, #9276, #28730, #2815, #31970, #15947, #19412 ),
 .UNSPECIFIED., .F., .F. ) 
 B_SPLINE_CURVE_WITH_KNOTS ( ( 3, 2, 2, 3 ),
 ( 0.1156716417910447492, 0.1169154228855721483, 0.1181592039800995753, 0.1194029850746269744 ),
 .UNSPECIFIED. ) 
 CURVE ( )  GEOMETRIC_REPRESENTATION_ITEM ( )  RATIONAL_B_SPLINE_CURVE ( ( 1.000000000000003109, 0.8660254037844358210, 1.000000000000000000, 0.8660254037844387076, 1.000000000000000000, 0.8660254037844267172, 1.000000000000011990 ) ) 
 REPRESENTATION_ITEM ( '' )  );
#1469 = CARTESIAN_POINT ( 'NONE',  ( 9.999999999999996447, -5.773502691896262640, -79.00000000409677625 ) ) ;
#1470 = CARTESIAN_POINT ( 'NONE',  ( 5.000000000000000000, 8.660254037844385522, -21.24999999999996447 ) ) ;
#1471 = CARTESIAN_POINT ( 'NONE',  ( -2.293366432827344421E-15, -12.48450537969573659, -37.71875000204835970 ) ) ;
#1472 = ORIENTED_EDGE ( 'NONE', *, *, #16310, .F. ) ;
#1473 = CARTESIAN_POINT ( 'NONE',  ( -10.81189881249999729, 6.242252689847871849, -198.9062500020484094 ) ) ;
#1474 = CARTESIAN_POINT ( 'NONE',  ( -5.405949406249996869, 9.363379034771805109, -25.03125000204836681 ) ) ;
#1475 = CARTESIAN_POINT ( 'NONE',  ( 5.405949406249999534, 9.363379034771803333, -10.09375000204834549 ) ) ;
#1476 = CARTESIAN_POINT ( 'NONE',  ( -10.00000000000051337, 5.773502691895962435, -142.3750000000000000 ) ) ;
#1477 = CARTESIAN_POINT ( 'NONE',  ( -10.00000000000000000, -5.773502691896251982, -4.500000004096754047 ) ) ;
#1478 = CARTESIAN_POINT ( 'NONE',  ( 7.644554776091147741E-16, 12.48450537969573659, -133.1562500020483810 ) ) ;
#1479 = CARTESIAN_POINT ( 'NONE',  ( -4.999999999999996447, 8.660254037844387298, -180.0000000000000000 ) ) ;
#1480 = FACE_OUTER_BOUND ( 'NONE', #34425, .T. ) ;
#1482 = ORIENTED_EDGE ( 'NONE', *, *, #30429, .T. ) ;
#1481 = CARTESIAN_POINT ( 'NONE',  ( -10.81189881249999907, -6.242252689847864744, -113.1562500020483952 ) ) ;
#1483 = CARTESIAN_POINT ( 'NONE',  ( -5.000000000000003553, -8.660254037844383745, -154.3750000040967905 ) ) ;
#1484 = ORIENTED_EDGE ( 'NONE', *, *, #33061, .T. ) ;
#1485 = ORIENTED_EDGE ( 'NONE', *, *, #41503, .F. ) ;
#1486 = CARTESIAN_POINT ( 'NONE',  ( 7.644554776091147741E-16, 12.48450537969573659, -35.65625000204835260 ) ) ;
#1487 = MANIFOLD_SOLID_BREP ( 'Cavity1', #17003 ) ;
#1488 = PERSON_AND_ORGANIZATION ( #11915, #17965 ) ;
#1489 = LOCAL_TIME ( 11, 57, 6.000000000000000000, #23940 ) ;
#1490 = ADVANCED_FACE ( 'NONE', ( #8269 ), #15358, .T. ) ;
#1491 = CARTESIAN_POINT ( 'NONE',  ( -10.81189881249999729, 1.324075727343319199E-15, -84.59375000204836681 ) ) ;
#1492 = CYLINDRICAL_SURFACE ( 'NONE', #13918, 9.999999999999998224 ) ;
#1493 = DIRECTION ( 'NONE',  ( 1.000000000000000000, 0.000000000000000000, 0.000000000000000000 ) ) ;
#1494 = CARTESIAN_POINT ( 'NONE',  ( 7.070501591499376803E-16, 11.54700538379251284, -170.0000000040967905 ) ) ;
#1495 = CARTESIAN_POINT ( 'NONE',  ( 10.81189881249999551, -6.242252689847874514, -165.1562500020483526 ) ) ;
#1496 = CARTESIAN_POINT ( 'NONE',  ( -4.999999999999996447, 8.660254037844387298, -54.37500000409675494 ) ) ;
#1497 = CARTESIAN_POINT ( 'NONE',  ( -10.81189881249999729, 6.242252689847871849, -123.7187500020483952 ) ) ;
#1498 = PRODUCT ( 'adapter key', 'adapter key', '', ( #33542 ) ) ;
#1499 = CARTESIAN_POINT ( 'NONE',  ( 5.405949406249999534, 9.363379034771803333, -89.59375000204838102 ) ) ;
#1500 = CARTESIAN_POINT ( 'NONE',  ( -10.81189881249999729, -6.242252689847864744, -3.656250002048349046 ) ) ;
#1501 = CARTESIAN_POINT ( 'NONE',  ( 10.81189881249999907, 6.242252689847868297, -193.2187500020484094 ) ) ;
#1502 = CARTESIAN_POINT ( 'NONE',  ( -2.293366432827344421E-15, -12.48450537969573659, -88.90625000204838102 ) ) ;
#1503 = CARTESIAN_POINT ( 'NONE',  ( 4.999999999999992006, -8.660254037844389075, -181.1250000040967905 ) ) ;
#1504 = CARTESIAN_POINT ( 'NONE',  ( 10.81189881249999729, 0.000000000000000000, -109.3437500020483810 ) ) ;
#1505 = CARTESIAN_POINT ( 'NONE',  ( -10.81189881249999729, 6.242252689847871849, -167.4062500020484094 ) ) ;
#1506 = CARTESIAN_POINT ( 'NONE',  ( 10.00000000000051159, -5.773502691895965988, -150.6250000000000000 ) ) ;
#1507 = CARTESIAN_POINT ( 'NONE',  ( 10.81189881249999551, -6.242252689847874514, -171.1562500020484094 ) ) ;
#1508 = CARTESIAN_POINT ( 'NONE',  ( -5.405949406249996869, 9.363379034771805109, -197.5312500020484094 ) ) ;
#1509 = CARTESIAN_POINT ( 'NONE',  ( 10.81189881249999729, 6.242252689847867408, -53.71875000204838102 ) ) ;
#1510 = CARTESIAN_POINT ( 'NONE',  ( 5.000000000000000000, 8.660254037844385522, -171.6250000040968189 ) ) ;
#1511 = CARTESIAN_POINT ( 'NONE',  ( -10.81189881249999729, 1.324075727343319199E-15, -12.78125000204835615 ) ) ;
#1512 = CARTESIAN_POINT ( 'NONE',  ( -10.81189881249999907, -6.242252689847864744, -19.96875000204837036 ) ) ;
#1513 = CARTESIAN_POINT ( 'NONE',  ( 4.999999999999992006, -8.660254037844389075, -152.6250000040967905 ) ) ;
#1514 = CARTESIAN_POINT ( 'NONE',  ( 10.81189881249999729, 0.000000000000000000, -118.3437500020483810 ) ) ;
#1515 = CARTESIAN_POINT ( 'NONE',  ( 4.999999999999992006, -8.660254037844389075, -93.74999999999998579 ) ) ;
#1516 = CARTESIAN_POINT ( 'NONE',  ( 5.405949406249999534, 9.363379034771803333, -25.28125000204836681 ) ) ;
#1517 = CARTESIAN_POINT ( 'NONE',  ( 7.070501591499377789E-16, 11.54700538379251284, -110.0000000040968047 ) ) ;
#1518 = CARTESIAN_POINT ( 'NONE',  ( -2.121150477449813534E-15, -11.54700538379251284, -49.25000000409676915 ) ) ;
#1519 = CARTESIAN_POINT ( 'NONE',  ( 10.00000000000000000, 5.773502691896255534, -54.37499999999997868 ) ) ;
#1520 = CARTESIAN_POINT ( 'NONE',  ( -10.81189881249999729, 6.242252689847871849, -120.9062500020483952 ) ) ;
#1521 = CARTESIAN_POINT ( 'NONE',  ( 7.644554776091147741E-16, 12.48450537969573659, -100.1562500020483952 ) ) ;
#1522 = EDGE_LOOP ( 'NONE', ( #14719, #38827, #7628, #15946 ) ) ;
#1523 = VECTOR ( 'NONE', #7678, 1000.000000000000000 ) ;
#1524 = CARTESIAN_POINT ( 'NONE',  ( 9.999999999999996447, -5.773502691896262640, -100.0000000040967763 ) ) ;
#1525 = CARTESIAN_POINT ( 'NONE',  ( 8.614196012143711556, -6.533971456633876684, 2.775557561562891351E-14 ) ) ;
#1526 = CARTESIAN_POINT ( 'NONE',  ( 7.644554776091147741E-16, 12.48450537969573659, -166.1562500020483810 ) ) ;
#1527 = CARTESIAN_POINT ( 'NONE',  ( -5.405949406250003975, -9.363379034771801557, -54.34375000204835970 ) ) ;
#1528 = ORIENTED_EDGE ( 'NONE', *, *, #29121, .F. ) ;
#1529 = CARTESIAN_POINT ( 'NONE',  ( 9.999999999999996447, -5.773502691896262640, -27.62499999999998579 ) ) ;
#1530 = CARTESIAN_POINT ( 'NONE',  ( -5.405949406250003975, -9.363379034771801557, -24.53125000204836681 ) ) ;
#1531 = CARTESIAN_POINT ( 'NONE',  ( 9.999999999999996447, -5.773502691896262640, -162.6250000000000284 ) ) ;
#1532 = CARTESIAN_POINT ( 'NONE',  ( 10.00000000000051159, -5.773502691895965988, -102.6249999999999858 ) ) ;
#1533 = CARTESIAN_POINT ( 'NONE',  ( -10.00000000000000000, -5.773502691896251982, -27.00000000409677625 ) ) ;
#1534 = CARTESIAN_POINT ( 'NONE',  ( 4.999999999999992006, -8.660254037844389075, -33.74999999999997158 ) ) ;
#1535 = CARTESIAN_POINT ( 'NONE',  ( -5.405949406249996869, 9.363379034771805109, -130.0312500020484094 ) ) ;
#1536 = CARTESIAN_POINT ( 'NONE',  ( 0.6477615133710965534, 10.23212146006973278, 1.249419088690773332E-14 ) ) ;
#1537 =( BOUNDED_CURVE ( )  B_SPLINE_CURVE ( 2, ( #23012, #29486, #22163, #26039, #22797, #29273, #36166 ),
 .UNSPECIFIED., .F., .F. ) 
 B_SPLINE_CURVE_WITH_KNOTS ( ( 3, 2, 2, 3 ),
 ( 0.1455223880597014963, 0.1467661691542288538, 0.1480099502487562391, 0.1492537313432835966 ),
 .UNSPECIFIED. ) 
 CURVE ( )  GEOMETRIC_REPRESENTATION_ITEM ( )  RATIONAL_B_SPLINE_CURVE ( ( 1.000000000000000000, 0.8660254037844387076, 1.000000000000000000, 0.8660254037844387076, 1.000000000000000000, 0.8660254037844357100, 1.000000000000003109 ) ) 
 REPRESENTATION_ITEM ( '' )  );
#1538 = LINE ( 'NONE', #14672, #12785 ) ;
#1539 = VERTEX_POINT ( 'NONE', #38464 ) ;
#1540 = CARTESIAN_POINT ( 'NONE',  ( 10.81189881249999907, 6.242252689847868297, -59.90625000204838813 ) ) ;
#1542 = VERTEX_POINT ( 'NONE', #8906 ) ;
#1541 = EDGE_LOOP ( 'NONE', ( #15994, #2474, #42330, #20143 ) ) ;
#1543 = CARTESIAN_POINT ( 'NONE',  ( 0.000000000000000000, 0.000000000000000000, -99.99999999999998579 ) ) ;
#1544 = AXIS2_PLACEMENT_3D ( 'NONE', #42021, #38801, #12243 ) ;
#1545 = LINE ( 'NONE', #40155, #18016 ) ;
#1546 = CARTESIAN_POINT ( 'NONE',  ( 10.81189881249999551, -6.242252689847874514, -164.9687500020484094 ) ) ;
#1547 = CARTESIAN_POINT ( 'NONE',  ( -10.81189881249999729, 6.242252689847871849, -186.9062500020484094 ) ) ;
#1548 = CARTESIAN_POINT ( 'NONE',  ( -10.81189881249999907, -6.242252689847864744, -16.96875000204836681 ) ) ;
#1549 = DIRECTION ( 'NONE',  ( -0.000000000000000000, -0.000000000000000000, 1.000000000000000000 ) ) ;
#1550 = CARTESIAN_POINT ( 'NONE',  ( -5.405949406249996869, 9.363379034771805109, -150.8437500020483810 ) ) ;
#1551 = CARTESIAN_POINT ( 'NONE',  ( 7.644554776091147741E-16, 12.48450537969573659, -125.4687500020483952 ) ) ;
#1552 = CARTESIAN_POINT ( 'NONE',  ( 7.644554776091147741E-16, 12.48450537969573659, -104.6562500020483810 ) ) ;
#1553 = CARTESIAN_POINT ( 'NONE',  ( -10.81189881249999729, 1.324075727343319199E-15, -116.0937500020483810 ) ) ;
#1554 = CARTESIAN_POINT ( 'NONE',  ( 7.070501591499376803E-16, 11.54700538379251284, -55.62499999999997158 ) ) ;
#1555 = CARTESIAN_POINT ( 'NONE',  ( -10.81189881249999729, 1.324075727343319199E-15, -128.2812500020483810 ) ) ;
#1556 = CARTESIAN_POINT ( 'NONE',  ( -5.405949406250003975, -9.363379034771801557, -4.843750002048369474 ) ) ;
#1558 = EDGE_CURVE ( 'NONE', #3006, #10534, #18160, .T. ) ;
#1557 = CARTESIAN_POINT ( 'NONE',  ( -2.293366432827344421E-15, -12.48450537969573659, -130.7187500020483810 ) ) ;
#1559 = CARTESIAN_POINT ( 'NONE',  ( -9.999999999998969713, -5.773502691896847949, -55.12499999999995737 ) ) ;
#1560 = CARTESIAN_POINT ( 'NONE',  ( 9.999999999999742428, 5.773502691896404748, -157.8750000000000000 ) ) ;
#1561 = CARTESIAN_POINT ( 'NONE',  ( -2.121150477449813534E-15, -11.54700538379251284, -149.3750000000000000 ) ) ;
#1562 = CARTESIAN_POINT ( 'NONE',  ( -5.000000000000003553, -8.660254037844383745, -21.99999999999996447 ) ) ;
#1563 = CIRCLE ( 'NONE', #31918, 57.00000000000002132 ) ;
#1564 = CARTESIAN_POINT ( 'NONE',  ( -10.81189881249999729, 6.242252689847871849, -74.21875000204836681 ) ) ;
#1565 = CARTESIAN_POINT ( 'NONE',  ( -5.405949406250003975, -9.363379034771801557, -64.84375000204836681 ) ) ;
#1566 = CARTESIAN_POINT ( 'NONE',  ( -9.999999999999998224, 1.224646799147353059E-15, -165.1250000040967905 ) ) ;
#1567 = CARTESIAN_POINT ( 'NONE',  ( 10.81189881249999907, 6.242252689847868297, -32.90625000204835970 ) ) ;
#1568 = CARTESIAN_POINT ( 'NONE',  ( -10.81189881249999729, 1.324075727343319199E-15, -42.59375000204837391 ) ) ;
#1569 = DIRECTION ( 'NONE',  ( -1.000000000000000000, 0.000000000000000000, 0.000000000000000000 ) ) ;
#1570 = CARTESIAN_POINT ( 'NONE',  ( -10.81189881249999729, 1.324075727343319199E-15, -152.0937500020483810 ) ) ;
#1571 = CARTESIAN_POINT ( 'NONE',  ( -2.121150477449813534E-15, -11.54700538379251284, -123.8749999999999858 ) ) ;
#1572 = CARTESIAN_POINT ( 'NONE',  ( -10.81189881249999729, 6.242252689847871849, -134.4062500020483810 ) ) ;
#1573 = PLANE ( 'NONE',  #12756 ) ;
#1574 = CARTESIAN_POINT ( 'NONE',  ( -5.000000000000003553, -8.660254037844383745, -78.99999999999998579 ) ) ;
#1575 = CARTESIAN_POINT ( 'NONE',  ( -5.405949406249996869, 9.363379034771805109, -11.53125000204835438 ) ) ;
#1576 = ORIENTED_EDGE ( 'NONE', *, *, #8183, .T. ) ;
#1577 = CARTESIAN_POINT ( 'NONE',  ( 5.405949406249999534, 9.363379034771803333, -100.2812500020483952 ) ) ;
#1578 = CARTESIAN_POINT ( 'NONE',  ( -9.999999999999998224, 5.773502691896259087, -120.2500000040967763 ) ) ;
#1579 = CARTESIAN_POINT ( 'NONE',  ( 9.999999999999998224, 0.000000000000000000, -200.0000000000000000 ) ) ;
#1580 = CARTESIAN_POINT ( 'NONE',  ( -2.121150477449813534E-15, -11.54700538379251284, -31.25000000409675494 ) ) ;
#1581 = LINE ( 'NONE', #26150, #8392 ) ;
#1582 = CARTESIAN_POINT ( 'NONE',  ( 5.405949406249999534, 9.363379034771803333, -43.28125000204838102 ) ) ;
#1583 =( BOUNDED_CURVE ( )  B_SPLINE_CURVE ( 2, ( #40246, #7044, #7248, #26260, #19765, #39409, #20398 ),
 .UNSPECIFIED., .F., .F. ) 
 B_SPLINE_CURVE_WITH_KNOTS ( ( 3, 2, 2, 3 ),
 ( 0.1716417910447761430, 0.1728855721393035005, 0.1741293532338308858, 0.1753731343283582433 ),
 .UNSPECIFIED. ) 
 CURVE ( )  GEOMETRIC_REPRESENTATION_ITEM ( )  RATIONAL_B_SPLINE_CURVE ( ( 0.9999999999999970024, 0.8660254037844417052, 1.000000000000000000, 0.8660254037844387076, 1.000000000000000000, 0.8660254037844357100, 1.000000000000003109 ) ) 
 REPRESENTATION_ITEM ( '' )  );
#1584 = CARTESIAN_POINT ( 'NONE',  ( -10.00000000000051337, 5.773502691895962435, -146.8749999999999716 ) ) ;
#1585 = CARTESIAN_POINT ( 'NONE',  ( 7.644554776091147741E-16, 12.48450537969573659, -151.1562500020484094 ) ) ;
#1586 = EDGE_CURVE ( 'NONE', #5725, #17896, #277, .T. ) ;
#1587 = CARTESIAN_POINT ( 'NONE',  ( -5.405949406250003975, -9.363379034771801557, -124.8437500020483810 ) ) ;
#1588 = LINE ( 'NONE', #17524, #37896 ) ;
#1589 = ORIENTED_EDGE ( 'NONE', *, *, #31560, .F. ) ;
#1590 = LINE ( 'NONE', #23815, #20361 ) ;
#1591 = VERTEX_POINT ( 'NONE', #28126 ) ;
#1592 = ORIENTED_EDGE ( 'NONE', *, *, #14066, .T. ) ;
#1593 = ORIENTED_EDGE ( 'NONE', *, *, #39837, .F. ) ;
#1594 = CARTESIAN_POINT ( 'NONE',  ( 5.000000000000000000, 8.660254037844385522, -189.2500000000000000 ) ) ;
#1595 = CARTESIAN_POINT ( 'NONE',  ( 5.405949406249992428, -9.363379034771808662, -190.5937500020484094 ) ) ;
#1596 = CARTESIAN_POINT ( 'NONE',  ( 10.81189881249999907, 6.242252689847868297, -41.71875000204835260 ) ) ;
#1597 = CARTESIAN_POINT ( 'NONE',  ( -3.354946414818984479, -9.739129128211180486, 6.879861566379088064E-16 ) ) ;
#1598 = CARTESIAN_POINT ( 'NONE',  ( 10.81189881249999551, -6.242252689847874514, -170.9687500020483810 ) ) ;
#1599 = CARTESIAN_POINT ( 'NONE',  ( 5.405949406249999534, 9.363379034771803333, -151.0937500020483810 ) ) ;
#1600 = CARTESIAN_POINT ( 'NONE',  ( 4.999999999999992006, -8.660254037844389075, -65.62500000409676204 ) ) ;
#1601 = CARTESIAN_POINT ( 'NONE',  ( 10.81189881249999907, 6.242252689847868297, -143.7187500020483810 ) ) ;
#1602 = CARTESIAN_POINT ( 'NONE',  ( 10.81189881249999551, -6.242252689847874514, -148.6562500020484094 ) ) ;
#1603 = CARTESIAN_POINT ( 'NONE',  ( 10.81189881249999729, 0.000000000000000000, -157.3437500020483810 ) ) ;
#1604 = CARTESIAN_POINT ( 'NONE',  ( 7.070501591499376803E-16, 11.54700538379251284, -126.5000000040967763 ) ) ;
#1605 = CARTESIAN_POINT ( 'NONE',  ( 0.000000000000000000, 0.000000000000000000, -99.99999999999998579 ) ) ;
#1606 = CARTESIAN_POINT ( 'NONE',  ( -9.999999999999998224, 5.773502691896259087, -172.3750000000000000 ) ) ;
#1607 = CARTESIAN_POINT ( 'NONE',  ( -5.405949406249996869, 9.363379034771805109, -86.34375000204836681 ) ) ;
#1608 = CYLINDRICAL_SURFACE ( 'NONE', #42379, 9.999999999999998224 ) ;
#1609 = CARTESIAN_POINT ( 'NONE',  ( 7.644554776091147741E-16, 12.48450537969573659, -58.15625000204838102 ) ) ;
#1610 = FACE_OUTER_BOUND ( 'NONE', #15524, .T. ) ;
#1611 = EDGE_CURVE ( 'NONE', #20180, #24638, #19344, .T. ) ;
#1612 = CARTESIAN_POINT ( 'NONE',  ( 10.81189881249999729, 0.000000000000000000, -176.8437500020483810 ) ) ;
#1613 = CARTESIAN_POINT ( 'NONE',  ( -5.405949406249996869, 9.363379034771805109, -118.0312500020483952 ) ) ;
#1614 = CARTESIAN_POINT ( 'NONE',  ( 7.644554776091147741E-16, 12.48450537969573659, -152.6562500020484094 ) ) ;
#1615 = CARTESIAN_POINT ( 'NONE',  ( -9.999999999999998224, 1.224646799147353059E-15, -11.74999999999995559 ) ) ;
#1616 = CARTESIAN_POINT ( 'NONE',  ( 10.81189881249999551, -6.242252689847874514, -45.15625000204836681 ) ) ;
#1617 = CARTESIAN_POINT ( 'NONE',  ( -5.000000000000003553, -8.660254037844383745, -133.3750000040967905 ) ) ;
#1618 = CARTESIAN_POINT ( 'NONE',  ( -4.999999999999996447, 8.660254037844387298, -95.99999999999998579 ) ) ;
#1619 = ORIENTED_EDGE ( 'NONE', *, *, #27249, .F. ) ;
#1620 = CARTESIAN_POINT ( 'NONE',  ( -10.81189881249999729, 6.242252689847871849, -126.9062500020483810 ) ) ;
#1621 = CARTESIAN_POINT ( 'NONE',  ( -4.999999999999996447, 8.660254037844387298, -145.8750000040967905 ) ) ;
#1622 = DIRECTION ( 'NONE',  ( -0.000000000000000000, 1.000000000000000000, -0.000000000000000000 ) ) ;
#1623 = CARTESIAN_POINT ( 'NONE',  ( 7.644554776091147741E-16, 12.48450537969573659, -179.6562500020484094 ) ) ;
#1624 = ORIENTED_EDGE ( 'NONE', *, *, #4298, .F. ) ;
#1625 = CARTESIAN_POINT ( 'NONE',  ( 10.81189881249999729, 0.000000000000000000, -170.8437500020484094 ) ) ;
#1626 = CARTESIAN_POINT ( 'NONE',  ( -4.999999999999996447, 8.660254037844387298, -54.37500000409675494 ) ) ;
#1627 = DIRECTION ( 'NONE',  ( 1.000000000000000000, 0.000000000000000000, 0.000000000000000000 ) ) ;
#1628 = DIRECTION ( 'NONE',  ( -0.000000000000000000, -0.000000000000000000, 1.000000000000000000 ) ) ;
#1629 = CARTESIAN_POINT ( 'NONE',  ( 10.81189881249999907, 6.242252689847868297, -68.90625000204839523 ) ) ;
#1630 = CARTESIAN_POINT ( 'NONE',  ( -5.405949406250003975, -9.363379034771801557, -51.53125000204835970 ) ) ;
#1631 = CARTESIAN_POINT ( 'NONE',  ( 7.070501591499377789E-16, 11.54700538379251284, -47.00000000409676915 ) ) ;
#1632 = CARTESIAN_POINT ( 'NONE',  ( 10.81189881249999729, 0.000000000000000000, -1.343750002048366143 ) ) ;
#1633 = CARTESIAN_POINT ( 'NONE',  ( -9.999999999999998224, 1.224646799147353059E-15, -192.1250000040967905 ) ) ;
#1634 = CARTESIAN_POINT ( 'NONE',  ( 7.644554776091147741E-16, 12.48450537969573659, -176.6562500020484094 ) ) ;
#1635 = LINE ( 'NONE', #30992, #16622 ) ;
#1636 = CARTESIAN_POINT ( 'NONE',  ( -45.00000000000000711, 0.000000000000000000, -217.0000000000000853 ) ) ;
#1637 = VERTEX_POINT ( 'NONE', #18825 ) ;
#1638 = CARTESIAN_POINT ( 'NONE',  ( 9.999999999999998224, 0.000000000000000000, -77.37500000409677625 ) ) ;
#1639 = CARTESIAN_POINT ( 'NONE',  ( -5.500000000000005329, -20.00000000000000000, -232.0000000000000000 ) ) ;
#1640 = CARTESIAN_POINT ( 'NONE',  ( -9.999999999999998224, 1.224646799147353059E-15, -73.24999999999998579 ) ) ;
#1642 = ORIENTED_EDGE ( 'NONE', *, *, #20048, .F. ) ;
#1641 = CARTESIAN_POINT ( 'NONE',  ( 10.81189881249999729, 0.000000000000000000, -87.03125000204838102 ) ) ;
#1644 = VERTEX_POINT ( 'NONE', #2013 ) ;
#1643 = DIRECTION ( 'NONE',  ( -1.000000000000000000, 0.000000000000000000, 0.000000000000000000 ) ) ;
#1645 = ORIENTED_EDGE ( 'NONE', *, *, #37760, .T. ) ;
#1646 = CARTESIAN_POINT ( 'NONE',  ( -10.81189881249999729, -6.242252689847864744, -33.46875000204834549 ) ) ;
#1647 = CARTESIAN_POINT ( 'NONE',  ( 5.000000000000000000, -20.00000000000000000, -235.0000000000000000 ) ) ;
#1648 = CARTESIAN_POINT ( 'NONE',  ( -10.81189881249999729, 1.324075727343319199E-15, -17.28125000204835970 ) ) ;
#1650 = VERTEX_POINT ( 'NONE', #15142 ) ;
#1649 = CARTESIAN_POINT ( 'NONE',  ( -10.81189881249999729, 6.242252689847871849, -60.71875000204838102 ) ) ;
#1651 = CARTESIAN_POINT ( 'NONE',  ( 10.00000000000025402, -5.773502691896113426, -131.1250000000000000 ) ) ;
#1652 = CARTESIAN_POINT ( 'NONE',  ( 9.999999999999998224, 0.000000000000000000, -39.49999999999997868 ) ) ;
#1653 = CARTESIAN_POINT ( 'NONE',  ( 5.405949406249999534, 9.363379034771803333, -182.5937500020483810 ) ) ;
#1654 = CARTESIAN_POINT ( 'NONE',  ( -2.293366432827344421E-15, -12.48450537969573659, -166.7187500020484094 ) ) ;
#1655 = CARTESIAN_POINT ( 'NONE',  ( -10.81189881249999729, 1.324075727343319199E-15, -179.0937500020484094 ) ) ;
#1656 = CARTESIAN_POINT ( 'NONE',  ( -4.999999999999996447, 8.660254037844387298, -199.5000000000000000 ) ) ;
#1657 = CARTESIAN_POINT ( 'NONE',  ( 10.00000000000000000, 5.773502691896255534, -192.3750000000000000 ) ) ;
#1659 = CARTESIAN_POINT ( 'NONE',  ( -5.405949406249996869, 9.363379034771805109, -114.8437500020483810 ) ) ;
#1658 = APPLICATION_CONTEXT ( 'configuration controlled 3d designs of mechanical parts and assemblies' ) ;
#1660 = CYLINDRICAL_SURFACE ( 'NONE', #36972, 20.00000000000000000 ) ;
#1661 = CARTESIAN_POINT ( 'NONE',  ( -2.293366432827344421E-15, -12.48450537969573659, -85.90625000204839523 ) ) ;
#1662 = EDGE_CURVE ( 'NONE', #4880, #35877, #28340, .T. ) ;
#1663 = CARTESIAN_POINT ( 'NONE',  ( 10.81189881249999729, 6.242252689847867408, -95.71875000204838102 ) ) ;
#1664 =( BOUNDED_CURVE ( )  B_SPLINE_CURVE ( 2, ( #16887, #3328, #42587, #528, #312, #3755, #13012 ),
 .UNSPECIFIED., .F., .F. ) 
 B_SPLINE_CURVE_WITH_KNOTS ( ( 3, 2, 2, 3 ),
 ( 0.3358208955223880854, 0.3370646766169154707, 0.3383084577114429670, 0.3395522388059703522 ),
 .UNSPECIFIED. ) 
 CURVE ( )  GEOMETRIC_REPRESENTATION_ITEM ( )  RATIONAL_B_SPLINE_CURVE ( ( 1.000000000000000000, 0.8660254037844387076, 1.000000000000000000, 0.8660254037844387076, 1.000000000000000000, 0.8660254037844148378, 1.000000000000023981 ) ) 
 REPRESENTATION_ITEM ( '' )  );
#1665 = CARTESIAN_POINT ( 'NONE',  ( 7.644554776091147741E-16, 12.48450537969573659, -62.46875000204838102 ) ) ;
#1666 = ADVANCED_FACE ( 'NONE', ( #3485 ), #9741, .F. ) ;
#1667 = CARTESIAN_POINT ( 'NONE',  ( -2.293366432827344421E-15, -12.48450537969573659, -69.40625000204838102 ) ) ;
#1668 = CARTESIAN_POINT ( 'NONE',  ( -9.999999999999998224, 1.224646799147353059E-15, -151.6250000040967905 ) ) ;
#1669 = CARTESIAN_POINT ( 'NONE',  ( 4.999999999999992006, -8.660254037844389075, -129.7499999999999716 ) ) ;
#1670 = EDGE_CURVE ( 'NONE', #32685, #13020, #6513, .T. ) ;
#1671 = CARTESIAN_POINT ( 'NONE',  ( 10.81189881249999551, -6.242252689847874514, -153.1562500020484094 ) ) ;
#1672 = CARTESIAN_POINT ( 'NONE',  ( 10.81189881249999551, -6.242252689847874514, -160.6562500020484379 ) ) ;
#1673 = CARTESIAN_POINT ( 'NONE',  ( 10.00000000000154010, -5.773502691895370020, -13.00000000409671941 ) ) ;
#1674 = FACE_OUTER_BOUND ( 'NONE', #527, .T. ) ;
#1675 = CARTESIAN_POINT ( 'NONE',  ( 10.81189881249999907, 6.242252689847868297, -97.21875000204836681 ) ) ;
#1676 = CARTESIAN_POINT ( 'NONE',  ( -4.999999999999996447, 8.660254037844387298, -42.37500000409677625 ) ) ;
#1677 = CARTESIAN_POINT ( 'NONE',  ( -9.999999999999998224, 1.224646799147353059E-15, -71.74999999999998579 ) ) ;
#1678 = CARTESIAN_POINT ( 'NONE',  ( -10.81189881249999729, 1.324075727343319199E-15, -195.5937500020484094 ) ) ;
#1679 = CARTESIAN_POINT ( 'NONE',  ( 5.000000000000000000, 8.660254037844385522, -78.62500000409677625 ) ) ;
#1680 = CARTESIAN_POINT ( 'NONE',  ( -7.482077728350252421, -6.785286198130088486, -179.9999999999999432 ) ) ;
#1681 = CARTESIAN_POINT ( 'NONE',  ( 10.81189881249999551, -6.242252689847874514, -90.15625000204836681 ) ) ;
#1682 = CARTESIAN_POINT ( 'NONE',  ( -5.405949406250003975, -9.363379034771801557, -78.53125000204838102 ) ) ;
#1683 = CARTESIAN_POINT ( 'NONE',  ( 10.00000000000000000, 5.773502691896255534, -69.75000000409679046 ) ) ;
#1684 = CARTESIAN_POINT ( 'NONE',  ( -10.00000000000051337, 5.773502691895962435, -112.7500000040967620 ) ) ;
#1685 = CARTESIAN_POINT ( 'NONE',  ( 10.81189881249999551, -6.242252689847874514, -28.46875000204837391 ) ) ;
#1686 = ORIENTED_EDGE ( 'NONE', *, *, #38833, .F. ) ;
#1687 = CARTESIAN_POINT ( 'NONE',  ( 9.999999999999998224, 0.000000000000000000, -1.999999999999974021 ) ) ;
#1688 = CARTESIAN_POINT ( 'NONE',  ( 5.405949406249999534, 9.363379034771803333, -17.78125000204835970 ) ) ;
#1689 = CARTESIAN_POINT ( 'NONE',  ( -5.405949406250003975, -9.363379034771801557, -13.84375000204834905 ) ) ;
#1690 = CARTESIAN_POINT ( 'NONE',  ( -9.999999999999998224, 1.224646799147353059E-15, -13.62500000409674961 ) ) ;
#1691 = EDGE_CURVE ( 'NONE', #31210, #317, #22583, .T. ) ;
#1692 = CARTESIAN_POINT ( 'NONE',  ( 7.070501591499377789E-16, 11.54700538379251284, -2.000000004096752715 ) ) ;
#1693 = CARTESIAN_POINT ( 'NONE',  ( -9.999999999999998224, 1.224646799147353059E-15, -196.2500000000000000 ) ) ;
#1694 = CARTESIAN_POINT ( 'NONE',  ( 5.405949406249992428, -9.363379034771808662, -130.7812500020483810 ) ) ;
#1695 = EDGE_CURVE ( 'NONE', #38211, #15832, #13172, .T. ) ;
#1696 = CARTESIAN_POINT ( 'NONE',  ( 10.00000000000000000, 5.773502691896255534, -184.8750000000000000 ) ) ;
#1697 = CARTESIAN_POINT ( 'NONE',  ( -5.000000000000003553, -8.660254037844383745, -35.87500000409676915 ) ) ;
#1699 = ORIENTED_EDGE ( 'NONE', *, *, #30651, .T. ) ;
#1698 = CARTESIAN_POINT ( 'NONE',  ( -5.405949406249996869, 9.363379034771805109, -112.0312500020483810 ) ) ;
#1700 = DIRECTION ( 'NONE',  ( 1.000000000000000000, 0.000000000000000000, 0.000000000000000000 ) ) ;
#1701 = EDGE_CURVE ( 'NONE', #8431, #29237, #19242, .T. ) ;
#1702 = ORIENTED_EDGE ( 'NONE', *, *, #36445, .T. ) ;
#1703 = PERSON ( 'NAUO-PER6', 'UNSPECIFIED', 'UNSPECIFIED', ('UNSPECIFIED'), ('UNSPECIFIED'), ('UNSPECIFIED') ) ;
#1704 = ORIENTED_EDGE ( 'NONE', *, *, #24624, .F. ) ;
#1705 = CARTESIAN_POINT ( 'NONE',  ( -10.81189881249999729, 6.242252689847871849, -35.40625000204836681 ) ) ;
#1706 = MECHANICAL_CONTEXT ( 'NONE', #34764, 'mechanical' ) ;
#1707 = CARTESIAN_POINT ( 'NONE',  ( -10.81189881249999729, 1.324075727343319199E-15, -86.09375000204836681 ) ) ;
#1708 = CARTESIAN_POINT ( 'NONE',  ( 0.000000000000000000, 0.000000000000000000, -99.99999999999998579 ) ) ;
#1709 = CARTESIAN_POINT ( 'NONE',  ( -9.999999999999998224, 1.224646799147353059E-15, -109.2499999999999858 ) ) ;
#1710 =( BOUNDED_CURVE ( )  B_SPLINE_CURVE ( 2, ( #32609, #42082, #25707, #9284, #6060, #9500, #15955 ),
 .UNSPECIFIED., .F., .F. ) 
 B_SPLINE_CURVE_WITH_KNOTS ( ( 3, 2, 2, 3 ),
 ( 0.2574626865671643117, 0.2587064676616916414, 0.2599502487562190267, 0.2611940298507463565 ),
 .UNSPECIFIED. ) 
 CURVE ( )  GEOMETRIC_REPRESENTATION_ITEM ( )  RATIONAL_B_SPLINE_CURVE ( ( 0.9999999999999880096, 0.8660254037844506980, 1.000000000000000000, 0.8660254037844387076, 1.000000000000000000, 0.8660254037844267172, 1.000000000000011990 ) ) 
 REPRESENTATION_ITEM ( '' )  );
#1711 = LINE ( 'NONE', #23570, #15010 ) ;
#1712 = CARTESIAN_POINT ( 'NONE',  ( -10.81189881249999729, 1.324075727343319199E-15, -167.2812500020484094 ) ) ;
#1713 = DIRECTION ( 'NONE',  ( -0.000000000000000000, -0.000000000000000000, -1.000000000000000000 ) ) ;
#1714 = CARTESIAN_POINT ( 'NONE',  ( 7.644554776091147741E-16, 12.48450537969573659, -120.9687500020483952 ) ) ;
#1715 = CARTESIAN_POINT ( 'NONE',  ( 10.81189881249999907, 6.242252689847868297, -89.71875000204836681 ) ) ;
#1716 = CARTESIAN_POINT ( 'NONE',  ( -9.999999999999998224, 1.224646799147353059E-15, -166.6250000040967905 ) ) ;
#1717 = CARTESIAN_POINT ( 'NONE',  ( -5.405949406250003975, -9.363379034771801557, -192.3437500020484094 ) ) ;
#1718 = CARTESIAN_POINT ( 'NONE',  ( -5.405949406249996869, 9.363379034771805109, -95.53125000204838102 ) ) ;
#1719 = CARTESIAN_POINT ( 'NONE',  ( 9.999999999999996447, -5.773502691896262640, -181.0000000040968189 ) ) ;
#1720 = CARTESIAN_POINT ( 'NONE',  ( 10.81189881249999551, -6.242252689847874514, -168.1562500020484094 ) ) ;
#1721 = EDGE_CURVE ( 'NONE', #40615, #41419, #39953, .T. ) ;
#1722 =( BOUNDED_CURVE ( )  B_SPLINE_CURVE ( 2, ( #19865, #682, #36283, #39510, #9732, #13586, #39931 ),
 .UNSPECIFIED., .F., .F. ) 
 B_SPLINE_CURVE_WITH_KNOTS ( ( 3, 2, 2, 3 ),
 ( 0.1865671641791045166, 0.1878109452736318741, 0.1890547263681592594, 0.1902985074626866169 ),
 .UNSPECIFIED. ) 
 CURVE ( )  GEOMETRIC_REPRESENTATION_ITEM ( )  RATIONAL_B_SPLINE_CURVE ( ( 0.9999999999999970024, 0.8660254037844417052, 1.000000000000000000, 0.8660254037844387076, 1.000000000000000000, 0.8660254037844327124, 1.000000000000005995 ) ) 
 REPRESENTATION_ITEM ( '' )  );
#1723 = LINE ( 'NONE', #15488, #13715 ) ;
#1724 = CARTESIAN_POINT ( 'NONE',  ( -5.405949406249996869, 9.363379034771805109, -175.0312500020484094 ) ) ;
#1725 = CARTESIAN_POINT ( 'NONE',  ( 10.81189881249999551, -6.242252689847874514, -192.1562500020484094 ) ) ;
#1726 = CARTESIAN_POINT ( 'NONE',  ( -2.293366432827344421E-15, -12.48450537969573659, -51.21875000204836681 ) ) ;
#1727 = EDGE_CURVE ( 'NONE', #30416, #22548, #14877, .T. ) ;
#1728 = CARTESIAN_POINT ( 'NONE',  ( 5.000000000000000000, 8.660254037844385522, -162.6250000040967905 ) ) ;
#1729 = CARTESIAN_POINT ( 'NONE',  ( 5.405949406249999534, 9.363379034771803333, -8.781250002048352599 ) ) ;
#1730 = CARTESIAN_POINT ( 'NONE',  ( -2.293366432827344421E-15, -12.48450537969573659, -13.71875000204836326 ) ) ;
#1731 = CARTESIAN_POINT ( 'NONE',  ( -9.999999999999998224, 1.224646799147353059E-15, -91.24999999999998579 ) ) ;
#1732 = CARTESIAN_POINT ( 'NONE',  ( -10.81189881249999729, 1.324075727343319199E-15, -122.0937500020483952 ) ) ;
#1733 = CARTESIAN_POINT ( 'NONE',  ( 9.999999999999996447, -5.773502691896262640, -101.1250000000000000 ) ) ;
#1734 = CARTESIAN_POINT ( 'NONE',  ( 7.644554776091147741E-16, 12.48450537969573659, -19.15625000204837391 ) ) ;
#1735 = CARTESIAN_POINT ( 'NONE',  ( 4.999999999999992006, -8.660254037844389075, -107.6250000040967763 ) ) ;
#1736 = FACE_OUTER_BOUND ( 'NONE', #34180, .T. ) ;
#1737 = CARTESIAN_POINT ( 'NONE',  ( 9.999999999999996447, -5.773502691896262640, -50.12499999999997868 ) ) ;
#1738 = CARTESIAN_POINT ( 'NONE',  ( 7.644554776091147741E-16, 12.48450537969573659, -118.1562500020483952 ) ) ;
#1739 = CARTESIAN_POINT ( 'NONE',  ( -2.293366432827344421E-15, -12.48450537969573659, -100.9062500020483952 ) ) ;
#1740 = ORIENTED_EDGE ( 'NONE', *, *, #6099, .T. ) ;
#1741 = CARTESIAN_POINT ( 'NONE',  ( 9.999999999999996447, -5.773502691896262640, -92.50000000409677625 ) ) ;
#1742 = CARTESIAN_POINT ( 'NONE',  ( 9.999999999999998224, 0.000000000000000000, -165.8750000040967905 ) ) ;
#1743 = CARTESIAN_POINT ( 'NONE',  ( 10.81189881249999729, 0.000000000000000000, -156.0312500020484094 ) ) ;
#1744 = CARTESIAN_POINT ( 'NONE',  ( -2.293366432827344421E-15, -12.48450537969573659, -46.71875000204835970 ) ) ;
#1745 = ORIENTED_EDGE ( 'NONE', *, *, #21741, .F. ) ;
#1746 = CARTESIAN_POINT ( 'NONE',  ( -4.999999999999996447, 8.660254037844387298, -28.49999999999997158 ) ) ;
#1747 = CARTESIAN_POINT ( 'NONE',  ( 10.81189881249999729, 6.242252689847867408, -31.40625000204834905 ) ) ;
#1748 = CARTESIAN_POINT ( 'NONE',  ( 4.999999999999992006, -8.660254037844389075, -164.2500000000000000 ) ) ;
#1749 = CYLINDRICAL_SURFACE ( 'NONE', #11124, 9.999999999999998224 ) ;
#1750 = CARTESIAN_POINT ( 'NONE',  ( 5.000000000000000000, 8.660254037844385522, -30.62500000409676559 ) ) ;
#1751 = EDGE_CURVE ( 'NONE', #16776, #39083, #12547, .T. ) ;
#1752 = CARTESIAN_POINT ( 'NONE',  ( 9.999999999999998224, 0.000000000000000000, -33.49999999999997158 ) ) ;
#1753 = CARTESIAN_POINT ( 'NONE',  ( 5.405949406249992428, -9.363379034771808662, -136.7812500020483810 ) ) ;
#1754 = CARTESIAN_POINT ( 'NONE',  ( 8.934005281565452705, 5.771751285519217234, -7.741086494507744060E-15 ) ) ;
#1755 = CARTESIAN_POINT ( 'NONE',  ( -9.999999999999479527, -5.773502691896549521, -69.00000000409677625 ) ) ;
#1756 = VERTEX_POINT ( 'NONE', #38891 ) ;
#1757 = CARTESIAN_POINT ( 'NONE',  ( 5.405949406249999534, 9.363379034771803333, -59.78125000204836681 ) ) ;
#1758 = CALENDAR_DATE ( 2026, 28, 9 ) ;
#1760 = VERTEX_POINT ( 'NONE', #10162 ) ;
#1759 = ORIENTED_EDGE ( 'NONE', *, *, #41440, .T. ) ;
#1761 = DIRECTION ( 'NONE',  ( -0.000000000000000000, -0.000000000000000000, 1.000000000000000000 ) ) ;
#1762 = CARTESIAN_POINT ( 'NONE',  ( 5.405949406249999534, 9.363379034771803333, -158.5937500020483810 ) ) ;
#1763 = AXIS2_PLACEMENT_3D ( 'NONE', #7556, #33682, #13996 ) ;
#1764 = CARTESIAN_POINT ( 'NONE',  ( 10.81189881249999907, 6.242252689847868297, -188.9062500020484379 ) ) ;
#1765 = CARTESIAN_POINT ( 'NONE',  ( -10.81189881249999729, 1.324075727343319199E-15, -8.093750002048343717 ) ) ;
#1766 = DIRECTION ( 'NONE',  ( -0.000000000000000000, -0.000000000000000000, 1.000000000000000000 ) ) ;
#1767 = CARTESIAN_POINT ( 'NONE',  ( -2.293366432827344421E-15, -12.48450537969573659, -147.2187500020484094 ) ) ;
#1768 = CARTESIAN_POINT ( 'NONE',  ( -10.81189881249999907, -6.242252689847864744, -104.1562500020483668 ) ) ;
#1769 = CARTESIAN_POINT ( 'NONE',  ( 5.405949406249999534, 9.363379034771803333, -107.5937500020483810 ) ) ;
#1770 = CARTESIAN_POINT ( 'NONE',  ( -5.405949406250003975, -9.363379034771801557, -117.5312500020483952 ) ) ;
#1771 = CARTESIAN_POINT ( 'NONE',  ( 5.405949406249999534, 9.363379034771803333, -2.593750002048367254 ) ) ;
#1772 = CARTESIAN_POINT ( 'NONE',  ( 10.81189881249999551, -6.242252689847874514, -130.4687500020483810 ) ) ;
#1773 = CARTESIAN_POINT ( 'NONE',  ( 5.405949406249999534, 9.363379034771803333, -194.7812500020484094 ) ) ;
#1774 = CARTESIAN_POINT ( 'NONE',  ( 9.999999999999998224, 0.000000000000000000, -200.0000000000000000 ) ) ;
#1775 = CARTESIAN_POINT ( 'NONE',  ( 4.999999999999992006, -8.660254037844389075, -146.2500000000000000 ) ) ;
#1776 = CARTESIAN_POINT ( 'NONE',  ( 9.999999999999998224, 0.000000000000000000, -13.99999999999995737 ) ) ;
#1777 = CARTESIAN_POINT ( 'NONE',  ( -10.81189881249999729, 1.324075727343319199E-15, -75.59375000204838102 ) ) ;
#1778 = CARTESIAN_POINT ( 'NONE',  ( -10.81189881249999907, -6.242252689847864744, -60.46875000204838102 ) ) ;
#1779 = CARTESIAN_POINT ( 'NONE',  ( 5.000000000000000000, 8.660254037844385522, -191.1250000040967905 ) ) ;
#1780 = CARTESIAN_POINT ( 'NONE',  ( -5.405949406250003975, -9.363379034771801557, -33.53125000204837391 ) ) ;
#1781 = CARTESIAN_POINT ( 'NONE',  ( 10.81189881249999551, -6.242252689847874514, -35.96875000204835260 ) ) ;
#1782 = DIRECTION ( 'NONE',  ( -1.000000000000000000, 0.000000000000000000, 0.000000000000000000 ) ) ;
#1783 = CARTESIAN_POINT ( 'NONE',  ( 5.405949406249992428, -9.363379034771808662, -144.0937500020483810 ) ) ;
#1784 = CARTESIAN_POINT ( 'NONE',  ( 9.999999999999998224, 0.000000000000000000, -125.0000000000000000 ) ) ;
#1785 = CARTESIAN_POINT ( 'NONE',  ( 4.999999999999992006, -8.660254037844389075, -101.6250000040967905 ) ) ;
#1786 = CIRCLE ( 'NONE', #33508, 15.00000000000001066 ) ;
#1787 = CARTESIAN_POINT ( 'NONE',  ( -2.121150477449813534E-15, -11.54700538379251284, -77.37499999999997158 ) ) ;
#1788 = CARTESIAN_POINT ( 'NONE',  ( 10.81189881249999551, -6.242252689847874514, -10.65625000204838280 ) ) ;
#1789 = VERTEX_POINT ( 'NONE', #19450 ) ;
#1790 = CARTESIAN_POINT ( 'NONE',  ( -6.652853726956785785, 8.522716305231336165, -100.0000000000000142 ) ) ;
#1791 = CARTESIAN_POINT ( 'NONE',  ( 7.070501591499377789E-16, 11.54700538379251284, -126.5000000040967905 ) ) ;
#1792 = DIRECTION ( 'NONE',  ( 1.000000000000000000, 0.000000000000000000, 0.000000000000000000 ) ) ;
#1793 = CARTESIAN_POINT ( 'NONE',  ( -10.81189881249999729, 1.324075727343319199E-15, -78.59375000204838102 ) ) ;
#1794 = ADVANCED_FACE ( 'NONE', ( #19875 ), #16405, .T. ) ;
#1795 = CARTESIAN_POINT ( 'NONE',  ( -9.999999999999998224, 5.773502691896259087, -37.75000000409676204 ) ) ;
#1796 = VECTOR ( 'NONE', #15573, 1000.000000000000000 ) ;
#1797 =( BOUNDED_CURVE ( )  B_SPLINE_CURVE ( 2, ( #37492, #33630, #3642, #16769, #11574, #41355, #27788 ),
 .UNSPECIFIED., .F., .F. ) 
 B_SPLINE_CURVE_WITH_KNOTS ( ( 3, 2, 2, 3 ),
 ( 0.3246268656716419510, 0.3258706467661692807, 0.3271144278606965550, 0.3283582089552238847 ),
 .UNSPECIFIED. ) 
 CURVE ( )  GEOMETRIC_REPRESENTATION_ITEM ( )  RATIONAL_B_SPLINE_CURVE ( ( 0.9999999999999820144, 0.8660254037844566932, 1.000000000000000000, 0.8660254037844387076, 1.000000000000000000, 0.8660254037844387076, 1.000000000000000000 ) ) 
 REPRESENTATION_ITEM ( '' )  );
#1798 = CYLINDRICAL_SURFACE ( 'NONE', #42121, 9.999999999999998224 ) ;
#1799 = CARTESIAN_POINT ( 'NONE',  ( -10.81189881249999729, 6.242252689847871849, -42.90625000204836681 ) ) ;
#1800 = CARTESIAN_POINT ( 'NONE',  ( 9.999999999999994671, -5.773502691896262640, -137.1250000000000000 ) ) ;
#1801 = CARTESIAN_POINT ( 'NONE',  ( 5.405949406249992428, -9.363379034771808662, -147.2812500020483810 ) ) ;
#1802 = CARTESIAN_POINT ( 'NONE',  ( -10.81189881249999907, -6.242252689847864744, -123.4687500020483810 ) ) ;
#1803 = CARTESIAN_POINT ( 'NONE',  ( 10.00000000000000000, 5.773502691896255534, -165.7500000040967905 ) ) ;
#1804 = FACE_OUTER_BOUND ( 'NONE', #27162, .T. ) ;
#1806 = EDGE_CURVE ( 'NONE', #22821, #35538, #264, .T. ) ;
#1805 = ORIENTED_EDGE ( 'NONE', *, *, #14608, .F. ) ;
#1807 = ORIENTED_EDGE ( 'NONE', *, *, #32387, .F. ) ;
#1808 = ORIENTED_EDGE ( 'NONE', *, *, #29272, .F. ) ;
#1809 = AXIS2_PLACEMENT_3D ( 'NONE', #26701, #34039, #16752 ) ;
#1810 = DIRECTION ( 'NONE',  ( 0.000000000000000000, 1.000000000000000000, 0.000000000000000000 ) ) ;
#1811 = CARTESIAN_POINT ( 'NONE',  ( -5.405949406249996869, 9.363379034771805109, -182.3437500020483810 ) ) ;
#1812 = CARTESIAN_POINT ( 'NONE',  ( 10.81189881249999907, 6.242252689847868297, -38.71875000204835260 ) ) ;
#1813 = CARTESIAN_POINT ( 'NONE',  ( 7.070501591499376803E-16, 11.54700538379251284, -118.6250000000000142 ) ) ;
#1814 = CARTESIAN_POINT ( 'NONE',  ( -10.81189881249999729, 1.324075727343319199E-15, -173.0937500020484094 ) ) ;
#1815 = AXIS2_PLACEMENT_3D ( 'NONE', #36846, #20441, #33626 ) ;
#1816 = CARTESIAN_POINT ( 'NONE',  ( -5.405949406249996869, 9.363379034771805109, -156.8437500020483810 ) ) ;
#1817 = CARTESIAN_POINT ( 'NONE',  ( -9.999999999999998224, 1.224646799147353059E-15, -123.1250000040967905 ) ) ;
#1818 = CARTESIAN_POINT ( 'NONE',  ( 10.81189881249999729, 0.000000000000000000, -131.8437500020484094 ) ) ;
#1819 = CARTESIAN_POINT ( 'NONE',  ( 7.644554776091147741E-16, 12.48450537969573659, -137.6562500020483810 ) ) ;
#1820 = CARTESIAN_POINT ( 'NONE',  ( -10.81189881249999729, 6.242252689847871849, -152.2187500020483810 ) ) ;
#1821 = CARTESIAN_POINT ( 'NONE',  ( -9.999999999999998224, 1.224646799147353059E-15, -134.7499999999999716 ) ) ;
#1822 = CARTESIAN_POINT ( 'NONE',  ( 9.999999999999998224, 0.000000000000000000, -177.8750000040967905 ) ) ;
#1823 = CARTESIAN_POINT ( 'NONE',  ( -5.000000000000003553, -8.660254037844383745, -173.5000000000000284 ) ) ;
#1824 = CARTESIAN_POINT ( 'NONE',  ( -5.405949406249996869, 9.363379034771805109, -81.84375000204838102 ) ) ;
#1825 = CARTESIAN_POINT ( 'NONE',  ( 10.81189881249999907, 6.242252689847868297, -56.90625000204837391 ) ) ;
#1826 = CARTESIAN_POINT ( 'NONE',  ( -7.870332919771452218, 7.330147429241407053, -99.99999999999998579 ) ) ;
#1827 = CARTESIAN_POINT ( 'NONE',  ( -5.405949406249996869, 9.363379034771805109, -168.8437500020484094 ) ) ;
#1828 = CARTESIAN_POINT ( 'NONE',  ( 7.644554776091147741E-16, 12.48450537969573659, -110.6562500020483952 ) ) ;
#1829 = CARTESIAN_POINT ( 'NONE',  ( 5.405949406249992428, -9.363379034771808662, -156.2812500020484094 ) ) ;
#1830 = CARTESIAN_POINT ( 'NONE',  ( 5.000000000000000000, 8.660254037844385522, -15.62500000409675138 ) ) ;
#1831 = CARTESIAN_POINT ( 'NONE',  ( 5.405949406249999534, 9.363379034771803333, -46.28125000204838813 ) ) ;
#1832 = CARTESIAN_POINT ( 'NONE',  ( -4.999999999999996447, 8.660254037844387298, -132.3750000040967905 ) ) ;
#1833 = CARTESIAN_POINT ( 'NONE',  ( 4.999999999999992006, -8.660254037844389075, -101.2499999999999858 ) ) ;
#1834 =( BOUNDED_CURVE ( )  B_SPLINE_CURVE ( 2, ( #17768, #11077, #4194, #40015, #10445, #23637, #33560 ),
 .UNSPECIFIED., .F., .F. ) 
 B_SPLINE_CURVE_WITH_KNOTS ( ( 3, 2, 2, 3 ),
 ( 0.5037313432835821558, 0.5049751243781095411, 0.5062189054726369264, 0.5074626865671643117 ),
 .UNSPECIFIED. ) 
 CURVE ( )  GEOMETRIC_REPRESENTATION_ITEM ( )  RATIONAL_B_SPLINE_CURVE ( ( 0.9999999999999880096, 0.8660254037844506980, 1.000000000000000000, 0.8660254037844387076, 1.000000000000000000, 0.8660254037844267172, 1.000000000000011990 ) ) 
 REPRESENTATION_ITEM ( '' )  );
#1835 = EDGE_CURVE ( 'NONE', #1650, #37987, #25230, .T. ) ;
#1836 = ORIENTED_EDGE ( 'NONE', *, *, #19334, .F. ) ;
#1837 = CARTESIAN_POINT ( 'NONE',  ( 5.405949406249999534, 9.363379034771803333, -125.7812500020483668 ) ) ;
#1838 = CARTESIAN_POINT ( 'NONE',  ( 10.00000000000000000, 5.773502691896255534, -149.2500000040968189 ) ) ;
#1839 = CARTESIAN_POINT ( 'NONE',  ( -2.121150477449813534E-15, -11.54700538379251284, -167.3750000000000000 ) ) ;
#1840 = CARTESIAN_POINT ( 'NONE',  ( 10.81189881249999551, -6.242252689847874514, -178.6562500020484094 ) ) ;
#1841 = VERTEX_POINT ( 'NONE', #25739 ) ;
#1842 = CARTESIAN_POINT ( 'NONE',  ( 5.405949406249992428, -9.363379034771808662, -175.5937500020484094 ) ) ;
#1843 = CARTESIAN_POINT ( 'NONE',  ( -2.121150477449813534E-15, -11.54700538379251284, -61.25000000409677625 ) ) ;
#1844 = CARTESIAN_POINT ( 'NONE',  ( -10.00000000000000000, -5.773502691896252870, -166.1249999999999716 ) ) ;
#1845 = CARTESIAN_POINT ( 'NONE',  ( 9.999999999999742428, 5.773502691896404748, -130.8749999999999716 ) ) ;
#1846 = CARTESIAN_POINT ( 'NONE',  ( -10.81189881249999729, 1.324075727343319199E-15, -69.78125000204838102 ) ) ;
#1847 = CIRCLE ( 'NONE', #5285, 5.500000000000003553 ) ;
#1848 = CARTESIAN_POINT ( 'NONE',  ( 9.999999999999998224, 0.000000000000000000, -44.37500000409677625 ) ) ;
#1849 = CARTESIAN_POINT ( 'NONE',  ( 10.81189881249999907, 6.242252689847868297, -5.718750002048356151 ) ) ;
#1850 = CARTESIAN_POINT ( 'NONE',  ( -10.00000000000051337, 5.773502691895962435, -147.2500000040967905 ) ) ;
#1851 = CARTESIAN_POINT ( 'NONE',  ( -5.405949406250003975, -9.363379034771801557, -165.5312500020484094 ) ) ;
#1852 = CARTESIAN_POINT ( 'NONE',  ( 9.999999999997939426, 5.773502691897446581, -7.874999999999921840 ) ) ;
#1853 = FACE_OUTER_BOUND ( 'NONE', #36551, .T. ) ;
#1855 = ORIENTED_EDGE ( 'NONE', *, *, #6433, .T. ) ;
#1854 = EDGE_CURVE ( 'NONE', #24638, #18719, #14148, .T. ) ;
#1856 = CARTESIAN_POINT ( 'NONE',  ( 7.070501591499376803E-16, 11.54700538379251284, -84.50000000409677625 ) ) ;
#1857 = CARTESIAN_POINT ( 'NONE',  ( -2.121150477449813534E-15, -11.54700538379251284, -153.8749999999999716 ) ) ;
#1858 = CARTESIAN_POINT ( 'NONE',  ( -9.999999999999998224, 1.224646799147353059E-15, -163.6250000040967905 ) ) ;
#1860 = ORIENTED_EDGE ( 'NONE', *, *, #9956, .F. ) ;
#1859 = CARTESIAN_POINT ( 'NONE',  ( 5.405949406249999534, 9.363379034771803333, -79.28125000204838102 ) ) ;
#1861 = CARTESIAN_POINT ( 'NONE',  ( 0.000000000000000000, 0.000000000000000000, 0.000000000000000000 ) ) ;
#1863 = ORIENTED_EDGE ( 'NONE', *, *, #34252, .F. ) ;
#1862 = CARTESIAN_POINT ( 'NONE',  ( 0.000000000000000000, 0.000000000000000000, -99.99999999999998579 ) ) ;
#1864 = ORIENTED_EDGE ( 'NONE', *, *, #33908, .F. ) ;
#1865 = CARTESIAN_POINT ( 'NONE',  ( -10.81189881249999729, 1.324075727343319199E-15, -38.09375000204837391 ) ) ;
#1866 = DIRECTION ( 'NONE',  ( -1.000000000000000000, 0.000000000000000000, 0.000000000000000000 ) ) ;
#1867 = CARTESIAN_POINT ( 'NONE',  ( 5.405949406249992428, -9.363379034771808662, -6.281250002048377468 ) ) ;
#1869 = ORIENTED_EDGE ( 'NONE', *, *, #25929, .F. ) ;
#1868 = CARTESIAN_POINT ( 'NONE',  ( -10.81189881249999907, -6.242252689847864744, -60.46875000204838102 ) ) ;
#1870 = CARTESIAN_POINT ( 'NONE',  ( 5.000000000000000000, 8.660254037844385522, -112.7499999999999858 ) ) ;
#1871 = CARTESIAN_POINT ( 'NONE',  ( -10.00000000000000000, -5.773502691896251982, -37.12499999999995737 ) ) ;
#1872 = CARTESIAN_POINT ( 'NONE',  ( 5.405949406249999534, 9.363379034771803333, -197.5937500020484094 ) ) ;
#1873 = CARTESIAN_POINT ( 'NONE',  ( 7.644554776091147741E-16, 12.48450537969573659, -180.9687500020484094 ) ) ;
#1874 = CARTESIAN_POINT ( 'NONE',  ( -10.81189881249999729, 1.324075727343319199E-15, -167.0937500020484094 ) ) ;
#1875 = DIRECTION ( 'NONE',  ( -0.000000000000000000, -0.000000000000000000, -1.000000000000000000 ) ) ;
#1876 = CARTESIAN_POINT ( 'NONE',  ( 10.00000000000000000, 5.773502691896255534, -199.8750000000000284 ) ) ;
#1877 = CARTESIAN_POINT ( 'NONE',  ( -9.999999999999998224, 1.224646799147353059E-15, -197.7500000000000000 ) ) ;
#1878 = CARTESIAN_POINT ( 'NONE',  ( 10.81189881249999729, 0.000000000000000000, -113.8437500020483810 ) ) ;
#1879 = FACE_OUTER_BOUND ( 'NONE', #40938, .T. ) ;
#1880 = CARTESIAN_POINT ( 'NONE',  ( -5.405949406250003975, -9.363379034771801557, -83.03125000204838102 ) ) ;
#1881 = CARTESIAN_POINT ( 'NONE',  ( -2.293366432827344421E-15, -12.48450537969573659, -93.21875000204838102 ) ) ;
#1882 = CARTESIAN_POINT ( 'NONE',  ( -2.293366432827344421E-15, -12.48450537969573659, -66.40625000204838102 ) ) ;
#1883 = CARTESIAN_POINT ( 'NONE',  ( -9.999999999999998224, 1.224646799147353059E-15, -153.1250000040967905 ) ) ;
#1884 = CARTESIAN_POINT ( 'NONE',  ( 7.070501591499377789E-16, 11.54700538379251284, -120.1249999999999858 ) ) ;
#1885 = CARTESIAN_POINT ( 'NONE',  ( -2.293366432827344421E-15, -12.48450537969573659, -147.4062500020483810 ) ) ;
#1886 = CARTESIAN_POINT ( 'NONE',  ( 5.405949406249999534, 9.363379034771803333, -164.7812500020484094 ) ) ;
#1887 = CARTESIAN_POINT ( 'NONE',  ( -9.999999999999479527, -5.773502691896549521, -40.12499999999995026 ) ) ;
#1888 = CARTESIAN_POINT ( 'NONE',  ( 9.999999999999872102, 5.773502691896329253, -159.7500000040967905 ) ) ;
#1889 = CARTESIAN_POINT ( 'NONE',  ( 7.644554776091147741E-16, 12.48450537969573659, -95.46875000204839523 ) ) ;
#1890 = ORIENTED_EDGE ( 'NONE', *, *, #2901, .T. ) ;
#1891 = CARTESIAN_POINT ( 'NONE',  ( 9.999999999999998224, 0.000000000000000000, -69.49999999999997158 ) ) ;
#1892 = CARTESIAN_POINT ( 'NONE',  ( -10.81189881249999907, -6.242252689847864744, -196.9687500020484379 ) ) ;
#1893 = CARTESIAN_POINT ( 'NONE',  ( -5.000000000000003553, -8.660254037844383745, -85.37500000409677625 ) ) ;
#1894 = DIRECTION ( 'NONE',  ( -0.000000000000000000, -0.000000000000000000, -1.000000000000000000 ) ) ;
#1895 = CARTESIAN_POINT ( 'NONE',  ( -10.81189881249999729, 1.324075727343319199E-15, -89.28125000204838102 ) ) ;
#1896 = CARTESIAN_POINT ( 'NONE',  ( 10.81189881249999729, 6.242252689847867408, -76.40625000204836681 ) ) ;
#1897 = CARTESIAN_POINT ( 'NONE',  ( -4.999999999999996447, 8.660254037844387298, -64.87500000409676204 ) ) ;
#1898 = CYLINDRICAL_SURFACE ( 'NONE', #24332, 9.999999999999998224 ) ;
#1899 = CARTESIAN_POINT ( 'NONE',  ( -2.293366432827344421E-15, -12.48450537969573659, -24.21875000204837036 ) ) ;
#1900 = ORIENTED_EDGE ( 'NONE', *, *, #36380, .T. ) ;
#1901 = CARTESIAN_POINT ( 'NONE',  ( -2.293366432827344421E-15, -12.48450537969573659, -198.4062500020484094 ) ) ;
#1902 = CARTESIAN_POINT ( 'NONE',  ( -10.81189881249999729, 6.242252689847871849, -23.40625000204837747 ) ) ;
#1903 = CARTESIAN_POINT ( 'NONE',  ( -10.81189881249999729, 6.242252689847871849, -3.718750002048365477 ) ) ;
#1904 = CARTESIAN_POINT ( 'NONE',  ( -5.000000000000003553, -8.660254037844383745, -64.37500000409676204 ) ) ;
#1905 = CARTESIAN_POINT ( 'NONE',  ( 5.405949406249992428, -9.363379034771808662, -139.5937500020483810 ) ) ;
#1906 = CARTESIAN_POINT ( 'NONE',  ( 10.00000000000076916, -5.773502691895816774, -107.5000000040967620 ) ) ;
#1907 = CARTESIAN_POINT ( 'NONE',  ( 9.999999999999998224, 0.000000000000000000, -200.0000000000000000 ) ) ;
#1908 = CARTESIAN_POINT ( 'NONE',  ( -5.405949406249996869, 9.363379034771805109, -128.5312500020484094 ) ) ;
#1909 = CARTESIAN_POINT ( 'NONE',  ( 10.00000000000000000, 5.773502691896255534, -181.8750000000000000 ) ) ;
#1910 = CARTESIAN_POINT ( 'NONE',  ( 5.000000000000000000, 8.660254037844385522, -176.1250000040968189 ) ) ;
#1912 = ORIENTED_EDGE ( 'NONE', *, *, #2506, .T. ) ;
#1911 = CARTESIAN_POINT ( 'NONE',  ( -10.81189881249999729, 1.324075727343319199E-15, -98.28125000204839523 ) ) ;
#1913 = LINE ( 'NONE', #7523, #37956 ) ;
#1914 = EDGE_CURVE ( 'NONE', #40028, #30244, #7708, .T. ) ;
#1915 = ORIENTED_EDGE ( 'NONE', *, *, #23824, .T. ) ;
#1916 = EDGE_CURVE ( 'NONE', #32801, #14436, #26787, .T. ) ;
#1917 = VERTEX_POINT ( 'NONE', #17050 ) ;
#1918 = CARTESIAN_POINT ( 'NONE',  ( 10.81189881249999551, -6.242252689847874514, -37.65625000204836681 ) ) ;
#1919 = PERSON_AND_ORGANIZATION_ROLE ( 'creator' ) ;
#1920 = CARTESIAN_POINT ( 'NONE',  ( 10.81189881249999729, 0.000000000000000000, -83.84375000204836681 ) ) ;
#1921 = CARTESIAN_POINT ( 'NONE',  ( 5.000000000000000000, 8.660254037844385522, -128.1250000040967620 ) ) ;
#1922 = AXIS2_PLACEMENT_3D ( 'NONE', #7273, #40268, #30377 ) ;
#1923 = DIRECTION ( 'NONE',  ( 1.000000000000000000, 0.000000000000000000, 0.000000000000000000 ) ) ;
#1924 =( BOUNDED_CURVE ( )  B_SPLINE_CURVE ( 2, ( #23390, #306, #9366, #16881, #19709, #35915, #13425 ),
 .UNSPECIFIED., .F., .F. ) 
 B_SPLINE_CURVE_WITH_KNOTS ( ( 3, 2, 2, 3 ),
 ( 0.6268656716417911889, 0.6281094527363185742, 0.6293532338308458485, 0.6305970149253732338 ),
 .UNSPECIFIED. ) 
 CURVE ( )  GEOMETRIC_REPRESENTATION_ITEM ( )  RATIONAL_B_SPLINE_CURVE ( ( 0.9999999999999880096, 0.8660254037844506980, 1.000000000000000000, 0.8660254037844387076, 1.000000000000000000, 0.8660254037844267172, 1.000000000000011990 ) ) 
 REPRESENTATION_ITEM ( '' )  );
#1925 = CARTESIAN_POINT ( 'NONE',  ( 4.999999999999992006, -8.660254037844389075, -32.62500000409676915 ) ) ;
#1926 = CARTESIAN_POINT ( 'NONE',  ( 7.644554776091147741E-16, 12.48450537969573659, -163.1562500020484094 ) ) ;
#1927 = CARTESIAN_POINT ( 'NONE',  ( 9.999999999999998224, 0.000000000000000000, -171.8750000040968189 ) ) ;
#1928 = CARTESIAN_POINT ( 'NONE',  ( -10.81189881249999729, -6.242252689847864744, -115.9687500020483810 ) ) ;
#1929 = CARTESIAN_POINT ( 'NONE',  ( -10.81189881249999907, -6.242252689847864744, -84.46875000204836681 ) ) ;
#1930 = CARTESIAN_POINT ( 'NONE',  ( 9.999999999999998224, 0.000000000000000000, -101.3750000040967905 ) ) ;
#1931 = CARTESIAN_POINT ( 'NONE',  ( 7.644554776091147741E-16, 12.48450537969573659, -197.4687500020484094 ) ) ;
#1932 = CARTESIAN_POINT ( 'NONE',  ( -10.81189881249999729, 1.324075727343319199E-15, -92.28125000204838102 ) ) ;
#1933 = CARTESIAN_POINT ( 'NONE',  ( 4.999999999999992006, -8.660254037844389075, -175.1250000040968189 ) ) ;
#1934 = CARTESIAN_POINT ( 'NONE',  ( -10.81189881249999729, 1.324075727343319199E-15, -167.2812500020484094 ) ) ;
#1935 = CARTESIAN_POINT ( 'NONE',  ( 5.000000000000000000, 8.660254037844385522, -102.6250000040967905 ) ) ;
#1936 = CARTESIAN_POINT ( 'NONE',  ( 5.405949406249992428, -9.363379034771808662, -175.7812500020484094 ) ) ;
#1937 = CARTESIAN_POINT ( 'NONE',  ( 5.405949406249992428, -9.363379034771808662, -189.2812500020484094 ) ) ;
#1938 = CARTESIAN_POINT ( 'NONE',  ( 10.81189881249999729, 0.000000000000000000, -43.34375000204837391 ) ) ;
#1939 = CARTESIAN_POINT ( 'NONE',  ( 4.999999999999992006, -8.660254037844389075, -166.1250000040967905 ) ) ;
#1940 = CARTESIAN_POINT ( 'NONE',  ( 5.405949406249992428, -9.363379034771808662, -6.281250002048377468 ) ) ;
#1941 = CARTESIAN_POINT ( 'NONE',  ( 10.81189881249999907, 6.242252689847868297, -16.21875000204836326 ) ) ;
#1942 = CARTESIAN_POINT ( 'NONE',  ( -9.999999999999998224, 1.224646799147353059E-15, -53.74999999999996447 ) ) ;
#1943 = CARTESIAN_POINT ( 'NONE',  ( 10.81189881249999551, -6.242252689847874514, -119.9687500020483952 ) ) ;
#1944 = CARTESIAN_POINT ( 'NONE',  ( 7.070501591499377789E-16, 11.54700538379251284, -99.12500000000000000 ) ) ;
#1945 = CARTESIAN_POINT ( 'NONE',  ( -10.81189881249999729, 6.242252689847871849, -20.40625000204837391 ) ) ;
#1946 = CARTESIAN_POINT ( 'NONE',  ( -9.999999999999998224, 5.773502691896259087, -102.2500000040967763 ) ) ;
#1947 = CARTESIAN_POINT ( 'NONE',  ( -4.999999999999996447, 8.660254037844387298, -82.49999999999998579 ) ) ;
#1948 = CARTESIAN_POINT ( 'NONE',  ( 9.999999999999998224, 0.000000000000000000, -51.49999999999996447 ) ) ;
#1949 = CARTESIAN_POINT ( 'NONE',  ( 10.81189881249999729, 0.000000000000000000, -118.5312500020483952 ) ) ;
#1950 = CARTESIAN_POINT ( 'NONE',  ( 5.405949406249992428, -9.363379034771808662, -99.28125000204839523 ) ) ;
#1951 = ORIENTED_EDGE ( 'NONE', *, *, #16415, .F. ) ;
#1952 = CARTESIAN_POINT ( 'NONE',  ( 10.00000000000000000, 5.773502691896255534, -89.25000000409677625 ) ) ;
#1953 = CARTESIAN_POINT ( 'NONE',  ( -9.999999999999998224, 1.224646799147353059E-15, -55.24999999999996447 ) ) ;
#1954 = CARTESIAN_POINT ( 'NONE',  ( -5.405949406249996869, 9.363379034771805109, -160.0312500020484094 ) ) ;
#1955 = CARTESIAN_POINT ( 'NONE',  ( -10.81189881249999907, -6.242252689847864744, -51.46875000204837391 ) ) ;
#1956 = ORIENTED_EDGE ( 'NONE', *, *, #19624, .F. ) ;
#1957 = CARTESIAN_POINT ( 'NONE',  ( 5.000000000000000000, 8.660254037844385522, -24.24999999999996447 ) ) ;
#1958 = CARTESIAN_POINT ( 'NONE',  ( -5.405949406250003975, -9.363379034771801557, -26.03125000204836681 ) ) ;
#1959 = CARTESIAN_POINT ( 'NONE',  ( -2.121150477449813534E-15, -11.54700538379251284, -161.3750000000000000 ) ) ;
#1960 = VECTOR ( 'NONE', #12558, 1000.000000000000000 ) ;
#1961 = CARTESIAN_POINT ( 'NONE',  ( -9.999999999999998224, 1.224646799147353059E-15, -22.62500000409675849 ) ) ;
#1962 = CARTESIAN_POINT ( 'NONE',  ( -9.999999999999479527, -5.773502691896549521, -81.00000000409674783 ) ) ;
#1963 = CARTESIAN_POINT ( 'NONE',  ( -2.293366432827344421E-15, -12.48450537969573659, -132.4062500020483810 ) ) ;
#1964 = FACE_OUTER_BOUND ( 'NONE', #28728, .T. ) ;
#1965 = EDGE_CURVE ( 'NONE', #41954, #2320, #10794, .T. ) ;
#1966 = CARTESIAN_POINT ( 'NONE',  ( -9.999999999999998224, 0.000000000000000000, -99.99999999999998579 ) ) ;
#1967 = VERTEX_POINT ( 'NONE', #17262 ) ;
#1968 = EDGE_CURVE ( 'NONE', #25274, #27810, #13476, .T. ) ;
#1969 =( BOUNDED_CURVE ( )  B_SPLINE_CURVE ( 2, ( #14952, #28150, #24707, #41284, #11723, #4620, #30960 ),
 .UNSPECIFIED., .F., .F. ) 
 B_SPLINE_CURVE_WITH_KNOTS ( ( 3, 2, 2, 3 ),
 ( 0.3171641791044778058, 0.3184079601990050801, 0.3196517412935324653, 0.3208955223880597396 ),
 .UNSPECIFIED. ) 
 CURVE ( )  GEOMETRIC_REPRESENTATION_ITEM ( )  RATIONAL_B_SPLINE_CURVE ( ( 0.9999999999999820144, 0.8660254037844566932, 1.000000000000000000, 0.8660254037844387076, 1.000000000000000000, 0.8660254037844327124, 1.000000000000005995 ) ) 
 REPRESENTATION_ITEM ( '' )  );
#1970 = CARTESIAN_POINT ( 'NONE',  ( -10.81189881249999729, 6.242252689847871849, -59.40625000204838813 ) ) ;
#1971 = DATE_AND_TIME ( #30522, #31794 ) ;
#1972 = EDGE_CURVE ( 'NONE', #24961, #41628, #30250, .T. ) ;
#1974 = ORIENTED_EDGE ( 'NONE', *, *, #5249, .F. ) ;
#1973 = EDGE_LOOP ( 'NONE', ( #218, #36575, #20996, #11706 ) ) ;
#1975 = CARTESIAN_POINT ( 'NONE',  ( -2.121150477449813534E-15, -11.54700538379251284, -46.25000000409676915 ) ) ;
#1976 = CC_DESIGN_PERSON_AND_ORGANIZATION_ASSIGNMENT ( #5626, #35829, ( #22864 ) ) ;
#1977 = CARTESIAN_POINT ( 'NONE',  ( -9.999999999999998224, 1.224646799147353059E-15, -200.0000000000000000 ) ) ;
#1978 = CARTESIAN_POINT ( 'NONE',  ( -2.293366432827344421E-15, -12.48450537969573659, -154.7187500020483810 ) ) ;
#1979 =( BOUNDED_CURVE ( )  B_SPLINE_CURVE ( 2, ( #2008, #18167, #34595, #1359, #27898, #37606, #31361 ),
 .UNSPECIFIED., .F., .F. ) 
 B_SPLINE_CURVE_WITH_KNOTS ( ( 3, 2, 2, 3 ),
 ( 0.2723880597014926574, 0.2736318407960199872, 0.2748756218905473725, 0.2761194029850747578 ),
 .UNSPECIFIED. ) 
 CURVE ( )  GEOMETRIC_REPRESENTATION_ITEM ( )  RATIONAL_B_SPLINE_CURVE ( ( 0.9999999999999880096, 0.8660254037844506980, 1.000000000000000000, 0.8660254037844387076, 1.000000000000000000, 0.8660254037844267172, 1.000000000000011990 ) ) 
 REPRESENTATION_ITEM ( '' )  );
#1980 = CARTESIAN_POINT ( 'NONE',  ( -10.81189881249999907, -6.242252689847864744, -186.6562500020484094 ) ) ;
#1981 = CARTESIAN_POINT ( 'NONE',  ( -5.405949406250003975, -9.363379034771801557, -10.84375000204834727 ) ) ;
#1982 = CARTESIAN_POINT ( 'NONE',  ( -10.81189881249999729, -6.242252689847864744, -138.4687500020483810 ) ) ;
#1983 = CARTESIAN_POINT ( 'NONE',  ( -5.405949406249996869, 9.363379034771805109, -97.03125000204839523 ) ) ;
#1984 = CARTESIAN_POINT ( 'NONE',  ( 7.644554776091147741E-16, 12.48450537969573659, -111.9687500020483952 ) ) ;
#1985 = CARTESIAN_POINT ( 'NONE',  ( 9.999999999999998224, 0.000000000000000000, -180.8750000040967905 ) ) ;
#1986 = CARTESIAN_POINT ( 'NONE',  ( -5.405949406250003975, -9.363379034771801557, -120.5312500020483952 ) ) ;
#1987 = CARTESIAN_POINT ( 'NONE',  ( 5.405949406249999534, 9.363379034771803333, -1.093750002048365921 ) ) ;
#1988 = CARTESIAN_POINT ( 'NONE',  ( -10.81189881249999729, 6.242252689847871849, -122.2187500020483810 ) ) ;
#1989 = CARTESIAN_POINT ( 'NONE',  ( -5.405949406250003975, -9.363379034771801557, -195.5312500020484094 ) ) ;
#1990 = CARTESIAN_POINT ( 'NONE',  ( 0.000000000000000000, 0.000000000000000000, -200.0000000000000000 ) ) ;
#1991 = CARTESIAN_POINT ( 'NONE',  ( 9.999999999999998224, 0.000000000000000000, -149.0000000000000000 ) ) ;
#1992 = CARTESIAN_POINT ( 'NONE',  ( 10.00000000000000000, 5.773502691896255534, -9.374999999999966249 ) ) ;
#1993 = EDGE_CURVE ( 'NONE', #5068, #24022, #30032, .T. ) ;
#1994 = CARTESIAN_POINT ( 'NONE',  ( 10.81189881249999729, 6.242252689847867408, -73.21875000204836681 ) ) ;
#1995 = CARTESIAN_POINT ( 'NONE',  ( -5.405949406249996869, 9.363379034771805109, -56.34375000204835970 ) ) ;
#1996 = CARTESIAN_POINT ( 'NONE',  ( 4.999999999999992006, -8.660254037844389075, -190.1250000040967905 ) ) ;
#1997 = CARTESIAN_POINT ( 'NONE',  ( 5.405949406249992428, -9.363379034771808662, -22.78125000204836326 ) ) ;
#1998 = CARTESIAN_POINT ( 'NONE',  ( -10.81189881249999729, 1.324075727343319199E-15, -39.59375000204837391 ) ) ;
#1999 = CARTESIAN_POINT ( 'NONE',  ( 5.405949406249999534, 9.363379034771803333, -146.5937500020483810 ) ) ;
#2000 = CARTESIAN_POINT ( 'NONE',  ( -4.999999999999996447, 8.660254037844387298, -124.5000000000000000 ) ) ;
#2001 = FACE_OUTER_BOUND ( 'NONE', #8783, .T. ) ;
#2002 = CARTESIAN_POINT ( 'NONE',  ( -2.121150477449813534E-15, -11.54700538379251284, -74.37499999999995737 ) ) ;
#2003 = CARTESIAN_POINT ( 'NONE',  ( -10.81189881249999729, 6.242252689847871849, -138.9062500020484094 ) ) ;
#2004 = CARTESIAN_POINT ( 'NONE',  ( 10.81189881249999729, 0.000000000000000000, -9.031250002048352599 ) ) ;
#2005 = ORIENTED_EDGE ( 'NONE', *, *, #26483, .T. ) ;
#2006 = CARTESIAN_POINT ( 'NONE',  ( -5.405949406249996869, 9.363379034771805109, -103.0312500020483952 ) ) ;
#2007 = CARTESIAN_POINT ( 'NONE',  ( 4.999999999999992006, -8.660254037844389075, -113.6250000040967763 ) ) ;
#2008 = CARTESIAN_POINT ( 'NONE',  ( -9.999999999999998224, 1.224646799147353059E-15, -144.1250000040967905 ) ) ;
#2009 = CARTESIAN_POINT ( 'NONE',  ( -2.293366432827344421E-15, -12.48450537969573659, -70.71875000204838102 ) ) ;
#2010 = CARTESIAN_POINT ( 'NONE',  ( 5.000000000000000000, 8.660254037844385522, -29.12500000409676204 ) ) ;
#2011 = LINE ( 'NONE', #18170, #26980 ) ;
#2012 = CARTESIAN_POINT ( 'NONE',  ( 10.81189881249999551, -6.242252689847874514, -46.65625000204836681 ) ) ;
#2013 = CARTESIAN_POINT ( 'NONE',  ( 9.999999999999998224, 0.000000000000000000, -149.0000000000000000 ) ) ;
#2014 = CARTESIAN_POINT ( 'NONE',  ( -10.81189881249999729, 6.242252689847871849, -143.4062500020484094 ) ) ;
#2015 = CARTESIAN_POINT ( 'NONE',  ( 5.405949406249992428, -9.363379034771808662, -127.5937500020483668 ) ) ;
#2016 = CARTESIAN_POINT ( 'NONE',  ( -9.999999999999998224, 1.224646799147353059E-15, -14.74999999999995737 ) ) ;
#2017 = AXIS2_PLACEMENT_3D ( 'NONE', #6538, #22950, #36317 ) ;
#2018 = DIRECTION ( 'NONE',  ( -0.000000000000000000, -0.000000000000000000, 1.000000000000000000 ) ) ;
#2019 = VERTEX_POINT ( 'NONE', #31473 ) ;
#2020 = AXIS2_PLACEMENT_3D ( 'NONE', #5758, #34905, #15016 ) ;
#2021 = ORIENTED_EDGE ( 'NONE', *, *, #14598, .T. ) ;
#2022 = EDGE_LOOP ( 'NONE', ( #31999, #38521, #40889, #7106 ) ) ;
#2023 = CARTESIAN_POINT ( 'NONE',  ( -5.000000000000003553, -8.660254037844383745, -176.8750000040967905 ) ) ;
#2024 = CARTESIAN_POINT ( 'NONE',  ( -5.405949406250003975, -9.363379034771801557, -183.3437500020483810 ) ) ;
#2026 = ADVANCED_FACE ( 'NONE', ( #8164 ), #10577, .F. ) ;
#2025 = CARTESIAN_POINT ( 'NONE',  ( 10.81189881249999907, 6.242252689847868297, -32.71875000204834549 ) ) ;
#2027 = CARTESIAN_POINT ( 'NONE',  ( 9.999999999999998224, 0.000000000000000000, -90.49999999999998579 ) ) ;
#2028 = CARTESIAN_POINT ( 'NONE',  ( -5.405949406250003975, -9.363379034771801557, -172.8437500020484094 ) ) ;
#2029 = CARTESIAN_POINT ( 'NONE',  ( 10.81189881249999729, 0.000000000000000000, -149.8437500020483810 ) ) ;
#2030 = CARTESIAN_POINT ( 'NONE',  ( 0.000000000000000000, 0.000000000000000000, -200.0000000000000000 ) ) ;
#2031 = CARTESIAN_POINT ( 'NONE',  ( -5.405949406249996869, 9.363379034771805109, -137.3437500020484094 ) ) ;
#2032 = CARTESIAN_POINT ( 'NONE',  ( 7.644554776091147741E-16, 12.48450537969573659, -142.1562500020483810 ) ) ;
#2033 = CARTESIAN_POINT ( 'NONE',  ( -10.81189881249999729, -6.242252689847864744, -144.4687500020484094 ) ) ;
#2034 = CARTESIAN_POINT ( 'NONE',  ( 0.000000000000000000, 0.000000000000000000, -200.0000000000000000 ) ) ;
#2035 = CARTESIAN_POINT ( 'NONE',  ( 5.000000000000000000, 8.660254037844385522, -70.74999999999998579 ) ) ;
#2036 = CARTESIAN_POINT ( 'NONE',  ( 9.999999999999998224, 0.000000000000000000, -174.5000000000000284 ) ) ;
#2037 = CARTESIAN_POINT ( 'NONE',  ( -5.405949406249996869, 9.363379034771805109, -80.34375000204838102 ) ) ;
#2038 = CARTESIAN_POINT ( 'NONE',  ( 9.999999999999998224, 0.000000000000000000, -112.9999999999999858 ) ) ;
#2039 = CARTESIAN_POINT ( 'NONE',  ( 5.405949406249992428, -9.363379034771808662, -60.28125000204836681 ) ) ;
#2040 = CYLINDRICAL_SURFACE ( 'NONE', #21999, 9.999999999999998224 ) ;
#2041 = CARTESIAN_POINT ( 'NONE',  ( 10.81189881249999551, -6.242252689847874514, -166.4687500020484094 ) ) ;
#2042 = CARTESIAN_POINT ( 'NONE',  ( 5.405949406249992428, -9.363379034771808662, -115.7812500020483952 ) ) ;
#2043 = CARTESIAN_POINT ( 'NONE',  ( -10.81189881249999729, -6.242252689847864744, -144.6562500020484094 ) ) ;
#2044 =( BOUNDED_CURVE ( )  B_SPLINE_CURVE ( 2, ( #32659, #3088, #16428, #16216, #29627, #70, #13194 ),
 .UNSPECIFIED., .F., .F. ) 
 B_SPLINE_CURVE_WITH_KNOTS ( ( 3, 2, 2, 3 ),
 ( 0.4813432835820896649, 0.4825870646766170502, 0.4838308457711443800, 0.4850746268656717652 ),
 .UNSPECIFIED. ) 
 CURVE ( )  GEOMETRIC_REPRESENTATION_ITEM ( )  RATIONAL_B_SPLINE_CURVE ( ( 0.9999999999999880096, 0.8660254037844506980, 1.000000000000000000, 0.8660254037844387076, 1.000000000000000000, 0.8660254037844267172, 1.000000000000011990 ) ) 
 REPRESENTATION_ITEM ( '' )  );
#2045 = DIRECTION ( 'NONE',  ( -1.000000000000000000, 0.000000000000000000, 0.000000000000000000 ) ) ;
#2046 = CARTESIAN_POINT ( 'NONE',  ( -10.81189881249999729, 1.324075727343319199E-15, -45.78125000204838813 ) ) ;
#2047 = CARTESIAN_POINT ( 'NONE',  ( -5.000000000000003553, -8.660254037844383745, -119.8750000040967905 ) ) ;
#2048 = CARTESIAN_POINT ( 'NONE',  ( 10.00000000000000000, 5.773502691896255534, -97.87499999999998579 ) ) ;
#2049 = EDGE_LOOP ( 'NONE', ( #3538, #34072, #39048, #41696 ) ) ;
#2050 = CARTESIAN_POINT ( 'NONE',  ( -5.405949406249996869, 9.363379034771805109, -124.0312500020483952 ) ) ;
#2051 = CARTESIAN_POINT ( 'NONE',  ( -2.121150477449813534E-15, -11.54700538379251284, -136.2500000040967620 ) ) ;
#2052 = CARTESIAN_POINT ( 'NONE',  ( 5.000000000000000000, 8.660254037844385522, -68.12500000409677625 ) ) ;
#2053 = AXIS2_PLACEMENT_3D ( 'NONE', #3803, #16942, #30139 ) ;
#2054 = CARTESIAN_POINT ( 'NONE',  ( -5.405949406249996869, 9.363379034771805109, -179.5312500020483810 ) ) ;
#2055 = EDGE_LOOP ( 'NONE', ( #1805, #11917, #19083, #26416 ) ) ;
#2056 = CARTESIAN_POINT ( 'NONE',  ( 10.81189881249999551, -6.242252689847874514, -175.4687500020484094 ) ) ;
#2057 = CARTESIAN_POINT ( 'NONE',  ( 9.999999999999996447, -5.773502691896262640, -47.50000000409677625 ) ) ;
#2058 = CARTESIAN_POINT ( 'NONE',  ( 10.00000000000102318, -5.773502691895667560, -18.62499999999994671 ) ) ;
#2059 = DIRECTION ( 'NONE',  ( 1.000000000000000000, 0.000000000000000000, 0.000000000000000000 ) ) ;
#2060 = CARTESIAN_POINT ( 'NONE',  ( -10.81189881249999729, 6.242252689847871849, -66.90625000204839523 ) ) ;
#2061 = CARTESIAN_POINT ( 'NONE',  ( -2.121150477449813534E-15, -11.54700538379251284, -43.25000000409676204 ) ) ;
#2062 = AXIS2_PLACEMENT_3D ( 'NONE', #513, #3519, #33313 ) ;
#2063 = CARTESIAN_POINT ( 'NONE',  ( -5.405949406250003975, -9.363379034771801557, -3.343750002048367698 ) ) ;
#2064 = DIRECTION ( 'NONE',  ( -0.000000000000000000, -0.000000000000000000, 1.000000000000000000 ) ) ;
#2065 = CARTESIAN_POINT ( 'NONE',  ( -2.293366432827344421E-15, -12.48450537969573659, -172.9062500020484379 ) ) ;
#2066 = DIRECTION ( 'NONE',  ( 1.000000000000000000, 0.000000000000000000, 0.000000000000000000 ) ) ;
#2067 = CARTESIAN_POINT ( 'NONE',  ( -1.040834085586084257E-14, 139.9999999999999716, 2.499999999999992006 ) ) ;
#2068 = EDGE_LOOP ( 'NONE', ( #40227, #42312 ) ) ;
#2069 = CARTESIAN_POINT ( 'NONE',  ( -9.999999999999998224, 1.224646799147353059E-15, -84.12500000409677625 ) ) ;
#2070 = CARTESIAN_POINT ( 'NONE',  ( -4.999999999999996447, 8.660254037844387298, -123.3750000040967905 ) ) ;
#2071 = CARTESIAN_POINT ( 'NONE',  ( 9.999999999998969713, 5.773502691896851502, -39.75000000409674072 ) ) ;
#2073 = ORIENTED_EDGE ( 'NONE', *, *, #14435, .F. ) ;
#2072 = CARTESIAN_POINT ( 'NONE',  ( -10.81189881249999729, 1.324075727343319199E-15, -78.78125000204838102 ) ) ;
#2075 = EDGE_LOOP ( 'NONE', ( #25697, #38619, #32120, #34720 ) ) ;
#2074 = CARTESIAN_POINT ( 'NONE',  ( 9.999999999999998224, 0.000000000000000000, -119.0000000000000000 ) ) ;
#2076 = ORIENTED_EDGE ( 'NONE', *, *, #15327, .F. ) ;
#2077 = CARTESIAN_POINT ( 'NONE',  ( -2.293366432827344421E-15, -12.48450537969573659, -25.71875000204837391 ) ) ;
#2078 = CARTESIAN_POINT ( 'NONE',  ( 0.000000000000000000, 0.000000000000000000, -200.0000000000000000 ) ) ;
#2079 = CARTESIAN_POINT ( 'NONE',  ( 10.81189881249999551, -6.242252689847874514, -9.156250002048375691 ) ) ;
#2080 = VECTOR ( 'NONE', #35351, 1000.000000000000000 ) ;
#2082 = VERTEX_POINT ( 'NONE', #36919 ) ;
#2081 = CARTESIAN_POINT ( 'NONE',  ( -5.405949406249996869, 9.363379034771805109, -54.84375000204835970 ) ) ;
#2083 = CARTESIAN_POINT ( 'NONE',  ( 18.76388374866293773, 2.499999999999956923, 49.99999999999998579 ) ) ;
#2084 = CARTESIAN_POINT ( 'NONE',  ( -2.121150477449813534E-15, -11.54700538379251284, -35.37499999999996447 ) ) ;
#2085 = CARTESIAN_POINT ( 'NONE',  ( -2.293366432827344421E-15, -12.48450537969573659, -195.2187500020484094 ) ) ;
#2086 = CARTESIAN_POINT ( 'NONE',  ( -10.81189881249999907, -6.242252689847864744, -178.9687500020484094 ) ) ;
#2087 = CARTESIAN_POINT ( 'NONE',  ( 10.81189881249999907, 6.242252689847868297, -157.2187500020483810 ) ) ;
#2088 =( BOUNDED_CURVE ( )  B_SPLINE_CURVE ( 2, ( #35542, #12841, #5972, #35118, #19123, #38548, #32308 ),
 .UNSPECIFIED., .F., .F. ) 
 B_SPLINE_CURVE_WITH_KNOTS ( ( 3, 2, 2, 3 ),
 ( 0.7350746268656719318, 0.7363184079601993171, 0.7375621890547265913, 0.7388059701492539766 ),
 .UNSPECIFIED. ) 
 CURVE ( )  GEOMETRIC_REPRESENTATION_ITEM ( )  RATIONAL_B_SPLINE_CURVE ( ( 0.9999999999999641398, 0.8660254037844745678, 1.000000000000000000, 0.8660254037844387076, 1.000000000000000000, 0.8660254037844148378, 1.000000000000023981 ) ) 
 REPRESENTATION_ITEM ( '' )  );
#2089 = CARTESIAN_POINT ( 'NONE',  ( -10.81189881249999729, 1.324075727343319199E-15, -174.5937500020484094 ) ) ;
#2090 = DIRECTION ( 'NONE',  ( -0.000000000000000000, -0.000000000000000000, 1.000000000000000000 ) ) ;
#2091 = CARTESIAN_POINT ( 'NONE',  ( -9.999999999998456346, -5.773502691897145489, -25.12499999999994316 ) ) ;
#2092 = CARTESIAN_POINT ( 'NONE',  ( 9.999999999999996447, -5.773502691896262640, -194.1250000000000284 ) ) ;
#2093 = CARTESIAN_POINT ( 'NONE',  ( 10.81189881249999551, -6.242252689847874514, -107.9687500020483810 ) ) ;
#2094 = DIRECTION ( 'NONE',  ( -0.000000000000000000, -0.000000000000000000, -1.000000000000000000 ) ) ;
#2095 = CARTESIAN_POINT ( 'NONE',  ( -10.81189881249999907, -6.242252689847864744, -80.15625000204839523 ) ) ;
#2096 = CARTESIAN_POINT ( 'NONE',  ( 7.644554776091147741E-16, 12.48450537969573659, -89.46875000204838102 ) ) ;
#2097 = CARTESIAN_POINT ( 'NONE',  ( 10.81189881249999551, -6.242252689847874514, -67.65625000204838102 ) ) ;
#2098 = CARTESIAN_POINT ( 'NONE',  ( -2.121150477449813534E-15, -11.54700538379251284, -142.2500000040967905 ) ) ;
#2099 = CARTESIAN_POINT ( 'NONE',  ( -2.121150477449813534E-15, -11.54700538379251284, -125.3749999999999858 ) ) ;
#2100 = EDGE_CURVE ( 'NONE', #5246, #9953, #41342, .T. ) ;
#2101 = ORIENTED_EDGE ( 'NONE', *, *, #35354, .T. ) ;
#2102 = CARTESIAN_POINT ( 'NONE',  ( 7.644554776091147741E-16, 12.48450537969573659, -152.6562500020484094 ) ) ;
#2103 = CARTESIAN_POINT ( 'NONE',  ( -5.405949406250003975, -9.363379034771801557, -161.0312500020484094 ) ) ;
#2104 = CARTESIAN_POINT ( 'NONE',  ( 10.00000000000102318, -5.773502691895667560, -39.62499999999992895 ) ) ;
#2105 = CARTESIAN_POINT ( 'NONE',  ( 9.999999999999998224, 0.000000000000000000, -27.87500000409676204 ) ) ;
#2106 = CARTESIAN_POINT ( 'NONE',  ( -5.405949406249996869, 9.363379034771805109, -96.84375000204838102 ) ) ;
#2107 = EDGE_LOOP ( 'NONE', ( #19879, #6050, #26566, #8377 ) ) ;
#2108 = CARTESIAN_POINT ( 'NONE',  ( -9.999999999999998224, 1.224646799147353059E-15, -65.74999999999997158 ) ) ;
#2109 = CARTESIAN_POINT ( 'NONE',  ( -2.293366432827344421E-15, -12.48450537969573659, -193.7187500020484094 ) ) ;
#2110 = CARTESIAN_POINT ( 'NONE',  ( -5.000000000000003553, -8.660254037844383745, -79.37500000409677625 ) ) ;
#2111 = CARTESIAN_POINT ( 'NONE',  ( -4.534034563800342532, -9.223041764796271025, -180.0000000000000000 ) ) ;
#2112 = LINE ( 'NONE', #2325, #18986 ) ;
#2113 = CARTESIAN_POINT ( 'NONE',  ( -5.405949406250003975, -9.363379034771801557, -92.03125000204838102 ) ) ;
#2114 = CARTESIAN_POINT ( 'NONE',  ( 10.81189881249999551, -6.242252689847874514, -79.65625000204838102 ) ) ;
#2115 = CARTESIAN_POINT ( 'NONE',  ( -5.000000000000003553, -8.660254037844383745, -64.37500000409676204 ) ) ;
#2116 = FACE_OUTER_BOUND ( 'NONE', #38256, .T. ) ;
#2117 = CARTESIAN_POINT ( 'NONE',  ( 10.81189881249999729, 0.000000000000000000, -26.84375000204835970 ) ) ;
#2118 = VERTEX_POINT ( 'NONE', #23558 ) ;
#2119 = CARTESIAN_POINT ( 'NONE',  ( 7.644554776091147741E-16, 12.48450537969573659, -196.1562500020484379 ) ) ;
#2120 = CARTESIAN_POINT ( 'NONE',  ( -10.81189881249999729, 6.242252689847871849, -17.40625000204837391 ) ) ;
#2121 = CARTESIAN_POINT ( 'NONE',  ( 5.405949406249999534, 9.363379034771803333, -8.593750002048345493 ) ) ;
#2122 = CARTESIAN_POINT ( 'NONE',  ( 5.000000000000000000, 8.660254037844385522, -160.7500000000000000 ) ) ;
#2123 = CARTESIAN_POINT ( 'NONE',  ( -5.405949406250003975, -9.363379034771801557, -144.3437500020483810 ) ) ;
#2124 = CARTESIAN_POINT ( 'NONE',  ( -9.999999999999998224, 1.224646799147353059E-15, -63.12500000409676204 ) ) ;
#2125 = DIRECTION ( 'NONE',  ( -0.8660254037844382635, -0.5000000000000008882, 0.000000000000000000 ) ) ;
#2126 = CARTESIAN_POINT ( 'NONE',  ( 10.00000000000000000, 5.773502691896255534, -171.3750000000000000 ) ) ;
#2127 = LINE ( 'NONE', #4925, #21375 ) ;
#2129 = ORIENTED_EDGE ( 'NONE', *, *, #22815, .F. ) ;
#2128 = CARTESIAN_POINT ( 'NONE',  ( 7.644554776091147741E-16, 12.48450537969573659, -104.6562500020483810 ) ) ;
#2130 = CARTESIAN_POINT ( 'NONE',  ( 9.999999999999998224, 0.000000000000000000, -179.3750000040967905 ) ) ;
#2131 = ORIENTED_EDGE ( 'NONE', *, *, #9361, .F. ) ;
#2132 = VERTEX_POINT ( 'NONE', #18070 ) ;
#2133 = CARTESIAN_POINT ( 'NONE',  ( -2.293366432827344421E-15, -12.48450537969573659, -33.40625000204835970 ) ) ;
#2134 = PERSON_AND_ORGANIZATION_ROLE ( 'design_owner' ) ;
#2135 = CARTESIAN_POINT ( 'NONE',  ( -5.405949406249996869, 9.363379034771805109, -87.84375000204836681 ) ) ;
#2136 = CARTESIAN_POINT ( 'NONE',  ( -9.999999999999998224, 1.224646799147353059E-15, -173.7500000000000284 ) ) ;
#2137 = CARTESIAN_POINT ( 'NONE',  ( -9.999999999999998224, 1.224646799147353059E-15, -125.7499999999999716 ) ) ;
#2138 = CARTESIAN_POINT ( 'NONE',  ( -10.00000000000051337, 5.773502691895962435, -124.3749999999999858 ) ) ;
#2139 = CARTESIAN_POINT ( 'NONE',  ( -2.293366432827344421E-15, -12.48450537969573659, -166.9062500020483810 ) ) ;
#2140 = CARTESIAN_POINT ( 'NONE',  ( 9.999999999999998224, 0.000000000000000000, -11.37500000409674783 ) ) ;
#2141 = CARTESIAN_POINT ( 'NONE',  ( -5.000000000000003553, -8.660254037844383745, -77.49999999999998579 ) ) ;
#2142 = APPROVAL_PERSON_ORGANIZATION ( #32690, #11985, #19719 ) ;
#2143 = CARTESIAN_POINT ( 'NONE',  ( 5.405949406249992428, -9.363379034771808662, -120.0937500020483952 ) ) ;
#2144 = CARTESIAN_POINT ( 'NONE',  ( -10.81189881249999729, 6.242252689847871849, -84.71875000204836681 ) ) ;
#2145 = CARTESIAN_POINT ( 'NONE',  ( -10.81189881249999729, 1.324075727343319199E-15, -195.5937500020484094 ) ) ;
#2146 = CARTESIAN_POINT ( 'NONE',  ( 10.81189881249999907, 6.242252689847868297, -89.90625000204839523 ) ) ;
#2147 = CARTESIAN_POINT ( 'NONE',  ( 4.999999999999992006, -8.660254037844389075, -178.1250000040968189 ) ) ;
#2148 = CARTESIAN_POINT ( 'NONE',  ( -10.81189881249999729, 6.242252689847871849, -173.4062500020483810 ) ) ;
#2149 = CARTESIAN_POINT ( 'NONE',  ( -9.999999999998969713, -5.773502691896847949, -1.500000004096725403 ) ) ;
#2150 = CARTESIAN_POINT ( 'NONE',  ( 7.644554776091147741E-16, 12.48450537969573659, -176.6562500020484094 ) ) ;
#2151 = CARTESIAN_POINT ( 'NONE',  ( 10.81189881249999907, 6.242252689847868297, -191.9062500020484094 ) ) ;
#2152 = CARTESIAN_POINT ( 'NONE',  ( 5.405949406249992428, -9.363379034771808662, -42.09375000204837391 ) ) ;
#2153 = CARTESIAN_POINT ( 'NONE',  ( 9.999999999999996447, -5.773502691896262640, -166.0000000040967905 ) ) ;
#2154 = CARTESIAN_POINT ( 'NONE',  ( -10.81189881249999729, 6.242252689847871849, -2.406250002048375247 ) ) ;
#2155 = CARTESIAN_POINT ( 'NONE',  ( -5.405949406250003975, -9.363379034771801557, -12.34375000204834905 ) ) ;
#2156 = CARTESIAN_POINT ( 'NONE',  ( 4.999999999999992006, -8.660254037844389075, -193.1250000040967905 ) ) ;
#2157 = CARTESIAN_POINT ( 'NONE',  ( -10.81189881249999729, 6.242252689847871849, -125.2187500020483810 ) ) ;
#2158 = EDGE_CURVE ( 'NONE', #8575, #38512, #33280, .T. ) ;
#2159 = CARTESIAN_POINT ( 'NONE',  ( -9.999999999999998224, 1.224646799147353059E-15, -89.74999999999998579 ) ) ;
#2160 = CARTESIAN_POINT ( 'NONE',  ( 10.81189881249999729, 0.000000000000000000, -21.03125000204836326 ) ) ;
#2161 = CARTESIAN_POINT ( 'NONE',  ( -4.999999999999996447, 8.660254037844387298, -109.8750000040967763 ) ) ;
#2162 = CARTESIAN_POINT ( 'NONE',  ( 4.999999999999992006, -8.660254037844389075, -136.1250000040967620 ) ) ;
#2163 = CARTESIAN_POINT ( 'NONE',  ( -2.121150477449813534E-15, -11.54700538379251284, -50.37499999999997158 ) ) ;
#2164 = CARTESIAN_POINT ( 'NONE',  ( 10.81189881249999907, 6.242252689847868297, -119.9062500020483810 ) ) ;
#2165 = CARTESIAN_POINT ( 'NONE',  ( -5.405949406249996869, 9.363379034771805109, -98.53125000204839523 ) ) ;
#2166 = ORIENTED_EDGE ( 'NONE', *, *, #6386, .F. ) ;
#2167 = CARTESIAN_POINT ( 'NONE',  ( -9.999999999999998224, 1.224646799147353059E-15, -91.62500000409677625 ) ) ;
#2168 = CARTESIAN_POINT ( 'NONE',  ( 9.999999999999479527, 5.773502691896553074, -72.37499999999997158 ) ) ;
#2169 = CARTESIAN_POINT ( 'NONE',  ( 10.81189881249999729, 0.000000000000000000, -160.5312500020484094 ) ) ;
#2170 = CARTESIAN_POINT ( 'NONE',  ( -10.81189881249999907, -6.242252689847864744, -48.46875000204837391 ) ) ;
#2171 = EDGE_LOOP ( 'NONE', ( #33284, #15417, #26687, #53 ) ) ;
#2172 = CARTESIAN_POINT ( 'NONE',  ( -9.999999999999998224, 5.773502691896259087, -17.87499999999997513 ) ) ;
#2173 = CARTESIAN_POINT ( 'NONE',  ( -2.293366432827344421E-15, -12.48450537969573659, -25.90625000204839168 ) ) ;
#2174 = CARTESIAN_POINT ( 'NONE',  ( 4.999999999999992006, -8.660254037844389075, -153.7500000000000000 ) ) ;
#2175 = CARTESIAN_POINT ( 'NONE',  ( -5.000000000000003553, -8.660254037844383745, -17.87500000409675138 ) ) ;
#2176 = AXIS2_PLACEMENT_3D ( 'NONE', #10835, #17308, #13636 ) ;
#2177 = LOCAL_TIME ( 11, 57, 6.000000000000000000, #25897 ) ;
#2178 = CARTESIAN_POINT ( 'NONE',  ( -5.000000000000003553, -8.660254037844383745, -80.87500000409677625 ) ) ;
#2179 = CARTESIAN_POINT ( 'NONE',  ( 10.81189881249999729, 0.000000000000000000, -123.0312500020483952 ) ) ;
#2180 = LINE ( 'NONE', #18985, #13807 ) ;
#2181 = DIRECTION ( 'NONE',  ( 1.000000000000000000, 0.000000000000000000, 0.000000000000000000 ) ) ;
#2182 = ORIENTED_EDGE ( 'NONE', *, *, #9425, .F. ) ;
#2183 = CARTESIAN_POINT ( 'NONE',  ( -10.81189881249999729, 1.324075727343319199E-15, -51.78125000204835970 ) ) ;
#2184 = COORDINATED_UNIVERSAL_TIME_OFFSET ( 6, 0, .AHEAD. ) ;
#2185 = VECTOR ( 'NONE', #6823, 1000.000000000000000 ) ;
#2186 = CARTESIAN_POINT ( 'NONE',  ( 7.644554776091147741E-16, 12.48450537969573659, -107.4687500020483668 ) ) ;
#2188 = VERTEX_POINT ( 'NONE', #1693 ) ;
#2187 = ORIENTED_EDGE ( 'NONE', *, *, #38630, .T. ) ;
#2189 = DIRECTION ( 'NONE',  ( -0.000000000000000000, -0.000000000000000000, 1.000000000000000000 ) ) ;
#2190 = FACE_OUTER_BOUND ( 'NONE', #25433, .T. ) ;
#2191 = CARTESIAN_POINT ( 'NONE',  ( 5.405949406249999534, 9.363379034771803333, -154.0937500020483810 ) ) ;
#2192 = CARTESIAN_POINT ( 'NONE',  ( -10.81189881249999729, 6.242252689847871849, -191.4062500020484094 ) ) ;
#2193 = CARTESIAN_POINT ( 'NONE',  ( -10.81189881249999907, -6.242252689847864744, -9.468750002048359704 ) ) ;
#2194 = CARTESIAN_POINT ( 'NONE',  ( 5.405949406249999534, 9.363379034771803333, -143.5937500020483810 ) ) ;
#2195 = CARTESIAN_POINT ( 'NONE',  ( 5.405949406249999534, 9.363379034771803333, -110.5937500020483810 ) ) ;
#2196 = CARTESIAN_POINT ( 'NONE',  ( -4.999999999999996447, 8.660254037844387298, -190.8750000040967905 ) ) ;
#2197 = CARTESIAN_POINT ( 'NONE',  ( 10.81189881249999907, 6.242252689847868297, -115.4062500020484094 ) ) ;
#2198 = CARTESIAN_POINT ( 'NONE',  ( 10.81189881249999729, 0.000000000000000000, -4.343750002048368586 ) ) ;
#2199 = CARTESIAN_POINT ( 'NONE',  ( 10.81189881249999729, 6.242252689847867408, -122.7187500020483952 ) ) ;
#2200 = VECTOR ( 'NONE', #3034, 1000.000000000000000 ) ;
#2201 = CARTESIAN_POINT ( 'NONE',  ( -2.293366432827344421E-15, -12.48450537969573659, -192.4062500020484094 ) ) ;
#2202 = CARTESIAN_POINT ( 'NONE',  ( -10.00000000000025580, 5.773502691896109873, -157.3750000000000000 ) ) ;
#2203 = CARTESIAN_POINT ( 'NONE',  ( -10.00000000000000000, -5.773502691896251982, -149.6250000000000284 ) ) ;
#2204 = CARTESIAN_POINT ( 'NONE',  ( 9.999999999999996447, -5.773502691896262640, -15.62499999999997158 ) ) ;
#2205 = CC_DESIGN_APPROVAL ( #30950, ( #40065 ) ) ;
#2206 = CARTESIAN_POINT ( 'NONE',  ( 10.81189881249999551, -6.242252689847874514, -68.96875000204838102 ) ) ;
#2207 = CARTESIAN_POINT ( 'NONE',  ( 10.81189881249999551, -6.242252689847874514, -58.46875000204836681 ) ) ;
#2208 = CARTESIAN_POINT ( 'NONE',  ( 10.00000000000000000, 5.773502691896255534, -189.7500000040968189 ) ) ;
#2209 = CARTESIAN_POINT ( 'NONE',  ( 10.81189881249999907, 6.242252689847868297, -28.40625000204838813 ) ) ;
#2210 = CARTESIAN_POINT ( 'NONE',  ( -10.81189881249999729, 6.242252689847871849, -38.21875000204835970 ) ) ;
#2211 = CARTESIAN_POINT ( 'NONE',  ( 9.999999999999998224, 0.000000000000000000, -37.99999999999997868 ) ) ;
#2212 = CARTESIAN_POINT ( 'NONE',  ( 5.405949406249992428, -9.363379034771808662, -142.5937500020483810 ) ) ;
#2213 = ADVANCED_FACE ( 'NONE', ( #14820 ), #895, .F. ) ;
#2214 = CARTESIAN_POINT ( 'NONE',  ( -4.999999999999996447, 8.660254037844387298, -112.4999999999999858 ) ) ;
#2215 = CARTESIAN_POINT ( 'NONE',  ( 10.00000000000012257, -5.773502691896187144, -170.1250000000000000 ) ) ;
#2216 = EDGE_CURVE ( 'NONE', #17639, #19092, #3050, .T. ) ;
#2217 = CARTESIAN_POINT ( 'NONE',  ( -2.121150477449813534E-15, -11.54700538379251284, -78.87500000000000000 ) ) ;
#2218 = CARTESIAN_POINT ( 'NONE',  ( 5.405949406249999534, 9.363379034771803333, -137.7812500020483810 ) ) ;
#2219 = CARTESIAN_POINT ( 'NONE',  ( 5.405949406249992428, -9.363379034771808662, -10.78125000204835438 ) ) ;
#2220 =( BOUNDED_CURVE ( )  B_SPLINE_CURVE ( 2, ( #18721, #19353, #32333, #29086, #28880, #5567, #2130 ),
 .UNSPECIFIED., .F., .F. ) 
 B_SPLINE_CURVE_WITH_KNOTS ( ( 3, 2, 2, 3 ),
 ( 0.09390547265583264192, 0.09452736318407961580, 0.09577114427860701495, 0.09701492537313441411 ),
 .UNSPECIFIED. ) 
 CURVE ( )  GEOMETRIC_REPRESENTATION_ITEM ( )  RATIONAL_B_SPLINE_CURVE ( ( 0.9330127018922194093, 0.9330127039406161948, 1.000000000000000000, 0.8660254037844387076, 1.000000000000000000, 0.8660254037844297148, 1.000000000000008882 ) ) 
 REPRESENTATION_ITEM ( '' )  );
#2221 = EDGE_CURVE ( 'NONE', #5513, #38469, #34186, .T. ) ;
#2222 = VERTEX_POINT ( 'NONE', #5563 ) ;
#2223 = CARTESIAN_POINT ( 'NONE',  ( 9.999999999999998224, 0.000000000000000000, -176.0000000000000000 ) ) ;
#2224 = CARTESIAN_POINT ( 'NONE',  ( -2.121150477449813534E-15, -11.54700538379251284, -119.7500000040967905 ) ) ;
#2225 = FACE_OUTER_BOUND ( 'NONE', #37868, .T. ) ;
#2226 = CARTESIAN_POINT ( 'NONE',  ( 10.81189881249999551, -6.242252689847874514, -71.96875000204836681 ) ) ;
#2227 = CARTESIAN_POINT ( 'NONE',  ( 9.999999999999996447, -5.773502691896262640, -48.62499999999997868 ) ) ;
#2228 = CARTESIAN_POINT ( 'NONE',  ( 9.999999999999996447, -5.773502691896262640, -23.50000000409677625 ) ) ;
#2229 = CARTESIAN_POINT ( 'NONE',  ( -4.999999999999996447, 8.660254037844387298, -130.5000000000000000 ) ) ;
#2230 = APPROVAL ( #23244, 'UNKNOWN' ) ;
#2231 = CARTESIAN_POINT ( 'NONE',  ( 5.405949406249992428, -9.363379034771808662, -40.78125000204838102 ) ) ;
#2232 =( BOUNDED_CURVE ( )  B_SPLINE_CURVE ( 2, ( #8298, #14738, #1179, #24921, #17766, #11505, #27715 ),
 .UNSPECIFIED., .F., .F. ) 
 B_SPLINE_CURVE_WITH_KNOTS ( ( 3, 2, 2, 3 ),
 ( 0.08955223880597024122, 0.09079601990049755711, 0.09203980099502487300, 0.09328358208955218889 ),
 .UNSPECIFIED. ) 
 CURVE ( )  GEOMETRIC_REPRESENTATION_ITEM ( )  RATIONAL_B_SPLINE_CURVE ( ( 0.9999999999999895639, 0.8660254037844491437, 1.000000000000000000, 0.8660254037844387076, 1.000000000000000000, 0.8660254037844447028, 0.9999999999999940048 ) ) 
 REPRESENTATION_ITEM ( '' )  );
#2233 = CARTESIAN_POINT ( 'NONE',  ( -2.275517850991317657E-15, -20.00000000000000000, -220.0000000000000000 ) ) ;
#2234 = CARTESIAN_POINT ( 'NONE',  ( -5.405949406249996869, 9.363379034771805109, -142.0312500020483810 ) ) ;
#2235 = CARTESIAN_POINT ( 'NONE',  ( -2.293366432827344421E-15, -12.48450537969573659, -151.9062500020483810 ) ) ;
#2236 = CARTESIAN_POINT ( 'NONE',  ( -10.00000000000025580, 5.773502691896109873, -152.8750000000000000 ) ) ;
#2237 = EDGE_CURVE ( 'NONE', #31040, #30574, #2753, .T. ) ;
#2238 = CARTESIAN_POINT ( 'NONE',  ( 4.999999999999992006, -8.660254037844389075, -127.1250000040967620 ) ) ;
#2239 = VERTEX_POINT ( 'NONE', #35563 ) ;
#2240 = VECTOR ( 'NONE', #34079, 1000.000000000000000 ) ;
#2241 =( BOUNDED_CURVE ( )  B_SPLINE_CURVE ( 2, ( #25776, #29433, #19275, #12163, #38929, #35497, #12371 ),
 .UNSPECIFIED., .F., .F. ) 
 B_SPLINE_CURVE_WITH_KNOTS ( ( 3, 2, 2, 3 ),
 ( 0.2014925373134328901, 0.2027363184079602476, 0.2039800995024875774, 0.2052238805970149627 ),
 .UNSPECIFIED. ) 
 CURVE ( )  GEOMETRIC_REPRESENTATION_ITEM ( )  RATIONAL_B_SPLINE_CURVE ( ( 0.9999999999999940048, 0.8660254037844447028, 1.000000000000000000, 0.8660254037844387076, 1.000000000000000000, 0.8660254037844357100, 1.000000000000002887 ) ) 
 REPRESENTATION_ITEM ( '' )  );
#2242 = EDGE_CURVE ( 'NONE', #7196, #19666, #21957, .T. ) ;
#2243 = ORIENTED_EDGE ( 'NONE', *, *, #42575, .T. ) ;
#2244 = ORIENTED_EDGE ( 'NONE', *, *, #20142, .F. ) ;
#2245 = EDGE_CURVE ( 'NONE', #3757, #15077, #8800, .T. ) ;
#2246 = CARTESIAN_POINT ( 'NONE',  ( 5.000000000000000000, 8.660254037844385522, -135.6250000040967620 ) ) ;
#2247 = CARTESIAN_POINT ( 'NONE',  ( -10.81189881249999729, 6.242252689847871849, -179.2187500020483810 ) ) ;
#2248 = CONICAL_SURFACE ( 'NONE', #30493, 57.00000000000002132, 0.7853981633974401744 ) ;
#2249 = CARTESIAN_POINT ( 'NONE',  ( -10.81189881249999729, 6.242252689847871849, -35.21875000204835260 ) ) ;
#2250 = CARTESIAN_POINT ( 'NONE',  ( 9.999999999999998224, 0.000000000000000000, -119.0000000000000000 ) ) ;
#2251 = CARTESIAN_POINT ( 'NONE',  ( -5.405949406250003975, -9.363379034771801557, -165.3437500020484094 ) ) ;
#2252 = CARTESIAN_POINT ( 'NONE',  ( -5.405949406249996869, 9.363379034771805109, -149.3437500020483810 ) ) ;
#2253 = EDGE_CURVE ( 'NONE', #14889, #10615, #26993, .T. ) ;
#2254 = LINE ( 'NONE', #18408, #29341 ) ;
#2255 = CARTESIAN_POINT ( 'NONE',  ( 7.644554776091147741E-16, 12.48450537969573659, -131.4687500020483810 ) ) ;
#2256 = CARTESIAN_POINT ( 'NONE',  ( -2.293366432827344421E-15, -12.48450537969573659, -142.9062500020483810 ) ) ;
#2257 = CARTESIAN_POINT ( 'NONE',  ( 10.81189881249999551, -6.242252689847874514, -142.4687500020483810 ) ) ;
#2258 = CARTESIAN_POINT ( 'NONE',  ( 5.000000000000000000, 8.660254037844385522, -129.2499999999999716 ) ) ;
#2259 = CARTESIAN_POINT ( 'NONE',  ( -9.999999999999998224, 1.224646799147353059E-15, -200.0000000000000000 ) ) ;
#2260 = CARTESIAN_POINT ( 'NONE',  ( -9.999999999999998224, 5.773502691896259087, -170.8750000000000000 ) ) ;
#2261 = CARTESIAN_POINT ( 'NONE',  ( 10.81189881249999729, 0.000000000000000000, -80.84375000204838102 ) ) ;
#2262 = CARTESIAN_POINT ( 'NONE',  ( 0.000000000000000000, 0.000000000000000000, -200.0000000000000000 ) ) ;
#2263 = CARTESIAN_POINT ( 'NONE',  ( 10.81189881249999551, -6.242252689847874514, -48.15625000204836681 ) ) ;
#2264 = CARTESIAN_POINT ( 'NONE',  ( -9.999999999999998224, 1.224646799147353059E-15, -59.74999999999997158 ) ) ;
#2265 = CARTESIAN_POINT ( 'NONE',  ( 5.405949406249992428, -9.363379034771808662, -168.0937500020484094 ) ) ;
#2266 = CARTESIAN_POINT ( 'NONE',  ( -9.999999999999998224, 1.224646799147353059E-15, -137.7499999999999716 ) ) ;
#2267 = CARTESIAN_POINT ( 'NONE',  ( -5.405949406250003975, -9.363379034771801557, -147.5312500020483810 ) ) ;
#2268 = CARTESIAN_POINT ( 'NONE',  ( -9.999999999999998224, 1.224646799147353059E-15, -142.6250000040967905 ) ) ;
#2269 = CARTESIAN_POINT ( 'NONE',  ( -10.81189881249999729, 1.324075727343319199E-15, -33.78125000204837391 ) ) ;
#2270 = CARTESIAN_POINT ( 'NONE',  ( -9.999999999999998224, 1.224646799147353059E-15, -123.1250000040967905 ) ) ;
#2271 = CARTESIAN_POINT ( 'NONE',  ( 9.999999999999996447, -5.773502691896262640, -101.1250000000000000 ) ) ;
#2272 = AXIS2_PLACEMENT_3D ( 'NONE', #14325, #20388, #33375 ) ;
#2273 = ORIENTED_EDGE ( 'NONE', *, *, #17957, .T. ) ;
#2274 = CARTESIAN_POINT ( 'NONE',  ( 10.81189881249999729, 0.000000000000000000, -118.5312500020483952 ) ) ;
#2275 = CARTESIAN_POINT ( 'NONE',  ( 10.00000000000000000, 5.773502691896255534, -143.2500000040967905 ) ) ;
#2276 = CARTESIAN_POINT ( 'NONE',  ( -2.121150477449813534E-15, -11.54700538379251284, -48.87499999999997158 ) ) ;
#2277 = CARTESIAN_POINT ( 'NONE',  ( -10.81189881249999729, 6.242252689847871849, -179.4062500020484094 ) ) ;
#2278 = ORIENTED_EDGE ( 'NONE', *, *, #27004, .F. ) ;
#2279 = CARTESIAN_POINT ( 'NONE',  ( 10.00000000000000000, 5.773502691896255534, -48.75000000409676204 ) ) ;
#2280 = CARTESIAN_POINT ( 'NONE',  ( 5.000000000000000000, 8.660254037844385522, -130.7499999999999716 ) ) ;
#2281 = CARTESIAN_POINT ( 'NONE',  ( 5.405949406249999534, 9.363379034771803333, -67.28125000204838102 ) ) ;
#2282 = CARTESIAN_POINT ( 'NONE',  ( 0.000000000000000000, 0.000000000000000000, -200.0000000000000000 ) ) ;
#2283 = CARTESIAN_POINT ( 'NONE',  ( -5.405949406250003975, -9.363379034771801557, -173.0312500020484094 ) ) ;
#2284 = CARTESIAN_POINT ( 'NONE',  ( 7.070501591499376803E-16, 11.54700538379251284, -7.624999999999972466 ) ) ;
#2285 = CARTESIAN_POINT ( 'NONE',  ( 10.00000000000154010, -5.773502691895370020, -56.12499999999992895 ) ) ;
#2286 = EDGE_LOOP ( 'NONE', ( #18485, #33810 ) ) ;
#2287 = CARTESIAN_POINT ( 'NONE',  ( 0.000000000000000000, 0.000000000000000000, -200.0000000000000000 ) ) ;
#2288 = CARTESIAN_POINT ( 'NONE',  ( 7.070501591499376803E-16, 11.54700538379251284, -173.0000000040967905 ) ) ;
#2289 = CARTESIAN_POINT ( 'NONE',  ( 4.999999999999992006, -8.660254037844389075, -71.24999999999998579 ) ) ;
#2291 = VERTEX_POINT ( 'NONE', #38994 ) ;
#2290 = CARTESIAN_POINT ( 'NONE',  ( -10.81189881249999729, 1.324075727343319199E-15, -75.78125000204838102 ) ) ;
#2293 = VERTEX_POINT ( 'NONE', #5990 ) ;
#2292 = CARTESIAN_POINT ( 'NONE',  ( -9.999999999999998224, 1.224646799147353059E-15, -98.74999999999998579 ) ) ;
#2294 = ORIENTED_EDGE ( 'NONE', *, *, #14066, .F. ) ;
#2295 = CARTESIAN_POINT ( 'NONE',  ( -2.293366432827344421E-15, -12.48450537969573659, -30.21875000204834549 ) ) ;
#2296 = DIRECTION ( 'NONE',  ( 0.000000000000000000, 0.000000000000000000, -1.000000000000000000 ) ) ;
#2297 = CARTESIAN_POINT ( 'NONE',  ( 10.81189881249999729, 0.000000000000000000, -3.031250002048374803 ) ) ;
#2299 = EDGE_LOOP ( 'NONE', ( #17913, #27942, #12689, #35616 ) ) ;
#2298 = CARTESIAN_POINT ( 'NONE',  ( -2.293366432827344421E-15, -12.48450537969573659, -57.21875000204835970 ) ) ;
#2300 = CARTESIAN_POINT ( 'NONE',  ( 9.999999999999996447, -5.773502691896262640, -39.62499999999995737 ) ) ;
#2301 = CARTESIAN_POINT ( 'NONE',  ( -2.293366432827344421E-15, -12.48450537969573659, -190.7187500020484094 ) ) ;
#2302 = CARTESIAN_POINT ( 'NONE',  ( 10.81189881249999907, 6.242252689847868297, -179.7187500020484094 ) ) ;
#2303 =( BOUNDED_CURVE ( )  B_SPLINE_CURVE ( 2, ( #1822, #2666, #28791, #19058, #41922, #35478, #28578 ),
 .UNSPECIFIED., .F., .F. ) 
 B_SPLINE_CURVE_WITH_KNOTS ( ( 3, 2, 2, 3 ),
 ( 0.1044776119402986148, 0.1057213930348259306, 0.1069651741293532465, 0.1082089552238805485 ),
 .UNSPECIFIED. ) 
 CURVE ( )  GEOMETRIC_REPRESENTATION_ITEM ( )  RATIONAL_B_SPLINE_CURVE ( ( 0.9999999999999880096, 0.8660254037844506980, 1.000000000000000000, 0.8660254037844387076, 1.000000000000000000, 0.8660254037844431485, 0.9999999999999955591 ) ) 
 REPRESENTATION_ITEM ( '' )  );
#2304 = CARTESIAN_POINT ( 'NONE',  ( -10.81189881249999729, 1.324075727343319199E-15, -161.0937500020484094 ) ) ;
#2305 = CARTESIAN_POINT ( 'NONE',  ( -2.293366432827344421E-15, -12.48450537969573659, -166.7187500020483810 ) ) ;
#2306 = CARTESIAN_POINT ( 'NONE',  ( 4.999999999999992006, -8.660254037844389075, -75.74999999999998579 ) ) ;
#2307 = LINE ( 'NONE', #42185, #12936 ) ;
#2308 = CARTESIAN_POINT ( 'NONE',  ( 10.00000000000000000, 5.773502691896255534, -193.8750000000000284 ) ) ;
#2309 = CARTESIAN_POINT ( 'NONE',  ( -5.405949406250003975, -9.363379034771801557, -105.3437500020483810 ) ) ;
#2310 = CARTESIAN_POINT ( 'NONE',  ( 5.405949406249992428, -9.363379034771808662, -70.78125000204838102 ) ) ;
#2311 = CARTESIAN_POINT ( 'NONE',  ( 10.81189881249999729, 0.000000000000000000, -92.84375000204838102 ) ) ;
#2312 = CARTESIAN_POINT ( 'NONE',  ( 10.81189881249999551, -6.242252689847874514, -70.65625000204839523 ) ) ;
#2313 = CARTESIAN_POINT ( 'NONE',  ( -9.999999999999998224, 1.224646799147353059E-15, -148.6250000040967905 ) ) ;
#2314 = CARTESIAN_POINT ( 'NONE',  ( 9.999999999999996447, -5.773502691896262640, -122.1250000000000000 ) ) ;
#2315 = ORIENTED_EDGE ( 'NONE', *, *, #39416, .F. ) ;
#2316 = CARTESIAN_POINT ( 'NONE',  ( 10.81189881249999729, 6.242252689847867408, -148.4062500020484094 ) ) ;
#2317 = CARTESIAN_POINT ( 'NONE',  ( -5.405949406250003975, -9.363379034771801557, -165.5312500020484094 ) ) ;
#2318 = CARTESIAN_POINT ( 'NONE',  ( 4.999999999999992006, -8.660254037844389075, -179.2500000000000284 ) ) ;
#2319 = CARTESIAN_POINT ( 'NONE',  ( 10.81189881249999729, 0.000000000000000000, -94.34375000204838102 ) ) ;
#2320 = VERTEX_POINT ( 'NONE', #19347 ) ;
#2321 = CARTESIAN_POINT ( 'NONE',  ( -10.00000000000000000, -5.773502691896251982, -62.62499999999996447 ) ) ;
#2322 = CARTESIAN_POINT ( 'NONE',  ( -10.81189881249999729, 6.242252689847871849, -198.7187500020484379 ) ) ;
#2323 = CARTESIAN_POINT ( 'NONE',  ( -10.00000000000000000, -5.773502691896251982, -76.50000000409677625 ) ) ;
#2324 = CARTESIAN_POINT ( 'NONE',  ( -7.747353181636939645, -6.452982553152641465, -179.9999999999999432 ) ) ;
#2325 = CARTESIAN_POINT ( 'NONE',  ( 9.999999999999998224, 0.000000000000000000, -200.0000000000000000 ) ) ;
#2326 = CARTESIAN_POINT ( 'NONE',  ( 5.405949406249999534, 9.363379034771803333, -92.78125000204838102 ) ) ;
#2327 = CARTESIAN_POINT ( 'NONE',  ( 10.81189881249999551, -6.242252689847874514, -66.15625000204839523 ) ) ;
#2328 = CARTESIAN_POINT ( 'NONE',  ( -2.121150477449813534E-15, -11.54700538379251284, -64.25000000409677625 ) ) ;
#2329 = FACE_OUTER_BOUND ( 'NONE', #10062, .T. ) ;
#2330 = CARTESIAN_POINT ( 'NONE',  ( -10.81189881249999729, 6.242252689847871849, -27.71875000204837391 ) ) ;
#2331 = CARTESIAN_POINT ( 'NONE',  ( 9.999999999999998224, 0.000000000000000000, -100.9999999999999858 ) ) ;
#2332 = CARTESIAN_POINT ( 'NONE',  ( 5.405949406249992428, -9.363379034771808662, -190.7812500020484094 ) ) ;
#2333 = ADVANCED_FACE ( 'NONE', ( #6201 ), #9430, .T. ) ;
#2334 = CARTESIAN_POINT ( 'NONE',  ( 7.644554776091147741E-16, 12.48450537969573659, -23.65625000204838102 ) ) ;
#2335 = CARTESIAN_POINT ( 'NONE',  ( 10.81189881249999551, -6.242252689847874514, -8.968750002048359704 ) ) ;
#2336 = DIRECTION ( 'NONE',  ( -1.000000000000000000, 0.000000000000000000, 0.000000000000000000 ) ) ;
#2337 = CARTESIAN_POINT ( 'NONE',  ( 9.999999999999998224, 0.000000000000000000, -177.5000000000000000 ) ) ;
#2338 = CARTESIAN_POINT ( 'NONE',  ( 5.000000000000000000, 8.660254037844385522, -1.749999999999973799 ) ) ;
#2340 = ORIENTED_EDGE ( 'NONE', *, *, #1727, .T. ) ;
#2339 = CARTESIAN_POINT ( 'NONE',  ( 10.81189881249999729, 0.000000000000000000, -102.0312500020483952 ) ) ;
#2341 = CARTESIAN_POINT ( 'NONE',  ( -9.999999999999996447, 5.773502691896259975, -169.7500000040967905 ) ) ;
#2342 = VERTEX_POINT ( 'NONE', #42008 ) ;
#2343 = ORIENTED_EDGE ( 'NONE', *, *, #6261, .T. ) ;
#2344 = EDGE_CURVE ( 'NONE', #5784, #15394, #41602, .T. ) ;
#2345 =( BOUNDED_CURVE ( )  B_SPLINE_CURVE ( 2, ( #21279, #34465, #7482, #31231, #34681, #37044, #18249 ),
 .UNSPECIFIED., .F., .F. ) 
 B_SPLINE_CURVE_WITH_KNOTS ( ( 3, 2, 2, 3 ),
 ( 0.6940298507462688837, 0.6952736318407962690, 0.6965174129353237653, 0.6977611940298510396 ),
 .UNSPECIFIED. ) 
 CURVE ( )  GEOMETRIC_REPRESENTATION_ITEM ( )  RATIONAL_B_SPLINE_CURVE ( ( 0.9999999999999761302, 0.8660254037844625774, 1.000000000000000000, 0.8660254037844387076, 1.000000000000000000, 0.8660254037844028474, 1.000000000000035971 ) ) 
 REPRESENTATION_ITEM ( '' )  );
#2346 = CARTESIAN_POINT ( 'NONE',  ( 5.405949406249992428, -9.363379034771808662, -30.28125000204837036 ) ) ;
#2347 = DATE_AND_TIME ( #6214, #18726 ) ;
#2348 = CARTESIAN_POINT ( 'NONE',  ( -5.405949406250003975, -9.363379034771801557, -75.34375000204838102 ) ) ;
#2349 = CARTESIAN_POINT ( 'NONE',  ( -9.999999999999998224, 0.000000000000000000, -99.99999999999998579 ) ) ;
#2350 = CARTESIAN_POINT ( 'NONE',  ( 9.462123412026320679, -3.482913390811684717, -100.0000000000000426 ) ) ;
#2351 = CARTESIAN_POINT ( 'NONE',  ( 7.070501591499376803E-16, 11.54700538379251284, -124.6249999999999858 ) ) ;
#2352 = CARTESIAN_POINT ( 'NONE',  ( -10.81189881249999907, -6.242252689847864744, -161.1562500020484094 ) ) ;
#2353 = CARTESIAN_POINT ( 'NONE',  ( -9.999999999999998224, 1.224646799147353059E-15, -10.62500000409674605 ) ) ;
#2354 = CARTESIAN_POINT ( 'NONE',  ( -9.999999999999998224, 1.224646799147353059E-15, -86.74999999999998579 ) ) ;
#2355 = CARTESIAN_POINT ( 'NONE',  ( 7.644554776091147741E-16, 12.48450537969573659, -129.9687500020483810 ) ) ;
#2356 = CARTESIAN_POINT ( 'NONE',  ( 10.81189881249999551, -6.242252689847874514, -113.9687500020483668 ) ) ;
#2357 = CARTESIAN_POINT ( 'NONE',  ( 10.81189881249999729, 0.000000000000000000, -88.34375000204838102 ) ) ;
#2358 = CARTESIAN_POINT ( 'NONE',  ( 7.644554776091147741E-16, 12.48450537969573659, -92.65625000204839523 ) ) ;
#2359 = CARTESIAN_POINT ( 'NONE',  ( 9.999999999999998224, 0.000000000000000000, -168.8750000040967905 ) ) ;
#2360 = CARTESIAN_POINT ( 'NONE',  ( -10.81189881249999729, 1.324075727343319199E-15, -173.2812500020484094 ) ) ;
#2361 = CARTESIAN_POINT ( 'NONE',  ( 9.999999999999998224, 0.000000000000000000, -27.87500000409676204 ) ) ;
#2362 = CARTESIAN_POINT ( 'NONE',  ( 5.405949406249999534, 9.363379034771803333, -172.2812500020484094 ) ) ;
#2363 = CARTESIAN_POINT ( 'NONE',  ( 5.405949406249992428, -9.363379034771808662, -192.2812500020484094 ) ) ;
#2364 = CARTESIAN_POINT ( 'NONE',  ( 10.81189881249999729, 6.242252689847867408, -44.71875000204837391 ) ) ;
#2365 = CARTESIAN_POINT ( 'NONE',  ( -9.999999999999998224, 5.773502691896259087, -163.7500000040967905 ) ) ;
#2366 = CARTESIAN_POINT ( 'NONE',  ( 9.999999999999998224, 0.000000000000000000, -86.37500000409677625 ) ) ;
#2367 = CARTESIAN_POINT ( 'NONE',  ( 10.81189881249999907, 6.242252689847868297, -17.71875000204836681 ) ) ;
#2368 = DIRECTION ( 'NONE',  ( -0.000000000000000000, -0.000000000000000000, 1.000000000000000000 ) ) ;
#2369 = CARTESIAN_POINT ( 'NONE',  ( 5.405949406249992428, -9.363379034771808662, -121.5937500020483952 ) ) ;
#2370 = CARTESIAN_POINT ( 'NONE',  ( 4.999999999999992006, -8.660254037844389075, -92.24999999999998579 ) ) ;
#2371 = CARTESIAN_POINT ( 'NONE',  ( -10.81189881249999907, -6.242252689847864744, -23.15625000204837747 ) ) ;
#2372 = CARTESIAN_POINT ( 'NONE',  ( -4.999999999999996447, 8.660254037844387298, -96.37500000409677625 ) ) ;
#2373 = CARTESIAN_POINT ( 'NONE',  ( -9.999999999999998224, 1.224646799147353059E-15, -150.1250000040967905 ) ) ;
#2374 = CARTESIAN_POINT ( 'NONE',  ( 5.405949406249992428, -9.363379034771808662, -115.7812500020483952 ) ) ;
#2375 = CARTESIAN_POINT ( 'NONE',  ( 10.81189881249999551, -6.242252689847874514, -102.1562500020483952 ) ) ;
#2376 = VERTEX_POINT ( 'NONE', #38567 ) ;
#2377 = EDGE_CURVE ( 'NONE', #33916, #36657, #22178, .T. ) ;
#2378 = CARTESIAN_POINT ( 'NONE',  ( -4.999999999999996447, 8.660254037844387298, -94.87500000409677625 ) ) ;
#2379 = DIRECTION ( 'NONE',  ( 0.000000000000000000, 0.000000000000000000, -1.000000000000000000 ) ) ;
#2380 = CARTESIAN_POINT ( 'NONE',  ( -10.81189881249999729, 6.242252689847871849, -159.9062500020483810 ) ) ;
#2381 = CARTESIAN_POINT ( 'NONE',  ( -5.405949406249996869, 9.363379034771805109, -50.34375000204835260 ) ) ;
#2382 = ORIENTED_EDGE ( 'NONE', *, *, #1313, .F. ) ;
#2383 = CARTESIAN_POINT ( 'NONE',  ( 4.999999999999992006, -8.660254037844389075, -18.74999999999996092 ) ) ;
#2384 = CARTESIAN_POINT ( 'NONE',  ( -10.81189881249999729, 6.242252689847871849, -26.40625000204837747 ) ) ;
#2385 = CARTESIAN_POINT ( 'NONE',  ( 4.999999999999992006, -8.660254037844389075, -156.7500000000000000 ) ) ;
#2386 = CARTESIAN_POINT ( 'NONE',  ( -5.000000000000003553, -8.660254037844383745, -16.37500000409675138 ) ) ;
#2387 = CARTESIAN_POINT ( 'NONE',  ( 10.00000000000051159, -5.773502691895965988, -119.5000000040967905 ) ) ;
#2389 = ORIENTED_EDGE ( 'NONE', *, *, #4119, .T. ) ;
#2388 = CARTESIAN_POINT ( 'NONE',  ( -10.81189881249999729, 1.324075727343319199E-15, -129.7812500020483810 ) ) ;
#2390 = CARTESIAN_POINT ( 'NONE',  ( -8.660253955908514101, -5.000000141917089636, -180.0000000000000284 ) ) ;
#2391 = ORIENTED_EDGE ( 'NONE', *, *, #21343, .F. ) ;
#2392 = CARTESIAN_POINT ( 'NONE',  ( 10.81189881249999907, 6.242252689847868297, -52.40625000204838813 ) ) ;
#2393 = DATE_AND_TIME ( #6047, #33865 ) ;
#2394 = CARTESIAN_POINT ( 'NONE',  ( 10.81189881249999907, 6.242252689847868297, -106.2187500020483668 ) ) ;
#2395 = EDGE_CURVE ( 'NONE', #15576, #38192, #6322, .T. ) ;
#2397 = ORIENTED_EDGE ( 'NONE', *, *, #41638, .T. ) ;
#2396 = ORIENTED_EDGE ( 'NONE', *, *, #1177, .T. ) ;
#2398 = CYLINDRICAL_SURFACE ( 'NONE', #14178, 9.999999999999998224 ) ;
#2399 = CARTESIAN_POINT ( 'NONE',  ( -2.293366432827344421E-15, -12.48450537969573659, -159.2187500020483810 ) ) ;
#2400 = CARTESIAN_POINT ( 'NONE',  ( -2.293366432827344421E-15, -12.48450537969573659, -186.4062500020484094 ) ) ;
#2401 = CARTESIAN_POINT ( 'NONE',  ( -2.293366432827344421E-15, -12.48450537969573659, -4.718750002048369474 ) ) ;
#2402 = FACE_OUTER_BOUND ( 'NONE', #32173, .T. ) ;
#2403 = CARTESIAN_POINT ( 'NONE',  ( -5.405949406249996869, 9.363379034771805109, -141.8437500020483810 ) ) ;
#2404 = CARTESIAN_POINT ( 'NONE',  ( 10.81189881249999729, 0.000000000000000000, -109.3437500020483810 ) ) ;
#2405 = CARTESIAN_POINT ( 'NONE',  ( 9.999999999998456346, 5.773502691897149042, -55.87499999999995026 ) ) ;
#2406 = CARTESIAN_POINT ( 'NONE',  ( 5.405949406249992428, -9.363379034771808662, -114.2812500020483952 ) ) ;
#2407 = CARTESIAN_POINT ( 'NONE',  ( -9.999999999999998224, 5.773502691896259087, -193.7500000040967905 ) ) ;
#2408 = CARTESIAN_POINT ( 'NONE',  ( 5.405949406249999534, 9.363379034771803333, -124.0937500020483952 ) ) ;
#2409 = CARTESIAN_POINT ( 'NONE',  ( -10.81189881249999729, 6.242252689847871849, -192.9062500020484094 ) ) ;
#2410 = CARTESIAN_POINT ( 'NONE',  ( 0.000000000000000000, 0.000000000000000000, -200.0000000000000000 ) ) ;
#2411 = CARTESIAN_POINT ( 'NONE',  ( 4.999999999999992006, -8.660254037844389075, -138.7499999999999716 ) ) ;
#2412 = CARTESIAN_POINT ( 'NONE',  ( -9.999999999999998224, 5.773502691896259087, -13.37499999999996980 ) ) ;
#2413 = CARTESIAN_POINT ( 'NONE',  ( 10.81189881249999551, -6.242252689847874514, -70.46875000204839523 ) ) ;
#2414 = CARTESIAN_POINT ( 'NONE',  ( -10.81189881249999729, 6.242252689847871849, -54.71875000204838102 ) ) ;
#2415 = CARTESIAN_POINT ( 'NONE',  ( 4.999999999999992006, -8.660254037844389075, -191.6250000040967905 ) ) ;
#2416 = CARTESIAN_POINT ( 'NONE',  ( -5.405949406250003975, -9.363379034771801557, -29.03125000204837036 ) ) ;
#2417 = CARTESIAN_POINT ( 'NONE',  ( 5.405949406249999534, 9.363379034771803333, -35.59375000204836681 ) ) ;
#2418 = CARTESIAN_POINT ( 'NONE',  ( -10.00000000000102496, 5.773502691895664007, -52.75000000409673362 ) ) ;
#2419 = CARTESIAN_POINT ( 'NONE',  ( 10.81189881249999729, 0.000000000000000000, -149.8437500020483810 ) ) ;
#2420 = CARTESIAN_POINT ( 'NONE',  ( 10.00000000000000000, 5.773502691896255534, -112.8749999999999858 ) ) ;
#2421 = CARTESIAN_POINT ( 'NONE',  ( 10.00000000000000000, 5.773502691896255534, -136.8750000000000000 ) ) ;
#2422 = CARTESIAN_POINT ( 'NONE',  ( 4.999999999999992006, -8.660254037844389075, -77.24999999999998579 ) ) ;
#2423 = CARTESIAN_POINT ( 'NONE',  ( 5.405949406249992428, -9.363379034771808662, -141.2812500020483810 ) ) ;
#2424 = CARTESIAN_POINT ( 'NONE',  ( 10.81189881249999729, 0.000000000000000000, -12.03125000204835438 ) ) ;
#2425 = VERTEX_POINT ( 'NONE', #25632 ) ;
#2426 = DIRECTION ( 'NONE',  ( -0.000000000000000000, -0.000000000000000000, 1.000000000000000000 ) ) ;
#2427 = CARTESIAN_POINT ( 'NONE',  ( -5.000000000000003553, -8.660254037844383745, -116.8750000040967905 ) ) ;
#2428 = CARTESIAN_POINT ( 'NONE',  ( 10.81189881249999907, 6.242252689847868297, -71.71875000204836681 ) ) ;
#2429 = CARTESIAN_POINT ( 'NONE',  ( 4.999999999999992006, -8.660254037844389075, -38.24999999999997868 ) ) ;
#2430 = CARTESIAN_POINT ( 'NONE',  ( -5.000000000000003553, -8.660254037844383745, -22.37500000409675494 ) ) ;
#2431 = CARTESIAN_POINT ( 'NONE',  ( 10.81189881249999729, 0.000000000000000000, -52.53125000204835970 ) ) ;
#2432 = CARTESIAN_POINT ( 'NONE',  ( -4.999999999999996447, 8.660254037844387298, -118.8750000040967905 ) ) ;
#2433 = CARTESIAN_POINT ( 'NONE',  ( -10.81189881249999729, 1.324075727343319199E-15, -35.28125000204837391 ) ) ;
#2434 = DIRECTION ( 'NONE',  ( 1.000000000000000000, 0.000000000000000000, 0.000000000000000000 ) ) ;
#2435 = CARTESIAN_POINT ( 'NONE',  ( 5.405949406249999534, 9.363379034771803333, -145.2812500020483810 ) ) ;
#2436 = CARTESIAN_POINT ( 'NONE',  ( -10.81189881249999907, -6.242252689847864744, -147.6562500020483810 ) ) ;
#2437 = CARTESIAN_POINT ( 'NONE',  ( 9.999999999999998224, 0.000000000000000000, -64.99999999999997158 ) ) ;
#2438 = CARTESIAN_POINT ( 'NONE',  ( 0.000000000000000000, 0.000000000000000000, -200.0000000000000000 ) ) ;
#2439 = ORIENTED_EDGE ( 'NONE', *, *, #20097, .F. ) ;
#2440 = AXIS2_PLACEMENT_3D ( 'NONE', #39241, #35600, #42257 ) ;
#2441 = ORIENTED_EDGE ( 'NONE', *, *, #24077, .T. ) ;
#2442 = ADVANCED_FACE ( 'NONE', ( #34927 ), #5348, .F. ) ;
#2443 = EDGE_LOOP ( 'NONE', ( #16410, #16308 ) ) ;
#2444 = EDGE_CURVE ( 'NONE', #6831, #23986, #28456, .T. ) ;
#2445 = CARTESIAN_POINT ( 'NONE',  ( 4.999999999999992006, -8.660254037844389075, -176.6250000040968189 ) ) ;
#2446 = CARTESIAN_POINT ( 'NONE',  ( 10.81189881249999907, 6.242252689847868297, -181.2187500020484094 ) ) ;
#2447 = CARTESIAN_POINT ( 'NONE',  ( 10.81189881249999729, 0.000000000000000000, -34.34375000204836681 ) ) ;
#2448 = LINE ( 'NONE', #25119, #40478 ) ;
#2449 = CARTESIAN_POINT ( 'NONE',  ( 7.644554776091147741E-16, 12.48450537969573659, -165.9687500020483810 ) ) ;
#2450 = CARTESIAN_POINT ( 'NONE',  ( 5.405949406249999534, 9.363379034771803333, -154.0937500020483810 ) ) ;
#2451 = CARTESIAN_POINT ( 'NONE',  ( -2.121150477449813534E-15, -11.54700538379251284, -176.3750000000000000 ) ) ;
#2452 = CARTESIAN_POINT ( 'NONE',  ( -2.293366432827344421E-15, -12.48450537969573659, -132.2187500020483810 ) ) ;
#2453 = VECTOR ( 'NONE', #31359, 1000.000000000000000 ) ;
#2454 = CARTESIAN_POINT ( 'NONE',  ( -10.81189881249999729, 6.242252689847871849, -141.9062500020484094 ) ) ;
#2456 = CARTESIAN_POINT ( 'NONE',  ( -10.81189881249999907, -6.242252689847864744, -18.46875000204837036 ) ) ;
#2455 =( BOUNDED_CURVE ( )  B_SPLINE_CURVE ( 2, ( #13959, #23710, #26521, #20454, #7304, #13542, #4063 ),
 .UNSPECIFIED., .F., .F. ) 
 B_SPLINE_CURVE_WITH_KNOTS ( ( 3, 2, 2, 3 ),
 ( 0.7611940298507464675, 0.7624378109452738528, 0.7636815920398011270, 0.7649253731343285123 ),
 .UNSPECIFIED. ) 
 CURVE ( )  GEOMETRIC_REPRESENTATION_ITEM ( )  RATIONAL_B_SPLINE_CURVE ( ( 0.9999999999999761302, 0.8660254037844625774, 1.000000000000000000, 0.8660254037844387076, 1.000000000000000000, 0.8660254037844267172, 1.000000000000011990 ) ) 
 REPRESENTATION_ITEM ( '' )  );
#2457 = CARTESIAN_POINT ( 'NONE',  ( 10.81189881249999729, 0.000000000000000000, -145.3437500020483810 ) ) ;
#2458 = CARTESIAN_POINT ( 'NONE',  ( -5.500000000000003553, 20.00000000000000000, -220.0000000000000000 ) ) ;
#2459 = DIRECTION ( 'NONE',  ( -0.000000000000000000, -0.000000000000000000, -1.000000000000000000 ) ) ;
#2460 = CARTESIAN_POINT ( 'NONE',  ( -9.999999999999998224, 5.773502691896259087, -169.3750000000000000 ) ) ;
#2461 = CARTESIAN_POINT ( 'NONE',  ( 7.644554776091147741E-16, 12.48450537969573659, -81.96875000204839523 ) ) ;
#2462 = CARTESIAN_POINT ( 'NONE',  ( -9.183694056713487929E-15, 20.00000000000000711, 12.49999999999999112 ) ) ;
#2463 = CARTESIAN_POINT ( 'NONE',  ( 10.81189881249999551, -6.242252689847874514, -49.65625000204837391 ) ) ;
#2464 = CARTESIAN_POINT ( 'NONE',  ( -2.293366432827344421E-15, -12.48450537969573659, -63.21875000204838102 ) ) ;
#2465 = CARTESIAN_POINT ( 'NONE',  ( 10.00000000000051159, -5.773502691895965988, -149.1249999999999716 ) ) ;
#2466 = CARTESIAN_POINT ( 'NONE',  ( 5.405949406249999534, 9.363379034771803333, -170.5937500020484094 ) ) ;
#2467 = ADVANCED_FACE ( 'NONE', ( #13697 ), #10263, .T. ) ;
#2468 = CARTESIAN_POINT ( 'NONE',  ( 10.00000000000000000, 5.773502691896255534, -138.3750000000000000 ) ) ;
#2469 = VECTOR ( 'NONE', #30727, 1000.000000000000000 ) ;
#2470 = CARTESIAN_POINT ( 'NONE',  ( 10.81189881249999551, -6.242252689847874514, -144.1562500020484094 ) ) ;
#2471 = CARTESIAN_POINT ( 'NONE',  ( 5.405949406249992428, -9.363379034771808662, -33.28125000204837391 ) ) ;
#2472 = CARTESIAN_POINT ( 'NONE',  ( 4.999999999999992006, -8.660254037844389075, -121.1250000040967905 ) ) ;
#2473 = CARTESIAN_POINT ( 'NONE',  ( 10.00000000000000000, 5.773502691896255534, -102.3749999999999858 ) ) ;
#2474 = ORIENTED_EDGE ( 'NONE', *, *, #18806, .T. ) ;
#2475 = CARTESIAN_POINT ( 'NONE',  ( 10.81189881249999729, 6.242252689847867408, -118.4062500020483810 ) ) ;
#2476 = CARTESIAN_POINT ( 'NONE',  ( -4.999999999999996447, 8.660254037844387298, -141.3750000040967905 ) ) ;
#2477 = CARTESIAN_POINT ( 'NONE',  ( 9.999999999999998224, 0.000000000000000000, -125.0000000000000000 ) ) ;
#2478 = CARTESIAN_POINT ( 'NONE',  ( -10.81189881249999907, -6.242252689847864744, -170.1562500020483810 ) ) ;
#2479 = CARTESIAN_POINT ( 'NONE',  ( -9.999999999999998224, 1.224646799147353059E-15, -46.62500000409677625 ) ) ;
#2480 = EDGE_CURVE ( 'NONE', #35035, #8964, #11432, .T. ) ;
#2481 = CARTESIAN_POINT ( 'NONE',  ( -5.000000000000003553, -8.660254037844383745, -98.49999999999998579 ) ) ;
#2482 = CARTESIAN_POINT ( 'NONE',  ( -5.405949406250003975, -9.363379034771801557, -59.03125000204836681 ) ) ;
#2483 = CARTESIAN_POINT ( 'NONE',  ( 10.00000000000025402, -5.773502691896113426, -134.5000000040967905 ) ) ;
#2484 = CARTESIAN_POINT ( 'NONE',  ( 10.81189881249999729, 0.000000000000000000, -169.5312500020484094 ) ) ;
#2485 = DIRECTION ( 'NONE',  ( -0.3779644730092255878, -0.6546536707079759765, 0.6546536707079793072 ) ) ;
#2486 = CARTESIAN_POINT ( 'NONE',  ( -9.999999999999998224, 1.224646799147353059E-15, -178.2500000000000284 ) ) ;
#2487 = ORIENTED_EDGE ( 'NONE', *, *, #39307, .F. ) ;
#2488 = CARTESIAN_POINT ( 'NONE',  ( -9.999999999999868550, 5.773502691896333694, -176.8750000000000000 ) ) ;
#2489 = AXIS2_PLACEMENT_3D ( 'NONE', #21699, #28618, #1866 ) ;
#2490 = AXIS2_PLACEMENT_3D ( 'NONE', #26366, #42534, #23345 ) ;
#2491 = CARTESIAN_POINT ( 'NONE',  ( -1.040834085586084257E-14, 125.0000000000000000, 22.49999999999999289 ) ) ;
#2493 = VERTEX_POINT ( 'NONE', #33169 ) ;
#2492 = CARTESIAN_POINT ( 'NONE',  ( -5.405949406250003975, -9.363379034771801557, -77.03125000204838102 ) ) ;
#2494 = DIRECTION ( 'NONE',  ( 1.000000000000000000, 0.000000000000000000, 0.000000000000000000 ) ) ;
#2495 = EDGE_CURVE ( 'NONE', #14436, #20180, #26679, .T. ) ;
#2497 = VERTEX_POINT ( 'NONE', #39412 ) ;
#2496 = CARTESIAN_POINT ( 'NONE',  ( 4.999999999999992006, -8.660254037844389075, -140.2500000000000000 ) ) ;
#2498 = AXIS2_PLACEMENT_3D ( 'NONE', #31974, #14726, #8283 ) ;
#2499 = ORIENTED_EDGE ( 'NONE', *, *, #3935, .T. ) ;
#2500 = EDGE_CURVE ( 'NONE', #342, #5087, #34448, .T. ) ;
#2501 = CARTESIAN_POINT ( 'NONE',  ( 7.644554776091147741E-16, 12.48450537969573659, -27.96875000204838457 ) ) ;
#2502 = CARTESIAN_POINT ( 'NONE',  ( -9.999999999999998224, 1.224646799147353059E-15, -73.62500000409677625 ) ) ;
#2503 = CARTESIAN_POINT ( 'NONE',  ( -2.293366432827344421E-15, -12.48450537969573659, -4.906250002048355263 ) ) ;
#2506 = EDGE_CURVE ( 'NONE', #41485, #10102, #8689, .T. ) ;
#2505 = ORIENTED_EDGE ( 'NONE', *, *, #42040, .F. ) ;
#2504 = CARTESIAN_POINT ( 'NONE',  ( 10.81189881249999551, -6.242252689847874514, -55.46875000204837391 ) ) ;
#2507 = CARTESIAN_POINT ( 'NONE',  ( 0.000000000000000000, 0.000000000000000000, -200.0000000000000000 ) ) ;
#2508 = CARTESIAN_POINT ( 'NONE',  ( 10.00000000000000000, 5.773502691896255534, -33.37499999999996447 ) ) ;
#2509 = CARTESIAN_POINT ( 'NONE',  ( 5.405949406249992428, -9.363379034771808662, -187.5937500020483810 ) ) ;
#2510 = CARTESIAN_POINT ( 'NONE',  ( -10.81189881249999907, -6.242252689847864744, -174.4687500020484094 ) ) ;
#2511 = CARTESIAN_POINT ( 'NONE',  ( -10.81189881249999907, -6.242252689847864744, -156.4687500020484379 ) ) ;
#2512 = CARTESIAN_POINT ( 'NONE',  ( -2.293366432827344421E-15, -12.48450537969573659, -169.7187500020483810 ) ) ;
#2513 = DIRECTION ( 'NONE',  ( -0.000000000000000000, -0.000000000000000000, 1.000000000000000000 ) ) ;
#2514 = LINE ( 'NONE', #13662, #3996 ) ;
#2515 = CARTESIAN_POINT ( 'NONE',  ( 9.999999999999998224, 0.000000000000000000, -192.5000000000000000 ) ) ;
#2516 = CARTESIAN_POINT ( 'NONE',  ( -10.81189881249999907, -6.242252689847864744, -106.9687500020483668 ) ) ;
#2517 = CARTESIAN_POINT ( 'NONE',  ( 9.999999999999998224, 0.000000000000000000, -84.49999999999997158 ) ) ;
#2518 = CARTESIAN_POINT ( 'NONE',  ( -10.81189881249999729, 6.242252689847871849, -75.90625000204838102 ) ) ;
#2519 = CARTESIAN_POINT ( 'NONE',  ( 5.405949406249999534, 9.363379034771803333, -89.59375000204838102 ) ) ;
#2520 = CARTESIAN_POINT ( 'NONE',  ( -10.81189881249999907, -6.242252689847864744, -59.15625000204838102 ) ) ;
#2521 = CARTESIAN_POINT ( 'NONE',  ( -10.00000000000000000, -5.773502691896251982, -148.5000000040967905 ) ) ;
#2522 = CARTESIAN_POINT ( 'NONE',  ( -4.999999999999996447, 8.660254037844387298, -120.0000000000000000 ) ) ;
#2523 = ADVANCED_FACE ( 'NONE', ( #29927 ), #10474, .F. ) ;
#2524 = ORIENTED_EDGE ( 'NONE', *, *, #8806, .T. ) ;
#2525 = CARTESIAN_POINT ( 'NONE',  ( -5.405949406250003975, -9.363379034771801557, -138.5312500020484094 ) ) ;
#2526 = CARTESIAN_POINT ( 'NONE',  ( -10.81189881249999729, 6.242252689847871849, -158.4062500020483810 ) ) ;
#2527 = CARTESIAN_POINT ( 'NONE',  ( 7.644554776091147741E-16, 12.48450537969573659, -199.1562500020484094 ) ) ;
#2528 = DIRECTION ( 'NONE',  ( -0.000000000000000000, -0.000000000000000000, 1.000000000000000000 ) ) ;
#2529 = CARTESIAN_POINT ( 'NONE',  ( 10.81189881249999907, 6.242252689847868297, -92.71875000204836681 ) ) ;
#2530 = ORIENTED_EDGE ( 'NONE', *, *, #4082, .F. ) ;
#2531 = CARTESIAN_POINT ( 'NONE',  ( -4.999999999999996447, 8.660254037844387298, -67.49999999999997158 ) ) ;
#2532 = CARTESIAN_POINT ( 'NONE',  ( -10.81189881249999729, 1.324075727343319199E-15, -185.0937500020483810 ) ) ;
#2533 = CARTESIAN_POINT ( 'NONE',  ( -9.999999999999998224, 5.773502691896259087, -72.25000000409676204 ) ) ;
#2534 = CARTESIAN_POINT ( 'NONE',  ( -4.999999999999996447, 8.660254037844387298, -165.0000000000000000 ) ) ;
#2535 = CARTESIAN_POINT ( 'NONE',  ( -5.000000000000003553, -8.660254037844383745, -145.0000000000000000 ) ) ;
#2536 = CARTESIAN_POINT ( 'NONE',  ( 5.405949406249999534, 9.363379034771803333, -95.78125000204838102 ) ) ;
#2537 = CARTESIAN_POINT ( 'NONE',  ( 10.81189881249999729, 0.000000000000000000, -64.53125000204836681 ) ) ;
#2538 = CARTESIAN_POINT ( 'NONE',  ( 7.070501591499377789E-16, 11.54700538379251284, -71.00000000409676204 ) ) ;
#2539 = DIRECTION ( 'NONE',  ( -0.000000000000000000, -0.000000000000000000, 1.000000000000000000 ) ) ;
#2540 = CARTESIAN_POINT ( 'NONE',  ( 10.81189881249999551, -6.242252689847874514, -22.46875000204837036 ) ) ;
#2541 = ORIENTED_EDGE ( 'NONE', *, *, #35673, .F. ) ;
#2542 = CARTESIAN_POINT ( 'NONE',  ( -10.81189881249999729, 1.324075727343319199E-15, -192.7812500020484094 ) ) ;
#2543 = CARTESIAN_POINT ( 'NONE',  ( -10.81189881249999907, -6.242252689847864744, -20.15625000204837747 ) ) ;
#2544 = CARTESIAN_POINT ( 'NONE',  ( -5.405949406249996869, 9.363379034771805109, -8.343750002048345493 ) ) ;
#2545 = DIRECTION ( 'NONE',  ( 0.000000000000000000, 0.000000000000000000, -1.000000000000000000 ) ) ;
#2546 = CARTESIAN_POINT ( 'NONE',  ( -9.999999999999479527, -5.773502691896549521, -37.50000000409674783 ) ) ;
#2547 = DIRECTION ( 'NONE',  ( -0.000000000000000000, -0.000000000000000000, 1.000000000000000000 ) ) ;
#2548 = CARTESIAN_POINT ( 'NONE',  ( -4.999999999999996447, 8.660254037844387298, -172.5000000000000284 ) ) ;
#2549 = DIRECTION ( 'NONE',  ( -0.000000000000000000, -0.000000000000000000, 1.000000000000000000 ) ) ;
#2551 = ORIENTED_EDGE ( 'NONE', *, *, #34353, .F. ) ;
#2550 = CARTESIAN_POINT ( 'NONE',  ( 10.81189881249999729, 0.000000000000000000, -99.03125000204839523 ) ) ;
#2552 = CARTESIAN_POINT ( 'NONE',  ( 42.00000000000004974, 0.000000000000000000, -219.9999999999999716 ) ) ;
#2553 = VERTEX_POINT ( 'NONE', #35975 ) ;
#2554 =( BOUNDED_CURVE ( )  B_SPLINE_CURVE ( 2, ( #40314, #23946, #27387, #7534, #40952, #20687, #33873 ),
 .UNSPECIFIED., .F., .F. ) 
 B_SPLINE_CURVE_WITH_KNOTS ( ( 3, 2, 2, 3 ),
 ( 0.3059701492537313383, 0.3072139303482587791, 0.3084577114427861644, 0.3097014925373136052 ),
 .UNSPECIFIED. ) 
 CURVE ( )  GEOMETRIC_REPRESENTATION_ITEM ( )  RATIONAL_B_SPLINE_CURVE ( ( 1.000000000000000000, 0.8660254037844387076, 1.000000000000000000, 0.8660254037844387076, 1.000000000000000000, 0.8660254037844207220, 1.000000000000017986 ) ) 
 REPRESENTATION_ITEM ( '' )  );
#2555 = ORIENTED_EDGE ( 'NONE', *, *, #33288, .F. ) ;
#2556 = CARTESIAN_POINT ( 'NONE',  ( 10.81189881249999907, 6.242252689847868297, -26.90625000204838102 ) ) ;
#2557 = CC_DESIGN_SECURITY_CLASSIFICATION ( #27695, ( #42694 ) ) ;
#2558 = ITEM_DEFINED_TRANSFORMATION ( 'NONE', 'NONE', #29709,  #39998 ) ;
#2559 = CARTESIAN_POINT ( 'NONE',  ( -10.81189881249999729, 6.242252689847871849, -80.21875000204838102 ) ) ;
#2560 = CARTESIAN_POINT ( 'NONE',  ( -9.999999999998969713, -5.773502691896847949, -4.500000004096739836 ) ) ;
#2561 = LINE ( 'NONE', #31489, #24582 ) ;
#2562 = CARTESIAN_POINT ( 'NONE',  ( 9.999999999999998224, 0.000000000000000000, -49.99999999999998579 ) ) ;
#2563 = CARTESIAN_POINT ( 'NONE',  ( -10.81189881249999729, 1.324075727343319199E-15, -159.7812500020484094 ) ) ;
#2564 = CARTESIAN_POINT ( 'NONE',  ( -9.999999999999998224, 5.773502691896259087, -7.750000004096748718 ) ) ;
#2565 = CARTESIAN_POINT ( 'NONE',  ( 9.999999999999998224, 0.000000000000000000, -159.8750000040967905 ) ) ;
#2566 = EDGE_CURVE ( 'NONE', #13495, #41596, #28008, .T. ) ;
#2567 = CARTESIAN_POINT ( 'NONE',  ( 7.644554776091147741E-16, 12.48450537969573659, -126.9687500020483668 ) ) ;
#2568 = CARTESIAN_POINT ( 'NONE',  ( 10.81189881249999729, 0.000000000000000000, -115.3437500020483810 ) ) ;
#2569 = CARTESIAN_POINT ( 'NONE',  ( -10.81189881249999729, 6.242252689847871849, -81.71875000204838102 ) ) ;
#2570 = CARTESIAN_POINT ( 'NONE',  ( 10.81189881249999729, 0.000000000000000000, -88.53125000204838102 ) ) ;
#2571 = CARTESIAN_POINT ( 'NONE',  ( 9.999999999999996447, -5.773502691896262640, -167.5000000040968189 ) ) ;
#2572 = DIRECTION ( 'NONE',  ( -0.000000000000000000, -0.000000000000000000, -1.000000000000000000 ) ) ;
#2573 = CARTESIAN_POINT ( 'NONE',  ( 10.81189881249999729, 6.242252689847867408, -166.4062500020483810 ) ) ;
#2574 = CARTESIAN_POINT ( 'NONE',  ( 10.81189881249999551, -6.242252689847874514, -183.1562500020484094 ) ) ;
#2575 = CARTESIAN_POINT ( 'NONE',  ( 10.81189881249999729, 0.000000000000000000, -46.34375000204838102 ) ) ;
#2576 = CARTESIAN_POINT ( 'NONE',  ( -5.000000000000003553, -8.660254037844383745, -163.3750000040967905 ) ) ;
#2577 = CARTESIAN_POINT ( 'NONE',  ( 10.81189881249999729, 0.000000000000000000, -3.031250002048374803 ) ) ;
#2578 = CARTESIAN_POINT ( 'NONE',  ( 7.644554776091147741E-16, 12.48450537969573659, -14.46875000204836503 ) ) ;
#2579 = CARTESIAN_POINT ( 'NONE',  ( -9.999999999999998224, 1.224646799147353059E-15, -84.12500000409677625 ) ) ;
#2580 = CARTESIAN_POINT ( 'NONE',  ( -10.81189881249999729, 6.242252689847871849, -116.2187500020483810 ) ) ;
#2581 = CARTESIAN_POINT ( 'NONE',  ( 9.999999999999996447, -5.773502691896262640, -92.12499999999998579 ) ) ;
#2582 = CARTESIAN_POINT ( 'NONE',  ( -10.81189881249999729, 1.324075727343319199E-15, -20.28125000204836326 ) ) ;
#2583 = CARTESIAN_POINT ( 'NONE',  ( -2.121150477449813534E-15, -11.54700538379251284, -97.25000000409679046 ) ) ;
#2584 = CARTESIAN_POINT ( 'NONE',  ( 0.000000000000000000, 0.000000000000000000, -200.0000000000000000 ) ) ;
#2585 = CARTESIAN_POINT ( 'NONE',  ( -10.81189881249999729, 6.242252689847871849, -114.9062500020483952 ) ) ;
#2586 = CARTESIAN_POINT ( 'NONE',  ( 5.405949406249999534, 9.363379034771803333, -91.28125000204838102 ) ) ;
#2587 = ORIENTED_EDGE ( 'NONE', *, *, #31975, .F. ) ;
#2588 = CARTESIAN_POINT ( 'NONE',  ( -10.00000000000000000, -5.773502691896251982, -93.00000000409679046 ) ) ;
#2589 = FACE_OUTER_BOUND ( 'NONE', #11013, .T. ) ;
#2590 = CARTESIAN_POINT ( 'NONE',  ( 7.644554776091147741E-16, 12.48450537969573659, -157.1562500020484094 ) ) ;
#2591 = CARTESIAN_POINT ( 'NONE',  ( 5.405949406249999534, 9.363379034771803333, -50.59375000204835260 ) ) ;
#2592 = VERTEX_POINT ( 'NONE', #20402 ) ;
#2593 = CARTESIAN_POINT ( 'NONE',  ( 7.070501591499377789E-16, 11.54700538379251284, -21.12499999999997158 ) ) ;
#2594 = CARTESIAN_POINT ( 'NONE',  ( -10.81189881249999729, -6.242252689847864744, -23.15625000204837747 ) ) ;
#2595 = CARTESIAN_POINT ( 'NONE',  ( 4.999999999999992006, -8.660254037844389075, -155.2500000000000000 ) ) ;
#2596 = CARTESIAN_POINT ( 'NONE',  ( 7.070501591499377789E-16, 11.54700538379251284, -23.00000000409677270 ) ) ;
#2597 =( BOUNDED_CURVE ( )  B_SPLINE_CURVE ( 2, ( #8920, #5042, #18405, #15791, #21648, #25543, #28354 ),
 .UNSPECIFIED., .F., .F. ) 
 B_SPLINE_CURVE_WITH_KNOTS ( ( 3, 2, 2, 3 ),
 ( 0.3395522388059703522, 0.3407960199004976820, 0.3420398009950250118, 0.3432835820895522860 ),
 .UNSPECIFIED. ) 
 CURVE ( )  GEOMETRIC_REPRESENTATION_ITEM ( )  RATIONAL_B_SPLINE_CURVE ( ( 0.9999999999999761302, 0.8660254037844625774, 1.000000000000000000, 0.8660254037844387076, 1.000000000000000000, 0.8660254037844327124, 1.000000000000005995 ) ) 
 REPRESENTATION_ITEM ( '' )  );
#2598 = DIRECTION ( 'NONE',  ( 0.08682659386424779191, -0.08682659386424779191, 0.9924325091389669673 ) ) ;
#2600 = VERTEX_POINT ( 'NONE', #42638 ) ;
#2599 = CARTESIAN_POINT ( 'NONE',  ( 5.405949406249999534, 9.363379034771803333, -124.2812500020483952 ) ) ;
#2601 = CARTESIAN_POINT ( 'NONE',  ( -9.999999999998456346, -5.773502691897145489, -13.12499999999992717 ) ) ;
#2602 = ORIENTED_EDGE ( 'NONE', *, *, #11918, .F. ) ;
#2603 = CARTESIAN_POINT ( 'NONE',  ( -10.81189881249999729, 6.242252689847871849, -56.40625000204837391 ) ) ;
#2604 = APPROVAL_STATUS ( 'not_yet_approved' ) ;
#2605 = CARTESIAN_POINT ( 'NONE',  ( 5.405949406249999534, 9.363379034771803333, -104.5937500020483810 ) ) ;
#2607 = ORIENTED_EDGE ( 'NONE', *, *, #22754, .T. ) ;
#2606 = ORIENTED_EDGE ( 'NONE', *, *, #105, .F. ) ;
#2608 = CARTESIAN_POINT ( 'NONE',  ( -9.999999999999998224, 1.224646799147353059E-15, -30.12500000409676204 ) ) ;
#2609 = CARTESIAN_POINT ( 'NONE',  ( -10.81189881249999729, 1.324075727343319199E-15, -152.0937500020483810 ) ) ;
#2610 = CARTESIAN_POINT ( 'NONE',  ( 7.644554776091147741E-16, 12.48450537969573659, -179.6562500020484094 ) ) ;
#2611 = CARTESIAN_POINT ( 'NONE',  ( 10.81189881249999551, -6.242252689847874514, -4.468750002048369474 ) ) ;
#2612 = CYLINDRICAL_SURFACE ( 'NONE', #26607, 9.999999999999998224 ) ;
#2613 = CARTESIAN_POINT ( 'NONE',  ( 5.405949406249999534, 9.363379034771803333, -142.0937500020483810 ) ) ;
#2614 = CARTESIAN_POINT ( 'NONE',  ( -5.405949406249996869, 9.363379034771805109, -105.8437500020483810 ) ) ;
#2615 = CARTESIAN_POINT ( 'NONE',  ( -7.071067811865477282, 7.071067811865471064, -200.0000000000000000 ) ) ;
#2616 = CARTESIAN_POINT ( 'NONE',  ( 7.644554776091147741E-16, 12.48450537969573659, -118.1562500020483952 ) ) ;
#2617 = CARTESIAN_POINT ( 'NONE',  ( 9.999999999999996447, -5.773502691896262640, -191.5000000040968189 ) ) ;
#2618 = CARTESIAN_POINT ( 'NONE',  ( -10.81189881249999729, -6.242252689847864744, -118.9687500020483810 ) ) ;
#2619 = CARTESIAN_POINT ( 'NONE',  ( -10.81189881249999729, 6.242252689847871849, -194.4062500020484094 ) ) ;
#2620 = CARTESIAN_POINT ( 'NONE',  ( -10.00000000000051337, 5.773502691895962435, -148.7500000040967620 ) ) ;
#2621 = CARTESIAN_POINT ( 'NONE',  ( -10.00000000000000000, -5.773502691896251982, -142.1250000000000000 ) ) ;
#2622 = CARTESIAN_POINT ( 'NONE',  ( -2.121150477449813534E-15, -11.54700538379251284, -11.37499999999996803 ) ) ;
#2623 = CARTESIAN_POINT ( 'NONE',  ( 5.405949406249999534, 9.363379034771803333, -65.59375000204836681 ) ) ;
#2624 = CARTESIAN_POINT ( 'NONE',  ( 10.81189881249999729, 0.000000000000000000, -58.34375000204835970 ) ) ;
#2625 = CARTESIAN_POINT ( 'NONE',  ( -4.999999999999996447, 8.660254037844387298, -189.3750000040967905 ) ) ;
#2626 = CARTESIAN_POINT ( 'NONE',  ( 10.81189881249999551, -6.242252689847874514, -28.65625000204838813 ) ) ;
#2627 = CARTESIAN_POINT ( 'NONE',  ( -10.81189881249999729, 6.242252689847871849, -36.71875000204835260 ) ) ;
#2628 = CARTESIAN_POINT ( 'NONE',  ( -4.999999999999996447, 8.660254037844387298, -148.8750000040967905 ) ) ;
#2629 = CARTESIAN_POINT ( 'NONE',  ( 5.405949406249992428, -9.363379034771808662, -147.0937500020483810 ) ) ;
#2630 = CARTESIAN_POINT ( 'NONE',  ( 7.070501591499377789E-16, 11.54700538379251284, -109.6249999999999858 ) ) ;
#2631 = AXIS2_PLACEMENT_3D ( 'NONE', #16316, #39632, #20426 ) ;
#2632 = EDGE_CURVE ( 'NONE', #24776, #23457, #28398, .T. ) ;
#2633 = DIRECTION ( 'NONE',  ( -1.000000000000000000, 0.000000000000000000, 0.000000000000000000 ) ) ;
#2634 = CARTESIAN_POINT ( 'NONE',  ( 9.999999999999996447, -5.773502691896262640, -69.62499999999998579 ) ) ;
#2635 = CARTESIAN_POINT ( 'NONE',  ( 10.81189881249999907, 6.242252689847868297, -142.4062500020484094 ) ) ;
#2636 = CARTESIAN_POINT ( 'NONE',  ( 7.644554776091147741E-16, 12.48450537969573659, -116.6562500020483952 ) ) ;
#2637 = ORIENTED_EDGE ( 'NONE', *, *, #16988, .T. ) ;
#2638 = CARTESIAN_POINT ( 'NONE',  ( -2.121150477449813534E-15, -11.54700538379251284, -118.2500000040968047 ) ) ;
#2639 = DIRECTION ( 'NONE',  ( 0.000000000000000000, 0.000000000000000000, -1.000000000000000000 ) ) ;
#2640 = CARTESIAN_POINT ( 'NONE',  ( 7.644554776091147741E-16, 12.48450537969573659, -75.96875000204838102 ) ) ;
#2641 = CARTESIAN_POINT ( 'NONE',  ( 9.999999999999998224, 0.000000000000000000, -37.99999999999997868 ) ) ;
#2642 = CARTESIAN_POINT ( 'NONE',  ( -5.000000000000003553, -8.660254037844383745, -28.37500000409676204 ) ) ;
#2643 = CARTESIAN_POINT ( 'NONE',  ( 10.81189881249999729, 6.242252689847867408, -50.90625000204838102 ) ) ;
#2644 = CARTESIAN_POINT ( 'NONE',  ( -5.000000000000003553, -8.660254037844383745, -157.3750000040967905 ) ) ;
#2645 = CARTESIAN_POINT ( 'NONE',  ( -10.81189881249999729, 1.324075727343319199E-15, -33.78125000204837391 ) ) ;
#2646 = CARTESIAN_POINT ( 'NONE',  ( -10.81189881249999729, 6.242252689847871849, -144.9062500020484094 ) ) ;
#2647 = CARTESIAN_POINT ( 'NONE',  ( -5.405949406249996869, 9.363379034771805109, -152.5312500020484094 ) ) ;
#2648 = CARTESIAN_POINT ( 'NONE',  ( 9.999999999999998224, 0.000000000000000000, -78.87500000409677625 ) ) ;
#2649 = DIRECTION ( 'NONE',  ( -1.000000000000000000, 0.000000000000000000, 0.000000000000000000 ) ) ;
#2650 = ORIENTED_EDGE ( 'NONE', *, *, #8291, .T. ) ;
#2651 = EDGE_LOOP ( 'NONE', ( #20661, #18080, #34460, #33121 ) ) ;
#2652 = EDGE_LOOP ( 'NONE', ( #37130, #21052, #35179, #1 ) ) ;
#2653 = AXIS2_PLACEMENT_3D ( 'NONE', #9552, #6531, #13193 ) ;
#2654 = CARTESIAN_POINT ( 'NONE',  ( -9.999999999999998224, 1.224646799147353059E-15, -200.0000000000000000 ) ) ;
#2655 = CARTESIAN_POINT ( 'NONE',  ( 10.81189881249999907, 6.242252689847868297, -182.7187500020484094 ) ) ;
#2656 = CARTESIAN_POINT ( 'NONE',  ( 10.81189881249999907, 6.242252689847868297, -28.21875000204838457 ) ) ;
#2657 = DIRECTION ( 'NONE',  ( -0.000000000000000000, -0.000000000000000000, 1.000000000000000000 ) ) ;
#2658 = CARTESIAN_POINT ( 'NONE',  ( 10.81189881249999551, -6.242252689847874514, -163.4687500020483810 ) ) ;
#2659 = CARTESIAN_POINT ( 'NONE',  ( 5.405949406249992428, -9.363379034771808662, -147.0937500020483810 ) ) ;
#2660 = FACE_OUTER_BOUND ( 'NONE', #12502, .T. ) ;
#2661 = CARTESIAN_POINT ( 'NONE',  ( 10.81189881249999907, 6.242252689847868297, -131.7187500020483810 ) ) ;
#2662 = CARTESIAN_POINT ( 'NONE',  ( 5.405949406249992428, -9.363379034771808662, -139.7812500020483810 ) ) ;
#2663 = CARTESIAN_POINT ( 'NONE',  ( 10.81189881249999907, 6.242252689847868297, -20.71875000204836681 ) ) ;
#2664 = CARTESIAN_POINT ( 'NONE',  ( -5.405949406250003975, -9.363379034771801557, -144.3437500020483810 ) ) ;
#2665 = FACE_OUTER_BOUND ( 'NONE', #18507, .T. ) ;
#2666 = CARTESIAN_POINT ( 'NONE',  ( 9.999999999999479527, 5.773502691896553074, -177.7500000040967620 ) ) ;
#2667 = CARTESIAN_POINT ( 'NONE',  ( -10.00000000000000000, -5.773502691896251982, -163.1250000000000284 ) ) ;
#2668 = CARTESIAN_POINT ( 'NONE',  ( -5.405949406249996869, 9.363379034771805109, -84.84375000204836681 ) ) ;
#2669 = CARTESIAN_POINT ( 'NONE',  ( 1.351487262974977233, 10.72709830801206543, -100.0000000000000000 ) ) ;
#2670 = CARTESIAN_POINT ( 'NONE',  ( -10.81189881249999729, 1.324075727343319199E-15, -53.28125000204836681 ) ) ;
#2671 = CARTESIAN_POINT ( 'NONE',  ( -10.81189881249999907, -6.242252689847864744, -61.96875000204838102 ) ) ;
#2672 = LINE ( 'NONE', #5911, #13671 ) ;
#2673 = CARTESIAN_POINT ( 'NONE',  ( 5.405949406249999534, 9.363379034771803333, -173.5937500020484094 ) ) ;
#2674 = CARTESIAN_POINT ( 'NONE',  ( -2.121150477449813534E-15, -11.54700538379251284, -140.3750000000000000 ) ) ;
#2675 = CARTESIAN_POINT ( 'NONE',  ( -10.81189881249999729, -6.242252689847864744, -146.1562500020484094 ) ) ;
#2676 = CARTESIAN_POINT ( 'NONE',  ( -9.999999999999998224, 1.224646799147353059E-15, -113.7499999999999858 ) ) ;
#2677 = CARTESIAN_POINT ( 'NONE',  ( -2.121150477449813534E-15, -11.54700538379251284, -119.7500000040967905 ) ) ;
#2678 = CARTESIAN_POINT ( 'NONE',  ( 4.999999999999992006, -8.660254037844389075, -89.24999999999998579 ) ) ;
#2679 = ORIENTED_EDGE ( 'NONE', *, *, #40709, .F. ) ;
#2680 = CARTESIAN_POINT ( 'NONE',  ( 5.405949406249992428, -9.363379034771808662, -115.7812500020483952 ) ) ;
#2681 = CARTESIAN_POINT ( 'NONE',  ( -9.999999999999998224, 1.224646799147353059E-15, -141.1250000040967905 ) ) ;
#2682 = CARTESIAN_POINT ( 'NONE',  ( 10.00000000000102318, -5.773502691895667560, -48.62499999999993605 ) ) ;
#2683 = CARTESIAN_POINT ( 'NONE',  ( -10.81189881249999729, 6.242252689847871849, -171.9062500020484094 ) ) ;
#2684 = CARTESIAN_POINT ( 'NONE',  ( -10.00000000000000000, -5.773502691896251982, -52.50000000409676915 ) ) ;
#2685 = ADVANCED_FACE ( 'NONE', ( #788 ), #13066, .F. ) ;
#2686 = AXIS2_PLACEMENT_3D ( 'NONE', #37107, #1080, #7551 ) ;
#2687 = CARTESIAN_POINT ( 'NONE',  ( 11.54700538379253416, -19.99999999999999289, 0.000000000000000000 ) ) ;
#2688 = CARTESIAN_POINT ( 'NONE',  ( 10.81189881249999551, -6.242252689847874514, -61.65625000204838813 ) ) ;
#2689 = CARTESIAN_POINT ( 'NONE',  ( 9.999999999998969713, 5.773502691896851502, -84.37499999999997158 ) ) ;
#2690 = CARTESIAN_POINT ( 'NONE',  ( -2.293366432827344421E-15, -12.48450537969573659, -169.9062500020483810 ) ) ;
#2691 = CARTESIAN_POINT ( 'NONE',  ( -9.999999999999872102, -5.773502691896326589, -163.1250000000000000 ) ) ;
#2692 = CARTESIAN_POINT ( 'NONE',  ( -9.999999999999998224, 1.224646799147353059E-15, -200.0000000000000000 ) ) ;
#2693 = EDGE_LOOP ( 'NONE', ( #37783, #7800, #33658, #3709 ) ) ;
#2694 = CARTESIAN_POINT ( 'NONE',  ( 10.00000000000012257, -5.773502691896187144, -194.1250000000000568 ) ) ;
#2695 = CARTESIAN_POINT ( 'NONE',  ( 0.000000000000000000, 0.000000000000000000, -99.99999999999998579 ) ) ;
#2697 = ORIENTED_EDGE ( 'NONE', *, *, #31089, .T. ) ;
#2696 = CARTESIAN_POINT ( 'NONE',  ( -5.405949406250003975, -9.363379034771801557, -80.03125000204838102 ) ) ;
#2699 = ORIENTED_EDGE ( 'NONE', *, *, #31320, .T. ) ;
#2698 = CARTESIAN_POINT ( 'NONE',  ( 10.00000000000051159, -5.773502691895965988, -119.1249999999999858 ) ) ;
#2700 = ORIENTED_EDGE ( 'NONE', *, *, #19452, .T. ) ;
#2701 =( BOUNDED_CURVE ( )  B_SPLINE_CURVE ( 2, ( #9844, #29924, #23022, #26677, #36175, #16514, #33384 ),
 .UNSPECIFIED., .F., .F. ) 
 B_SPLINE_CURVE_WITH_KNOTS ( ( 3, 2, 2, 3 ),
 ( 0.4067164179104478250, 0.4079601990049751548, 0.4092039800995025400, 0.4104477611940299253 ),
 .UNSPECIFIED. ) 
 CURVE ( )  GEOMETRIC_REPRESENTATION_ITEM ( )  RATIONAL_B_SPLINE_CURVE ( ( 0.9999999999999940048, 0.8660254037844447028, 1.000000000000000000, 0.8660254037844387076, 1.000000000000000000, 0.8660254037844327124, 1.000000000000005995 ) ) 
 REPRESENTATION_ITEM ( '' )  );
#2702 = CARTESIAN_POINT ( 'NONE',  ( -10.81189881249999729, -6.242252689847864744, -25.96875000204837391 ) ) ;
#2703 = DIRECTION ( 'NONE',  ( 0.000000000000000000, 0.000000000000000000, -1.000000000000000000 ) ) ;
#2704 = CARTESIAN_POINT ( 'NONE',  ( -10.81189881249999729, 6.242252689847871849, -5.406250002048357928 ) ) ;
#2706 = ORIENTED_EDGE ( 'NONE', *, *, #20138, .F. ) ;
#2705 = CARTESIAN_POINT ( 'NONE',  ( -5.405949406250003975, -9.363379034771801557, -57.34375000204835970 ) ) ;
#2707 = FACE_OUTER_BOUND ( 'NONE', #8962, .T. ) ;
#2708 = CARTESIAN_POINT ( 'NONE',  ( 9.999999999999998224, 0.000000000000000000, -31.99999999999997158 ) ) ;
#2709 = CARTESIAN_POINT ( 'NONE',  ( 5.405949406249999534, 9.363379034771803333, -190.0937500020483810 ) ) ;
#2710 = CARTESIAN_POINT ( 'NONE',  ( -5.405949406250003975, -9.363379034771801557, -180.3437500020483810 ) ) ;
#2711 = CARTESIAN_POINT ( 'NONE',  ( -10.81189881249999907, -6.242252689847864744, -157.9687500020484379 ) ) ;
#2712 = CARTESIAN_POINT ( 'NONE',  ( 10.81189881249999729, 6.242252689847867408, -170.7187500020483810 ) ) ;
#2713 = CARTESIAN_POINT ( 'NONE',  ( -9.999999999999998224, 1.224646799147353059E-15, -200.0000000000000000 ) ) ;
#2714 = DIRECTION ( 'NONE',  ( -0.000000000000000000, -0.000000000000000000, -1.000000000000000000 ) ) ;
#2715 = CARTESIAN_POINT ( 'NONE',  ( -10.00000000000000000, -5.773502691896251982, -187.1250000000000284 ) ) ;
#2716 = AXIS2_PLACEMENT_3D ( 'NONE', #32719, #9196, #2730 ) ;
#2717 = CARTESIAN_POINT ( 'NONE',  ( -2.293366432827344421E-15, -12.48450537969573659, -108.2187500020483668 ) ) ;
#2718 = CARTESIAN_POINT ( 'NONE',  ( -9.999999999999998224, 1.224646799147353059E-15, -61.62500000409676204 ) ) ;
#2719 = CARTESIAN_POINT ( 'NONE',  ( 7.644554776091147741E-16, 12.48450537969573659, -73.15625000204836681 ) ) ;
#2720 = CARTESIAN_POINT ( 'NONE',  ( -4.999999999999996447, 8.660254037844387298, -88.87500000409677625 ) ) ;
#2721 = CARTESIAN_POINT ( 'NONE',  ( -5.405949406249996869, 9.363379034771805109, -87.84375000204836681 ) ) ;
#2722 = CARTESIAN_POINT ( 'NONE',  ( 10.81189881249999729, 0.000000000000000000, -60.03125000204836681 ) ) ;
#2723 = CARTESIAN_POINT ( 'NONE',  ( 7.070501591499377789E-16, 11.54700538379251284, -146.0000000040967905 ) ) ;
#2724 = CARTESIAN_POINT ( 'NONE',  ( -9.999999999999998224, 5.773502691896259087, -125.8749999999999858 ) ) ;
#2725 = ORIENTED_EDGE ( 'NONE', *, *, #651, .F. ) ;
#2726 = AXIS2_PLACEMENT_3D ( 'NONE', #867, #39910, #20909 ) ;
#2727 = CARTESIAN_POINT ( 'NONE',  ( -10.81189881249999729, 1.324075727343319199E-15, -140.2812500020483810 ) ) ;
#2728 = CARTESIAN_POINT ( 'NONE',  ( 7.644554776091147741E-16, 12.48450537969573659, -160.1562500020484094 ) ) ;
#2729 = CARTESIAN_POINT ( 'NONE',  ( 10.81189881249999551, -6.242252689847874514, -196.6562500020484379 ) ) ;
#2730 = DIRECTION ( 'NONE',  ( -1.000000000000000000, 0.000000000000000000, 0.000000000000000000 ) ) ;
#2731 = CARTESIAN_POINT ( 'NONE',  ( -2.293366432827344421E-15, -12.48450537969573659, -91.71875000204838102 ) ) ;
#2733 = ORIENTED_EDGE ( 'NONE', *, *, #18814, .T. ) ;
#2732 = EDGE_CURVE ( 'NONE', #23382, #12287, #31420, .T. ) ;
#2734 = CARTESIAN_POINT ( 'NONE',  ( 9.999999999999998224, 0.000000000000000000, -63.49999999999997158 ) ) ;
#2735 = CARTESIAN_POINT ( 'NONE',  ( -5.405949406250003975, -9.363379034771801557, -186.3437500020483810 ) ) ;
#2736 = CARTESIAN_POINT ( 'NONE',  ( -9.999999999999998224, 5.773502691896259087, -70.75000000409677625 ) ) ;
#2737 = ADVANCED_FACE ( 'NONE', ( #36598 ), #13279, .T. ) ;
#2738 = EDGE_CURVE ( 'NONE', #11060, #7201, #24090, .T. ) ;
#2739 = LINE ( 'NONE', #35760, #13424 ) ;
#2740 = CARTESIAN_POINT ( 'NONE',  ( 0.000000000000000000, 0.000000000000000000, -200.0000000000000000 ) ) ;
#2741 = CARTESIAN_POINT ( 'NONE',  ( 5.405949406249999534, 9.363379034771803333, -88.28125000204838102 ) ) ;
#2742 = CARTESIAN_POINT ( 'NONE',  ( -5.405949406250003975, -9.363379034771801557, -65.03125000204838102 ) ) ;
#2743 = EDGE_CURVE ( 'NONE', #35200, #17857, #10710, .T. ) ;
#2744 = CARTESIAN_POINT ( 'NONE',  ( -5.000000000000003553, -8.660254037844383745, -59.87500000409676204 ) ) ;
#2745 = CARTESIAN_POINT ( 'NONE',  ( 5.405949406249999534, 9.363379034771803333, -14.59375000204835082 ) ) ;
#2746 = ORIENTED_EDGE ( 'NONE', *, *, #1154, .F. ) ;
#2747 = CARTESIAN_POINT ( 'NONE',  ( -2.293366432827344421E-15, -12.48450537969573659, -190.9062500020483810 ) ) ;
#2748 = CARTESIAN_POINT ( 'NONE',  ( -10.81189881249999907, -6.242252689847864744, -15.65625000204837214 ) ) ;
#2749 = CARTESIAN_POINT ( 'NONE',  ( -5.405949406250003975, -9.363379034771801557, -1.843750002048366587 ) ) ;
#2750 = CARTESIAN_POINT ( 'NONE',  ( 9.999999999999998224, 0.000000000000000000, -186.8750000040967905 ) ) ;
#2751 = CARTESIAN_POINT ( 'NONE',  ( 10.00000000000038014, -5.773502691896040595, -180.6250000000000284 ) ) ;
#2752 = CC_DESIGN_DATE_AND_TIME_ASSIGNMENT ( #33445, #10749, ( #4933 ) ) ;
#2753 = LINE ( 'NONE', #26052, #5936 ) ;
#2754 = CARTESIAN_POINT ( 'NONE',  ( 9.999999999999998224, 0.000000000000000000, -174.5000000000000284 ) ) ;
#2755 = CARTESIAN_POINT ( 'NONE',  ( 4.999999999999992006, -8.660254037844389075, -36.74999999999997868 ) ) ;
#2756 = AXIS2_PLACEMENT_3D ( 'NONE', #17575, #18008, #41089 ) ;
#2758 = ORIENTED_EDGE ( 'NONE', *, *, #29095, .T. ) ;
#2757 = CARTESIAN_POINT ( 'NONE',  ( 5.405949406249999534, 9.363379034771803333, -101.7812500020483952 ) ) ;
#2759 = DIRECTION ( 'NONE',  ( -0.000000000000000000, -0.000000000000000000, 1.000000000000000000 ) ) ;
#2760 = ORIENTED_EDGE ( 'NONE', *, *, #35064, .F. ) ;
#2761 = ORIENTED_EDGE ( 'NONE', *, *, #34676, .F. ) ;
#2762 = CARTESIAN_POINT ( 'NONE',  ( -5.405949406249996869, 9.363379034771805109, -31.03125000204837036 ) ) ;
#2763 = ITEM_DEFINED_TRANSFORMATION ( 'NONE', 'NONE', #35920,  #39998 ) ;
#2764 = EDGE_CURVE ( 'NONE', #933, #20180, #8329, .T. ) ;
#2765 = CARTESIAN_POINT ( 'NONE',  ( -2.293366432827344421E-15, -12.48450537969573659, -76.71875000204838102 ) ) ;
#2766 = CARTESIAN_POINT ( 'NONE',  ( -5.000000000000003553, -8.660254037844383745, -4.375000004096768258 ) ) ;
#2767 = CARTESIAN_POINT ( 'NONE',  ( -9.999999999999998224, 1.224646799147353059E-15, -148.6250000040967905 ) ) ;
#2768 = CARTESIAN_POINT ( 'NONE',  ( 9.999999999999998224, 0.000000000000000000, -126.8750000040967905 ) ) ;
#2769 = CARTESIAN_POINT ( 'NONE',  ( -9.999999999999998224, 1.224646799147353059E-15, -128.7499999999999716 ) ) ;
#2770 = CARTESIAN_POINT ( 'NONE',  ( -5.405949406249996869, 9.363379034771805109, -160.0312500020484094 ) ) ;
#2771 = CARTESIAN_POINT ( 'NONE',  ( 10.00000000000000000, 5.773502691896255534, -11.25000000409676559 ) ) ;
#2772 = CARTESIAN_POINT ( 'NONE',  ( -2.121150477449813534E-15, -11.54700538379251284, -125.3749999999999858 ) ) ;
#2773 = CARTESIAN_POINT ( 'NONE',  ( -2.293366432827344421E-15, -12.48450537969573659, -132.2187500020483810 ) ) ;
#2774 = CARTESIAN_POINT ( 'NONE',  ( 5.405949406249992428, -9.363379034771808662, -99.28125000204839523 ) ) ;
#2775 = CARTESIAN_POINT ( 'NONE',  ( -10.81189881249999729, -6.242252689847864744, -112.9687500020483810 ) ) ;
#2776 = EDGE_CURVE ( 'NONE', #32481, #2118, #24311, .T. ) ;
#2777 = CARTESIAN_POINT ( 'NONE',  ( 10.81189881249999907, 6.242252689847868297, -79.21875000204838102 ) ) ;
#2778 = CARTESIAN_POINT ( 'NONE',  ( 5.405949406249992428, -9.363379034771808662, -81.28125000204839523 ) ) ;
#2779 = CARTESIAN_POINT ( 'NONE',  ( 5.000000000000000000, 8.660254037844385522, -171.6250000040968189 ) ) ;
#2780 = CYLINDRICAL_SURFACE ( 'NONE', #37877, 9.999999999999998224 ) ;
#2781 = CARTESIAN_POINT ( 'NONE',  ( 5.405949406249992428, -9.363379034771808662, -169.7812500020484094 ) ) ;
#2782 = CARTESIAN_POINT ( 'NONE',  ( 5.405949406249999534, 9.363379034771803333, -178.2812500020484094 ) ) ;
#2783 = CARTESIAN_POINT ( 'NONE',  ( 4.999999999999992006, -8.660254037844389075, -152.6250000040967905 ) ) ;
#2784 = CARTESIAN_POINT ( 'NONE',  ( 7.644554776091147741E-16, 12.48450537969573659, -4.156250002048351710 ) ) ;
#2785 = CARTESIAN_POINT ( 'NONE',  ( 7.644554776091147741E-16, 12.48450537969573659, -2.468750002048353043 ) ) ;
#2786 = CARTESIAN_POINT ( 'NONE',  ( -4.999999999999996447, 8.660254037844387298, -5.999999999999977796 ) ) ;
#2787 = CARTESIAN_POINT ( 'NONE',  ( -10.81189881249999729, 6.242252689847871849, -110.2187500020483810 ) ) ;
#2788 = CARTESIAN_POINT ( 'NONE',  ( -4.999999999999996447, 8.660254037844387298, -89.99999999999998579 ) ) ;
#2789 = CARTESIAN_POINT ( 'NONE',  ( -10.81189881249999729, 6.242252689847871849, -15.90625000204837036 ) ) ;
#2790 = CARTESIAN_POINT ( 'NONE',  ( 5.000000000000000000, 8.660254037844385522, -99.62500000409679046 ) ) ;
#2791 = CARTESIAN_POINT ( 'NONE',  ( 5.000000000000000000, 8.660254037844385522, -150.6250000040967905 ) ) ;
#2792 = CARTESIAN_POINT ( 'NONE',  ( 10.81189881249999907, 6.242252689847868297, -107.9062500020483668 ) ) ;
#2793 = CARTESIAN_POINT ( 'NONE',  ( -10.81189881249999729, 1.324075727343319199E-15, -93.78125000204838102 ) ) ;
#2794 = ORIENTED_EDGE ( 'NONE', *, *, #26453, .F. ) ;
#2795 = CARTESIAN_POINT ( 'NONE',  ( -4.999999999999996447, 8.660254037844387298, -82.87500000409676204 ) ) ;
#2796 = CARTESIAN_POINT ( 'NONE',  ( -5.000000000000003553, -8.660254037844383745, -101.5000000000000000 ) ) ;
#2797 = CARTESIAN_POINT ( 'NONE',  ( 5.405949406249992428, -9.363379034771808662, -40.59375000204837391 ) ) ;
#2798 = ORIENTED_EDGE ( 'NONE', *, *, #29945, .T. ) ;
#2799 = CARTESIAN_POINT ( 'NONE',  ( -4.999999999999996447, 8.660254037844387298, -19.49999999999996092 ) ) ;
#2800 = PRODUCT ( 'thrust bolt', 'thrust bolt', '', ( #1706 ) ) ;
#2801 = CARTESIAN_POINT ( 'NONE',  ( -9.999999999999998224, 1.224646799147353059E-15, -155.7500000000000000 ) ) ;
#2802 =( BOUNDED_CURVE ( )  B_SPLINE_CURVE ( 2, ( #16105, #35577, #22400, #35366, #38586, #4998, #32132 ),
 .UNSPECIFIED., .F., .F. ) 
 B_SPLINE_CURVE_WITH_KNOTS ( ( 3, 2, 2, 3 ),
 ( 0.8358208955223882519, 0.8370646766169156372, 0.8383084577114430225, 0.8395522388059704078 ),
 .UNSPECIFIED. ) 
 CURVE ( )  GEOMETRIC_REPRESENTATION_ITEM ( )  RATIONAL_B_SPLINE_CURVE ( ( 0.9999999999999761302, 0.8660254037844625774, 1.000000000000000000, 0.8660254037844387076, 1.000000000000000000, 0.8660254037844148378, 1.000000000000023981 ) ) 
 REPRESENTATION_ITEM ( '' )  );
#2803 = CARTESIAN_POINT ( 'NONE',  ( 4.999999999999992006, -8.660254037844389075, -17.62500000409675138 ) ) ;
#2804 = CARTESIAN_POINT ( 'NONE',  ( -10.00000000000000000, -5.773502691896251982, -196.1250000000000568 ) ) ;
#2805 = EDGE_CURVE ( 'NONE', #4916, #2592, #4676, .T. ) ;
#2807 = EDGE_LOOP ( 'NONE', ( #32693, #5933, #28776, #13228 ) ) ;
#2806 = CARTESIAN_POINT ( 'NONE',  ( 5.405949406249992428, -9.363379034771808662, -127.7812500020483810 ) ) ;
#2808 = CARTESIAN_POINT ( 'NONE',  ( 5.000000000000000000, 8.660254037844385522, -90.24999999999998579 ) ) ;
#2809 = ORIENTED_EDGE ( 'NONE', *, *, #37458, .T. ) ;
#2810 = CARTESIAN_POINT ( 'NONE',  ( -10.81189881249999907, -6.242252689847864744, -51.65625000204838102 ) ) ;
#2811 = CALENDAR_DATE ( 2026, 28, 9 ) ;
#2812 = CARTESIAN_POINT ( 'NONE',  ( -10.81189881249999907, -6.242252689847864744, -103.9687500020483668 ) ) ;
#2814 = ORIENTED_EDGE ( 'NONE', *, *, #14112, .F. ) ;
#2813 = ORIENTED_EDGE ( 'NONE', *, *, #21859, .F. ) ;
#2815 = CARTESIAN_POINT ( 'NONE',  ( -2.121150477449813534E-15, -11.54700538379251284, -175.2500000040968189 ) ) ;
#2816 = CARTESIAN_POINT ( 'NONE',  ( 7.070501591499376803E-16, 11.54700538379251284, -33.12499999999996447 ) ) ;
#2817 = CARTESIAN_POINT ( 'NONE',  ( 10.81189881249999907, 6.242252689847868297, -184.4062500020484094 ) ) ;
#2818 = CARTESIAN_POINT ( 'NONE',  ( -5.405949406249996869, 9.363379034771805109, 0.6562499979516356330 ) ) ;
#2819 = DIRECTION ( 'NONE',  ( -1.000000000000000000, 0.000000000000000000, 0.000000000000000000 ) ) ;
#2820 = CARTESIAN_POINT ( 'NONE',  ( -10.81189881249999729, 1.324075727343319199E-15, -140.0937500020483810 ) ) ;
#2821 = CARTESIAN_POINT ( 'NONE',  ( 5.405949406249992428, -9.363379034771808662, -103.5937500020483668 ) ) ;
#2822 = CARTESIAN_POINT ( 'NONE',  ( 9.999999999999998224, 0.000000000000000000, -113.3750000040967763 ) ) ;
#2823 = CARTESIAN_POINT ( 'NONE',  ( 7.644554776091147741E-16, 12.48450537969573659, -106.1562500020483952 ) ) ;
#2824 = CARTESIAN_POINT ( 'NONE',  ( -9.999999999999998224, 1.224646799147353059E-15, -196.6250000040967905 ) ) ;
#2825 = CARTESIAN_POINT ( 'NONE',  ( -5.405949406250003975, -9.363379034771801557, -118.8437500020483810 ) ) ;
#2826 = CARTESIAN_POINT ( 'NONE',  ( 10.81189881249999729, 0.000000000000000000, -186.0312500020484094 ) ) ;
#2827 = DIRECTION ( 'NONE',  ( 1.000000000000000000, 0.000000000000000000, 0.000000000000000000 ) ) ;
#2828 = CARTESIAN_POINT ( 'NONE',  ( -4.999999999999996447, 8.660254037844387298, -138.0000000000000000 ) ) ;
#2829 = CARTESIAN_POINT ( 'NONE',  ( -2.121150477449813534E-15, -11.54700538379251284, -5.374999999999963585 ) ) ;
#2830 = CARTESIAN_POINT ( 'NONE',  ( 5.405949406249999534, 9.363379034771803333, -67.09375000204836681 ) ) ;
#2831 = CARTESIAN_POINT ( 'NONE',  ( 10.81189881249999907, 6.242252689847868297, -46.21875000204837391 ) ) ;
#2832 = CARTESIAN_POINT ( 'NONE',  ( -9.999999999999998224, 1.224646799147353059E-15, -177.1250000040968189 ) ) ;
#2833 = CARTESIAN_POINT ( 'NONE',  ( 10.81189881249999551, -6.242252689847874514, -27.15625000204838102 ) ) ;
#2834 = CARTESIAN_POINT ( 'NONE',  ( -2.293366432827344421E-15, -12.48450537969573659, -31.71875000204834905 ) ) ;
#2835 = DIRECTION ( 'NONE',  ( 0.000000000000000000, 0.000000000000000000, 1.000000000000000000 ) ) ;
#2836 = CARTESIAN_POINT ( 'NONE',  ( -5.405949406250003975, -9.363379034771801557, -135.3437500020484094 ) ) ;
#2837 = CARTESIAN_POINT ( 'NONE',  ( -4.999999999999996447, 8.660254037844387298, -110.9999999999999858 ) ) ;
#2838 = CARTESIAN_POINT ( 'NONE',  ( -10.00000000000012434, 5.773502691896184480, -163.3750000000000000 ) ) ;
#2839 = CARTESIAN_POINT ( 'NONE',  ( -2.121150477449813534E-15, -11.54700538379251284, -66.87499999999998579 ) ) ;
#2840 = CARTESIAN_POINT ( 'NONE',  ( -2.293366432827344421E-15, -12.48450537969573659, -142.9062500020483810 ) ) ;
#2841 = CARTESIAN_POINT ( 'NONE',  ( 5.405949406249999534, 9.363379034771803333, -118.2812500020483952 ) ) ;
#2842 = EDGE_LOOP ( 'NONE', ( #40100, #1900, #35411, #10533 ) ) ;
#2843 =( BOUNDED_CURVE ( )  B_SPLINE_CURVE ( 2, ( #38433, #11881, #28306, #35211, #25499, #5641, #21820 ),
 .UNSPECIFIED., .F., .F. ) 
 B_SPLINE_CURVE_WITH_KNOTS ( ( 3, 2, 2, 3 ),
 ( 0.2425373134328359381, 0.2437810945273632957, 0.2450248756218906532, 0.2462686567164180107 ),
 .UNSPECIFIED. ) 
 CURVE ( )  GEOMETRIC_REPRESENTATION_ITEM ( )  RATIONAL_B_SPLINE_CURVE ( ( 0.9999999999999880096, 0.8660254037844506980, 1.000000000000000000, 0.8660254037844387076, 1.000000000000000000, 0.8660254037844267172, 1.000000000000011990 ) ) 
 REPRESENTATION_ITEM ( '' )  );
#2844 = FACE_OUTER_BOUND ( 'NONE', #29189, .T. ) ;
#2845 = CARTESIAN_POINT ( 'NONE',  ( 4.999999999999992006, -8.660254037844389075, -115.1250000040967905 ) ) ;
#2846 = CARTESIAN_POINT ( 'NONE',  ( 7.070501591499376803E-16, 11.54700538379251284, -169.6250000000000000 ) ) ;
#2847 = CARTESIAN_POINT ( 'NONE',  ( 7.644554776091147741E-16, 12.48450537969573659, -62.46875000204838102 ) ) ;
#2848 = CARTESIAN_POINT ( 'NONE',  ( 4.999999999999992006, -8.660254037844389075, -44.24999999999998579 ) ) ;
#2849 = PRODUCT_DEFINITION_FORMATION_WITH_SPECIFIED_SOURCE ( 'ANY', '', #31497, .NOT_KNOWN. ) ;
#2850 = CARTESIAN_POINT ( 'NONE',  ( -2.121150477449813534E-15, -11.54700538379251284, -25.25000000409676559 ) ) ;
#2851 = CARTESIAN_POINT ( 'NONE',  ( 5.405949406249992428, -9.363379034771808662, -40.78125000204838102 ) ) ;
#2852 = CARTESIAN_POINT ( 'NONE',  ( 9.999999999999998224, 0.000000000000000000, -168.8750000040967905 ) ) ;
#2853 = CARTESIAN_POINT ( 'NONE',  ( -10.00000000000000000, -5.773502691896251982, -42.00000000409675494 ) ) ;
#2854 = CARTESIAN_POINT ( 'NONE',  ( -10.81189881249999907, -6.242252689847864744, -33.65625000204835970 ) ) ;
#2855 =( BOUNDED_CURVE ( )  B_SPLINE_CURVE ( 2, ( #4115, #33482, #33051, #13799, #6713, #885, #23118 ),
 .UNSPECIFIED., .F., .F. ) 
 B_SPLINE_CURVE_WITH_KNOTS ( ( 3, 2, 2, 3 ),
 ( 0.01865671641791046345, 0.01990049751243783138, 0.02114427860696519584, 0.02238805970149256030 ),
 .UNSPECIFIED. ) 
 CURVE ( )  GEOMETRIC_REPRESENTATION_ITEM ( )  RATIONAL_B_SPLINE_CURVE ( ( 0.9999999999999981126, 0.8660254037844405950, 1.000000000000000000, 0.8660254037844387076, 1.000000000000000000, 0.8660254037844360431, 1.000000000000002665 ) ) 
 REPRESENTATION_ITEM ( '' )  );
#2856 = CARTESIAN_POINT ( 'NONE',  ( 5.000000000000000000, 8.660254037844385522, -166.7500000000000000 ) ) ;
#2857 = CARTESIAN_POINT ( 'NONE',  ( -5.405949406249996869, 9.363379034771805109, -134.5312500020484094 ) ) ;
#2858 = EDGE_CURVE ( 'NONE', #23382, #9326, #21044, .T. ) ;
#2859 = CARTESIAN_POINT ( 'NONE',  ( 10.81189881249999907, 6.242252689847868297, -148.4062500020484094 ) ) ;
#2860 = LINE ( 'NONE', #3708, #10013 ) ;
#2861 = ORIENTED_EDGE ( 'NONE', *, *, #19230, .F. ) ;
#2862 = ORIENTED_EDGE ( 'NONE', *, *, #7910, .F. ) ;
#2863 = ORIENTED_EDGE ( 'NONE', *, *, #39892, .T. ) ;
#2864 = ADVANCED_FACE ( 'NONE', ( #37885 ), #20831, .F. ) ;
#2865 = VECTOR ( 'NONE', #1147, 1000.000000000000000 ) ;
#2866 = CARTESIAN_POINT ( 'NONE',  ( 9.999999999999998224, 0.000000000000000000, -135.8750000040967905 ) ) ;
#2867 = CARTESIAN_POINT ( 'NONE',  ( 10.81189881249999907, 6.242252689847868297, -176.7187500020483810 ) ) ;
#2868 = CC_DESIGN_APPROVAL ( #37034, ( #3281 ) ) ;
#2869 = CARTESIAN_POINT ( 'NONE',  ( -2.293366432827344421E-15, -12.48450537969573659, -33.21875000204834549 ) ) ;
#2870 = LINE ( 'NONE', #26168, #1960 ) ;
#2871 = CARTESIAN_POINT ( 'NONE',  ( 10.81189881249999729, 6.242252689847867408, -164.7187500020483810 ) ) ;
#2872 = CARTESIAN_POINT ( 'NONE',  ( 10.81189881249999551, -6.242252689847874514, -148.4687500020484094 ) ) ;
#2873 = FACE_OUTER_BOUND ( 'NONE', #42621, .T. ) ;
#2874 = CARTESIAN_POINT ( 'NONE',  ( 10.81189881249999551, -6.242252689847874514, -127.4687500020483810 ) ) ;
#2875 = CARTESIAN_POINT ( 'NONE',  ( 5.405949406249992428, -9.363379034771808662, -130.7812500020483810 ) ) ;
#2876 = CARTESIAN_POINT ( 'NONE',  ( -5.405949406249996869, 9.363379034771805109, -15.84375000204835082 ) ) ;
#2877 = CARTESIAN_POINT ( 'NONE',  ( 10.81189881249999729, 0.000000000000000000, -148.3437500020483810 ) ) ;
#2878 = CARTESIAN_POINT ( 'NONE',  ( 10.75125155253628684, -1.347400678069339497, -179.9999999999999716 ) ) ;
#2879 = CARTESIAN_POINT ( 'NONE',  ( 7.070501591499376803E-16, 11.54700538379251284, -25.62499999999997868 ) ) ;
#2880 = CARTESIAN_POINT ( 'NONE',  ( -9.999999999999998224, 5.773502691896259087, -163.3750000000000000 ) ) ;
#2881 = VECTOR ( 'NONE', #271, 1000.000000000000000 ) ;
#2882 = CARTESIAN_POINT ( 'NONE',  ( -10.81189881249999907, -6.242252689847864744, -73.96875000204836681 ) ) ;
#2883 = CARTESIAN_POINT ( 'NONE',  ( 7.644554776091147741E-16, 12.48450537969573659, -50.65625000204838102 ) ) ;
#2884 = CARTESIAN_POINT ( 'NONE',  ( 10.81189881249999551, -6.242252689847874514, -61.46875000204837391 ) ) ;
#2885 = CARTESIAN_POINT ( 'NONE',  ( 9.999999999999998224, 0.000000000000000000, -174.5000000000000284 ) ) ;
#2886 = CARTESIAN_POINT ( 'NONE',  ( 10.81189881249999907, 6.242252689847868297, -161.7187500020483810 ) ) ;
#2887 = CARTESIAN_POINT ( 'NONE',  ( 7.070501591499377789E-16, 11.54700538379251284, -133.6250000000000000 ) ) ;
#2888 = CARTESIAN_POINT ( 'NONE',  ( 10.81189881249999729, 6.242252689847867408, -146.9062500020484379 ) ) ;
#2889 = DIRECTION ( 'NONE',  ( -0.000000000000000000, -0.000000000000000000, -1.000000000000000000 ) ) ;
#2890 = CARTESIAN_POINT ( 'NONE',  ( 5.000000000000000000, 8.660254037844385522, -119.1250000040967905 ) ) ;
#2891 = CARTESIAN_POINT ( 'NONE',  ( 5.000000000000000000, 8.660254037844385522, -88.74999999999998579 ) ) ;
#2892 = ORIENTED_EDGE ( 'NONE', *, *, #33101, .F. ) ;
#2893 = CARTESIAN_POINT ( 'NONE',  ( -10.81189881249999729, 6.242252689847871849, -119.4062500020483952 ) ) ;
#2894 = CARTESIAN_POINT ( 'NONE',  ( -4.999999999999996447, 8.660254037844387298, -139.8750000040968189 ) ) ;
#2895 = EDGE_CURVE ( 'NONE', #2913, #27845, #40667, .T. ) ;
#2896 = CARTESIAN_POINT ( 'NONE',  ( 10.81189881249999907, 6.242252689847868297, -170.9062500020484094 ) ) ;
#2897 = CARTESIAN_POINT ( 'NONE',  ( -4.999999999999996447, 8.660254037844387298, -51.37500000409675494 ) ) ;
#2898 = CARTESIAN_POINT ( 'NONE',  ( -9.999999999999998224, 1.224646799147353059E-15, -91.62500000409677625 ) ) ;
#2899 = CARTESIAN_POINT ( 'NONE',  ( 10.81189881249999907, 6.242252689847868297, -58.40625000204838102 ) ) ;
#2900 = VECTOR ( 'NONE', #23093, 1000.000000000000000 ) ;
#2901 = EDGE_CURVE ( 'NONE', #34857, #5520, #8109, .T. ) ;
#2902 = LINE ( 'NONE', #29227, #32461 ) ;
#2903 = CARTESIAN_POINT ( 'NONE',  ( 10.81189881249999551, -6.242252689847874514, -160.6562500020484379 ) ) ;
#2904 = CARTESIAN_POINT ( 'NONE',  ( -5.405949406250003975, -9.363379034771801557, -141.3437500020483810 ) ) ;
#2905 = DIRECTION ( 'NONE',  ( 0.000000000000000000, 1.000000000000000000, 0.000000000000000000 ) ) ;
#2906 = CARTESIAN_POINT ( 'NONE',  ( -10.00000000000051337, 5.773502691895962435, -79.75000000409677625 ) ) ;
#2907 = ORIENTED_EDGE ( 'NONE', *, *, #27941, .F. ) ;
#2908 = CARTESIAN_POINT ( 'NONE',  ( -9.999999999999996447, 5.773502691896259975, -172.7500000040967905 ) ) ;
#2910 = ORIENTED_EDGE ( 'NONE', *, *, #30528, .T. ) ;
#2909 = CARTESIAN_POINT ( 'NONE',  ( 10.81189881249999551, -6.242252689847874514, -66.15625000204839523 ) ) ;
#2911 = PERSON_AND_ORGANIZATION ( #11915, #17965 ) ;
#2913 = VERTEX_POINT ( 'NONE', #21262 ) ;
#2912 = DIRECTION ( 'NONE',  ( -0.000000000000000000, -0.000000000000000000, -1.000000000000000000 ) ) ;
#2914 =( BOUNDED_CURVE ( )  B_SPLINE_CURVE ( 2, ( #26707, #10293, #24063, #34210, #7652, #20803, #33991 ),
 .UNSPECIFIED., .F., .F. ) 
 B_SPLINE_CURVE_WITH_KNOTS ( ( 3, 2, 2, 3 ),
 ( 0.4179104477611941260, 0.4191542288557215112, 0.4203980099502488965, 0.4216417910447762818 ),
 .UNSPECIFIED. ) 
 CURVE ( )  GEOMETRIC_REPRESENTATION_ITEM ( )  RATIONAL_B_SPLINE_CURVE ( ( 0.9999999999999880096, 0.8660254037844506980, 1.000000000000000000, 0.8660254037844387076, 1.000000000000000000, 0.8660254037844207220, 1.000000000000017986 ) ) 
 REPRESENTATION_ITEM ( '' )  );
#2915 = ORIENTED_EDGE ( 'NONE', *, *, #25715, .T. ) ;
#2916 = CARTESIAN_POINT ( 'NONE',  ( 5.405949406249999534, 9.363379034771803333, -29.59375000204836326 ) ) ;
#2917 = DIRECTION ( 'NONE',  ( 0.000000000000000000, 0.000000000000000000, -1.000000000000000000 ) ) ;
#2918 = CARTESIAN_POINT ( 'NONE',  ( 5.405949406249999534, 9.363379034771803333, -1.281250002048373027 ) ) ;
#2919 = CARTESIAN_POINT ( 'NONE',  ( 7.644554776091147741E-16, 12.48450537969573659, -51.96875000204836681 ) ) ;
#2920 = LINE ( 'NONE', #39161, #36379 ) ;
#2921 = ADVANCED_FACE ( 'NONE', ( #5084 ), #998, .T. ) ;
#2922 = CARTESIAN_POINT ( 'NONE',  ( 9.999999999999998224, 0.000000000000000000, -27.49999999999996803 ) ) ;
#2923 = CARTESIAN_POINT ( 'NONE',  ( 7.644554776091147741E-16, 12.48450537969573659, -188.4687500020484094 ) ) ;
#2924 = CARTESIAN_POINT ( 'NONE',  ( 5.405949406249992428, -9.363379034771808662, -166.5937500020484094 ) ) ;
#2925 = CARTESIAN_POINT ( 'NONE',  ( 10.81189881249999551, -6.242252689847874514, -157.4687500020484094 ) ) ;
#2926 = VECTOR ( 'NONE', #25853, 1000.000000000000000 ) ;
#2927 = CARTESIAN_POINT ( 'NONE',  ( 5.405949406249992428, -9.363379034771808662, -174.0937500020484094 ) ) ;
#2928 = CARTESIAN_POINT ( 'NONE',  ( -9.999999999998969713, -5.773502691896847949, -76.12499999999998579 ) ) ;
#2929 = CARTESIAN_POINT ( 'NONE',  ( -10.00000000000022027, 5.773502691896128525, -187.7500000040967620 ) ) ;
#2930 = CARTESIAN_POINT ( 'NONE',  ( 9.999999999999996447, -5.773502691896262640, -191.1250000000000000 ) ) ;
#2931 = CARTESIAN_POINT ( 'NONE',  ( -10.81189881249999729, 1.324075727343319199E-15, -95.09375000204838102 ) ) ;
#2932 = CARTESIAN_POINT ( 'NONE',  ( 7.070501591499376803E-16, 11.54700538379251284, -108.5000000040967763 ) ) ;
#2933 = CARTESIAN_POINT ( 'NONE',  ( 10.81189881249999729, 0.000000000000000000, -73.53125000204838102 ) ) ;
#2934 = CARTESIAN_POINT ( 'NONE',  ( -10.00000000000051337, 5.773502691895962435, -96.25000000409676204 ) ) ;
#2935 = CARTESIAN_POINT ( 'NONE',  ( -5.405949406249996869, 9.363379034771805109, -195.8437500020484094 ) ) ;
#2936 = CARTESIAN_POINT ( 'NONE',  ( -10.81189881249999729, 1.324075727343319199E-15, -84.59375000204836681 ) ) ;
#2937 = CARTESIAN_POINT ( 'NONE',  ( 10.81189881249999907, 6.242252689847868297, -61.40625000204838102 ) ) ;
#2938 = CARTESIAN_POINT ( 'NONE',  ( 9.999999999999996447, -5.773502691896262640, -145.0000000040967905 ) ) ;
#2939 = CARTESIAN_POINT ( 'NONE',  ( -9.999999999999998224, 5.773502691896259087, -113.8750000000000000 ) ) ;
#2940 = EDGE_LOOP ( 'NONE', ( #37354, #29611, #22134, #12697 ) ) ;
#2941 = CARTESIAN_POINT ( 'NONE',  ( 10.81189881249999729, 6.242252689847867408, -145.4062500020484094 ) ) ;
#2942 = CARTESIAN_POINT ( 'NONE',  ( -5.405949406250003975, -9.363379034771801557, -153.5312500020484094 ) ) ;
#2943 = AXIS2_PLACEMENT_3D ( 'NONE', #28917, #28711, #6033 ) ;
#2944 = CARTESIAN_POINT ( 'NONE',  ( -10.81189881249999729, 1.324075727343319199E-15, -192.7812500020484094 ) ) ;
#2945 = CARTESIAN_POINT ( 'NONE',  ( 9.999999999999998224, 0.000000000000000000, -66.87500000409676204 ) ) ;
#2946 = CARTESIAN_POINT ( 'NONE',  ( -5.405949406249996869, 9.363379034771805109, -87.84375000204836681 ) ) ;
#2947 = ORIENTED_EDGE ( 'NONE', *, *, #17700, .T. ) ;
#2948 = CARTESIAN_POINT ( 'NONE',  ( -9.999999999999998224, 5.773502691896259087, -61.37499999999998579 ) ) ;
#2949 = CARTESIAN_POINT ( 'NONE',  ( 10.81189881249999907, 6.242252689847868297, -191.7187500020484094 ) ) ;
#2950 = CARTESIAN_POINT ( 'NONE',  ( -2.121150477449813534E-15, -11.54700538379251284, -74.75000000409677625 ) ) ;
#2951 = DIRECTION ( 'NONE',  ( -0.000000000000000000, -0.000000000000000000, -1.000000000000000000 ) ) ;
#2952 = CARTESIAN_POINT ( 'NONE',  ( -5.000000000000003553, -8.660254037844383745, -160.3750000040967905 ) ) ;
#2953 = CARTESIAN_POINT ( 'NONE',  ( 10.81189881249999907, 6.242252689847868297, -82.40625000204836681 ) ) ;
#2954 = CARTESIAN_POINT ( 'NONE',  ( 5.405949406249999534, 9.363379034771803333, -65.78125000204838102 ) ) ;
#2955 = CARTESIAN_POINT ( 'NONE',  ( -9.999999999999998224, 1.224646799147353059E-15, -60.12500000409676204 ) ) ;
#2956 = CARTESIAN_POINT ( 'NONE',  ( -5.405949406250003975, -9.363379034771801557, -15.34375000204835082 ) ) ;
#2957 = CARTESIAN_POINT ( 'NONE',  ( 9.999999999999998224, 1.224646799147353059E-15, -99.99999999999998579 ) ) ;
#2958 = CARTESIAN_POINT ( 'NONE',  ( -10.81189881249999729, 1.324075727343319199E-15, -191.2812500020484094 ) ) ;
#2959 = CARTESIAN_POINT ( 'NONE',  ( -5.405949406250003975, -9.363379034771801557, -11.03125000204835438 ) ) ;
#2960 = DIRECTION ( 'NONE',  ( 0.08682659386424779191, 0.08682659386424779191, 0.9924325091389669673 ) ) ;
#2961 = PLANE ( 'NONE',  #37337 ) ;
#2962 = CARTESIAN_POINT ( 'NONE',  ( 4.999999999999992006, -8.660254037844389075, -112.1250000040967763 ) ) ;
#2963 =( BOUNDED_CURVE ( )  B_SPLINE_CURVE ( 2, ( #12592, #5724, #28395, #41535, #11963, #35079, #38511 ),
 .UNSPECIFIED., .F., .F. ) 
 B_SPLINE_CURVE_WITH_KNOTS ( ( 3, 2, 2, 3 ),
 ( 0.8171641791044778058, 0.8184079601990051911, 0.8196517412935324653, 0.8208955223880598506 ),
 .UNSPECIFIED. ) 
 CURVE ( )  GEOMETRIC_REPRESENTATION_ITEM ( )  RATIONAL_B_SPLINE_CURVE ( ( 0.9999999999999761302, 0.8660254037844625774, 1.000000000000000000, 0.8660254037844387076, 1.000000000000000000, 0.8660254037844267172, 1.000000000000011990 ) ) 
 REPRESENTATION_ITEM ( '' )  );
#2964 = CARTESIAN_POINT ( 'NONE',  ( -2.121150477449813534E-15, -11.54700538379251284, -173.3750000000000000 ) ) ;
#2965 = FACE_OUTER_BOUND ( 'NONE', #36246, .T. ) ;
#2967 = EDGE_LOOP ( 'NONE', ( #9119, #38047, #30125, #16707 ) ) ;
#2966 = CARTESIAN_POINT ( 'NONE',  ( 10.81189881249999551, -6.242252689847874514, -97.65625000204839523 ) ) ;
#2968 = CARTESIAN_POINT ( 'NONE',  ( -9.999999999999998224, 1.224646799147353059E-15, -164.7500000000000000 ) ) ;
#2969 = ORIENTED_EDGE ( 'NONE', *, *, #19490, .T. ) ;
#2970 = ORIENTED_EDGE ( 'NONE', *, *, #23291, .F. ) ;
#2971 = CARTESIAN_POINT ( 'NONE',  ( -10.81189881249999907, -6.242252689847864744, -37.96875000204837391 ) ) ;
#2972 = CARTESIAN_POINT ( 'NONE',  ( 7.644554776091147741E-16, 12.48450537969573659, -29.65625000204835970 ) ) ;
#2973 = SECURITY_CLASSIFICATION_LEVEL ( 'unclassified' ) ;
#2974 = EDGE_CURVE ( 'NONE', #18914, #15678, #38842, .T. ) ;
#2975 = CARTESIAN_POINT ( 'NONE',  ( -10.81189881249999729, 6.242252689847871849, -81.71875000204838102 ) ) ;
#2976 = LINE ( 'NONE', #28247, #25674 ) ;
#2977 = ADVANCED_FACE ( 'NONE', ( #37026 ), #1211, .T. ) ;
#2978 = CARTESIAN_POINT ( 'NONE',  ( -10.81189881249999907, -6.242252689847864744, -190.9687500020484379 ) ) ;
#2979 = EDGE_CURVE ( 'NONE', #5197, #32856, #17903, .T. ) ;
#2980 = LINE ( 'NONE', #15691, #23998 ) ;
#2981 = DIRECTION ( 'NONE',  ( 0.000000000000000000, 0.000000000000000000, 1.000000000000000000 ) ) ;
#2982 = CARTESIAN_POINT ( 'NONE',  ( 10.81189881249999551, -6.242252689847874514, -154.6562500020484379 ) ) ;
#2983 = CARTESIAN_POINT ( 'NONE',  ( -4.999999999999996447, 8.660254037844387298, -12.37500000409674783 ) ) ;
#2984 = DIRECTION ( 'NONE',  ( 1.000000000000000000, 0.000000000000000000, 0.000000000000000000 ) ) ;
#2985 = CARTESIAN_POINT ( 'NONE',  ( -10.81189881249999729, 6.242252689847871849, -128.2187500020483810 ) ) ;
#2986 = CARTESIAN_POINT ( 'NONE',  ( -5.405949406249996869, 9.363379034771805109, -101.5312500020483952 ) ) ;
#2987 = CARTESIAN_POINT ( 'NONE',  ( 10.81189881249999551, -6.242252689847874514, -107.9687500020483810 ) ) ;
#2988 = CARTESIAN_POINT ( 'NONE',  ( -2.293366432827344421E-15, -12.48450537969573659, -76.71875000204838102 ) ) ;
#2989 = CARTESIAN_POINT ( 'NONE',  ( 5.405949406249992428, -9.363379034771808662, -82.78125000204838102 ) ) ;
#2990 = CARTESIAN_POINT ( 'NONE',  ( -2.121150477449813534E-15, -11.54700538379251284, -173.7500000040968189 ) ) ;
#2991 = CARTESIAN_POINT ( 'NONE',  ( 9.999999999999998224, 0.000000000000000000, -33.49999999999997158 ) ) ;
#2992 = CARTESIAN_POINT ( 'NONE',  ( 10.81189881249999729, 6.242252689847867408, -167.9062500020484094 ) ) ;
#2993 = CARTESIAN_POINT ( 'NONE',  ( -10.81189881249999907, -6.242252689847864744, -180.6562500020484094 ) ) ;
#2994 = CARTESIAN_POINT ( 'NONE',  ( -10.00000000000000000, -5.773502691896251982, -156.0000000040967905 ) ) ;
#2995 = CARTESIAN_POINT ( 'NONE',  ( 9.999999999999998224, 0.000000000000000000, -189.5000000000000000 ) ) ;
#2996 = CARTESIAN_POINT ( 'NONE',  ( 10.81189881249999551, -6.242252689847874514, -7.468750002048357928 ) ) ;
#2997 = CARTESIAN_POINT ( 'NONE',  ( 9.999999999999998224, 0.000000000000000000, -162.8750000040967905 ) ) ;
#2998 = CARTESIAN_POINT ( 'NONE',  ( -5.405949406249996869, 9.363379034771805109, -117.8437500020483810 ) ) ;
#2999 = CARTESIAN_POINT ( 'NONE',  ( 7.070501591499377789E-16, 11.54700538379251284, -79.62500000000000000 ) ) ;
#3000 = CARTESIAN_POINT ( 'NONE',  ( -5.405949406250003975, -9.363379034771801557, -14.03125000204835615 ) ) ;
#3001 = CARTESIAN_POINT ( 'NONE',  ( 10.00000000000000000, 5.773502691896255534, -101.2500000040967905 ) ) ;
#3002 = ADVANCED_FACE ( 'NONE', ( #15827 ), #29024, .T. ) ;
#3003 = LINE ( 'NONE', #6452, #34136 ) ;
#3004 = CARTESIAN_POINT ( 'NONE',  ( 5.405949406249992428, -9.363379034771808662, -105.2812500020483810 ) ) ;
#3005 = CARTESIAN_POINT ( 'NONE',  ( -5.405949406249996869, 9.363379034771805109, -91.03125000204838102 ) ) ;
#3006 = VERTEX_POINT ( 'NONE', #38304 ) ;
#3007 = CARTESIAN_POINT ( 'NONE',  ( 5.000000000000000000, 8.660254037844385522, -83.12500000409676204 ) ) ;
#3008 = LINE ( 'NONE', #23068, #18798 ) ;
#3009 = CARTESIAN_POINT ( 'NONE',  ( -2.293366432827344421E-15, -12.48450537969573659, -39.21875000204835970 ) ) ;
#3010 = ORIENTED_EDGE ( 'NONE', *, *, #24247, .F. ) ;
#3011 = CARTESIAN_POINT ( 'NONE',  ( 9.999999999999998224, 0.000000000000000000, -15.49999999999995737 ) ) ;
#3012 = CARTESIAN_POINT ( 'NONE',  ( -10.00000000000000000, -5.773502691896251982, -152.6250000000000284 ) ) ;
#3013 = ADVANCED_FACE ( 'NONE', ( #15618 ), #35296, .T. ) ;
#3014 = CARTESIAN_POINT ( 'NONE',  ( 4.999999999999992006, -8.660254037844389075, -14.62500000409674961 ) ) ;
#3015 = CARTESIAN_POINT ( 'NONE',  ( -2.121150477449813534E-15, -11.54700538379251284, -119.7500000040967905 ) ) ;
#3017 = ORIENTED_EDGE ( 'NONE', *, *, #28328, .F. ) ;
#3016 = CARTESIAN_POINT ( 'NONE',  ( 5.405949406249992428, -9.363379034771808662, -124.7812500020483952 ) ) ;
#3018 = CARTESIAN_POINT ( 'NONE',  ( -9.999999999999998224, 1.224646799147353059E-15, -152.7500000000000000 ) ) ;
#3019 = ORIENTED_EDGE ( 'NONE', *, *, #21343, .T. ) ;
#3020 = CARTESIAN_POINT ( 'NONE',  ( 10.81189881249999729, 0.000000000000000000, -57.03125000204836681 ) ) ;
#3021 = DATE_TIME_ROLE ( 'creation_date' ) ;
#3022 = CARTESIAN_POINT ( 'NONE',  ( -2.293366432827344421E-15, -12.48450537969573659, -106.7187500020483668 ) ) ;
#3024 = ORIENTED_EDGE ( 'NONE', *, *, #1117, .T. ) ;
#3023 = ORIENTED_EDGE ( 'NONE', *, *, #27774, .F. ) ;
#3025 = CARTESIAN_POINT ( 'NONE',  ( 0.000000000000000000, 0.000000000000000000, -200.0000000000000000 ) ) ;
#3026 = DIRECTION ( 'NONE',  ( -0.9961946980917455452, 0.000000000000000000, -0.08715574274765837404 ) ) ;
#3027 = ADVANCED_FACE ( 'NONE', ( #24952 ), #38733, .T. ) ;
#3028 = CARTESIAN_POINT ( 'NONE',  ( 5.405949406249999534, 9.363379034771803333, -182.7812500020484094 ) ) ;
#3029 = CARTESIAN_POINT ( 'NONE',  ( 10.81189881249999907, 6.242252689847868297, -1.218750002048353709 ) ) ;
#3030 = CARTESIAN_POINT ( 'NONE',  ( 5.000000000000000000, 8.660254037844385522, -155.1250000040967905 ) ) ;
#3031 = EDGE_CURVE ( 'NONE', #15525, #23116, #8537, .T. ) ;
#3032 = CARTESIAN_POINT ( 'NONE',  ( 7.644554776091147741E-16, 12.48450537969573659, -131.4687500020483810 ) ) ;
#3033 = CARTESIAN_POINT ( 'NONE',  ( -5.405949406250003975, -9.363379034771801557, -103.8437500020483810 ) ) ;
#3034 = DIRECTION ( 'NONE',  ( -0.000000000000000000, -0.000000000000000000, 1.000000000000000000 ) ) ;
#3035 = CARTESIAN_POINT ( 'NONE',  ( 10.81189881249999729, 0.000000000000000000, -111.0312500020483810 ) ) ;
#3036 = CARTESIAN_POINT ( 'NONE',  ( 4.999999999999992006, -8.660254037844389075, -193.1250000040967905 ) ) ;
#3037 = CARTESIAN_POINT ( 'NONE',  ( 10.81189881249999551, -6.242252689847874514, -113.9687500020483668 ) ) ;
#3038 = CARTESIAN_POINT ( 'NONE',  ( -5.405949406249996869, 9.363379034771805109, -188.5312500020484094 ) ) ;
#3039 = CARTESIAN_POINT ( 'NONE',  ( -9.999999999999998224, 1.224646799147353059E-15, -148.6250000040967905 ) ) ;
#3040 = CARTESIAN_POINT ( 'NONE',  ( 9.999999999999998224, 0.000000000000000000, -137.0000000000000000 ) ) ;
#3041 = CARTESIAN_POINT ( 'NONE',  ( -5.000000000000003553, -8.660254037844383745, -5.499999999999976907 ) ) ;
#3042 = CARTESIAN_POINT ( 'NONE',  ( -10.81189881249999729, 1.324075727343319199E-15, -65.09375000204836681 ) ) ;
#3043 = CARTESIAN_POINT ( 'NONE',  ( 10.81189881249999551, -6.242252689847874514, -50.96875000204836681 ) ) ;
#3044 = CARTESIAN_POINT ( 'NONE',  ( 10.00000000000000000, 5.773502691896255534, -182.2500000040968189 ) ) ;
#3045 = CARTESIAN_POINT ( 'NONE',  ( -10.81189881249999907, -6.242252689847864744, -20.15625000204838102 ) ) ;
#3046 = CARTESIAN_POINT ( 'NONE',  ( -10.81189881249999729, 6.242252689847871849, -29.21875000204834905 ) ) ;
#3047 = CARTESIAN_POINT ( 'NONE',  ( -4.999999999999996447, 8.660254037844387298, -117.0000000000000000 ) ) ;
#3048 = CARTESIAN_POINT ( 'NONE',  ( -10.81189881249999729, 6.242252689847871849, -135.7187500020483810 ) ) ;
#3049 = CARTESIAN_POINT ( 'NONE',  ( -2.121150477449813534E-15, -11.54700538379251284, -113.3749999999999858 ) ) ;
#3050 =( BOUNDED_CURVE ( )  B_SPLINE_CURVE ( 2, ( #18286, #36706, #28235, #25008, #7145, #16834, #32326 ),
 .UNSPECIFIED., .F., .F. ) 
 B_SPLINE_CURVE_WITH_KNOTS ( ( 3, 2, 2, 3 ),
 ( 0.3283582089552238847, 0.3296019900497513255, 0.3308457711442787108, 0.3320895522388061516 ),
 .UNSPECIFIED. ) 
 CURVE ( )  GEOMETRIC_REPRESENTATION_ITEM ( )  RATIONAL_B_SPLINE_CURVE ( ( 1.000000000000000000, 0.8660254037844387076, 1.000000000000000000, 0.8660254037844387076, 1.000000000000000000, 0.8660254037844207220, 1.000000000000017986 ) ) 
 REPRESENTATION_ITEM ( '' )  );
#3051 = DIRECTION ( 'NONE',  ( -1.000000000000000000, 0.000000000000000000, 0.000000000000000000 ) ) ;
#3052 = CARTESIAN_POINT ( 'NONE',  ( 5.000000000000000000, 8.660254037844385522, -64.74999999999997158 ) ) ;
#3053 = CARTESIAN_POINT ( 'NONE',  ( -5.405949406250003975, -9.363379034771801557, -132.5312500020484094 ) ) ;
#3054 = CARTESIAN_POINT ( 'NONE',  ( -10.81189881249999729, 1.324075727343319199E-15, -116.2812500020483952 ) ) ;
#3055 = ADVANCED_FACE ( 'NONE', ( #25785 ), #28180, .F. ) ;
#3056 = VERTEX_POINT ( 'NONE', #41538 ) ;
#3057 = LINE ( 'NONE', #32209, #27242 ) ;
#3058 = CARTESIAN_POINT ( 'NONE',  ( -4.999999999999996447, 8.660254037844387298, -111.3750000040967763 ) ) ;
#3059 = CARTESIAN_POINT ( 'NONE',  ( 12.99038105676667243, 7.500000000000067502, 49.99999999999998579 ) ) ;
#3060 = CARTESIAN_POINT ( 'NONE',  ( -5.405949406249996869, 9.363379034771805109, -69.84375000204836681 ) ) ;
#3061 = VERTEX_POINT ( 'NONE', #22332 ) ;
#3062 = CARTESIAN_POINT ( 'NONE',  ( 5.000000000000000000, 8.660254037844385522, -43.74999999999998579 ) ) ;
#3063 = CARTESIAN_POINT ( 'NONE',  ( 7.070501591499377789E-16, 11.54700538379251284, -18.50000000409676559 ) ) ;
#3064 = CARTESIAN_POINT ( 'NONE',  ( 10.81189881249999551, -6.242252689847874514, -40.65625000204836681 ) ) ;
#3065 = CARTESIAN_POINT ( 'NONE',  ( 9.999999999999998224, 0.000000000000000000, -16.99999999999996092 ) ) ;
#3066 = CARTESIAN_POINT ( 'NONE',  ( 10.00000000000000000, 5.773502691896255534, -38.25000000409675494 ) ) ;
#3067 = CARTESIAN_POINT ( 'NONE',  ( -10.81189881249999729, 1.324075727343319199E-15, -39.78125000204838102 ) ) ;
#3068 = CARTESIAN_POINT ( 'NONE',  ( 7.423074889580975722, -12.85714285714295180, 52.14285714285716011 ) ) ;
#3069 = CARTESIAN_POINT ( 'NONE',  ( -2.293366432827344421E-15, -12.48450537969573659, -139.9062500020484094 ) ) ;
#3070 = CARTESIAN_POINT ( 'NONE',  ( 5.405949406249999534, 9.363379034771803333, -148.2812500020483810 ) ) ;
#3071 = CARTESIAN_POINT ( 'NONE',  ( -10.00000000000051337, 5.773502691895962435, -150.2500000040967620 ) ) ;
#3072 = VERTEX_POINT ( 'NONE', #25368 ) ;
#3073 = ORIENTED_EDGE ( 'NONE', *, *, #2738, .T. ) ;
#3074 = ORIENTED_EDGE ( 'NONE', *, *, #26692, .F. ) ;
#3075 = LINE ( 'NONE', #29833, #24954 ) ;
#3076 = CARTESIAN_POINT ( 'NONE',  ( 5.405949406249999534, 9.363379034771803333, -173.5937500020484094 ) ) ;
#3077 = CARTESIAN_POINT ( 'NONE',  ( -2.293366432827344421E-15, -12.48450537969573659, -19.71875000204837747 ) ) ;
#3078 = CARTESIAN_POINT ( 'NONE',  ( 5.000000000000000000, 8.660254037844385522, -111.6250000040967763 ) ) ;
#3079 = CARTESIAN_POINT ( 'NONE',  ( -10.81189881249999729, 6.242252689847871849, -155.2187500020483810 ) ) ;
#3080 = CARTESIAN_POINT ( 'NONE',  ( -10.81189881249999907, -6.242252689847864744, -141.4687500020484094 ) ) ;
#3081 = CARTESIAN_POINT ( 'NONE',  ( -9.999999999999998224, 1.224646799147353059E-15, -67.24999999999997158 ) ) ;
#3082 = CARTESIAN_POINT ( 'NONE',  ( 10.81189881249999729, 0.000000000000000000, -122.8437500020483952 ) ) ;
#3083 = CARTESIAN_POINT ( 'NONE',  ( 7.644554776091147741E-16, 12.48450537969573659, -131.6562500020483810 ) ) ;
#3084 = CARTESIAN_POINT ( 'NONE',  ( 5.405949406249999534, 9.363379034771803333, -14.59375000204835082 ) ) ;
#3085 = CARTESIAN_POINT ( 'NONE',  ( -10.81189881249999729, 1.324075727343319199E-15, -138.5937500020483810 ) ) ;
#3086 = CARTESIAN_POINT ( 'NONE',  ( 10.80649504056860088, 0.7923051018166373805, -180.0000000000000000 ) ) ;
#3087 =( BOUNDED_CURVE ( )  B_SPLINE_CURVE ( 2, ( #41226, #2405, #5208, #1554, #8666, #24864, #18580 ),
 .UNSPECIFIED., .F., .F. ) 
 B_SPLINE_CURVE_WITH_KNOTS ( ( 3, 2, 2, 3 ),
 ( 0.7164179104477614857, 0.7176616915422888709, 0.7189054726368161452, 0.7201492537313435305 ),
 .UNSPECIFIED. ) 
 CURVE ( )  GEOMETRIC_REPRESENTATION_ITEM ( )  RATIONAL_B_SPLINE_CURVE ( ( 0.9999999999999641398, 0.8660254037844745678, 1.000000000000000000, 0.8660254037844387076, 1.000000000000000000, 0.8660254037844148378, 1.000000000000023981 ) ) 
 REPRESENTATION_ITEM ( '' )  );
#3088 = CARTESIAN_POINT ( 'NONE',  ( -9.999999999999479527, -5.773502691896549521, -103.1249999999999858 ) ) ;
#3089 = CARTESIAN_POINT ( 'NONE',  ( 9.999999999999998224, 0.000000000000000000, -164.0000000000000000 ) ) ;
#3090 = CARTESIAN_POINT ( 'NONE',  ( 9.999999999999479527, 5.773502691896553074, -99.75000000409679046 ) ) ;
#3091 = EDGE_CURVE ( 'NONE', #900, #22125, #533, .T. ) ;
#3092 = CARTESIAN_POINT ( 'NONE',  ( 10.81189881249999907, 6.242252689847868297, -70.21875000204840944 ) ) ;
#3093 = CARTESIAN_POINT ( 'NONE',  ( 5.405949406249999534, 9.363379034771803333, -49.28125000204838813 ) ) ;
#3094 = CARTESIAN_POINT ( 'NONE',  ( -10.81189881249999907, -6.242252689847864744, -49.96875000204837391 ) ) ;
#3095 = CARTESIAN_POINT ( 'NONE',  ( 5.405949406249992428, -9.363379034771808662, -163.5937500020484094 ) ) ;
#3096 = CARTESIAN_POINT ( 'NONE',  ( -10.00000000000000000, -5.773502691896251982, -137.6250000000000000 ) ) ;
#3097 = CARTESIAN_POINT ( 'NONE',  ( 5.405949406249999534, 9.363379034771803333, -139.2812500020483810 ) ) ;
#3098 = CARTESIAN_POINT ( 'NONE',  ( 4.999999999999992006, -8.660254037844389075, -98.62500000409677625 ) ) ;
#3099 = CARTESIAN_POINT ( 'NONE',  ( 4.999999999999992006, -8.660254037844389075, -116.6250000040967905 ) ) ;
#3100 = CARTESIAN_POINT ( 'NONE',  ( -4.999999999999996447, 8.660254037844387298, -88.49999999999998579 ) ) ;
#3101 = ORIENTED_EDGE ( 'NONE', *, *, #33115, .T. ) ;
#3102 =( BOUNDED_CURVE ( )  B_SPLINE_CURVE ( 2, ( #15926, #42054, #2796, #29127, #41416, #38829, #28500 ),
 .UNSPECIFIED., .F., .F. ) 
 B_SPLINE_CURVE_WITH_KNOTS ( ( 3, 2, 2, 3 ),
 ( 0.4888059701492538101, 0.4900497512437811398, 0.4912935323383085806, 0.4925373134328359104 ),
 .UNSPECIFIED. ) 
 CURVE ( )  GEOMETRIC_REPRESENTATION_ITEM ( )  RATIONAL_B_SPLINE_CURVE ( ( 0.9999999999999940048, 0.8660254037844447028, 1.000000000000000000, 0.8660254037844387076, 1.000000000000000000, 0.8660254037844267172, 1.000000000000011990 ) ) 
 REPRESENTATION_ITEM ( '' )  );
#3103 = CARTESIAN_POINT ( 'NONE',  ( -10.81189881249999729, 6.242252689847871849, -122.4062500020483952 ) ) ;
#3104 = CARTESIAN_POINT ( 'NONE',  ( 4.999999999999992006, -8.660254037844389075, -136.1250000040967620 ) ) ;
#3105 = CARTESIAN_POINT ( 'NONE',  ( -2.121150477449813534E-15, -11.54700538379251284, -140.7500000040967905 ) ) ;
#3106 = CARTESIAN_POINT ( 'NONE',  ( -2.293366432827344421E-15, -12.48450537969573659, -175.9062500020483810 ) ) ;
#3107 = CARTESIAN_POINT ( 'NONE',  ( 4.999999999999992006, -8.660254037844389075, -41.62500000409677625 ) ) ;
#3108 = CARTESIAN_POINT ( 'NONE',  ( 7.644554776091147741E-16, 12.48450537969573659, -62.65625000204838813 ) ) ;
#3109 = EDGE_CURVE ( 'NONE', #17742, #4273, #23718, .T. ) ;
#3110 = AXIS2_PLACEMENT_3D ( 'NONE', #25408, #5334, #8580 ) ;
#3111 = CARTESIAN_POINT ( 'NONE',  ( 9.999999999999479527, 5.773502691896553074, -45.37499999999995737 ) ) ;
#3112 = CARTESIAN_POINT ( 'NONE',  ( 5.405949406249999534, 9.363379034771803333, -160.2812500020484094 ) ) ;
#3113 = CARTESIAN_POINT ( 'NONE',  ( -5.405949406249996869, 9.363379034771805109, -146.3437500020483810 ) ) ;
#3114 = CARTESIAN_POINT ( 'NONE',  ( 5.000000000000000000, 8.660254037844385522, -167.1250000040967905 ) ) ;
#3115 = CARTESIAN_POINT ( 'NONE',  ( 5.000000000000000000, 8.660254037844385522, -174.2500000000000284 ) ) ;
#3116 = ORIENTED_EDGE ( 'NONE', *, *, #37024, .F. ) ;
#3117 = CARTESIAN_POINT ( 'NONE',  ( 9.999999999999998224, 0.000000000000000000, -30.49999999999997158 ) ) ;
#3119 = ORIENTED_EDGE ( 'NONE', *, *, #33868, .T. ) ;
#3118 = CARTESIAN_POINT ( 'NONE',  ( 10.81189881249999551, -6.242252689847874514, -73.65625000204836681 ) ) ;
#3120 = SECURITY_CLASSIFICATION_LEVEL ( 'unclassified' ) ;
#3122 = ORIENTED_EDGE ( 'NONE', *, *, #36245, .F. ) ;
#3121 = CARTESIAN_POINT ( 'NONE',  ( -5.405949406249996869, 9.363379034771805109, -120.8437500020483952 ) ) ;
#3123 = ORIENTED_EDGE ( 'NONE', *, *, #3935, .F. ) ;
#3124 = VECTOR ( 'NONE', #15169, 1000.000000000000000 ) ;
#3125 = CARTESIAN_POINT ( 'NONE',  ( -10.81189881249999729, 6.242252689847871849, -21.71875000204837036 ) ) ;
#3126 = CARTESIAN_POINT ( 'NONE',  ( -5.405949406249996869, 9.363379034771805109, -1.031250002048372805 ) ) ;
#3127 = CARTESIAN_POINT ( 'NONE',  ( -5.405949406250003975, -9.363379034771801557, -49.84375000204838102 ) ) ;
#3128 = CARTESIAN_POINT ( 'NONE',  ( -5.000000000000003553, -8.660254037844383745, -71.87500000409677625 ) ) ;
#3129 = CARTESIAN_POINT ( 'NONE',  ( -9.999999999999998224, 1.224646799147353059E-15, -28.24999999999996803 ) ) ;
#3130 = CARTESIAN_POINT ( 'NONE',  ( -10.81189881249999729, 6.242252689847871849, -185.2187500020484379 ) ) ;
#3131 = CARTESIAN_POINT ( 'NONE',  ( 5.405949406249999534, 9.363379034771803333, -166.0937500020484094 ) ) ;
#3132 = CARTESIAN_POINT ( 'NONE',  ( -10.81189881249999729, 6.242252689847871849, -152.2187500020483526 ) ) ;
#3134 = EDGE_CURVE ( 'NONE', #21806, #30027, #4937, .T. ) ;
#3133 = CARTESIAN_POINT ( 'NONE',  ( -5.405949406250003975, -9.363379034771801557, -169.8437500020484094 ) ) ;
#3135 = CARTESIAN_POINT ( 'NONE',  ( -4.999999999999996447, 8.660254037844387298, -123.3750000040967905 ) ) ;
#3136 = VECTOR ( 'NONE', #7346, 1000.000000000000114 ) ;
#3137 = CARTESIAN_POINT ( 'NONE',  ( -9.999999999999998224, 1.224646799147353059E-15, -19.62500000409675494 ) ) ;
#3138 = CARTESIAN_POINT ( 'NONE',  ( -10.00000000000000000, -5.773502691896251982, -188.6250000000000284 ) ) ;
#3139 = CARTESIAN_POINT ( 'NONE',  ( 10.81189881249999551, -6.242252689847874514, -97.46875000204838102 ) ) ;
#3140 = CARTESIAN_POINT ( 'NONE',  ( -9.999999999999998224, 1.224646799147353059E-15, -85.24999999999997158 ) ) ;
#3141 = CARTESIAN_POINT ( 'NONE',  ( -10.81189881249999907, -6.242252689847864744, -75.65625000204839523 ) ) ;
#3142 = DIRECTION ( 'NONE',  ( -0.000000000000000000, -0.000000000000000000, 1.000000000000000000 ) ) ;
#3143 = CARTESIAN_POINT ( 'NONE',  ( -10.81189881249999907, -6.242252689847864744, -189.4687500020484094 ) ) ;
#3144 = CARTESIAN_POINT ( 'NONE',  ( -10.81189881249999729, 6.242252689847871849, -164.4062500020483810 ) ) ;
#3145 = CARTESIAN_POINT ( 'NONE',  ( 10.81189881249999551, -6.242252689847874514, -60.15625000204838813 ) ) ;
#3146 = CARTESIAN_POINT ( 'NONE',  ( 5.000000000000000000, 8.660254037844385522, -140.1250000040967905 ) ) ;
#3147 = CARTESIAN_POINT ( 'NONE',  ( -5.000000000000003553, -8.660254037844383745, -114.9999999999999858 ) ) ;
#3148 = ORIENTED_EDGE ( 'NONE', *, *, #19813, .T. ) ;
#3149 = CARTESIAN_POINT ( 'NONE',  ( 5.405949406249992428, -9.363379034771808662, -139.7812500020483810 ) ) ;
#3150 = CARTESIAN_POINT ( 'NONE',  ( -5.405949406249996869, 9.363379034771805109, -157.0312500020484094 ) ) ;
#3151 = CARTESIAN_POINT ( 'NONE',  ( 5.405949406249992428, -9.363379034771808662, -196.7812500020484094 ) ) ;
#3152 = CARTESIAN_POINT ( 'NONE',  ( -4.999999999999996447, 8.660254037844387298, -104.9999999999999858 ) ) ;
#3153 = CARTESIAN_POINT ( 'NONE',  ( -10.81189881249999729, 1.324075727343319199E-15, -87.59375000204836681 ) ) ;
#3154 = ORIENTED_EDGE ( 'NONE', *, *, #16310, .T. ) ;
#3155 = CARTESIAN_POINT ( 'NONE',  ( 7.070501591499377789E-16, 11.54700538379251284, -54.12499999999997158 ) ) ;
#3156 = CARTESIAN_POINT ( 'NONE',  ( -10.81189881249999729, 1.324075727343319199E-15, -191.0937500020484094 ) ) ;
#3157 = CARTESIAN_POINT ( 'NONE',  ( 9.999999999999998224, 0.000000000000000000, -72.87500000409677625 ) ) ;
#3158 = EDGE_CURVE ( 'NONE', #18128, #20886, #15127, .T. ) ;
#3159 = CARTESIAN_POINT ( 'NONE',  ( 9.999999999998969713, 5.773502691896851502, -66.37499999999997158 ) ) ;
#3160 = DIRECTION ( 'NONE',  ( -0.000000000000000000, -0.000000000000000000, -1.000000000000000000 ) ) ;
#3161 = CARTESIAN_POINT ( 'NONE',  ( 10.81189881249999907, 6.242252689847868297, -86.90625000204836681 ) ) ;
#3162 = AXIS2_PLACEMENT_3D ( 'NONE', #7151, #10168, #4128 ) ;
#3163 = CARTESIAN_POINT ( 'NONE',  ( 10.81189881249999551, -6.242252689847874514, -69.15625000204840944 ) ) ;
#3164 = AXIS2_PLACEMENT_3D ( 'NONE', #18503, #2125, #15256 ) ;
#3165 = CARTESIAN_POINT ( 'NONE',  ( 10.00000000000000000, 5.773502691896255534, -60.75000000409676915 ) ) ;
#3166 = CARTESIAN_POINT ( 'NONE',  ( 10.81189881249999729, 0.000000000000000000, -17.84375000204835260 ) ) ;
#3167 = CARTESIAN_POINT ( 'NONE',  ( -5.000000000000003553, -8.660254037844383745, -137.8750000040967905 ) ) ;
#3168 = CARTESIAN_POINT ( 'NONE',  ( -5.405949406249996869, 9.363379034771805109, -188.5312500020484094 ) ) ;
#3169 = CARTESIAN_POINT ( 'NONE',  ( 7.644554776091147741E-16, 12.48450537969573659, -16.15625000204837391 ) ) ;
#3170 = CARTESIAN_POINT ( 'NONE',  ( -5.405949406249996869, 9.363379034771805109, -0.8437500020483656993 ) ) ;
#3171 = CARTESIAN_POINT ( 'NONE',  ( 9.999999999999998224, 0.000000000000000000, -110.3750000040967763 ) ) ;
#3172 = VECTOR ( 'NONE', #40705, 1000.000000000000000 ) ;
#3173 =( BOUNDED_CURVE ( )  B_SPLINE_CURVE ( 2, ( #22582, #13055, #26249, #12424, #9202, #6400, #41995 ),
 .UNSPECIFIED., .F., .F. ) 
 B_SPLINE_CURVE_WITH_KNOTS ( ( 3, 2, 2, 3 ),
 ( 0.4067164179104478250, 0.4079601990049751548, 0.4092039800995025400, 0.4104477611940299253 ),
 .UNSPECIFIED. ) 
 CURVE ( )  GEOMETRIC_REPRESENTATION_ITEM ( )  RATIONAL_B_SPLINE_CURVE ( ( 0.9999999999999940048, 0.8660254037844447028, 1.000000000000000000, 0.8660254037844387076, 1.000000000000000000, 0.8660254037844327124, 1.000000000000005995 ) ) 
 REPRESENTATION_ITEM ( '' )  );
#3174 = CARTESIAN_POINT ( 'NONE',  ( -9.999999999999479527, -5.773502691896549521, -46.12499999999995026 ) ) ;
#3175 = CARTESIAN_POINT ( 'NONE',  ( -2.275517850991317657E-15, -20.00000000000000000, -219.9999999999999716 ) ) ;
#3176 = CARTESIAN_POINT ( 'NONE',  ( -2.121150477449813534E-15, -11.54700538379251284, -168.8750000000000000 ) ) ;
#3177 = CARTESIAN_POINT ( 'NONE',  ( 5.000000000000000000, 8.660254037844385522, -166.7500000000000000 ) ) ;
#3179 = EDGE_LOOP ( 'NONE', ( #26005, #32252, #14720, #39877 ) ) ;
#3178 = CARTESIAN_POINT ( 'NONE',  ( 5.405949406249992428, -9.363379034771808662, -97.78125000204839523 ) ) ;
#3180 = CARTESIAN_POINT ( 'NONE',  ( 9.999999999999998224, 0.000000000000000000, -162.5000000000000000 ) ) ;
#3182 = ORIENTED_EDGE ( 'NONE', *, *, #26935, .F. ) ;
#3181 = CARTESIAN_POINT ( 'NONE',  ( 5.405949406249999534, 9.363379034771803333, -101.5937500020483810 ) ) ;
#3183 = ORIENTED_EDGE ( 'NONE', *, *, #13019, .F. ) ;
#3184 = CARTESIAN_POINT ( 'NONE',  ( 7.644554776091147741E-16, 12.48450537969573659, -32.46875000204835970 ) ) ;
#3185 = CARTESIAN_POINT ( 'NONE',  ( -2.293366432827344421E-15, -12.48450537969573659, -24.40625000204838457 ) ) ;
#3186 = CARTESIAN_POINT ( 'NONE',  ( -10.81189881249999729, 1.324075727343319199E-15, -75.59375000204838102 ) ) ;
#3187 = CARTESIAN_POINT ( 'NONE',  ( -5.000000000000003553, -8.660254037844383745, -83.87500000409677625 ) ) ;
#3188 = CARTESIAN_POINT ( 'NONE',  ( -5.405949406249996869, 9.363379034771805109, -192.8437500020484094 ) ) ;
#3189 = VECTOR ( 'NONE', #15892, 1000.000000000000000 ) ;
#3190 = CARTESIAN_POINT ( 'NONE',  ( -4.999999999999996447, 8.660254037844387298, -72.37500000409677625 ) ) ;
#3191 = DIRECTION ( 'NONE',  ( 1.000000000000000000, 0.000000000000000000, 0.000000000000000000 ) ) ;
#3192 = CARTESIAN_POINT ( 'NONE',  ( -5.405949406249996869, 9.363379034771805109, -154.0312500020484094 ) ) ;
#3193 = CARTESIAN_POINT ( 'NONE',  ( 7.070501591499377789E-16, 11.54700538379251284, -5.000000004096767370 ) ) ;
#3194 = CARTESIAN_POINT ( 'NONE',  ( -9.999999999999998224, 1.224646799147353059E-15, -130.2499999999999716 ) ) ;
#3195 = CARTESIAN_POINT ( 'NONE',  ( -2.293366432827344421E-15, -12.48450537969573659, -124.7187500020483668 ) ) ;
#3196 = CARTESIAN_POINT ( 'NONE',  ( 10.81189881249999907, 6.242252689847868297, -97.40625000204839523 ) ) ;
#3197 = CARTESIAN_POINT ( 'NONE',  ( 5.405949406249992428, -9.363379034771808662, -111.0937500020483810 ) ) ;
#3198 = CARTESIAN_POINT ( 'NONE',  ( -2.293366432827344421E-15, -12.48450537969573659, -78.21875000204838102 ) ) ;
#3199 = CARTESIAN_POINT ( 'NONE',  ( -5.405949406250003975, -9.363379034771801557, -81.53125000204839523 ) ) ;
#3200 = CARTESIAN_POINT ( 'NONE',  ( 7.070501591499377789E-16, 11.54700538379251284, -165.5000000040967905 ) ) ;
#3201 = DIRECTION ( 'NONE',  ( 1.000000000000000000, 0.000000000000000000, 0.000000000000000000 ) ) ;
#3202 = CARTESIAN_POINT ( 'NONE',  ( -5.405949406249996869, 9.363379034771805109, -164.5312500020484094 ) ) ;
#3203 = CARTESIAN_POINT ( 'NONE',  ( 7.644554776091147741E-16, 12.48450537969573659, -176.6562500020484094 ) ) ;
#3204 = CARTESIAN_POINT ( 'NONE',  ( -5.000000000000003553, -8.660254037844383745, -154.3750000040967905 ) ) ;
#3205 = FACE_OUTER_BOUND ( 'NONE', #36082, .T. ) ;
#3206 = CARTESIAN_POINT ( 'NONE',  ( -10.81189881249999729, 6.242252689847871849, -8.218750002048357928 ) ) ;
#3207 = CARTESIAN_POINT ( 'NONE',  ( -9.999999999999998224, 1.224646799147353059E-15, -127.2499999999999716 ) ) ;
#3208 = CARTESIAN_POINT ( 'NONE',  ( 10.81189881249999551, -6.242252689847874514, -116.9687500020483952 ) ) ;
#3209 = CARTESIAN_POINT ( 'NONE',  ( 7.070501591499377789E-16, 11.54700538379251284, -82.62500000000000000 ) ) ;
#3210 = CARTESIAN_POINT ( 'NONE',  ( -10.81189881249999907, -6.242252689847864744, -11.15625000204836859 ) ) ;
#3211 = CARTESIAN_POINT ( 'NONE',  ( -9.999999999999998224, 5.773502691896259087, -94.75000000409677625 ) ) ;
#3212 = DIRECTION ( 'NONE',  ( -0.000000000000000000, -0.000000000000000000, 1.000000000000000000 ) ) ;
#3213 = CARTESIAN_POINT ( 'NONE',  ( 10.81189881249999729, 0.000000000000000000, -108.0312500020483810 ) ) ;
#3214 = CARTESIAN_POINT ( 'NONE',  ( -5.405949406249996869, 9.363379034771805109, -92.53125000204838102 ) ) ;
#3215 = ORIENTED_EDGE ( 'NONE', *, *, #6620, .F. ) ;
#3216 =( BOUNDED_CURVE ( )  B_SPLINE_CURVE ( 2, ( #11619, #11839, #4521, #25040, #24827, #8417, #8626 ),
 .UNSPECIFIED., .F., .F. ) 
 B_SPLINE_CURVE_WITH_KNOTS ( ( 3, 2, 2, 3 ),
 ( 0.1679104477611940427, 0.1691542288557214002, 0.1703980099502487855, 0.1716417910447761430 ),
 .UNSPECIFIED. ) 
 CURVE ( )  GEOMETRIC_REPRESENTATION_ITEM ( )  RATIONAL_B_SPLINE_CURVE ( ( 1.000000000000000000, 0.8660254037844387076, 1.000000000000000000, 0.8660254037844387076, 1.000000000000000000, 0.8660254037844357100, 1.000000000000003109 ) ) 
 REPRESENTATION_ITEM ( '' )  );
#3217 = CARTESIAN_POINT ( 'NONE',  ( 4.999999999999992006, -8.660254037844389075, -80.62500000409677625 ) ) ;
#3218 = CARTESIAN_POINT ( 'NONE',  ( -9.999999999999998224, 1.224646799147353059E-15, -141.1250000040967905 ) ) ;
#3219 = CARTESIAN_POINT ( 'NONE',  ( 10.81189881249999551, -6.242252689847874514, -43.46875000204836681 ) ) ;
#3220 = ORIENTED_EDGE ( 'NONE', *, *, #29989, .F. ) ;
#3221 = CARTESIAN_POINT ( 'NONE',  ( 9.999999999999996447, -5.773502691896262640, -12.62499999999996270 ) ) ;
#3222 = EDGE_CURVE ( 'NONE', #38687, #3910, #19288, .T. ) ;
#3223 = CARTESIAN_POINT ( 'NONE',  ( 10.00000000000000000, 5.773502691896255534, -144.3750000000000284 ) ) ;
#3224 = CARTESIAN_POINT ( 'NONE',  ( -2.121150477449813534E-15, -11.54700538379251284, -11.75000000409676026 ) ) ;
#3225 = EDGE_CURVE ( 'NONE', #33328, #28517, #33114, .T. ) ;
#3226 = CARTESIAN_POINT ( 'NONE',  ( 9.999999999999996447, -5.773502691896262640, -188.1250000000000284 ) ) ;
#3228 = VERTEX_POINT ( 'NONE', #30090 ) ;
#3227 = CARTESIAN_POINT ( 'NONE',  ( -5.405949406250003975, -9.363379034771801557, -116.0312500020483952 ) ) ;
#3229 = LINE ( 'NONE', #23288, #20688 ) ;
#3230 = ORIENTED_EDGE ( 'NONE', *, *, #36245, .T. ) ;
#3231 = CARTESIAN_POINT ( 'NONE',  ( -5.405949406250003975, -9.363379034771801557, -42.53125000204838102 ) ) ;
#3232 = APPROVAL_DATE_TIME ( #28726, #26222 ) ;
#3233 = CARTESIAN_POINT ( 'NONE',  ( 5.405949406249999534, 9.363379034771803333, -106.0937500020483810 ) ) ;
#3234 = CARTESIAN_POINT ( 'NONE',  ( -10.81189881249999729, 6.242252689847871849, -125.4062500020483810 ) ) ;
#3235 = ORIENTED_EDGE ( 'NONE', *, *, #33571, .T. ) ;
#3236 = CYLINDRICAL_SURFACE ( 'NONE', #36275, 9.999999999999998224 ) ;
#3237 = CARTESIAN_POINT ( 'NONE',  ( -9.999999999999998224, 1.224646799147353059E-15, -126.1250000040967620 ) ) ;
#3238 = CARTESIAN_POINT ( 'NONE',  ( -10.81189881249999907, -6.242252689847864744, -179.1562500020484094 ) ) ;
#3239 = LINE ( 'NONE', #29147, #41974 ) ;
#3240 = FACE_OUTER_BOUND ( 'NONE', #25788, .T. ) ;
#3241 = CARTESIAN_POINT ( 'NONE',  ( 10.81189881249999729, 6.242252689847867408, -133.2187500020483810 ) ) ;
#3242 = CARTESIAN_POINT ( 'NONE',  ( -10.81189881249999907, -6.242252689847864744, -100.9687500020483810 ) ) ;
#3243 = CARTESIAN_POINT ( 'NONE',  ( -2.121150477449813534E-15, -11.54700538379251284, -158.3750000000000000 ) ) ;
#3244 = CARTESIAN_POINT ( 'NONE',  ( 10.81189881249999551, -6.242252689847874514, -109.6562500020483810 ) ) ;
#3245 = CARTESIAN_POINT ( 'NONE',  ( -10.00000000000000000, -5.773502691896251982, -195.0000000040967905 ) ) ;
#3246 = CARTESIAN_POINT ( 'NONE',  ( 7.644554776091147741E-16, 12.48450537969573659, -114.9687500020483668 ) ) ;
#3247 = CARTESIAN_POINT ( 'NONE',  ( 5.405949406249999534, 9.363379034771803333, -185.7812500020484094 ) ) ;
#3248 = CARTESIAN_POINT ( 'NONE',  ( -5.000000000000003553, -8.660254037844383745, -185.8750000040967905 ) ) ;
#3249 = CARTESIAN_POINT ( 'NONE',  ( 4.999999999999992006, -8.660254037844389075, -141.7500000000000000 ) ) ;
#3250 = CARTESIAN_POINT ( 'NONE',  ( -5.000000000000003553, -8.660254037844383745, -2.499999999999974243 ) ) ;
#3251 = CARTESIAN_POINT ( 'NONE',  ( -10.81189881249999729, 1.324075727343319199E-15, -60.59375000204836681 ) ) ;
#3252 = CARTESIAN_POINT ( 'NONE',  ( 10.81189881249999551, -6.242252689847874514, -47.96875000204836681 ) ) ;
#3253 = UNCERTAINTY_MEASURE_WITH_UNIT (LENGTH_MEASURE( 1.000000000000000082E-05 ), #41955, 'distance_accuracy_value', 'NONE');
#3254 = CARTESIAN_POINT ( 'NONE',  ( 4.999999999999992006, -8.660254037844389075, -184.1250000040967905 ) ) ;
#3255 = CARTESIAN_POINT ( 'NONE',  ( 7.644554776091147741E-16, 12.48450537969573659, -22.15625000204837391 ) ) ;
#3256 = CARTESIAN_POINT ( 'NONE',  ( 10.81189881249999729, 0.000000000000000000, -29.84375000204836326 ) ) ;
#3257 = CARTESIAN_POINT ( 'NONE',  ( -9.999999999999998224, 1.224646799147353059E-15, -148.6250000040967905 ) ) ;
#3258 = CARTESIAN_POINT ( 'NONE',  ( -10.81189881249999729, 6.242252689847871849, -140.2187500020483810 ) ) ;
#3259 = CARTESIAN_POINT ( 'NONE',  ( -9.999999999999998224, 5.773502691896259087, -106.3749999999999858 ) ) ;
#3260 = CARTESIAN_POINT ( 'NONE',  ( 5.405949406249999534, 9.363379034771803333, -35.78125000204837391 ) ) ;
#3261 = CYLINDRICAL_SURFACE ( 'NONE', #18288, 9.999999999999998224 ) ;
#3262 = CARTESIAN_POINT ( 'NONE',  ( 7.070501591499377789E-16, 11.54700538379251284, -66.12500000000000000 ) ) ;
#3263 = CARTESIAN_POINT ( 'NONE',  ( 5.405949406249992428, -9.363379034771808662, -132.2812500020483810 ) ) ;
#3264 = CARTESIAN_POINT ( 'NONE',  ( 10.81189881249999729, 6.242252689847867408, -118.4062500020483810 ) ) ;
#3265 = EDGE_LOOP ( 'NONE', ( #20993, #9522, #25953, #23706 ) ) ;
#3266 = CYLINDRICAL_SURFACE ( 'NONE', #20331, 9.999999999999998224 ) ;
#3267 = CARTESIAN_POINT ( 'NONE',  ( 7.070501591499377789E-16, 11.54700538379251284, -107.0000000040967763 ) ) ;
#3268 = CARTESIAN_POINT ( 'NONE',  ( 5.405949406249992428, -9.363379034771808662, -69.09375000204836681 ) ) ;
#3269 = ORIENTED_EDGE ( 'NONE', *, *, #15533, .F. ) ;
#3270 = CARTESIAN_POINT ( 'NONE',  ( -4.999999999999996447, 8.660254037844387298, -44.99999999999998579 ) ) ;
#3271 = CARTESIAN_POINT ( 'NONE',  ( -4.999999999999996447, 8.660254037844387298, -15.37500000409675138 ) ) ;
#3272 = EDGE_CURVE ( 'NONE', #25139, #4764, #1664, .T. ) ;
#3273 = CARTESIAN_POINT ( 'NONE',  ( -10.81189881249999729, -6.242252689847864744, -42.65625000204837391 ) ) ;
#3274 = CARTESIAN_POINT ( 'NONE',  ( -5.000000000000003553, -8.660254037844383745, -131.8750000040967905 ) ) ;
#3275 = CARTESIAN_POINT ( 'NONE',  ( 4.999999999999992006, -8.660254037844389075, -32.62500000409676915 ) ) ;
#3276 = EDGE_CURVE ( 'NONE', #516, #6299, #13646, .T. ) ;
#3277 = CARTESIAN_POINT ( 'NONE',  ( -9.999999999999998224, 0.000000000000000000, -99.99999999999998579 ) ) ;
#3278 = CARTESIAN_POINT ( 'NONE',  ( -10.81189881249999907, -6.242252689847864744, -137.1562500020483810 ) ) ;
#3279 = EDGE_CURVE ( 'NONE', #795, #25379, #31162, .T. ) ;
#3280 = CARTESIAN_POINT ( 'NONE',  ( 5.405949406249992428, -9.363379034771808662, -139.7812500020483810 ) ) ;
#3281 = PRODUCT_DEFINITION ( 'UNKNOWN', '', #22864, #26130 ) ;
#3282 = CARTESIAN_POINT ( 'NONE',  ( 9.999999999999998224, 0.000000000000000000, -122.3750000040967905 ) ) ;
#3283 = ORIENTED_EDGE ( 'NONE', *, *, #35723, .T. ) ;
#3284 = VERTEX_POINT ( 'NONE', #16460 ) ;
#3285 = ORIENTED_EDGE ( 'NONE', *, *, #12511, .F. ) ;
#3286 = CARTESIAN_POINT ( 'NONE',  ( 4.999999999999992006, -8.660254037844389075, -129.7499999999999716 ) ) ;
#3287 = CARTESIAN_POINT ( 'NONE',  ( -2.293366432827344421E-15, -12.48450537969573659, -172.7187500020484094 ) ) ;
#3288 = EDGE_CURVE ( 'NONE', #2291, #8915, #19541, .T. ) ;
#3289 = CARTESIAN_POINT ( 'NONE',  ( 5.405949406249992428, -9.363379034771808662, -25.59375000204835970 ) ) ;
#3290 = DIRECTION ( 'NONE',  ( -0.000000000000000000, -0.000000000000000000, 1.000000000000000000 ) ) ;
#3291 = AXIS2_PLACEMENT_3D ( 'NONE', #10282, #23469, #36616 ) ;
#3292 = CARTESIAN_POINT ( 'NONE',  ( -5.405949406250003975, -9.363379034771801557, -153.3437500020483810 ) ) ;
#3293 = CARTESIAN_POINT ( 'NONE',  ( 10.81189881249999551, -6.242252689847874514, -142.4687500020483810 ) ) ;
#3294 =( BOUNDED_CURVE ( )  B_SPLINE_CURVE ( 2, ( #33749, #14064, #27258, #40397, #10844, #37176, #20776 ),
 .UNSPECIFIED., .F., .F. ) 
 B_SPLINE_CURVE_WITH_KNOTS ( ( 3, 2, 2, 3 ),
 ( 0.1716417910447761430, 0.1728855721393035005, 0.1741293532338308858, 0.1753731343283582433 ),
 .UNSPECIFIED. ) 
 CURVE ( )  GEOMETRIC_REPRESENTATION_ITEM ( )  RATIONAL_B_SPLINE_CURVE ( ( 0.9999999999999970024, 0.8660254037844417052, 1.000000000000000000, 0.8660254037844387076, 1.000000000000000000, 0.8660254037844357100, 1.000000000000003109 ) ) 
 REPRESENTATION_ITEM ( '' )  );
#3295 = CARTESIAN_POINT ( 'NONE',  ( -9.999999999998456346, -5.773502691897145489, -10.12499999999994671 ) ) ;
#3296 = CARTESIAN_POINT ( 'NONE',  ( 10.81189881249999907, 6.242252689847868297, -125.7187500020483810 ) ) ;
#3297 = CARTESIAN_POINT ( 'NONE',  ( -10.81189881249999729, 1.324075727343319199E-15, -129.7812500020483810 ) ) ;
#3298 = CARTESIAN_POINT ( 'NONE',  ( -2.293366432827344421E-15, -12.48450537969573659, -21.21875000204837036 ) ) ;
#3299 = CARTESIAN_POINT ( 'NONE',  ( -5.405949406249996869, 9.363379034771805109, -135.8437500020484094 ) ) ;
#3300 = FACE_OUTER_BOUND ( 'NONE', #20729, .T. ) ;
#3301 = CARTESIAN_POINT ( 'NONE',  ( 5.000000000000000000, 8.660254037844385522, -166.7500000000000000 ) ) ;
#3302 = CARTESIAN_POINT ( 'NONE',  ( -10.00000000000051337, 5.773502691895962435, -99.25000000409679046 ) ) ;
#3303 = CARTESIAN_POINT ( 'NONE',  ( 5.405949406249992428, -9.363379034771808662, -76.59375000204838102 ) ) ;
#3304 = CARTESIAN_POINT ( 'NONE',  ( -10.81189881249999907, -6.242252689847864744, -42.65625000204837391 ) ) ;
#3305 = CARTESIAN_POINT ( 'NONE',  ( -10.81189881249999729, 1.324075727343319199E-15, -57.59375000204835970 ) ) ;
#3306 = DIRECTION ( 'NONE',  ( -0.000000000000000000, -0.000000000000000000, 1.000000000000000000 ) ) ;
#3307 = CARTESIAN_POINT ( 'NONE',  ( -5.405949406250003975, -9.363379034771801557, -163.8437500020484094 ) ) ;
#3308 = CARTESIAN_POINT ( 'NONE',  ( 9.999999999999998224, 0.000000000000000000, -128.0000000000000000 ) ) ;
#3309 = CARTESIAN_POINT ( 'NONE',  ( 7.644554776091147741E-16, 12.48450537969573659, -134.6562500020483810 ) ) ;
#3310 = CARTESIAN_POINT ( 'NONE',  ( -9.999999999999998224, 1.224646799147353059E-15, -151.2500000000000000 ) ) ;
#3311 = CARTESIAN_POINT ( 'NONE',  ( -9.999999999999998224, 5.773502691896259087, -115.7500000040967763 ) ) ;
#3312 = CARTESIAN_POINT ( 'NONE',  ( 9.999999999999998224, 0.000000000000000000, -87.49999999999998579 ) ) ;
#3313 = VERTEX_POINT ( 'NONE', #26204 ) ;
#3314 = CARTESIAN_POINT ( 'NONE',  ( -5.405949406250003975, -9.363379034771801557, -107.0312500020483810 ) ) ;
#3315 = CARTESIAN_POINT ( 'NONE',  ( -9.999999999999998224, 5.773502691896259087, -133.7500000040967905 ) ) ;
#3316 = CARTESIAN_POINT ( 'NONE',  ( -10.81189881249999729, 6.242252689847871849, -170.4062500020484094 ) ) ;
#3317 = CARTESIAN_POINT ( 'NONE',  ( 7.070501591499377789E-16, 11.54700538379251284, -42.50000000409675494 ) ) ;
#3318 = CARTESIAN_POINT ( 'NONE',  ( -5.500000000000003553, 20.00000000000000000, -232.0000000000000000 ) ) ;
#3319 = CARTESIAN_POINT ( 'NONE',  ( -10.81189881249999729, 1.324075727343319199E-15, -57.78125000204836681 ) ) ;
#3320 = CARTESIAN_POINT ( 'NONE',  ( -9.999999999999998224, 1.224646799147353059E-15, -124.2500000000000000 ) ) ;
#3321 = CARTESIAN_POINT ( 'NONE',  ( 5.405949406249999534, 9.363379034771803333, -157.2812500020484094 ) ) ;
#3322 = CARTESIAN_POINT ( 'NONE',  ( 10.81189881249999729, 0.000000000000000000, -139.3437500020484094 ) ) ;
#3323 = VECTOR ( 'NONE', #37906, 1000.000000000000000 ) ;
#3324 = DIRECTION ( 'NONE',  ( 1.000000000000000000, 0.000000000000000000, 0.000000000000000000 ) ) ;
#3325 = CARTESIAN_POINT ( 'NONE',  ( -9.999999999999998224, 1.224646799147353059E-15, -79.24999999999998579 ) ) ;
#3326 = AXIS2_PLACEMENT_3D ( 'NONE', #16008, #16214, #36518 ) ;
#3327 = ORIENTED_EDGE ( 'NONE', *, *, #4709, .T. ) ;
#3328 = CARTESIAN_POINT ( 'NONE',  ( 10.00000000000000000, 5.773502691896255534, -131.2500000040967905 ) ) ;
#3329 = ADVANCED_FACE ( 'NONE', ( #6357 ), #20144, .T. ) ;
#3331 = ORIENTED_EDGE ( 'NONE', *, *, #19158, .T. ) ;
#3330 = CARTESIAN_POINT ( 'NONE',  ( -10.81189881249999907, -6.242252689847864744, -69.65625000204839523 ) ) ;
#3332 = DATE_AND_TIME ( #10214, #12458 ) ;
#3334 = ORIENTED_EDGE ( 'NONE', *, *, #11748, .T. ) ;
#3333 = CARTESIAN_POINT ( 'NONE',  ( -10.81189881249999907, -6.242252689847864744, -115.9687500020483810 ) ) ;
#3335 = VERTEX_POINT ( 'NONE', #22972 ) ;
#3336 = CARTESIAN_POINT ( 'NONE',  ( -2.293366432827344421E-15, -12.48450537969573659, -24.21875000204836326 ) ) ;
#3337 =( BOUNDED_CURVE ( )  B_SPLINE_CURVE ( 2, ( #37639, #33985, #27931, #1392, #37853, #27500, #2038 ),
 .UNSPECIFIED., .F., .F. ) 
 B_SPLINE_CURVE_WITH_KNOTS ( ( 3, 2, 2, 3 ),
 ( 0.4291044776119404269, 0.4303482587064677567, 0.4315920398009951975, 0.4328358208955225273 ),
 .UNSPECIFIED. ) 
 CURVE ( )  GEOMETRIC_REPRESENTATION_ITEM ( )  RATIONAL_B_SPLINE_CURVE ( ( 0.9999999999999880096, 0.8660254037844506980, 1.000000000000000000, 0.8660254037844387076, 1.000000000000000000, 0.8660254037844207220, 1.000000000000017986 ) ) 
 REPRESENTATION_ITEM ( '' )  );
#3338 = CARTESIAN_POINT ( 'NONE',  ( -10.81189881249999907, -6.242252689847864744, -0.6562500020483670315 ) ) ;
#3339 = CARTESIAN_POINT ( 'NONE',  ( 10.81189881249999729, 0.000000000000000000, -44.84375000204837391 ) ) ;
#3340 = CARTESIAN_POINT ( 'NONE',  ( 9.999999999999998224, 0.000000000000000000, -200.0000000000000000 ) ) ;
#3341 = CARTESIAN_POINT ( 'NONE',  ( -2.121150477449813534E-15, -11.54700538379251284, -29.37499999999995381 ) ) ;
#3342 = CARTESIAN_POINT ( 'NONE',  ( -2.293366432827344421E-15, -12.48450537969573659, -183.2187500020484094 ) ) ;
#3343 = CARTESIAN_POINT ( 'NONE',  ( 10.81189881249999551, -6.242252689847874514, -169.4687500020483810 ) ) ;
#3344 = CARTESIAN_POINT ( 'NONE',  ( -5.405949406249996869, 9.363379034771805109, -152.3437500020483810 ) ) ;
#3345 = CARTESIAN_POINT ( 'NONE',  ( -10.81189881249999729, -6.242252689847864744, -162.4687500020483526 ) ) ;
#3346 = CARTESIAN_POINT ( 'NONE',  ( 0.000000000000000000, 20.00000000000000000, -232.0000000000000000 ) ) ;
#3347 =( BOUNDED_CURVE ( )  B_SPLINE_CURVE ( 2, ( #30566, #24513, #33589, #14553, #27102, #37666, #4224 ),
 .UNSPECIFIED., .F., .F. ) 
 B_SPLINE_CURVE_WITH_KNOTS ( ( 3, 2, 2, 3 ),
 ( 0.6231343283582090331, 0.6243781094527364184, 0.6256218905472638037, 0.6268656716417911889 ),
 .UNSPECIFIED. ) 
 CURVE ( )  GEOMETRIC_REPRESENTATION_ITEM ( )  RATIONAL_B_SPLINE_CURVE ( ( 0.9999999999999880096, 0.8660254037844506980, 1.000000000000000000, 0.8660254037844387076, 1.000000000000000000, 0.8660254037844267172, 1.000000000000011990 ) ) 
 REPRESENTATION_ITEM ( '' )  );
#3348 = CARTESIAN_POINT ( 'NONE',  ( 5.000000000000000000, 8.660254037844385522, -189.2500000000000000 ) ) ;
#3349 = CARTESIAN_POINT ( 'NONE',  ( -10.81189881249999907, -6.242252689847864744, -93.46875000204836681 ) ) ;
#3350 = CARTESIAN_POINT ( 'NONE',  ( 5.000000000000000000, 8.660254037844385522, -198.6250000040967905 ) ) ;
#3351 = CARTESIAN_POINT ( 'NONE',  ( 5.405949406249999534, 9.363379034771803333, -62.78125000204837391 ) ) ;
#3352 = CARTESIAN_POINT ( 'NONE',  ( 9.999999999999994671, -5.773502691896262640, -131.5000000040967905 ) ) ;
#3353 = CARTESIAN_POINT ( 'NONE',  ( -5.405949406249996869, 9.363379034771805109, -185.3437500020483810 ) ) ;
#3354 = AXIS2_PLACEMENT_3D ( 'NONE', #14912, #21622, #11677 ) ;
#3355 = CARTESIAN_POINT ( 'NONE',  ( 5.405949406249992428, -9.363379034771808662, -163.7812500020484094 ) ) ;
#3356 = CARTESIAN_POINT ( 'NONE',  ( -10.81189881249999729, 6.242252689847871849, -59.40625000204838813 ) ) ;
#3357 = CARTESIAN_POINT ( 'NONE',  ( -9.999999999999998224, 1.224646799147353059E-15, -138.1250000040967620 ) ) ;
#3358 = CARTESIAN_POINT ( 'NONE',  ( 9.999999999999998224, 0.000000000000000000, -115.9999999999999858 ) ) ;
#3359 = ORIENTED_EDGE ( 'NONE', *, *, #11801, .F. ) ;
#3360 = CARTESIAN_POINT ( 'NONE',  ( 5.405949406249999534, 9.363379034771803333, -140.7812500020483810 ) ) ;
#3361 = CARTESIAN_POINT ( 'NONE',  ( -10.81189881249999729, 1.324075727343319199E-15, -156.7812500020484094 ) ) ;
#3362 = CARTESIAN_POINT ( 'NONE',  ( -5.405949406249996869, 9.363379034771805109, -196.0312500020484094 ) ) ;
#3363 = CARTESIAN_POINT ( 'NONE',  ( 0.000000000000000000, 0.000000000000000000, -99.99999999999998579 ) ) ;
#3364 = CARTESIAN_POINT ( 'NONE',  ( -5.405949406250003975, -9.363379034771801557, -93.34375000204838102 ) ) ;
#3365 = ORIENTED_EDGE ( 'NONE', *, *, #14669, .T. ) ;
#3366 = CARTESIAN_POINT ( 'NONE',  ( 4.999999999999992006, -8.660254037844389075, -56.24999999999996447 ) ) ;
#3367 = CARTESIAN_POINT ( 'NONE',  ( -10.81189881249999907, -6.242252689847864744, -190.9687500020484379 ) ) ;
#3368 = CARTESIAN_POINT ( 'NONE',  ( -9.999999999999998224, 1.224646799147353059E-15, -67.62500000409676204 ) ) ;
#3369 = CARTESIAN_POINT ( 'NONE',  ( -10.00000000000154188, 5.773502691895366468, -12.25000000409673184 ) ) ;
#3370 = CARTESIAN_POINT ( 'NONE',  ( -5.405949406250003975, -9.363379034771801557, -86.03125000204838102 ) ) ;
#3371 = CARTESIAN_POINT ( 'NONE',  ( -5.405949406250003975, -9.363379034771801557, -63.53125000204837391 ) ) ;
#3372 = CARTESIAN_POINT ( 'NONE',  ( 4.999999999999992006, -8.660254037844389075, -59.62500000409676204 ) ) ;
#3373 = CARTESIAN_POINT ( 'NONE',  ( -10.81189881249999729, 6.242252689847871849, -15.71875000204836503 ) ) ;
#3374 = CYLINDRICAL_SURFACE ( 'NONE', #18662, 9.999999999999998224 ) ;
#3375 = CARTESIAN_POINT ( 'NONE',  ( -10.81189881249999907, -6.242252689847864744, -186.6562500020484094 ) ) ;
#3376 = CARTESIAN_POINT ( 'NONE',  ( 10.81189881249999551, -6.242252689847874514, -15.15625000204837036 ) ) ;
#3377 = CARTESIAN_POINT ( 'NONE',  ( -10.00000000000051337, 5.773502691895962435, -40.37499999999996447 ) ) ;
#3378 = FACE_OUTER_BOUND ( 'NONE', #6460, .T. ) ;
#3379 = CARTESIAN_POINT ( 'NONE',  ( 9.999999999999998224, 0.000000000000000000, -156.5000000000000000 ) ) ;
#3380 = CARTESIAN_POINT ( 'NONE',  ( 9.999999999999998224, 0.000000000000000000, -134.3750000040967905 ) ) ;
#3381 = CARTESIAN_POINT ( 'NONE',  ( 7.070501591499377789E-16, 11.54700538379251284, -169.6250000000000000 ) ) ;
#3382 = CARTESIAN_POINT ( 'NONE',  ( -5.000000000000003553, -8.660254037844383745, -62.49999999999997158 ) ) ;
#3384 = ORIENTED_EDGE ( 'NONE', *, *, #5674, .F. ) ;
#3383 = CARTESIAN_POINT ( 'NONE',  ( -10.81189881249999729, 6.242252689847871849, -90.90625000204838102 ) ) ;
#3385 = CARTESIAN_POINT ( 'NONE',  ( 0.000000000000000000, 0.000000000000000000, -200.0000000000000000 ) ) ;
#3386 = AXIS2_PLACEMENT_3D ( 'NONE', #25176, #5097, #29038 ) ;
#3387 = EDGE_LOOP ( 'NONE', ( #39891, #19721, #3869, #2794 ) ) ;
#3388 = EDGE_LOOP ( 'NONE', ( #29268, #29544, #38794, #1702 ) ) ;
#3389 = CARTESIAN_POINT ( 'NONE',  ( -5.405949406249996869, 9.363379034771805109, -30.84375000204836326 ) ) ;
#3390 = CARTESIAN_POINT ( 'NONE',  ( 10.81189881249999551, -6.242252689847874514, -25.65625000204839168 ) ) ;
#3391 = APPROVAL_ROLE ( '' ) ;
#3392 = CARTESIAN_POINT ( 'NONE',  ( 5.405949406249999534, 9.363379034771803333, -73.09375000204838102 ) ) ;
#3393 = DIRECTION ( 'NONE',  ( -0.000000000000000000, -0.000000000000000000, 1.000000000000000000 ) ) ;
#3394 = CARTESIAN_POINT ( 'NONE',  ( -10.81189881249999729, 6.242252689847871849, -189.7187500020484379 ) ) ;
#3395 = CARTESIAN_POINT ( 'NONE',  ( -2.293366432827344421E-15, -12.48450537969573659, -153.2187500020483810 ) ) ;
#3396 = EDGE_CURVE ( 'NONE', #3609, #16045, #19502, .T. ) ;
#3397 = CARTESIAN_POINT ( 'NONE',  ( -5.000000000000003553, -8.660254037844383745, -79.37500000409677625 ) ) ;
#3398 = VECTOR ( 'NONE', #23149, 1000.000000000000000 ) ;
#3399 = FACE_BOUND ( 'NONE', #39258, .T. ) ;
#3400 = CARTESIAN_POINT ( 'NONE',  ( 5.405949406249999534, 9.363379034771803333, -157.2812500020484094 ) ) ;
#3401 = CARTESIAN_POINT ( 'NONE',  ( -2.121150477449813534E-15, -11.54700538379251284, -1.250000004096749828 ) ) ;
#3402 = CARTESIAN_POINT ( 'NONE',  ( -9.999999999999998224, 1.224646799147353059E-15, -121.2500000000000000 ) ) ;
#3403 = CARTESIAN_POINT ( 'NONE',  ( -5.405949406249996869, 9.363379034771805109, -119.3437500020483810 ) ) ;
#3404 = CARTESIAN_POINT ( 'NONE',  ( 7.644554776091147741E-16, 12.48450537969573659, -95.65625000204838102 ) ) ;
#3405 = CARTESIAN_POINT ( 'NONE',  ( 10.81189881249999729, 0.000000000000000000, -106.3437500020483810 ) ) ;
#3406 = CARTESIAN_POINT ( 'NONE',  ( 10.81189881249999729, 0.000000000000000000, -74.84375000204838102 ) ) ;
#3407 = CARTESIAN_POINT ( 'NONE',  ( 5.405949406249992428, -9.363379034771808662, -87.28125000204838102 ) ) ;
#3408 = CARTESIAN_POINT ( 'NONE',  ( 9.999999999999998224, 0.000000000000000000, -161.3750000040967905 ) ) ;
#3409 = CARTESIAN_POINT ( 'NONE',  ( 7.070501591499376803E-16, 11.54700538379251284, -81.50000000409677625 ) ) ;
#3410 = CARTESIAN_POINT ( 'NONE',  ( -5.405949406249996869, 9.363379034771805109, -163.0312500020484094 ) ) ;
#3411 = CARTESIAN_POINT ( 'NONE',  ( -10.81189881249999729, 6.242252689847871849, -183.9062500020484094 ) ) ;
#3412 = CARTESIAN_POINT ( 'NONE',  ( 7.070501591499377789E-16, 11.54700538379251284, -158.0000000040968189 ) ) ;
#3413 = DIRECTION ( 'NONE',  ( -0.000000000000000000, -0.000000000000000000, -1.000000000000000000 ) ) ;
#3414 = CARTESIAN_POINT ( 'NONE',  ( 5.405949406249992428, -9.363379034771808662, -7.593750002048343717 ) ) ;
#3415 = DIRECTION ( 'NONE',  ( -0.000000000000000000, -0.000000000000000000, -1.000000000000000000 ) ) ;
#3416 = CARTESIAN_POINT ( 'NONE',  ( -2.293366432827344421E-15, -12.48450537969573659, -114.2187500020483668 ) ) ;
#3417 = CARTESIAN_POINT ( 'NONE',  ( -9.999999999999998224, 1.224646799147353059E-15, -77.74999999999998579 ) ) ;
#3418 = CARTESIAN_POINT ( 'NONE',  ( 10.81189881249999551, -6.242252689847874514, -12.15625000204836859 ) ) ;
#3419 = CARTESIAN_POINT ( 'NONE',  ( 4.999999999999992006, -8.660254037844389075, -91.12500000409677625 ) ) ;
#3420 =( BOUNDED_CURVE ( )  B_SPLINE_CURVE ( 2, ( #38062, #15165, #15379, #28363, #8929, #33080, #13405 ),
 .UNSPECIFIED., .F., .F. ) 
 B_SPLINE_CURVE_WITH_KNOTS ( ( 3, 2, 2, 3 ),
 ( 0.08208955223880604057, 0.08333333333333339810, 0.08457711442786078337, 0.08582089552238814090 ),
 .UNSPECIFIED. ) 
 CURVE ( )  GEOMETRIC_REPRESENTATION_ITEM ( )  RATIONAL_B_SPLINE_CURVE ( ( 0.9999999999999924505, 0.8660254037844461461, 1.000000000000000000, 0.8660254037844387076, 1.000000000000000000, 0.8660254037844297148, 1.000000000000008882 ) ) 
 REPRESENTATION_ITEM ( '' )  );
#3421 = CARTESIAN_POINT ( 'NONE',  ( 7.644554776091147741E-16, 12.48450537969573659, -109.1562500020483810 ) ) ;
#3422 = CARTESIAN_POINT ( 'NONE',  ( 5.405949406249992428, -9.363379034771808662, -88.78125000204838102 ) ) ;
#3423 = ORIENTED_EDGE ( 'NONE', *, *, #31811, .T. ) ;
#3424 = CARTESIAN_POINT ( 'NONE',  ( -5.000000000000003553, -8.660254037844383745, -85.37500000409677625 ) ) ;
#3425 = CARTESIAN_POINT ( 'NONE',  ( -5.000000000000003553, -8.660254037844383745, -140.8750000040967905 ) ) ;
#3426 = CARTESIAN_POINT ( 'NONE',  ( -5.405949406250003975, -9.363379034771801557, -39.34375000204837391 ) ) ;
#3427 = ORIENTED_EDGE ( 'NONE', *, *, #18315, .F. ) ;
#3428 = CARTESIAN_POINT ( 'NONE',  ( -9.999999999999998224, 1.224646799147353059E-15, -11.74999999999995559 ) ) ;
#3429 = EDGE_CURVE ( 'NONE', #32487, #7438, #6080, .T. ) ;
#3430 = CARTESIAN_POINT ( 'NONE',  ( 5.000000000000000000, 8.660254037844385522, -142.7500000000000000 ) ) ;
#3431 = CARTESIAN_POINT ( 'NONE',  ( 0.000000000000000000, 0.000000000000000000, -200.0000000000000000 ) ) ;
#3432 = CARTESIAN_POINT ( 'NONE',  ( 4.999999999999992006, -8.660254037844389075, -8.625000004096744277 ) ) ;
#3433 = AXIS2_PLACEMENT_3D ( 'NONE', #8938, #6125, #25770 ) ;
#3434 = CARTESIAN_POINT ( 'NONE',  ( -10.00000000000000000, -5.773502691896251982, -187.1250000000000284 ) ) ;
#3436 = ORIENTED_EDGE ( 'NONE', *, *, #39059, .T. ) ;
#3435 = CARTESIAN_POINT ( 'NONE',  ( 10.81189881249999551, -6.242252689847874514, -120.1562500020483810 ) ) ;
#3437 = CARTESIAN_POINT ( 'NONE',  ( 9.999999999999998224, 0.000000000000000000, -74.37500000409677625 ) ) ;
#3438 = ORIENTED_EDGE ( 'NONE', *, *, #32558, .T. ) ;
#3439 = CARTESIAN_POINT ( 'NONE',  ( 10.81189881249999907, 6.242252689847868297, -43.40625000204837391 ) ) ;
#3440 = CALENDAR_DATE ( 2026, 28, 9 ) ;
#3441 = CARTESIAN_POINT ( 'NONE',  ( -10.81189881249999729, 1.324075727343319199E-15, -93.59375000204838102 ) ) ;
#3442 = CARTESIAN_POINT ( 'NONE',  ( -5.405949406249996869, 9.363379034771805109, -127.0312500020483952 ) ) ;
#3443 = ORIENTED_EDGE ( 'NONE', *, *, #13647, .T. ) ;
#3444 = CARTESIAN_POINT ( 'NONE',  ( 9.999999999999998224, 0.000000000000000000, -200.0000000000000000 ) ) ;
#3445 = CARTESIAN_POINT ( 'NONE',  ( 10.00000000000025402, -5.773502691896113426, -125.5000000040967763 ) ) ;
#3446 = CARTESIAN_POINT ( 'NONE',  ( 10.81189881249999551, -6.242252689847874514, -181.6562500020484379 ) ) ;
#3447 = CARTESIAN_POINT ( 'NONE',  ( 9.999999999999998224, 0.000000000000000000, -146.3750000040967905 ) ) ;
#3448 = EDGE_CURVE ( 'NONE', #21453, #419, #12086, .T. ) ;
#3449 = CARTESIAN_POINT ( 'NONE',  ( -5.405949406249996869, 9.363379034771805109, -132.8437500020484094 ) ) ;
#3450 = CARTESIAN_POINT ( 'NONE',  ( 5.405949406249999534, 9.363379034771803333, -100.0937500020483810 ) ) ;
#3451 = CARTESIAN_POINT ( 'NONE',  ( -1.040834085586084257E-14, -145.0000000000000000, 22.49999999999999289 ) ) ;
#3452 = CARTESIAN_POINT ( 'NONE',  ( 7.644554776091147741E-16, 12.48450537969573659, -107.6562500020483810 ) ) ;
#3453 = CARTESIAN_POINT ( 'NONE',  ( -2.121150477449813534E-15, -11.54700538379251284, -182.7500000040967905 ) ) ;
#3454 = CARTESIAN_POINT ( 'NONE',  ( 5.405949406249999534, 9.363379034771803333, -112.0937500020483810 ) ) ;
#3455 = CARTESIAN_POINT ( 'NONE',  ( 5.405949406249999534, 9.363379034771803333, -187.2812500020484094 ) ) ;
#3456 =( BOUNDED_CURVE ( )  B_SPLINE_CURVE ( 2, ( #26183, #26393, #32245, #6121, #39544, #36104, #2885 ),
 .UNSPECIFIED., .F., .F. ) 
 B_SPLINE_CURVE_WITH_KNOTS ( ( 3, 2, 2, 3 ),
 ( 0.1231343283582089221, 0.1243781094527362935, 0.1256218905472636649, 0.1268656716417910224 ),
 .UNSPECIFIED. ) 
 CURVE ( )  GEOMETRIC_REPRESENTATION_ITEM ( )  RATIONAL_B_SPLINE_CURVE ( ( 1.000000000000002887, 0.8660254037844355990, 1.000000000000000000, 0.8660254037844387076, 1.000000000000000000, 0.8660254037844417052, 0.9999999999999970024 ) ) 
 REPRESENTATION_ITEM ( '' )  );
#3457 = CARTESIAN_POINT ( 'NONE',  ( -10.00000000000051337, 5.773502691895962435, -6.250000004096728290 ) ) ;
#3458 = CARTESIAN_POINT ( 'NONE',  ( -1.119103713019287571, 10.75960476264953769, -99.99999999999997158 ) ) ;
#3459 = CARTESIAN_POINT ( 'NONE',  ( 4.999999999999992006, -8.660254037844389075, -131.2499999999999716 ) ) ;
#3460 = CARTESIAN_POINT ( 'NONE',  ( 5.000000000000000000, 8.660254037844385522, -1.749999999999973799 ) ) ;
#3461 = CARTESIAN_POINT ( 'NONE',  ( 7.644554776091147741E-16, 12.48450537969573659, -56.46875000204837391 ) ) ;
#3462 = CARTESIAN_POINT ( 'NONE',  ( 5.405949406249999534, 9.363379034771803333, -47.59375000204838102 ) ) ;
#3463 = CARTESIAN_POINT ( 'NONE',  ( -10.00000000000000000, -5.773502691896251982, -183.0000000040967905 ) ) ;
#3464 = CARTESIAN_POINT ( 'NONE',  ( -10.81189881249999729, 1.324075727343319199E-15, -20.28125000204836326 ) ) ;
#3465 = CARTESIAN_POINT ( 'NONE',  ( 10.81189881249999907, 6.242252689847868297, -31.21875000204835260 ) ) ;
#3466 = CARTESIAN_POINT ( 'NONE',  ( -9.999999999999998224, 1.224646799147353059E-15, -145.2500000000000000 ) ) ;
#3467 = CARTESIAN_POINT ( 'NONE',  ( -5.405949406250003975, -9.363379034771801557, -138.3437500020484094 ) ) ;
#3468 = CARTESIAN_POINT ( 'NONE',  ( 10.00000000000000000, 5.773502691896255534, -102.3749999999999858 ) ) ;
#3469 = CARTESIAN_POINT ( 'NONE',  ( 10.81189881249999729, 0.000000000000000000, -33.03125000204837391 ) ) ;
#3470 = FACE_OUTER_BOUND ( 'NONE', #14717, .T. ) ;
#3471 = CARTESIAN_POINT ( 'NONE',  ( 4.999999999999992006, -8.660254037844389075, -68.24999999999997158 ) ) ;
#3472 = CARTESIAN_POINT ( 'NONE',  ( 5.405949406249992428, -9.363379034771808662, -130.7812500020483810 ) ) ;
#3473 = CARTESIAN_POINT ( 'NONE',  ( -10.81189881249999729, 1.324075727343319199E-15, -113.2812500020483952 ) ) ;
#3474 = ORIENTED_EDGE ( 'NONE', *, *, #8536, .F. ) ;
#3475 = CARTESIAN_POINT ( 'NONE',  ( -9.999999999999227285, -5.773502691896698735, -128.6249999999999716 ) ) ;
#3476 = CARTESIAN_POINT ( 'NONE',  ( 9.999999999999996447, -5.773502691896262640, -109.0000000040967763 ) ) ;
#3477 = DIRECTION ( 'NONE',  ( 0.000000000000000000, 0.000000000000000000, 1.000000000000000000 ) ) ;
#3478 = CARTESIAN_POINT ( 'NONE',  ( -2.293366432827344421E-15, -12.48450537969573659, -69.21875000204839523 ) ) ;
#3479 = EDGE_LOOP ( 'NONE', ( #37947, #38840, #19933, #6103 ) ) ;
#3480 = CARTESIAN_POINT ( 'NONE',  ( -10.00000000000000000, -5.773502691896251982, -31.12499999999995381 ) ) ;
#3481 = CARTESIAN_POINT ( 'NONE',  ( -9.999999999999998224, 5.773502691896259087, -21.25000000409676204 ) ) ;
#3482 = CARTESIAN_POINT ( 'NONE',  ( 5.405949406249999534, 9.363379034771803333, -40.28125000204838102 ) ) ;
#3483 = CARTESIAN_POINT ( 'NONE',  ( 10.00000000000102318, -5.773502691895667560, -2.124999999999920064 ) ) ;
#3484 = CARTESIAN_POINT ( 'NONE',  ( 9.999999999999998224, 0.000000000000000000, -38.37500000409676915 ) ) ;
#3485 = FACE_OUTER_BOUND ( 'NONE', #38048, .T. ) ;
#3486 = AXIS2_PLACEMENT_3D ( 'NONE', #5561, #22176, #6410 ) ;
#3487 = CARTESIAN_POINT ( 'NONE',  ( 5.405949406249999534, 9.363379034771803333, -145.2812500020483810 ) ) ;
#3488 = CARTESIAN_POINT ( 'NONE',  ( -9.999999999999998224, 1.224646799147353059E-15, -16.24999999999995737 ) ) ;
#3489 = VERTEX_POINT ( 'NONE', #39776 ) ;
#3490 = VERTEX_POINT ( 'NONE', #23395 ) ;
#3491 = ORIENTED_EDGE ( 'NONE', *, *, #5970, .T. ) ;
#3492 = CARTESIAN_POINT ( 'NONE',  ( 9.999999999999998224, 0.000000000000000000, -200.0000000000000000 ) ) ;
#3493 = CARTESIAN_POINT ( 'NONE',  ( -5.405949406250003975, -9.363379034771801557, -171.3437500020484094 ) ) ;
#3494 = CARTESIAN_POINT ( 'NONE',  ( 10.81189881249999907, 6.242252689847868297, -23.71875000204836326 ) ) ;
#3495 = DIRECTION ( 'NONE',  ( -0.000000000000000000, -0.000000000000000000, -1.000000000000000000 ) ) ;
#3496 = ADVANCED_FACE ( 'NONE', ( #16037 ), #29232, .T. ) ;
#3497 = CARTESIAN_POINT ( 'NONE',  ( 10.81189881249999729, 6.242252689847867408, -152.7187500020483810 ) ) ;
#3498 = CARTESIAN_POINT ( 'NONE',  ( 10.81189881249999729, 0.000000000000000000, -148.3437500020483810 ) ) ;
#3499 = EDGE_CURVE ( 'NONE', #107, #10156, #14500, .T. ) ;
#3500 = CARTESIAN_POINT ( 'NONE',  ( -5.000000000000003553, -8.660254037844383745, -88.37500000409677625 ) ) ;
#3501 = CARTESIAN_POINT ( 'NONE',  ( -5.405949406249996869, 9.363379034771805109, -125.3437500020483952 ) ) ;
#3502 = CARTESIAN_POINT ( 'NONE',  ( -10.81189881249999907, -6.242252689847864744, -134.1562500020483810 ) ) ;
#3503 = CARTESIAN_POINT ( 'NONE',  ( 5.405949406249992428, -9.363379034771808662, -7.593750002048343717 ) ) ;
#3505 = EDGE_CURVE ( 'NONE', #20876, #17374, #37182, .T. ) ;
#3504 = CARTESIAN_POINT ( 'NONE',  ( -5.405949406249996869, 9.363379034771805109, -137.3437500020484094 ) ) ;
#3506 = FACE_OUTER_BOUND ( 'NONE', #9648, .T. ) ;
#3507 = CARTESIAN_POINT ( 'NONE',  ( -9.999999999999998224, 1.224646799147353059E-15, -200.0000000000000000 ) ) ;
#3508 = CARTESIAN_POINT ( 'NONE',  ( -9.999999999999998224, 5.773502691896259087, -160.3749999999999716 ) ) ;
#3509 = CARTESIAN_POINT ( 'NONE',  ( -4.999999999999996447, 8.660254037844387298, -99.37500000409679046 ) ) ;
#3510 = AXIS2_PLACEMENT_3D ( 'NONE', #24094, #26207, #6773 ) ;
#3511 = CARTESIAN_POINT ( 'NONE',  ( 10.81189881249999729, 0.000000000000000000, -73.34375000204838102 ) ) ;
#3512 = CARTESIAN_POINT ( 'NONE',  ( 10.81189881249999907, 6.242252689847868297, -44.90625000204836681 ) ) ;
#3513 = CARTESIAN_POINT ( 'NONE',  ( 10.81189881249999551, -6.242252689847874514, -55.46875000204837391 ) ) ;
#3514 = LINE ( 'NONE', #290, #32334 ) ;
#3515 = CARTESIAN_POINT ( 'NONE',  ( 5.405949406249992428, -9.363379034771808662, -165.0937500020484094 ) ) ;
#3516 = CARTESIAN_POINT ( 'NONE',  ( 4.999999999999992006, -8.660254037844389075, -126.7499999999999716 ) ) ;
#3517 = CARTESIAN_POINT ( 'NONE',  ( -10.81189881249999729, 6.242252689847871849, -137.4062500020484094 ) ) ;
#3518 = CC_DESIGN_PERSON_AND_ORGANIZATION_ASSIGNMENT ( #27381, #2134, ( #2800 ) ) ;
#3519 = DIRECTION ( 'NONE',  ( -0.000000000000000000, -0.000000000000000000, 1.000000000000000000 ) ) ;
#3520 = CARTESIAN_POINT ( 'NONE',  ( 10.00000000000000000, 5.773502691896255534, -117.7500000040967905 ) ) ;
#3521 = CARTESIAN_POINT ( 'NONE',  ( 9.999999999999996447, -5.773502691896262640, -90.62499999999998579 ) ) ;
#3522 = ORIENTED_EDGE ( 'NONE', *, *, #4036, .T. ) ;
#3523 = CARTESIAN_POINT ( 'NONE',  ( -5.405949406250003975, -9.363379034771801557, -111.5312500020483810 ) ) ;
#3524 = CARTESIAN_POINT ( 'NONE',  ( -5.000000000000003553, -8.660254037844383745, -133.3750000040967905 ) ) ;
#3525 = CARTESIAN_POINT ( 'NONE',  ( 9.999999999999998224, 0.000000000000000000, -185.0000000000000000 ) ) ;
#3526 = CARTESIAN_POINT ( 'NONE',  ( 5.405949406249999534, 9.363379034771803333, -166.2812500020484094 ) ) ;
#3527 = CARTESIAN_POINT ( 'NONE',  ( -5.000000000000003553, -8.660254037844383745, -44.87500000409677625 ) ) ;
#3528 = EDGE_CURVE ( 'NONE', #6885, #20093, #7452, .T. ) ;
#3529 = CYLINDRICAL_SURFACE ( 'NONE', #2176, 9.999999999999998224 ) ;
#3530 = CARTESIAN_POINT ( 'NONE',  ( 10.81189881249999551, -6.242252689847874514, -52.65625000204837391 ) ) ;
#3531 = DIRECTION ( 'NONE',  ( -0.000000000000000000, -0.000000000000000000, 1.000000000000000000 ) ) ;
#3532 = CARTESIAN_POINT ( 'NONE',  ( 10.81189881249999551, -6.242252689847874514, -162.1562500020484379 ) ) ;
#3533 = EDGE_CURVE ( 'NONE', #28805, #3574, #7624, .T. ) ;
#3534 = CARTESIAN_POINT ( 'NONE',  ( 10.81189881249999907, 6.242252689847868297, -137.7187500020484094 ) ) ;
#3535 = CARTESIAN_POINT ( 'NONE',  ( 9.999999999999998224, 0.000000000000000000, -158.0000000000000000 ) ) ;
#3536 = CARTESIAN_POINT ( 'NONE',  ( 9.999999999999998224, 0.000000000000000000, -150.5000000000000000 ) ) ;
#3537 = ADVANCED_FACE ( 'NONE', ( #36971 ), #945, .T. ) ;
#3538 = ORIENTED_EDGE ( 'NONE', *, *, #35604, .F. ) ;
#3539 = CARTESIAN_POINT ( 'NONE',  ( -10.00000000000076916, 5.773502691895813221, -114.2500000040967905 ) ) ;
#3540 = APPROVAL_PERSON_ORGANIZATION ( #7958, #31498, #31485 ) ;
#3542 = VERTEX_POINT ( 'NONE', #1157 ) ;
#3541 = CARTESIAN_POINT ( 'NONE',  ( -10.81189881249999729, 1.324075727343319199E-15, -66.78125000204838102 ) ) ;
#3543 =( NAMED_UNIT ( * ) SI_UNIT ( $, .STERADIAN. ) SOLID_ANGLE_UNIT ( ) );
#3545 = VERTEX_POINT ( 'NONE', #21206 ) ;
#3544 = CARTESIAN_POINT ( 'NONE',  ( -10.81189881249999729, 6.242252689847871849, -122.2187500020483810 ) ) ;
#3546 = EDGE_CURVE ( 'NONE', #34431, #19091, #738, .T. ) ;
#3547 =( BOUNDED_CURVE ( )  B_SPLINE_CURVE ( 2, ( #22379, #36806, #13691 ),
 .UNSPECIFIED., .F., .F. ) 
 B_SPLINE_CURVE_WITH_KNOTS ( ( 3, 3 ),
 ( 0.9888059701492539766, 0.9894244334336458335 ),
 .UNSPECIFIED. ) 
 CURVE ( )  GEOMETRIC_REPRESENTATION_ITEM ( )  RATIONAL_B_SPLINE_CURVE ( ( 0.9999999999999761302, 0.9333818714843358233, 0.9330147364001334376 ) ) 
 REPRESENTATION_ITEM ( '' )  );
#3548 = ORIENTED_EDGE ( 'NONE', *, *, #31857, .F. ) ;
#3549 = CARTESIAN_POINT ( 'NONE',  ( 5.405949406249992428, -9.363379034771808662, -19.59375000204835615 ) ) ;
#3550 = CARTESIAN_POINT ( 'NONE',  ( -5.405949406250003975, -9.363379034771801557, -0.5312500020483723606 ) ) ;
#3551 = AXIS2_PLACEMENT_3D ( 'NONE', #18996, #32180, #28298 ) ;
#3552 = CARTESIAN_POINT ( 'NONE',  ( -10.81189881249999907, -6.242252689847864744, -43.96875000204835970 ) ) ;
#3553 = CARTESIAN_POINT ( 'NONE',  ( -9.999999999999998224, 1.224646799147353059E-15, -89.74999999999998579 ) ) ;
#3554 = CARTESIAN_POINT ( 'NONE',  ( -9.999999999999998224, 5.773502691896259087, -29.87499999999995737 ) ) ;
#3555 = CARTESIAN_POINT ( 'NONE',  ( 7.644554776091147741E-16, 12.48450537969573659, -182.4687500020484094 ) ) ;
#3556 = CARTESIAN_POINT ( 'NONE',  ( -10.81189881249999729, 1.324075727343319199E-15, -167.0937500020484094 ) ) ;
#3557 = CARTESIAN_POINT ( 'NONE',  ( 5.405949406249999534, 9.363379034771803333, -146.5937500020483810 ) ) ;
#3559 = ADVANCED_FACE ( 'NONE', ( #24685 ), #24468, .T. ) ;
#3558 = CARTESIAN_POINT ( 'NONE',  ( -2.293366432827344421E-15, -12.48450537969573659, -160.7187500020483810 ) ) ;
#3560 = CARTESIAN_POINT ( 'NONE',  ( -9.999999999999998224, 0.000000000000000000, -99.99999999999998579 ) ) ;
#3561 = CARTESIAN_POINT ( 'NONE',  ( 9.999999999999884537, 5.773502691896319483, -194.2500000040968189 ) ) ;
#3562 = CARTESIAN_POINT ( 'NONE',  ( -4.999999999999996447, 8.660254037844387298, -184.5000000000000000 ) ) ;
#3563 = CARTESIAN_POINT ( 'NONE',  ( -2.293366432827344421E-15, -12.48450537969573659, -93.21875000204838102 ) ) ;
#3564 = CARTESIAN_POINT ( 'NONE',  ( 9.999999999999998224, 0.000000000000000000, -167.3750000040967905 ) ) ;
#3565 = CARTESIAN_POINT ( 'NONE',  ( 10.81189881249999729, 0.000000000000000000, -69.03125000204838102 ) ) ;
#3566 = FACE_OUTER_BOUND ( 'NONE', #31635, .T. ) ;
#3567 = CARTESIAN_POINT ( 'NONE',  ( -10.81189881249999729, 6.242252689847871849, -189.7187500020484379 ) ) ;
#3568 = CARTESIAN_POINT ( 'NONE',  ( 10.81189881249999551, -6.242252689847874514, -121.6562500020483952 ) ) ;
#3569 = CARTESIAN_POINT ( 'NONE',  ( -10.81189881249999729, 6.242252689847871849, -161.4062500020483810 ) ) ;
#3570 = CARTESIAN_POINT ( 'NONE',  ( -5.405949406250003975, -9.363379034771801557, -54.53125000204836681 ) ) ;
#3571 = CARTESIAN_POINT ( 'NONE',  ( 5.000000000000000000, 8.660254037844385522, -141.6250000040967905 ) ) ;
#3572 = CARTESIAN_POINT ( 'NONE',  ( 4.999999999999992006, -8.660254037844389075, -113.2499999999999858 ) ) ;
#3573 = VECTOR ( 'NONE', #36462, 1000.000000000000000 ) ;
#3574 = VERTEX_POINT ( 'NONE', #31157 ) ;
#3575 = CARTESIAN_POINT ( 'NONE',  ( 10.81189881249999551, -6.242252689847874514, -135.1562500020483810 ) ) ;
#3576 = CARTESIAN_POINT ( 'NONE',  ( 5.405949406249992428, -9.363379034771808662, -147.2812500020483810 ) ) ;
#3577 = LOCAL_TIME ( 11, 57, 6.000000000000000000, #6001 ) ;
#3578 = CARTESIAN_POINT ( 'NONE',  ( 5.405949406249999534, 9.363379034771803333, -185.7812500020484094 ) ) ;
#3579 = CARTESIAN_POINT ( 'NONE',  ( 5.000000000000000000, 8.660254037844385522, -131.1250000040967620 ) ) ;
#3580 = CARTESIAN_POINT ( 'NONE',  ( 5.405949406249999534, 9.363379034771803333, -85.09375000204836681 ) ) ;
#3581 = ORIENTED_EDGE ( 'NONE', *, *, #17700, .F. ) ;
#3582 = CARTESIAN_POINT ( 'NONE',  ( -4.999999999999996447, 8.660254037844387298, -59.99999999999997158 ) ) ;
#3583 = CARTESIAN_POINT ( 'NONE',  ( -2.293366432827344421E-15, -12.48450537969573659, -180.2187500020484094 ) ) ;
#3584 = CARTESIAN_POINT ( 'NONE',  ( 9.999999999999996447, -5.773502691896262640, -70.00000000409679046 ) ) ;
#3585 = CARTESIAN_POINT ( 'NONE',  ( 9.999999999999994671, -5.773502691896262640, -171.6250000000000000 ) ) ;
#3586 = FACE_OUTER_BOUND ( 'NONE', #2443, .T. ) ;
#3587 = CARTESIAN_POINT ( 'NONE',  ( 7.644554776091147741E-16, 12.48450537969573659, -80.65625000204839523 ) ) ;
#3588 = CARTESIAN_POINT ( 'NONE',  ( 5.405949406249999534, 9.363379034771803333, -62.78125000204837391 ) ) ;
#3589 =( BOUNDED_CURVE ( )  B_SPLINE_CURVE ( 2, ( #41800, #42435, #12442, #35568, #35355, #42223, #21753 ),
 .UNSPECIFIED., .F., .F. ) 
 B_SPLINE_CURVE_WITH_KNOTS ( ( 3, 2, 2, 3 ),
 ( 0.4104477611940299253, 0.4116915422885572551, 0.4129353233830846959, 0.4141791044776120256 ),
 .UNSPECIFIED. ) 
 CURVE ( )  GEOMETRIC_REPRESENTATION_ITEM ( )  RATIONAL_B_SPLINE_CURVE ( ( 0.9999999999999940048, 0.8660254037844447028, 1.000000000000000000, 0.8660254037844387076, 1.000000000000000000, 0.8660254037844267172, 1.000000000000011990 ) ) 
 REPRESENTATION_ITEM ( '' )  );
#3590 = EDGE_CURVE ( 'NONE', #19091, #33541, #1590, .T. ) ;
#3591 = CARTESIAN_POINT ( 'NONE',  ( -5.000000000000003553, -8.660254037844383745, -56.87500000409676204 ) ) ;
#3592 = CARTESIAN_POINT ( 'NONE',  ( -2.293366432827344421E-15, -12.48450537969573659, -7.718750002048357040 ) ) ;
#3593 = CARTESIAN_POINT ( 'NONE',  ( -2.121150477449813534E-15, -11.54700538379251284, -137.7500000040967905 ) ) ;
#3594 = CARTESIAN_POINT ( 'NONE',  ( 10.81189881249999551, -6.242252689847874514, -184.6562500020484094 ) ) ;
#3595 = VECTOR ( 'NONE', #2485, 1000.000000000000000 ) ;
#3596 = CARTESIAN_POINT ( 'NONE',  ( 10.81189881249999551, -6.242252689847874514, -13.65625000204837036 ) ) ;
#3597 = CARTESIAN_POINT ( 'NONE',  ( -4.999999999999996447, 8.660254037844387298, -40.49999999999997868 ) ) ;
#3598 = DIRECTION ( 'NONE',  ( -0.7071067811865483499, 8.659560562354942719E-17, 0.7071067811865466846 ) ) ;
#3599 = DIRECTION ( 'NONE',  ( -1.000000000000000000, 0.000000000000000000, 0.000000000000000000 ) ) ;
#3600 = CARTESIAN_POINT ( 'NONE',  ( -4.999999999999996447, 8.660254037844387298, -177.3750000040967905 ) ) ;
#3601 =( BOUNDED_CURVE ( )  B_SPLINE_CURVE ( 2, ( #35125, #20928, #2535, #15454, #21945, #12217, #25409 ),
 .UNSPECIFIED., .F., .F. ) 
 B_SPLINE_CURVE_WITH_KNOTS ( ( 3, 2, 2, 3 ),
 ( 0.2723880597014926574, 0.2736318407960199872, 0.2748756218905473725, 0.2761194029850747578 ),
 .UNSPECIFIED. ) 
 CURVE ( )  GEOMETRIC_REPRESENTATION_ITEM ( )  RATIONAL_B_SPLINE_CURVE ( ( 0.9999999999999880096, 0.8660254037844506980, 1.000000000000000000, 0.8660254037844387076, 1.000000000000000000, 0.8660254037844267172, 1.000000000000011990 ) ) 
 REPRESENTATION_ITEM ( '' )  );
#3602 = CARTESIAN_POINT ( 'NONE',  ( 4.999999999999992006, -8.660254037844389075, -168.7500000000000000 ) ) ;
#3603 = CARTESIAN_POINT ( 'NONE',  ( -9.999999999999998224, 1.224646799147353059E-15, -138.1250000040967620 ) ) ;
#3605 = VERTEX_POINT ( 'NONE', #30519 ) ;
#3604 = CARTESIAN_POINT ( 'NONE',  ( 5.405949406249999534, 9.363379034771803333, -92.78125000204838102 ) ) ;
#3606 = CARTESIAN_POINT ( 'NONE',  ( 9.999999999999998224, 0.000000000000000000, -83.37500000409677625 ) ) ;
#3608 = ORIENTED_EDGE ( 'NONE', *, *, #2495, .T. ) ;
#3607 = CARTESIAN_POINT ( 'NONE',  ( -9.999999999999479527, -5.773502691896549521, -70.12499999999998579 ) ) ;
#3609 = VERTEX_POINT ( 'NONE', #11483 ) ;
#3610 = CARTESIAN_POINT ( 'NONE',  ( 10.81189881249999907, 6.242252689847868297, -34.21875000204835260 ) ) ;
#3611 = CARTESIAN_POINT ( 'NONE',  ( -10.81189881249999729, 1.324075727343319199E-15, -18.78125000204835970 ) ) ;
#3612 =( BOUNDED_CURVE ( )  B_SPLINE_CURVE ( 2, ( #27385, #11768, #27169, #33870, #30212, #8344, #21705, #38111, #38321, #26954, #10541, #28197, #17014, #20263, #1872, #40521, #24969, #31436, #41330, #8555, #33451, #4084, #40109, #5311, #18463, #23727, #30631, #30426, #31651, #36878, #14186, #7322, #18245, #2085, #7532, #37089, #28414, #15215, #857, #41552, #11983, #20472, #25179, #10965, #24754, #3879, #40312, #4296, #648, #21495, #33660, #13974, #10752, #23944, #20685, #37901, #34677, #5099, #32495, #29041, #12820, #26011, #31870, #41756, #39163, #35311, #28625, #35930, #22770, #2301, #5953, #5741, #29244, #12191, #2709, #15427, #25382, #38529, #32285, #9595, #18894, #32074, #22137, #38748, #25800, #6161, #22555, #2923, #8971, #16053, #19103, #32699, #35731, #6371, #2509, #15633, #28835, #19301, #41966, #19515, #15841, #16259, #12400, #9177, #42179, #12606, #25593, #22348, #26220, #35524, #42388, #38956, #9390, #3130, #29458, #42601, #13027, #8762, #21918, #35098, #5523, #18673, #36558, #36771, #958, #39369, #6784, #325, #29673, #3342, #7208, #20360, #33550, #16474, #17328, #3555, #117, #19728, #13239, #33128, #3975, #17115, #30531, #36351, #40210, #30315, #9805, #13658, #40004, #16899, #26426, #750, #19939, #30101, #3766, #16689, #23626, #13872, #36985, #39577, #27067, #10642, #10012, #23833, #23190, #7004, #14076, #29885, #7421, #13444, #26640, #20571, #22984, #33761, #32909, #4184, #39789, #36141, #20155, #10222, #23409, #6572, #33345, #540, #26849, #10435, #27491, #7856, #8068, #20787, #34403, #31595, #8496, #4612, #14727, #27273, #34830, #18188, #34194, #7637, #4822, #30737, #31380, #11067, #21218, #17536, #41274, #5043, #28141, #11494, #1814, #14941, #2028, #27919, #21649, #11282, #10856, #11710, #37843, #24909, #38056, #8285, #24268, #21432, #5254, #17969, #18406, #1598, #37188, #24477, #31169, #37628, #40411, #33976, #24047, #41050, #40625, #4397, #40843, #37414, #1168, #24697, #21005, #34617, #14291, #17753, #30948, #1381, #14511, #27705, #35044, #42336, #29196, #8711, #12345, #12139, #35679, #5471, #9128, #21865, #31817, #39108, #18621, #19466, #11927, #41701, #28571, #2449, #32232, #12559, #28988, #38906, #2251, #9335, #25544, #9545, #42127, #2871, #25332, #15371, #38477, #22504, #8921, #28783, #25753, #6107, #22083, #2658, #5692, #35470, #35258, #15792, #18841, #12766, #25960, #32022, #15582, #19254, #41914, #38694, #22298, #32444, #16001, #22719, #5894, #35884, #19050, #6319, #38264, #32651, #15157, #28355, #41493, #25120, #36719, #29618, #39739, #36089, #17064, #23572, #3927, #9755, #7158, #26379, #36511, #10174, #23139, #30047, #494, #701, #33071, #19888, #10591, #13608, #61, #26801, #40160, #26588, #30262, #20103, #12972, #20310, #9961, #16636, #26169, #33294, #13820, #33503, #20521, #39316, #6524, #10383, #42548, #3079, #39951, #23359, #27013, #23778, #36931, #7375, #16206, #13186, #22936, #29408, #19674, #32861, #275, #39530, #3292, #16420, #6948, #36303, #6733, #3497, #3720, #29838, #13396, #16849, #24859, #30895, #4772, #31117, #17920, #14683, #7586, #27870, #1332, #14896, #1550, #21385, #17491, #20739, #37138, #41004, #27442, #18140, #27653, #34568, #11448, #33926, #24648, #40794, #4350, #14240, #8454, #30684, #4560, #37791, #8236, #1115, #21166, #24214, #11235, #40364, #34354, #37365, #31336, #1767, #7808, #40579, #4999, #20956, #23997, #10805, #28095, #41222, #11660, #11020, #38009, #34142, #17701, #14024, #14463, #24434, #33709, #37577, #8022, #4134, #17275, #30480, #909, #27219, #22249, #41862, #28303, #25705, #2194, #12300, #28736, #41657, #5845, #19001, #19208, #8873, #38431, #29150, #32186, #5426, #2613, #15952, #2403, #15743, #18787, #25497, #12512, #28525, #35209, #31549, #25074, #15328, #22037, #32397, #5639, #21817, #2820, #35419, #15534, #34998, #28943, #38646, #38856, #9282, #34784, #31976, #12093, #31766, #42080, #1982, #22454, #18578, #42289, #9081, #15108, #25908, #35631, #6058, #12710, #41441, #39060, #18360, #25286, #21605, #5205, #11878, #38219, #8664, #17017, #3669, #32810, #443, #6479, #29355, #19625, #36253, #13560, #13772, #6896, #7112, #12922, #26751, #30215, #39271, #33243, #16159, #19835, #26957, #9705, #36460, #42494, #3241, #20266, #23305, #3449, #22884, #10127, #16585, #39903, #32607, #26116, #10334, #36043, #36671, #23522, #3032, #6683, #16367, #29997, #29566, #29787, #12, #13135, #26331, #33019, #33454, #39482, #3882, #652, #228, #20049, #9915, #16798, #9498, #23091, #22666, #13350, #35838, #6270, #19416, #26541, #39690, #860, #7966, #33875, #24591, #34084, #27820, #17868, #27173, #21115, #4088, #7756, #20689, #14841, #13976, #4719, #23948, #10968, #37525, #24383, #40315, #27604, #30634, #17649, #17228, #40744, #1066, #37740, #8184, #14189, #10756, #31064, #27388, #30430, #37092, #34303, #1497, #14632, #7535, #18090, #4299, #17438, #20476, #40525, #24164, #40953, #37310, #20901, #11397, #4506, #30844, #1281, #14410, #11186, #21331, #34520, #4943, #31284, #1714, #40112, #10545, #23730, #36881, #7326, #33663, #2143, #35583, #38591, #11825, #9032, #22406, #8822, #22196, #25235, #35157, #18950, #34945, #41607, #37958, #42030, #12041, #38381, #15278, #21554, #18307, #35371, #5798, #28252, #8612, #21978, #34734, #5583, #32137, #5156, #6012, #5370, #31496, #8403, #1928, #21767, #25446, #25025, #15055, #2568, #38168, #18736, #41390, #12460, #15697, #28896, #12253, #25653, #18523, #31928, #2356, #31712, #38809, #9237, #19161, #28476, #15483, #32351, #2775, #28687, #28038, #41166, #41815, #11605, #24813, #25862, #42664, #39438, #29522, #39017, #29955, #13088, #26288, #3197, #9454, #6226, #23257, #12667, #33410, #39641, #36202, #20004, #26495, #10081, #33196, #29106, #9871, #22837, #395, #13515, #22620, #23045, #12880, #36417, #19371, #6639, #35795, #32559, #2987, #19789, #3627, #26075, #16754, #7071, #32976, #29739, #16323, #6851, #26703, #16111, #39855, #3405, #10289, #186, #23476, #42453, #29307, #39226, #36624, #9664, #20220, #16540, #15902, #42242, #35999, #6434, #19577, #13306, #32760, #21286, #20432, #11136, #30381, #17394, #1237, #30800, #4037, #34041, #37051, #24119, #10500, #4461, #7488, #1449, #14584, #20640, #33617, #37256, #37478, #34260, #3835, #17604, #40909, #30591, #30167, #7922, #14362, #21069, #4674, #23906, #607, #27772, #23688, #1022, #40069, #40694, #14142, #10925, #27343, #40477, #11351, #17824, #7278, #27129, #33828, #24544, #7707, #17183, #37695, #27560, #20857, #813, #24337, #31019, #8137, #26912, #36835, #16971, #10709, #13935, #13722, #40272, #4252, #18256, #12410, #18475, #1663, #38761, #5534, #8773, #15644, #27989, #9187, #31238, #31446, #5108, #21716, #21929, #18683, #15438, #8355, #28636, #31662, #28844, #31881, #22148, #1881, #21506, #37911, #2311, #28207, #18904, #28425, #35322, #12201, #34688, #41767, #41119, #15009, #41341, #34472, #11778, #25393, #24980, #5321, #38540, #8981, #38121, #35109, #8566, #11994, #11558, #5751, #34898, #32085, #2519, #2096, #15226, #41561, #25189, #24767, #38330, #41979, #25603, #4894, #18042, #14794, #29257, #25811, #2721, #38967, #16065, #20322, #6172, #9402, #13833, #19313, #16860, #35534, #39965, #23585, #40375, #3939, #505, #27027, #33516, #17077, #40172, #5962, #6960, #42401, #32506, #36732, #15853, #10603, #2936, #921, #20117, #30063, #29052, #22566, #42191, #3730, #23790, #12832, #36945, #14036, #33305, #7170, #22782, #30275, #26023, #30494, #714, #39175, #7387, #9609, #12618, #35943, #35744, #13621, #20534, #26813, #33723, #10395, #4146, #17290, #27232, #22358, #19114, #32297, #28314, #11033, #37803, #30697, #20968, #14907, #10817, #8249, #24227, #41016, #1345, #31131, #17502, #11460, #14474, #8466, #21617, #27669, #40591, #18152, #37378, #34154, #34368, #4363, #17932, #15119, #34796, #31561, #17714, #14252, #33941, #27455, #4572, #21396, #7821, #30909, #1777, #40807, #4784, #1129, #24872, #31347, #11672, #34581, #28106, #41234, #24010, #1564, #11247, #5011, #38022, #5216, #24445, #37590, #18372, #1994, #8034, #37152, #7598, #14694, #20753, #27883, #21178, #24661, #22260, #38656, #22678, #12721, #12310, #25508, #28747, #35008, #31776, #6069, #38230, #5438, #42090, #2413, #39070, #9509, #15545, #28535, #19218, #41667, #22047, #35429, #18590, #9294, #35641, #2206, #19427, #5651, #15338, #21829, #12102, #35220, #38865, #25297, #38440, #32408, #8884, #5857, #18799, #25919, #2830, #42300, #25716, #15964, #31987, #32196, #19011, #41873, #22464, #29160, #35848, #9093, #2623, #6281, #32617, #15755, #3042, #16170, #28953, #41455, #12523, #8675, #11890, #25085, #239, #39282, #664, #13361, #26553, #16596, #22897, #19637, #36682, #26127, #4097, #10344, #6906, #33465, #39914, #23532, #3891, #42505, #39701, #6489, #13783, #26966, #36053, #10137, #26341, #7122, #32821, #23317, #3251, #16378, #9715, #36471, #17026, #39493, #30225, #20486, #20060, #454, #29799, #13570, #20277, #29578, #40124, #33255, #10554, #26761, #23740, #13146, #23, #9924, #36893, #23103, #7337, #3681, #33672, #29365, #36265, #12932, #6696, #19847, #33031, #3461, #16809, #30008, #21341, #34745, #40964, #40327, #34529, #1075, #27832, #37968, #1292, #27183, #21564, #31076, #34315, #41176, #10769, #14200, #4953, #8413, #14421, #1509, #17660, #11407, #27400, #24823, #24601, #40536, #8194, #10979, #37102, #24175, #27615, #18100, #17239, #14643, #14853, #11197, #31295, #37750, #4309, #1726, #23958, #40755, #30439, #17448, #28050, #7545, #37322, #11615, #870, #13986, #20699, #33887, #7769, #30644, #24395, #17879, #20912, #34095, #4516, #30854, #37536, #7976, #21126, #4731, #5592, #28263, #18745, #6019, #38816, #15287, #41823, #5166, #22413, #32145, #28484, #9040, #5381, #38178, #2575, #18532, #31937, #8622, #42038, #15704, #28903, #38600, #12467, #25661, #18318, #25455, #35591, #2364, #15064, #9243, #35380, #38391, #19169, #5805, #31722, #18958, #31508, #15491, #1938, #22205, #21778, #28696, #12260, #41401, #11835, #25036, #12050, #34957, #2152, #41616, #25246, #8832, #21989, #35166, #24747, #21269, #5092, #11541, #37893, #18238, #14125, #27754, #7905, #11116, #14776, #24100, #31428, #27543, #24318, #27972, #37239, #40890, #40677, #21486, #34024, #37677, #7686, #17587, #20841, #24527, #1865, #37462, #14992, #34880, #11333, #41099, #1432, #8337, #21053, #8547, #34669, #8117, #24962, #28189, #41323, #34243, #30786, #4446, #11761, #4657, #38103, #34455, #21698, #5303, #1220, #18455, #14345, #4876, #1007, #17807, #27327, #40461, #31003, #14565, #10909, #18024, #31219, #1646, #22129, #9170, #38314, #32277, #35304, #29239, #42381, #5735, #18666, #38949, #31863, #12184, #12391, #42172, #12599, #25793, #8755, #9589, #38522, #35090, #11975, #5515, #25375, #29033, #15419, #2295, #22549, #28617, #25587, #21910, #2916, #9383, #32489, #41749, #35724, #8965, #22341, #38741, #18887, #15833, #6154, #12813, #32067, #2501, #39158, #19295, #15626, #16046, #26006, #35517, #22764, #5946, #41545, #35926, #28828, #41959, #25170, #6365, #19094, #2702, #31644, #2077, #15208, #28407, #16253, #36979, #534, #39783, #23621, #30096, #13653, #36766, #32694, #3336, #39363, #110, #19509, #36135, #26844, #16469, #33122, #16894, #3761, #19723, #6997, #10005, #10217, #26213, #20150, #23185, #17110, #30310, #36346, #3125, #29667, #6777, #9800, #22979, #39995, #10428, #7203, #6567, #40207, #26421, #32903, #42596, #13233, #39572, #20356, #19934, #3549, #33545, #16684, #29880, #3970, #744, #13866, #27062, #10637, #23827, #29453, #33339, #13021, #319, #13439, #26634, #23402, #36552, #17629, #24571, #40503, #37719, #8380, #7515, #8161, #11161, #21095, #4919, #20879, #27583, #23928, #28015, #40721, #24360, #1262, #20664, #4276, #21309, #10736, #31470, #34498, #34283, #18067, #31264, #37072, #17418, #1689, #10948, #33852, #41144, #11582, #30615, #37502, #24145, #14818, #1043, #7945, #14168, #27367, #37284, #4698, #24790, #7731, #34066, #4487, #14386, #31044, #11373, #27799, #37935, #30824, #21530, #17847, #34712, #40931, #5134, #1475, #14610, #18280, #13958, #27152, #40294, #38564, #9427, #34922, #2335, #9006, #22175, #2121, #15251, #2544, #35347, #19138, #25005, #5344, #32323, #28452, #21743, #29078, #15876, #38147, #41792, #41586, #28662, #11803, #6197, #15670, #18929, #25835, #8590, #19342, #41366, #12018, #25214, #31905, #32112, #42005, #28871, #25629, #18499, #38787, #12227, #38990, #31688, #38358, #25419, #35560, #1903, #12433, #42215, #8796, #5987, #22592, #21954, #15463, #5775, #9211, #35135, #5560, #15033, #18712, #22382, #2749, #28231, #12643, #35769, #7043, #16297, #365, #155, #3170, #9843, #40041, #29711, #29923, #36809, #32532, #42635, #36174 ),
 .UNSPECIFIED., .F., .F. ) 
 B_SPLINE_CURVE_WITH_KNOTS ( ( 3, 2, 2, 2, 2, 2, 2, 2, 2, 2, 2, 2, 2, 2, 2, 2, 2, 2, 2, 2, 2, 2, 2, 2, 2, 2, 2, 2, 2, 2, 2, 2, 2, 2, 2, 2, 2, 2, 2, 2, 2, 2, 2, 2, 2, 2, 2, 2, 2, 2, 2, 2, 2, 2, 2, 2, 2, 2, 2, 2, 2, 2, 2, 2, 2, 2, 2, 2, 2, 2, 2, 2, 2, 2, 2, 2, 2, 2, 2, 2, 2, 2, 2, 2, 2, 2, 2, 2, 2, 2, 2, 2, 2, 2, 2, 2, 2, 2, 2, 2, 2, 2, 2, 2, 2, 2, 2, 2, 2, 2, 2, 2, 2, 2, 2, 2, 2, 2, 2, 2, 2, 2, 2, 2, 2, 2, 2, 2, 2, 2, 2, 2, 2, 2, 2, 2, 2, 2, 2, 2, 2, 2, 2, 2, 2, 2, 2, 2, 2, 2, 2, 2, 2, 2, 2, 2, 2, 2, 2, 2, 2, 2, 2, 2, 2, 2, 2, 2, 2, 2, 2, 2, 2, 2, 2, 2, 2, 2, 2, 2, 2, 2, 2, 2, 2, 2, 2, 2, 2, 2, 2, 2, 2, 2, 2, 2, 2, 2, 2, 2, 2, 2, 2, 2, 2, 2, 2, 2, 2, 2, 2, 2, 2, 2, 2, 2, 2, 2, 2, 2, 2, 2, 2, 2, 2, 2, 2, 2, 2, 2, 2, 2, 2, 2, 2, 2, 2, 2, 2, 2, 2, 2, 2, 2, 2, 2, 2, 2, 2, 2, 2, 2, 2, 2, 2, 2, 2, 2, 2, 2, 2, 2, 2, 2, 2, 2, 2, 2, 2, 2, 2, 2, 2, 2, 2, 2, 2, 2, 2, 2, 2, 2, 2, 2, 2, 2, 2, 2, 2, 2, 2, 2, 2, 2, 2, 2, 2, 2, 2, 2, 2, 2, 2, 2, 2, 2, 2, 2, 2, 2, 2, 2, 2, 2, 2, 2, 2, 2, 2, 2, 2, 2, 2, 2, 2, 2, 2, 2, 2, 2, 2, 2, 2, 2, 2, 2, 2, 2, 2, 2, 2, 2, 2, 2, 2, 2, 2, 2, 2, 2, 2, 2, 2, 2, 2, 2, 2, 2, 2, 2, 2, 2, 2, 2, 2, 2, 2, 2, 2, 2, 2, 2, 2, 2, 2, 2, 2, 2, 2, 2, 2, 2, 2, 2, 2, 2, 2, 2, 2, 2, 2, 2, 2, 2, 2, 2, 2, 2, 2, 2, 2, 2, 2, 2, 2, 2, 2, 2, 2, 2, 2, 2, 2, 2, 2, 2, 2, 2, 2, 2, 2, 2, 2, 2, 2, 2, 2, 2, 2, 2, 2, 2, 2, 2, 2, 2, 2, 2, 2, 2, 2, 2, 2, 2, 2, 2, 2, 2, 2, 2, 2, 2, 2, 2, 2, 2, 2, 2, 2, 2, 2, 2, 2, 2, 2, 2, 2, 2, 2, 2, 2, 2, 2, 2, 2, 2, 2, 2, 2, 2, 2, 2, 2, 2, 2, 2, 2, 2, 2, 2, 2, 2, 2, 2, 2, 2, 2, 2, 2, 2, 2, 2, 2, 2, 2, 2, 2, 2, 2, 2, 2, 2, 2, 2, 2, 2, 2, 2, 2, 2, 2, 2, 2, 2, 2, 2, 2, 2, 2, 2, 2, 2, 2, 2, 2, 2, 2, 2, 2, 2, 2, 2, 2, 2, 2, 2, 2, 2, 2, 2, 2, 2, 2, 2, 2, 2, 2, 2, 2, 2, 2, 2, 2, 2, 2, 2, 2, 2, 2, 2, 2, 2, 2, 2, 2, 2, 2, 2, 2, 2, 2, 2, 2, 2, 2, 2, 2, 2, 2, 2, 2, 2, 2, 2, 2, 2, 2, 2, 2, 2, 2, 2, 2, 2, 2, 2, 2, 2, 2, 2, 2, 2, 2, 2, 2, 2, 2, 2, 2, 2, 2, 2, 2, 2, 2, 2, 2, 2, 2, 2, 2, 2, 2, 2, 2, 2, 2, 2, 2, 2, 2, 2, 2, 2, 2, 2, 2, 2, 2, 2, 2, 2, 2, 2, 2, 2, 2, 2, 2, 2, 2, 2, 2, 2, 2, 2, 2, 2, 2, 2, 2, 2, 2, 2, 2, 2, 2, 2, 2, 2, 2, 2, 2, 2, 2, 2, 2, 2, 2, 2, 2, 2, 2, 2, 2, 2, 2, 2, 2, 2, 2, 2, 2, 2, 2, 2, 2, 2, 2, 2, 2, 2, 2, 2, 2, 2, 2, 2, 2, 2, 2, 2, 2, 2, 2, 2, 2, 2, 2, 2, 2, 2, 2, 2, 2, 2, 2, 2, 2, 2, 2, 2, 2, 2, 2, 2, 2, 2, 2, 2, 2, 2, 2, 2, 2, 2, 2, 2, 2, 2, 2, 2, 2, 2, 2, 2, 2, 2, 2, 2, 2, 2, 2, 2, 2, 2, 2, 2, 2, 2, 2, 2, 2, 2, 2, 2, 2, 2, 2, 2, 2, 2, 2, 2, 2, 2, 2, 2, 3 ),
 ( 0.000000000000000000, 0.001243781094527363160, 0.002487562189054726321, 0.003731343283582089481, 0.004975124378109452641, 0.006218905472636816235, 0.007462686567164178962, 0.008706467661691542556, 0.009950248756218905283, 0.01119402985074626801, 0.01243781094527363247, 0.01368159203980099520, 0.01492537313432835792, 0.01616915422885572065, 0.01741293532338308511, 0.01865671641791044610, 0.01990049751243781057, 0.02114427860696517503, 0.02238805970149253602, 0.02363184079601990048, 0.02487562189054726494, 0.02611940298507462593, 0.02736318407960199039, 0.02860696517412935486, 0.02985074626865671585, 0.03109452736318408031, 0.03233830845771144130, 0.03358208955223880576, 0.03482587064676617022, 0.03606965174129353469, 0.03731343283582089221, 0.03855721393034825667, 0.03980099502487562113, 0.04104477611940298559, 0.04228855721393035005, 0.04353233830845771452, 0.04477611940298507204, 0.04601990049751243650, 0.04726368159203980096, 0.04850746268656716542, 0.04975124378109452988, 0.05099502487562188741, 0.05223880597014925187, 0.05348258706467661633, 0.05472636815920398079, 0.05597014925373134525, 0.05721393034825870971, 0.05845771144278606724, 0.05970149253731343170, 0.06094527363184079616, 0.06218905472636816062, 0.06343283582089552508, 0.06467661691542288260, 0.06592039800995025400, 0.06716417910447761153, 0.06840796019900496905, 0.06965174129353234045, 0.07089552238805969797, 0.07213930348258706937, 0.07338308457711442689, 0.07462686567164178442, 0.07587064676616915582, 0.07711442786069651334, 0.07835820895522388474, 0.07960199004975124226, 0.08084577114427861366, 0.08208955223880597118, 0.08333333333333332871, 0.08457711442786070011, 0.08582089552238805763, 0.08706467661691542903, 0.08830845771144278655, 0.08955223880597014408, 0.09079601990049751548, 0.09203980099502487300, 0.09328358208955224440, 0.09452736318407960192, 0.09577114427860695944, 0.09701492537313433084, 0.09825870646766168837, 0.09950248756218905977, 0.1007462686567164173, 0.1019900497512437748, 0.1032338308457711462, 0.1044776119402985037, 0.1057213930348258751, 0.1069651741293532327, 0.1082089552238805902, 0.1094527363184079616, 0.1106965174129353191, 0.1119402985074626905, 0.1131840796019900480, 0.1144278606965174194, 0.1156716417910447769, 0.1169154228855721345, 0.1181592039800995059, 0.1194029850746268634, 0.1206467661691542348, 0.1218905472636815923, 0.1231343283582089498, 0.1243781094527363212, 0.1256218905472636926, 0.1268656716417910502, 0.1281094527363184077, 0.1293532338308457652, 0.1305970149253731227, 0.1318407960199005080, 0.1330845771144278655, 0.1343283582089552231, 0.1355721393034825806, 0.1368159203980099381, 0.1380597014925373234, 0.1393034825870646809, 0.1405472636815920384, 0.1417910447761193959, 0.1430348258706467535, 0.1442786069651741387, 0.1455223880597014963, 0.1467661691542288538, 0.1480099502487562113, 0.1492537313432835688, 0.1504975124378109541, 0.1517412935323383116, 0.1529850746268656692, 0.1542288557213930267, 0.1554726368159203842, 0.1567164179104477695, 0.1579601990049751270, 0.1592039800995024845, 0.1604477611940298420, 0.1616915422885572273, 0.1629353233830845848, 0.1641791044776119424, 0.1654228855721392999, 0.1666666666666666574, 0.1679104477611940427, 0.1691542288557214002, 0.1703980099502487577, 0.1716417910447761153, 0.1728855721393034728, 0.1741293532338308581, 0.1753731343283582156, 0.1766169154228855731, 0.1778606965174129306, 0.1791044776119402882, 0.1803482587064676734, 0.1815920398009950310, 0.1828358208955223885, 0.1840796019900497460, 0.1853233830845771035, 0.1865671641791044888, 0.1878109452736318463, 0.1890547263681592038, 0.1902985074626865614, 0.1915422885572139189, 0.1927860696517413042, 0.1940298507462686617, 0.1952736318407960192, 0.1965174129353233767, 0.1977611940298507343, 0.1990049751243781195, 0.2002487562189054771, 0.2014925373134328346, 0.2027363184079601921, 0.2039800995024875496, 0.2052238805970149349, 0.2064676616915422924, 0.2077114427860696499, 0.2089552238805970075, 0.2101990049751243650, 0.2114427860696517503, 0.2126865671641791078, 0.2139303482587064653, 0.2151741293532338228, 0.2164179104477611804, 0.2176616915422885656, 0.2189054726368159232, 0.2201492537313432807, 0.2213930348258706382, 0.2226368159203980235, 0.2238805970149253810, 0.2251243781094527385, 0.2263681592039800961, 0.2276119402985074536, 0.2288557213930348389, 0.2300995024875621964, 0.2313432835820895539, 0.2325870646766169114, 0.2338308457711442689, 0.2350746268656716542, 0.2363184079601990117, 0.2375621890547263693, 0.2388059701492537268, 0.2400497512437810843, 0.2412935323383084696, 0.2425373134328358271, 0.2437810945273631846, 0.2450248756218905422, 0.2462686567164178997, 0.2475124378109452850, 0.2487562189054726425, 0.2500000000000000000, 0.2512437810945273853, 0.2524875621890547150, 0.2537313432835821003, 0.2549751243781094301, 0.2562189054726368154, 0.2574626865671642006, 0.2587064676616915304, 0.2599502487562189157, 0.2611940298507462455, 0.2624378109452736307, 0.2636815920398010160, 0.2649253731343283458, 0.2661691542288557311, 0.2674129353233830608, 0.2686567164179104461, 0.2699004975124378314, 0.2711442786069651611, 0.2723880597014925464, 0.2736318407960198762, 0.2748756218905472615, 0.2761194029850746468, 0.2773631840796019765, 0.2786069651741293618, 0.2798507462686566916, 0.2810945273631840768, 0.2823383084577114621, 0.2835820895522387919, 0.2848258706467661772, 0.2860696517412935069, 0.2873134328358208922, 0.2885572139303482775, 0.2898009950248756073, 0.2910447761194029925, 0.2922885572139303223, 0.2935323383084577076, 0.2947761194029850929, 0.2960199004975124226, 0.2972636815920398079, 0.2985074626865671377, 0.2997512437810945229, 0.3009950248756219082, 0.3022388059701492380, 0.3034825870646766233, 0.3047263681592039530, 0.3059701492537313383, 0.3072139303482587236, 0.3084577114427860534, 0.3097014925373134386, 0.3109452736318407684, 0.3121890547263681537, 0.3134328358208955390, 0.3146766169154228687, 0.3159203980099502540, 0.3171641791044776393, 0.3184079601990049690, 0.3196517412935323543, 0.3208955223880596841, 0.3221393034825870694, 0.3233830845771144546, 0.3246268656716417844, 0.3258706467661691697, 0.3271144278606964995, 0.3283582089552238847, 0.3296019900497512700, 0.3308457711442785998, 0.3320895522388059851, 0.3333333333333333148, 0.3345771144278607001, 0.3358208955223880854, 0.3370646766169154152, 0.3383084577114428004, 0.3395522388059701302, 0.3407960199004975155, 0.3420398009950249008, 0.3432835820895522305, 0.3445273631840796158, 0.3457711442786069456, 0.3470149253731343308, 0.3482587064676617161, 0.3495024875621890459, 0.3507462686567164312, 0.3519900497512437609, 0.3532338308457711462, 0.3544776119402985315, 0.3557213930348258613, 0.3569651741293532465, 0.3582089552238805763, 0.3594527363184079616, 0.3606965174129353469, 0.3619402985074626766, 0.3631840796019900619, 0.3644278606965173917, 0.3656716417910447769, 0.3669154228855721622, 0.3681592039800994920, 0.3694029850746268773, 0.3706467661691542070, 0.3718905472636815923, 0.3731343283582089776, 0.3743781094527363074, 0.3756218905472636926, 0.3768656716417910224, 0.3781094527363184077, 0.3793532338308457930, 0.3805970149253731227, 0.3818407960199005080, 0.3830845771144278378, 0.3843283582089552231, 0.3855721393034826083, 0.3868159203980099381, 0.3880597014925373234, 0.3893034825870646531, 0.3905472636815920384, 0.3917910447761194237, 0.3930348258706467535, 0.3942786069651741387, 0.3955223880597014685, 0.3967661691542288538, 0.3980099502487562391, 0.3992537313432835688, 0.4004975124378109541, 0.4017412935323382839, 0.4029850746268656692, 0.4042288557213930544, 0.4054726368159203842, 0.4067164179104477695, 0.4079601990049750992, 0.4092039800995024845, 0.4104477611940298698, 0.4116915422885571996, 0.4129353233830845848, 0.4141791044776119146, 0.4154228855721392999, 0.4166666666666666297, 0.4179104477611940149, 0.4191542288557214002, 0.4203980099502487300, 0.4216417910447761153, 0.4228855721393035005, 0.4241293532338308303, 0.4253731343283582156, 0.4266169154228855454, 0.4278606965174129306, 0.4291044776119403159, 0.4303482587064676457, 0.4315920398009950310, 0.4328358208955223607, 0.4340796019900497460, 0.4353233830845771313, 0.4365671641791044610, 0.4378109452736318463, 0.4390547263681592316, 0.4402985074626865614, 0.4415422885572139466, 0.4427860696517412764, 0.4440298507462686617, 0.4452736318407960470, 0.4465174129353233767, 0.4477611940298507620, 0.4490049751243780918, 0.4502487562189054771, 0.4514925373134328623, 0.4527363184079601921, 0.4539800995024875774, 0.4552238805970149071, 0.4564676616915422924, 0.4577114427860696777, 0.4589552238805970075, 0.4601990049751243927, 0.4614427860696517225, 0.4626865671641791078, 0.4639303482587064931, 0.4651741293532338228, 0.4664179104477612081, 0.4676616915422885379, 0.4689054726368159232, 0.4701492537313433084, 0.4713930348258706382, 0.4726368159203980235, 0.4738805970149253532, 0.4751243781094527385, 0.4763681592039801238, 0.4776119402985074536, 0.4788557213930348389, 0.4800995024875621686, 0.4813432835820895539, 0.4825870646766169392, 0.4838308457711442689, 0.4850746268656716542, 0.4863184079601989840, 0.4875621890547263693, 0.4888059701492537545, 0.4900497512437810843, 0.4912935323383084696, 0.4925373134328357994, 0.4937810945273631846, 0.4950248756218905699, 0.4962686567164178997, 0.4975124378109452850, 0.4987562189054726147, 0.5000000000000000000, 0.5012437810945273853, 0.5024875621890547706, 0.5037313432835820448, 0.5049751243781094301, 0.5062189054726368154, 0.5074626865671642006, 0.5087064676616915859, 0.5099502487562188602, 0.5111940298507462455, 0.5124378109452736307, 0.5136815920398010160, 0.5149253731343284013, 0.5161691542288556755, 0.5174129353233830608, 0.5186567164179104461, 0.5199004975124378314, 0.5211442786069652167, 0.5223880597014924909, 0.5236318407960198762, 0.5248756218905472615, 0.5261194029850746468, 0.5273631840796020320, 0.5286069651741293063, 0.5298507462686566916, 0.5310945273631840768, 0.5323383084577114621, 0.5335820895522388474, 0.5348258706467661217, 0.5360696517412935069, 0.5373134328358208922, 0.5385572139303482775, 0.5398009950248756628, 0.5410447761194029370, 0.5422885572139303223, 0.5435323383084577076, 0.5447761194029850929, 0.5460199004975124781, 0.5472636815920397524, 0.5485074626865671377, 0.5497512437810945229, 0.5509950248756219082, 0.5522388059701492935, 0.5534825870646765678, 0.5547263681592039530, 0.5559701492537313383, 0.5572139303482587236, 0.5584577114427861089, 0.5597014925373133831, 0.5609452736318407684, 0.5621890547263681537, 0.5634328358208955390, 0.5646766169154229242, 0.5659203980099501985, 0.5671641791044775838, 0.5684079601990049690, 0.5696517412935323543, 0.5708955223880597396, 0.5721393034825870139, 0.5733830845771143991, 0.5746268656716417844, 0.5758706467661691697, 0.5771144278606965550, 0.5783582089552238292, 0.5796019900497512145, 0.5808457711442785998, 0.5820895522388059851, 0.5833333333333333703, 0.5845771144278606446, 0.5858208955223880299, 0.5870646766169154152, 0.5883084577114428004, 0.5895522388059701857, 0.5907960199004974600, 0.5920398009950248452, 0.5932835820895522305, 0.5945273631840796158, 0.5957711442786070011, 0.5970149253731342753, 0.5982587064676616606, 0.5995024875621890459, 0.6007462686567164312, 0.6019900497512438164, 0.6032338308457710907, 0.6044776119402984760, 0.6057213930348258613, 0.6069651741293532465, 0.6082089552238806318, 0.6094527363184079061, 0.6106965174129352913, 0.6119402985074626766, 0.6131840796019900619, 0.6144278606965174472, 0.6156716417910447214, 0.6169154228855721067, 0.6181592039800994920, 0.6194029850746268773, 0.6206467661691542625, 0.6218905472636815368, 0.6231343283582089221, 0.6243781094527363074, 0.6256218905472636926, 0.6268656716417910779, 0.6281094527363184632, 0.6293532338308457375, 0.6305970149253731227, 0.6318407960199005080, 0.6330845771144278933, 0.6343283582089552786, 0.6355721393034825528, 0.6368159203980099381, 0.6380597014925373234, 0.6393034825870647087, 0.6405472636815920939, 0.6417910447761193682, 0.6430348258706467535, 0.6442786069651741387, 0.6455223880597015240, 0.6467661691542289093, 0.6480099502487561836, 0.6492537313432835688, 0.6504975124378109541, 0.6517412935323383394, 0.6529850746268657247, 0.6542288557213929989, 0.6554726368159203842, 0.6567164179104477695, 0.6579601990049751548, 0.6592039800995025400, 0.6604477611940298143, 0.6616915422885571996, 0.6629353233830845848, 0.6641791044776119701, 0.6654228855721393554, 0.6666666666666666297, 0.6679104477611940149, 0.6691542288557214002, 0.6703980099502487855, 0.6716417910447761708, 0.6728855721393034450, 0.6741293532338308303, 0.6753731343283582156, 0.6766169154228856009, 0.6778606965174129861, 0.6791044776119402604, 0.6803482587064676457, 0.6815920398009950310, 0.6828358208955224162, 0.6840796019900498015, 0.6853233830845770758, 0.6865671641791044610, 0.6878109452736318463, 0.6890547263681592316, 0.6902985074626866169, 0.6915422885572138911, 0.6927860696517412764, 0.6940298507462686617, 0.6952736318407960470, 0.6965174129353234322, 0.6977611940298507065, 0.6990049751243780918, 0.7002487562189054771, 0.7014925373134328623, 0.7027363184079602476, 0.7039800995024875219, 0.7052238805970149071, 0.7064676616915422924, 0.7077114427860696777, 0.7089552238805970630, 0.7101990049751243372, 0.7114427860696517225, 0.7126865671641791078, 0.7139303482587064931, 0.7151741293532338783, 0.7164179104477611526, 0.7176616915422885379, 0.7189054726368159232, 0.7201492537313433084, 0.7213930348258706937, 0.7226368159203979680, 0.7238805970149253532, 0.7251243781094527385, 0.7263681592039801238, 0.7276119402985075091, 0.7288557213930347833, 0.7300995024875621686, 0.7313432835820895539, 0.7325870646766169392, 0.7338308457711443245, 0.7350746268656715987, 0.7363184079601989840, 0.7375621890547263693, 0.7388059701492537545, 0.7400497512437811398, 0.7412935323383084141, 0.7425373134328357994, 0.7437810945273631846, 0.7450248756218905699, 0.7462686567164179552, 0.7475124378109452294, 0.7487562189054726147, 0.7500000000000000000, 0.7512437810945273853, 0.7524875621890547706, 0.7537313432835820448, 0.7549751243781094301, 0.7562189054726368154, 0.7574626865671642006, 0.7587064676616915859, 0.7599502487562188602, 0.7611940298507462455, 0.7624378109452736307, 0.7636815920398010160, 0.7649253731343284013, 0.7661691542288556755, 0.7674129353233830608, 0.7686567164179104461, 0.7699004975124378314, 0.7711442786069652167, 0.7723880597014924909, 0.7736318407960198762, 0.7748756218905472615, 0.7761194029850746468, 0.7773631840796020320, 0.7786069651741293063, 0.7798507462686566916, 0.7810945273631840768, 0.7823383084577114621, 0.7835820895522388474, 0.7848258706467661217, 0.7860696517412935069, 0.7873134328358208922, 0.7885572139303482775, 0.7898009950248756628, 0.7910447761194029370, 0.7922885572139303223, 0.7935323383084577076, 0.7947761194029850929, 0.7960199004975124781, 0.7972636815920397524, 0.7985074626865671377, 0.7997512437810945229, 0.8009950248756219082, 0.8022388059701492935, 0.8034825870646765678, 0.8047263681592039530, 0.8059701492537313383, 0.8072139303482587236, 0.8084577114427861089, 0.8097014925373133831, 0.8109452736318407684, 0.8121890547263681537, 0.8134328358208955390, 0.8146766169154229242, 0.8159203980099501985, 0.8171641791044775838, 0.8184079601990049690, 0.8196517412935323543, 0.8208955223880597396, 0.8221393034825870139, 0.8233830845771143991, 0.8246268656716417844, 0.8258706467661691697, 0.8271144278606965550, 0.8283582089552238292, 0.8296019900497512145, 0.8308457711442785998, 0.8320895522388059851, 0.8333333333333332593, 0.8345771144278606446, 0.8358208955223880299, 0.8370646766169154152, 0.8383084577114428004, 0.8395522388059701857, 0.8407960199004974600, 0.8420398009950248452, 0.8432835820895522305, 0.8445273631840796158, 0.8457711442786070011, 0.8470149253731342753, 0.8482587064676616606, 0.8495024875621890459, 0.8507462686567164312, 0.8519900497512438164, 0.8532338308457710907, 0.8544776119402984760, 0.8557213930348258613, 0.8569651741293532465, 0.8582089552238806318, 0.8594527363184079061, 0.8606965174129352913, 0.8619402985074626766, 0.8631840796019900619, 0.8644278606965174472, 0.8656716417910447214, 0.8669154228855721067, 0.8681592039800994920, 0.8694029850746268773, 0.8706467661691542625, 0.8718905472636815368, 0.8731343283582089221, 0.8743781094527363074, 0.8756218905472636926, 0.8768656716417910779, 0.8781094527363184632, 0.8793532338308457375, 0.8805970149253731227, 0.8818407960199005080, 0.8830845771144278933, 0.8843283582089552786, 0.8855721393034825528, 0.8868159203980099381, 0.8880597014925373234, 0.8893034825870647087, 0.8905472636815920939, 0.8917910447761193682, 0.8930348258706467535, 0.8942786069651741387, 0.8955223880597015240, 0.8967661691542289093, 0.8980099502487561836, 0.8992537313432835688, 0.9004975124378109541, 0.9017412935323383394, 0.9029850746268657247, 0.9042288557213929989, 0.9054726368159203842, 0.9067164179104477695, 0.9079601990049751548, 0.9092039800995025400, 0.9104477611940298143, 0.9116915422885571996, 0.9129353233830845848, 0.9141791044776120811, 0.9154228855721393554, 0.9166666666666666297, 0.9179104477611940149, 0.9191542288557214002, 0.9203980099502487855, 0.9216417910447761708, 0.9228855721393034450, 0.9241293532338308303, 0.9253731343283582156, 0.9266169154228856009, 0.9278606965174129861, 0.9291044776119402604, 0.9303482587064676457, 0.9315920398009950310, 0.9328358208955224162, 0.9340796019900498015, 0.9353233830845770758, 0.9365671641791044610, 0.9378109452736318463, 0.9390547263681592316, 0.9402985074626866169, 0.9415422885572138911, 0.9427860696517412764, 0.9440298507462686617, 0.9452736318407960470, 0.9465174129353234322, 0.9477611940298507065, 0.9490049751243780918, 0.9502487562189054771, 0.9514925373134328623, 0.9527363184079602476, 0.9539800995024875219, 0.9552238805970149071, 0.9564676616915422924, 0.9577114427860696777, 0.9589552238805970630, 0.9601990049751243372, 0.9614427860696517225, 0.9626865671641791078, 0.9639303482587064931, 0.9651741293532338783, 0.9664179104477611526, 0.9676616915422885379, 0.9689054726368159232, 0.9701492537313433084, 0.9713930348258706937, 0.9726368159203979680, 0.9738805970149253532, 0.9751243781094527385, 0.9763681592039801238, 0.9776119402985075091, 0.9788557213930347833, 0.9800995024875621686, 0.9813432835820895539, 0.9825870646766169392, 0.9838308457711443245, 0.9850746268656715987, 0.9863184079601989840, 0.9875621890547263693, 0.9888059701492537545, 0.9900497512437811398, 0.9912935323383084141, 0.9917697938471236041 ),
 .UNSPECIFIED. ) 
 CURVE ( )  GEOMETRIC_REPRESENTATION_ITEM ( )  RATIONAL_B_SPLINE_CURVE ( ( 1.000000000000000000, 0.8660254037844387076, 1.000000000000000000, 0.8660254037844387076, 1.000000000000000000, 0.8660254037844387076, 1.000000000000000000, 0.8660254037844387076, 1.000000000000000000, 0.8660254037844387076, 1.000000000000000000, 0.8660254037844387076, 1.000000000000000000, 0.8660254037844387076, 1.000000000000000000, 0.8660254037844387076, 1.000000000000000000, 0.8660254037844387076, 1.000000000000000000, 0.8660254037844387076, 1.000000000000000000, 0.8660254037844387076, 1.000000000000000000, 0.8660254037844387076, 1.000000000000000000, 0.8660254037844387076, 1.000000000000000000, 0.8660254037844387076, 1.000000000000000000, 0.8660254037844387076, 1.000000000000000000, 0.8660254037844387076, 1.000000000000000000, 0.8660254037844387076, 1.000000000000000000, 0.8660254037844387076, 1.000000000000000000, 0.8660254037844387076, 1.000000000000000000, 0.8660254037844387076, 1.000000000000000000, 0.8660254037844387076, 1.000000000000000000, 0.8660254037844387076, 1.000000000000000000, 0.8660254037844387076, 1.000000000000000000, 0.8660254037844387076, 1.000000000000000000, 0.8660254037844387076, 1.000000000000000000, 0.8660254037844387076, 1.000000000000000000, 0.8660254037844387076, 1.000000000000000000, 0.8660254037844387076, 1.000000000000000000, 0.8660254037844387076, 1.000000000000000000, 0.8660254037844387076, 1.000000000000000000, 0.8660254037844387076, 1.000000000000000000, 0.8660254037844387076, 1.000000000000000000, 0.8660254037844387076, 1.000000000000000000, 0.8660254037844387076, 1.000000000000000000, 0.8660254037844387076, 1.000000000000000000, 0.8660254037844387076, 1.000000000000000000, 0.8660254037844387076, 1.000000000000000000, 0.8660254037844387076, 1.000000000000000000, 0.8660254037844387076, 1.000000000000000000, 0.8660254037844387076, 1.000000000000000000, 0.8660254037844387076, 1.000000000000000000, 0.8660254037844387076, 1.000000000000000000, 0.8660254037844387076, 1.000000000000000000, 0.8660254037844387076, 1.000000000000000000, 0.8660254037844387076, 1.000000000000000000, 0.8660254037844387076, 1.000000000000000000, 0.8660254037844387076, 1.000000000000000000, 0.8660254037844387076, 1.000000000000000000, 0.8660254037844387076, 1.000000000000000000, 0.8660254037844387076, 1.000000000000000000, 0.8660254037844387076, 1.000000000000000000, 0.8660254037844387076, 1.000000000000000000, 0.8660254037844387076, 1.000000000000000000, 0.8660254037844387076, 1.000000000000000000, 0.8660254037844387076, 1.000000000000000000, 0.8660254037844387076, 1.000000000000000000, 0.8660254037844387076, 1.000000000000000000, 0.8660254037844387076, 1.000000000000000000, 0.8660254037844387076, 1.000000000000000000, 0.8660254037844387076, 1.000000000000000000, 0.8660254037844387076, 1.000000000000000000, 0.8660254037844387076, 1.000000000000000000, 0.8660254037844387076, 1.000000000000000000, 0.8660254037844387076, 1.000000000000000000, 0.8660254037844387076, 1.000000000000000000, 0.8660254037844387076, 1.000000000000000000, 0.8660254037844387076, 1.000000000000000000, 0.8660254037844387076, 1.000000000000000000, 0.8660254037844387076, 1.000000000000000000, 0.8660254037844387076, 1.000000000000000000, 0.8660254037844387076, 1.000000000000000000, 0.8660254037844387076, 1.000000000000000000, 0.8660254037844387076, 1.000000000000000000, 0.8660254037844387076, 1.000000000000000000, 0.8660254037844387076, 1.000000000000000000, 0.8660254037844387076, 1.000000000000000000, 0.8660254037844387076, 1.000000000000000000, 0.8660254037844387076, 1.000000000000000000, 0.8660254037844387076, 1.000000000000000000, 0.8660254037844387076, 1.000000000000000000, 0.8660254037844387076, 1.000000000000000000, 0.8660254037844387076, 1.000000000000000000, 0.8660254037844387076, 1.000000000000000000, 0.8660254037844387076, 1.000000000000000000, 0.8660254037844387076, 1.000000000000000000, 0.8660254037844387076, 1.000000000000000000, 0.8660254037844387076, 1.000000000000000000, 0.8660254037844387076, 1.000000000000000000, 0.8660254037844387076, 1.000000000000000000, 0.8660254037844387076, 1.000000000000000000, 0.8660254037844387076, 1.000000000000000000, 0.8660254037844387076, 1.000000000000000000, 0.8660254037844387076, 1.000000000000000000, 0.8660254037844387076, 1.000000000000000000, 0.8660254037844387076, 1.000000000000000000, 0.8660254037844387076, 1.000000000000000000, 0.8660254037844387076, 1.000000000000000000, 0.8660254037844387076, 1.000000000000000000, 0.8660254037844387076, 1.000000000000000000, 0.8660254037844387076, 1.000000000000000000, 0.8660254037844387076, 1.000000000000000000, 0.8660254037844387076, 1.000000000000000000, 0.8660254037844387076, 1.000000000000000000, 0.8660254037844387076, 1.000000000000000000, 0.8660254037844387076, 1.000000000000000000, 0.8660254037844387076, 1.000000000000000000, 0.8660254037844387076, 1.000000000000000000, 0.8660254037844387076, 1.000000000000000000, 0.8660254037844387076, 1.000000000000000000, 0.8660254037844387076, 1.000000000000000000, 0.8660254037844387076, 1.000000000000000000, 0.8660254037844387076, 1.000000000000000000, 0.8660254037844387076, 1.000000000000000000, 0.8660254037844387076, 1.000000000000000000, 0.8660254037844387076, 1.000000000000000000, 0.8660254037844387076, 1.000000000000000000, 0.8660254037844387076, 1.000000000000000000, 0.8660254037844387076, 1.000000000000000000, 0.8660254037844387076, 1.000000000000000000, 0.8660254037844387076, 1.000000000000000000, 0.8660254037844387076, 1.000000000000000000, 0.8660254037844387076, 1.000000000000000000, 0.8660254037844387076, 1.000000000000000000, 0.8660254037844387076, 1.000000000000000000, 0.8660254037844387076, 1.000000000000000000, 0.8660254037844387076, 1.000000000000000000, 0.8660254037844387076, 1.000000000000000000, 0.8660254037844387076, 1.000000000000000000, 0.8660254037844387076, 1.000000000000000000, 0.8660254037844387076, 1.000000000000000000, 0.8660254037844387076, 1.000000000000000000, 0.8660254037844387076, 1.000000000000000000, 0.8660254037844387076, 1.000000000000000000, 0.8660254037844387076, 1.000000000000000000, 0.8660254037844387076, 1.000000000000000000, 0.8660254037844387076, 1.000000000000000000, 0.8660254037844387076, 1.000000000000000000, 0.8660254037844387076, 1.000000000000000000, 0.8660254037844387076, 1.000000000000000000, 0.8660254037844387076, 1.000000000000000000, 0.8660254037844387076, 1.000000000000000000, 0.8660254037844387076, 1.000000000000000000, 0.8660254037844387076, 1.000000000000000000, 0.8660254037844387076, 1.000000000000000000, 0.8660254037844387076, 1.000000000000000000, 0.8660254037844387076, 1.000000000000000000, 0.8660254037844387076, 1.000000000000000000, 0.8660254037844387076, 1.000000000000000000, 0.8660254037844387076, 1.000000000000000000, 0.8660254037844387076, 1.000000000000000000, 0.8660254037844387076, 1.000000000000000000, 0.8660254037844387076, 1.000000000000000000, 0.8660254037844387076, 1.000000000000000000, 0.8660254037844387076, 1.000000000000000000, 0.8660254037844387076, 1.000000000000000000, 0.8660254037844387076, 1.000000000000000000, 0.8660254037844387076, 1.000000000000000000, 0.8660254037844387076, 1.000000000000000000, 0.8660254037844387076, 1.000000000000000000, 0.8660254037844387076, 1.000000000000000000, 0.8660254037844387076, 1.000000000000000000, 0.8660254037844387076, 1.000000000000000000, 0.8660254037844387076, 1.000000000000000000, 0.8660254037844387076, 1.000000000000000000, 0.8660254037844387076, 1.000000000000000000, 0.8660254037844387076, 1.000000000000000000, 0.8660254037844387076, 1.000000000000000000, 0.8660254037844387076, 1.000000000000000000, 0.8660254037844387076, 1.000000000000000000, 0.8660254037844387076, 1.000000000000000000, 0.8660254037844387076, 1.000000000000000000, 0.8660254037844387076, 1.000000000000000000, 0.8660254037844387076, 1.000000000000000000, 0.8660254037844387076, 1.000000000000000000, 0.8660254037844387076, 1.000000000000000000, 0.8660254037844387076, 1.000000000000000000, 0.8660254037844387076, 1.000000000000000000, 0.8660254037844387076, 1.000000000000000000, 0.8660254037844387076, 1.000000000000000000, 0.8660254037844387076, 1.000000000000000000, 0.8660254037844387076, 1.000000000000000000, 0.8660254037844387076, 1.000000000000000000, 0.8660254037844387076, 1.000000000000000000, 0.8660254037844387076, 1.000000000000000000, 0.8660254037844387076, 1.000000000000000000, 0.8660254037844387076, 1.000000000000000000, 0.8660254037844387076, 1.000000000000000000, 0.8660254037844387076, 1.000000000000000000, 0.8660254037844387076, 1.000000000000000000, 0.8660254037844387076, 1.000000000000000000, 0.8660254037844387076, 1.000000000000000000, 0.8660254037844387076, 1.000000000000000000, 0.8660254037844387076, 1.000000000000000000, 0.8660254037844387076, 1.000000000000000000, 0.8660254037844387076, 1.000000000000000000, 0.8660254037844387076, 1.000000000000000000, 0.8660254037844387076, 1.000000000000000000, 0.8660254037844387076, 1.000000000000000000, 0.8660254037844387076, 1.000000000000000000, 0.8660254037844387076, 1.000000000000000000, 0.8660254037844387076, 1.000000000000000000, 0.8660254037844387076, 1.000000000000000000, 0.8660254037844387076, 1.000000000000000000, 0.8660254037844387076, 1.000000000000000000, 0.8660254037844387076, 1.000000000000000000, 0.8660254037844387076, 1.000000000000000000, 0.8660254037844387076, 1.000000000000000000, 0.8660254037844387076, 1.000000000000000000, 0.8660254037844387076, 1.000000000000000000, 0.8660254037844387076, 1.000000000000000000, 0.8660254037844387076, 1.000000000000000000, 0.8660254037844387076, 1.000000000000000000, 0.8660254037844387076, 1.000000000000000000, 0.8660254037844387076, 1.000000000000000000, 0.8660254037844387076, 1.000000000000000000, 0.8660254037844387076, 1.000000000000000000, 0.8660254037844387076, 1.000000000000000000, 0.8660254037844387076, 1.000000000000000000, 0.8660254037844387076, 1.000000000000000000, 0.8660254037844387076, 1.000000000000000000, 0.8660254037844387076, 1.000000000000000000, 0.8660254037844387076, 1.000000000000000000, 0.8660254037844387076, 1.000000000000000000, 0.8660254037844387076, 1.000000000000000000, 0.8660254037844387076, 1.000000000000000000, 0.8660254037844387076, 1.000000000000000000, 0.8660254037844387076, 1.000000000000000000, 0.8660254037844387076, 1.000000000000000000, 0.8660254037844387076, 1.000000000000000000, 0.8660254037844387076, 1.000000000000000000, 0.8660254037844387076, 1.000000000000000000, 0.8660254037844387076, 1.000000000000000000, 0.8660254037844387076, 1.000000000000000000, 0.8660254037844387076, 1.000000000000000000, 0.8660254037844387076, 1.000000000000000000, 0.8660254037844387076, 1.000000000000000000, 0.8660254037844387076, 1.000000000000000000, 0.8660254037844387076, 1.000000000000000000, 0.8660254037844387076, 1.000000000000000000, 0.8660254037844387076, 1.000000000000000000, 0.8660254037844387076, 1.000000000000000000, 0.8660254037844387076, 1.000000000000000000, 0.8660254037844387076, 1.000000000000000000, 0.8660254037844387076, 1.000000000000000000, 0.8660254037844387076, 1.000000000000000000, 0.8660254037844387076, 1.000000000000000000, 0.8660254037844387076, 1.000000000000000000, 0.8660254037844387076, 1.000000000000000000, 0.8660254037844387076, 1.000000000000000000, 0.8660254037844387076, 1.000000000000000000, 0.8660254037844387076, 1.000000000000000000, 0.8660254037844387076, 1.000000000000000000, 0.8660254037844387076, 1.000000000000000000, 0.8660254037844387076, 1.000000000000000000, 0.8660254037844387076, 1.000000000000000000, 0.8660254037844387076, 1.000000000000000000, 0.8660254037844387076, 1.000000000000000000, 0.8660254037844387076, 1.000000000000000000, 0.8660254037844387076, 1.000000000000000000, 0.8660254037844387076, 1.000000000000000000, 0.8660254037844387076, 1.000000000000000000, 0.8660254037844387076, 1.000000000000000000, 0.8660254037844387076, 1.000000000000000000, 0.8660254037844387076, 1.000000000000000000, 0.8660254037844387076, 1.000000000000000000, 0.8660254037844387076, 1.000000000000000000, 0.8660254037844387076, 1.000000000000000000, 0.8660254037844387076, 1.000000000000000000, 0.8660254037844387076, 1.000000000000000000, 0.8660254037844387076, 1.000000000000000000, 0.8660254037844387076, 1.000000000000000000, 0.8660254037844387076, 1.000000000000000000, 0.8660254037844387076, 1.000000000000000000, 0.8660254037844387076, 1.000000000000000000, 0.8660254037844387076, 1.000000000000000000, 0.8660254037844387076, 1.000000000000000000, 0.8660254037844387076, 1.000000000000000000, 0.8660254037844387076, 1.000000000000000000, 0.8660254037844387076, 1.000000000000000000, 0.8660254037844387076, 1.000000000000000000, 0.8660254037844387076, 1.000000000000000000, 0.8660254037844387076, 1.000000000000000000, 0.8660254037844387076, 1.000000000000000000, 0.8660254037844387076, 1.000000000000000000, 0.8660254037844387076, 1.000000000000000000, 0.8660254037844387076, 1.000000000000000000, 0.8660254037844387076, 1.000000000000000000, 0.8660254037844387076, 1.000000000000000000, 0.8660254037844387076, 1.000000000000000000, 0.8660254037844387076, 1.000000000000000000, 0.8660254037844387076, 1.000000000000000000, 0.8660254037844387076, 1.000000000000000000, 0.8660254037844387076, 1.000000000000000000, 0.8660254037844387076, 1.000000000000000000, 0.8660254037844387076, 1.000000000000000000, 0.8660254037844387076, 1.000000000000000000, 0.8660254037844387076, 1.000000000000000000, 0.8660254037844387076, 1.000000000000000000, 0.8660254037844387076, 1.000000000000000000, 0.8660254037844387076, 1.000000000000000000, 0.8660254037844387076, 1.000000000000000000, 0.8660254037844387076, 1.000000000000000000, 0.8660254037844387076, 1.000000000000000000, 0.8660254037844387076, 1.000000000000000000, 0.8660254037844387076, 1.000000000000000000, 0.8660254037844387076, 1.000000000000000000, 0.8660254037844387076, 1.000000000000000000, 0.8660254037844387076, 1.000000000000000000, 0.8660254037844387076, 1.000000000000000000, 0.8660254037844387076, 1.000000000000000000, 0.8660254037844387076, 1.000000000000000000, 0.8660254037844387076, 1.000000000000000000, 0.8660254037844387076, 1.000000000000000000, 0.8660254037844387076, 1.000000000000000000, 0.8660254037844387076, 1.000000000000000000, 0.8660254037844387076, 1.000000000000000000, 0.8660254037844387076, 1.000000000000000000, 0.8660254037844387076, 1.000000000000000000, 0.8660254037844387076, 1.000000000000000000, 0.8660254037844387076, 1.000000000000000000, 0.8660254037844387076, 1.000000000000000000, 0.8660254037844387076, 1.000000000000000000, 0.8660254037844387076, 1.000000000000000000, 0.8660254037844387076, 1.000000000000000000, 0.8660254037844387076, 1.000000000000000000, 0.8660254037844387076, 1.000000000000000000, 0.8660254037844387076, 1.000000000000000000, 0.8660254037844387076, 1.000000000000000000, 0.8660254037844387076, 1.000000000000000000, 0.8660254037844387076, 1.000000000000000000, 0.8660254037844387076, 1.000000000000000000, 0.8660254037844387076, 1.000000000000000000, 0.8660254037844387076, 1.000000000000000000, 0.8660254037844387076, 1.000000000000000000, 0.8660254037844387076, 1.000000000000000000, 0.8660254037844387076, 1.000000000000000000, 0.8660254037844387076, 1.000000000000000000, 0.8660254037844387076, 1.000000000000000000, 0.8660254037844387076, 1.000000000000000000, 0.8660254037844387076, 1.000000000000000000, 0.8660254037844387076, 1.000000000000000000, 0.8660254037844387076, 1.000000000000000000, 0.8660254037844387076, 1.000000000000000000, 0.8660254037844387076, 1.000000000000000000, 0.8660254037844387076, 1.000000000000000000, 0.8660254037844387076, 1.000000000000000000, 0.8660254037844387076, 1.000000000000000000, 0.8660254037844387076, 1.000000000000000000, 0.8660254037844387076, 1.000000000000000000, 0.8660254037844387076, 1.000000000000000000, 0.8660254037844387076, 1.000000000000000000, 0.8660254037844387076, 1.000000000000000000, 0.8660254037844387076, 1.000000000000000000, 0.8660254037844387076, 1.000000000000000000, 0.8660254037844387076, 1.000000000000000000, 0.8660254037844387076, 1.000000000000000000, 0.8660254037844387076, 1.000000000000000000, 0.8660254037844387076, 1.000000000000000000, 0.8660254037844387076, 1.000000000000000000, 0.8660254037844387076, 1.000000000000000000, 0.8660254037844387076, 1.000000000000000000, 0.8660254037844387076, 1.000000000000000000, 0.8660254037844387076, 1.000000000000000000, 0.8660254037844387076, 1.000000000000000000, 0.8660254037844387076, 1.000000000000000000, 0.8660254037844387076, 1.000000000000000000, 0.8660254037844387076, 1.000000000000000000, 0.8660254037844387076, 1.000000000000000000, 0.8660254037844387076, 1.000000000000000000, 0.8660254037844387076, 1.000000000000000000, 0.8660254037844387076, 1.000000000000000000, 0.8660254037844387076, 1.000000000000000000, 0.8660254037844387076, 1.000000000000000000, 0.8660254037844387076, 1.000000000000000000, 0.8660254037844387076, 1.000000000000000000, 0.8660254037844387076, 1.000000000000000000, 0.8660254037844387076, 1.000000000000000000, 0.8660254037844387076, 1.000000000000000000, 0.8660254037844387076, 1.000000000000000000, 0.8660254037844387076, 1.000000000000000000, 0.8660254037844387076, 1.000000000000000000, 0.8660254037844387076, 1.000000000000000000, 0.8660254037844387076, 1.000000000000000000, 0.8660254037844387076, 1.000000000000000000, 0.8660254037844387076, 1.000000000000000000, 0.8660254037844387076, 1.000000000000000000, 0.8660254037844387076, 1.000000000000000000, 0.8660254037844387076, 1.000000000000000000, 0.8660254037844387076, 1.000000000000000000, 0.8660254037844387076, 1.000000000000000000, 0.8660254037844387076, 1.000000000000000000, 0.8660254037844387076, 1.000000000000000000, 0.8660254037844387076, 1.000000000000000000, 0.8660254037844387076, 1.000000000000000000, 0.8660254037844387076, 1.000000000000000000, 0.8660254037844387076, 1.000000000000000000, 0.8660254037844387076, 1.000000000000000000, 0.8660254037844387076, 1.000000000000000000, 0.8660254037844387076, 1.000000000000000000, 0.8660254037844387076, 1.000000000000000000, 0.8660254037844387076, 1.000000000000000000, 0.8660254037844387076, 1.000000000000000000, 0.8660254037844387076, 1.000000000000000000, 0.8660254037844387076, 1.000000000000000000, 0.8660254037844387076, 1.000000000000000000, 0.8660254037844387076, 1.000000000000000000, 0.8660254037844387076, 1.000000000000000000, 0.8660254037844387076, 1.000000000000000000, 0.8660254037844387076, 1.000000000000000000, 0.8660254037844387076, 1.000000000000000000, 0.8660254037844387076, 1.000000000000000000, 0.8660254037844387076, 1.000000000000000000, 0.8660254037844387076, 1.000000000000000000, 0.8660254037844387076, 1.000000000000000000, 0.8660254037844387076, 1.000000000000000000, 0.8660254037844387076, 1.000000000000000000, 0.8660254037844387076, 1.000000000000000000, 0.8660254037844387076, 1.000000000000000000, 0.8660254037844387076, 1.000000000000000000, 0.8660254037844387076, 1.000000000000000000, 0.8660254037844387076, 1.000000000000000000, 0.8660254037844387076, 1.000000000000000000, 0.8660254037844387076, 1.000000000000000000, 0.8660254037844387076, 1.000000000000000000, 0.8660254037844387076, 1.000000000000000000, 0.8660254037844387076, 1.000000000000000000, 0.8660254037844387076, 1.000000000000000000, 0.8660254037844387076, 1.000000000000000000, 0.8660254037844387076, 1.000000000000000000, 0.8660254037844387076, 1.000000000000000000, 0.8660254037844387076, 1.000000000000000000, 0.8660254037844387076, 1.000000000000000000, 0.8660254037844387076, 1.000000000000000000, 0.8660254037844387076, 1.000000000000000000, 0.8660254037844387076, 1.000000000000000000, 0.8660254037844387076, 1.000000000000000000, 0.8660254037844387076, 1.000000000000000000, 0.8660254037844387076, 1.000000000000000000, 0.8660254037844387076, 1.000000000000000000, 0.8660254037844387076, 1.000000000000000000, 0.8660254037844387076, 1.000000000000000000, 0.8660254037844387076, 1.000000000000000000, 0.8660254037844387076, 1.000000000000000000, 0.8660254037844387076, 1.000000000000000000, 0.8660254037844387076, 1.000000000000000000, 0.8660254037844387076, 1.000000000000000000, 0.8660254037844387076, 1.000000000000000000, 0.8660254037844387076, 1.000000000000000000, 0.8660254037844387076, 1.000000000000000000, 0.8660254037844387076, 1.000000000000000000, 0.8660254037844387076, 1.000000000000000000, 0.8660254037844387076, 1.000000000000000000, 0.8660254037844387076, 1.000000000000000000, 0.8660254037844387076, 1.000000000000000000, 0.8660254037844387076, 1.000000000000000000, 0.8660254037844387076, 1.000000000000000000, 0.8660254037844387076, 1.000000000000000000, 0.8660254037844387076, 1.000000000000000000, 0.8660254037844387076, 1.000000000000000000, 0.8660254037844387076, 1.000000000000000000, 0.8660254037844387076, 1.000000000000000000, 0.8660254037844387076, 1.000000000000000000, 0.8660254037844387076, 1.000000000000000000, 0.8660254037844387076, 1.000000000000000000, 0.8660254037844387076, 1.000000000000000000, 0.8660254037844387076, 1.000000000000000000, 0.8660254037844387076, 1.000000000000000000, 0.8660254037844387076, 1.000000000000000000, 0.8660254037844387076, 1.000000000000000000, 0.8660254037844387076, 1.000000000000000000, 0.8660254037844387076, 1.000000000000000000, 0.8660254037844387076, 1.000000000000000000, 0.8660254037844387076, 1.000000000000000000, 0.8660254037844387076, 1.000000000000000000, 0.8660254037844387076, 1.000000000000000000, 0.8660254037844387076, 1.000000000000000000, 0.8660254037844387076, 1.000000000000000000, 0.8660254037844387076, 1.000000000000000000, 0.8660254037844387076, 1.000000000000000000, 0.8660254037844387076, 1.000000000000000000, 0.8660254037844387076, 1.000000000000000000, 0.8660254037844387076, 1.000000000000000000, 0.8660254037844387076, 1.000000000000000000, 0.8660254037844387076, 1.000000000000000000, 0.8660254037844387076, 1.000000000000000000, 0.8660254037844387076, 1.000000000000000000, 0.8660254037844387076, 1.000000000000000000, 0.8660254037844387076, 1.000000000000000000, 0.8660254037844387076, 1.000000000000000000, 0.8660254037844387076, 1.000000000000000000, 0.8660254037844387076, 1.000000000000000000, 0.8660254037844387076, 1.000000000000000000, 0.8660254037844387076, 1.000000000000000000, 0.8660254037844387076, 1.000000000000000000, 0.8660254037844387076, 1.000000000000000000, 0.8660254037844387076, 1.000000000000000000, 0.8660254037844387076, 1.000000000000000000, 0.8660254037844387076, 1.000000000000000000, 0.8660254037844387076, 1.000000000000000000, 0.8660254037844387076, 1.000000000000000000, 0.8660254037844387076, 1.000000000000000000, 0.8660254037844387076, 1.000000000000000000, 0.8660254037844387076, 1.000000000000000000, 0.8660254037844387076, 1.000000000000000000, 0.8660254037844387076, 1.000000000000000000, 0.8660254037844387076, 1.000000000000000000, 0.8660254037844387076, 1.000000000000000000, 0.8660254037844387076, 1.000000000000000000, 0.8660254037844387076, 1.000000000000000000, 0.8660254037844387076, 1.000000000000000000, 0.8660254037844387076, 1.000000000000000000, 0.8660254037844387076, 1.000000000000000000, 0.8660254037844387076, 1.000000000000000000, 0.8660254037844387076, 1.000000000000000000, 0.8660254037844387076, 1.000000000000000000, 0.8660254037844387076, 1.000000000000000000, 0.8660254037844387076, 1.000000000000000000, 0.8660254037844387076, 1.000000000000000000, 0.8660254037844387076, 1.000000000000000000, 0.8660254037844387076, 1.000000000000000000, 0.8660254037844387076, 1.000000000000000000, 0.8660254037844387076, 1.000000000000000000, 0.8660254037844387076, 1.000000000000000000, 0.8660254037844387076, 1.000000000000000000, 0.8660254037844387076, 1.000000000000000000, 0.8660254037844387076, 1.000000000000000000, 0.8660254037844387076, 1.000000000000000000, 0.8660254037844387076, 1.000000000000000000, 0.8660254037844387076, 1.000000000000000000, 0.8660254037844387076, 1.000000000000000000, 0.8660254037844387076, 1.000000000000000000, 0.8660254037844387076, 1.000000000000000000, 0.8660254037844387076, 1.000000000000000000, 0.8660254037844387076, 1.000000000000000000, 0.8660254037844387076, 1.000000000000000000, 0.8660254037844387076, 1.000000000000000000, 0.8660254037844387076, 1.000000000000000000, 0.8660254037844387076, 1.000000000000000000, 0.8660254037844387076, 1.000000000000000000, 0.8660254037844387076, 1.000000000000000000, 0.8660254037844387076, 1.000000000000000000, 0.8660254037844387076, 1.000000000000000000, 0.8660254037844387076, 1.000000000000000000, 0.8660254037844387076, 1.000000000000000000, 0.8660254037844387076, 1.000000000000000000, 0.8660254037844387076, 1.000000000000000000, 0.8660254037844387076, 1.000000000000000000, 0.8660254037844387076, 1.000000000000000000, 0.8660254037844387076, 1.000000000000000000, 0.8660254037844387076, 1.000000000000000000, 0.8660254037844387076, 1.000000000000000000, 0.8660254037844387076, 1.000000000000000000, 0.8660254037844387076, 1.000000000000000000, 0.8660254037844387076, 1.000000000000000000, 0.8660254037844387076, 1.000000000000000000, 0.8660254037844387076, 1.000000000000000000, 0.8660254037844387076, 1.000000000000000000, 0.8660254037844387076, 1.000000000000000000, 0.8660254037844387076, 1.000000000000000000, 0.8660254037844387076, 1.000000000000000000, 0.8660254037844387076, 1.000000000000000000, 0.8660254037844387076, 1.000000000000000000, 0.8660254037844387076, 1.000000000000000000, 0.8660254037844387076, 1.000000000000000000, 0.8660254037844387076, 1.000000000000000000, 0.8660254037844387076, 1.000000000000000000, 0.8660254037844387076, 1.000000000000000000, 0.8660254037844387076, 1.000000000000000000, 0.8660254037844387076, 1.000000000000000000, 0.8660254037844387076, 1.000000000000000000, 0.8660254037844387076, 1.000000000000000000, 0.8660254037844387076, 1.000000000000000000, 0.8660254037844387076, 1.000000000000000000, 0.8660254037844387076, 1.000000000000000000, 0.8660254037844387076, 1.000000000000000000, 0.8660254037844387076, 1.000000000000000000, 0.8660254037844387076, 1.000000000000000000, 0.8660254037844387076, 1.000000000000000000, 0.8660254037844387076, 1.000000000000000000, 0.8660254037844387076, 1.000000000000000000, 0.8660254037844387076, 1.000000000000000000, 0.8660254037844387076, 1.000000000000000000, 0.8660254037844387076, 1.000000000000000000, 0.8660254037844387076, 1.000000000000000000, 0.8660254037844387076, 1.000000000000000000, 0.8660254037844387076, 1.000000000000000000, 0.8660254037844387076, 1.000000000000000000, 0.8660254037844387076, 1.000000000000000000, 0.8660254037844387076, 1.000000000000000000, 0.8660254037844387076, 1.000000000000000000, 0.8660254037844387076, 1.000000000000000000, 0.8660254037844387076, 1.000000000000000000, 0.8660254037844387076, 1.000000000000000000, 0.8660254037844387076, 1.000000000000000000, 0.8660254037844387076, 1.000000000000000000, 0.8660254037844387076, 1.000000000000000000, 0.8660254037844387076, 1.000000000000000000, 0.8660254037844387076, 1.000000000000000000, 0.8660254037844387076, 1.000000000000000000, 0.8660254037844387076, 1.000000000000000000, 0.8660254037844387076, 1.000000000000000000, 0.8660254037844387076, 1.000000000000000000, 0.8660254037844387076, 1.000000000000000000, 0.8660254037844387076, 1.000000000000000000, 0.8660254037844387076, 1.000000000000000000, 0.8660254037844387076, 1.000000000000000000, 0.8660254037844387076, 1.000000000000000000, 0.8660254037844387076, 1.000000000000000000, 0.8660254037844387076, 1.000000000000000000, 0.8660254037844387076, 1.000000000000000000, 0.8660254037844387076, 1.000000000000000000, 0.8660254037844387076, 1.000000000000000000, 0.8660254037844387076, 1.000000000000000000, 0.8660254037844387076, 1.000000000000000000, 0.8660254037844387076, 1.000000000000000000, 0.8660254037844387076, 1.000000000000000000, 0.8660254037844387076, 1.000000000000000000, 0.8660254037844387076, 1.000000000000000000, 0.8660254037844387076, 1.000000000000000000, 0.8660254037844387076, 1.000000000000000000, 0.8660254037844387076, 1.000000000000000000, 0.8660254037844387076, 1.000000000000000000, 0.8660254037844387076, 1.000000000000000000, 0.8660254037844387076, 1.000000000000000000, 0.8660254037844387076, 1.000000000000000000, 0.8660254037844387076, 1.000000000000000000, 0.8660254037844387076, 1.000000000000000000, 0.8660254037844387076, 1.000000000000000000, 0.8660254037844387076, 1.000000000000000000, 0.8660254037844387076, 1.000000000000000000, 0.8660254037844387076, 1.000000000000000000, 0.8660254037844387076, 1.000000000000000000, 0.8660254037844387076, 1.000000000000000000, 0.8660254037844387076, 1.000000000000000000, 0.8660254037844387076, 1.000000000000000000, 0.8660254037844387076, 1.000000000000000000, 0.8660254037844387076, 1.000000000000000000, 0.8660254037844387076, 1.000000000000000000, 0.8660254037844387076, 1.000000000000000000, 0.8660254037844387076, 1.000000000000000000, 0.8660254037844387076, 1.000000000000000000, 0.8660254037844387076, 1.000000000000000000, 0.8660254037844387076, 1.000000000000000000, 0.8660254037844387076, 1.000000000000000000, 0.8660254037844387076, 1.000000000000000000, 0.8660254037844387076, 1.000000000000000000, 0.8660254037844387076, 1.000000000000000000, 0.8660254037844387076, 1.000000000000000000, 0.8660254037844387076, 1.000000000000000000, 0.8660254037844387076, 1.000000000000000000, 0.8660254037844387076, 1.000000000000000000, 0.8660254037844387076, 1.000000000000000000, 0.8660254037844387076, 1.000000000000000000, 0.8660254037844387076, 1.000000000000000000, 0.8660254037844387076, 1.000000000000000000, 0.8660254037844387076, 1.000000000000000000, 0.8660254037844387076, 1.000000000000000000, 0.8660254037844387076, 1.000000000000000000, 0.8660254037844387076, 1.000000000000000000, 0.8660254037844387076, 1.000000000000000000, 0.8660254037844387076, 1.000000000000000000, 0.8660254037844387076, 1.000000000000000000, 0.8660254037844387076, 1.000000000000000000, 0.8660254037844387076, 1.000000000000000000, 0.8660254037844387076, 1.000000000000000000, 0.8660254037844387076, 1.000000000000000000, 0.8660254037844387076, 1.000000000000000000, 0.8660254037844387076, 1.000000000000000000, 0.8660254037844387076, 1.000000000000000000, 0.8660254037844387076, 1.000000000000000000, 0.8660254037844387076, 1.000000000000000000, 0.8660254037844387076, 1.000000000000000000, 0.8660254037844387076, 1.000000000000000000, 0.8660254037844387076, 1.000000000000000000, 0.8660254037844387076, 1.000000000000000000, 0.8660254037844387076, 1.000000000000000000, 0.8660254037844387076, 1.000000000000000000, 0.8660254037844387076, 1.000000000000000000, 0.8660254037844387076, 1.000000000000000000, 0.8660254037844387076, 1.000000000000000000, 0.8660254037844387076, 1.000000000000000000, 0.8660254037844387076, 1.000000000000000000, 0.8660254037844387076, 1.000000000000000000, 0.8660254037844387076, 1.000000000000000000, 0.8660254037844387076, 1.000000000000000000, 0.8660254037844387076, 1.000000000000000000, 0.8660254037844387076, 1.000000000000000000, 0.8660254037844387076, 1.000000000000000000, 0.8660254037844387076, 1.000000000000000000, 0.8660254037844387076, 1.000000000000000000, 0.8660254037844387076, 1.000000000000000000, 0.8660254037844387076, 1.000000000000000000, 0.8660254037844387076, 1.000000000000000000, 0.8660254037844387076, 1.000000000000000000, 0.8660254037844387076, 1.000000000000000000, 0.8660254037844387076, 1.000000000000000000, 0.8660254037844387076, 1.000000000000000000, 0.8660254037844387076, 1.000000000000000000, 0.8660254037844387076, 1.000000000000000000, 0.8660254037844387076, 1.000000000000000000, 0.8660254037844387076, 1.000000000000000000, 0.8660254037844387076, 1.000000000000000000, 0.8660254037844387076, 1.000000000000000000, 0.8660254037844387076, 1.000000000000000000, 0.8660254037844387076, 1.000000000000000000, 0.8660254037844387076, 1.000000000000000000, 0.8660254037844387076, 1.000000000000000000, 0.8660254037844387076, 1.000000000000000000, 0.8660254037844387076, 1.000000000000000000, 0.8660254037844387076, 1.000000000000000000, 0.8660254037844387076, 1.000000000000000000, 0.8660254037844387076, 1.000000000000000000, 0.8660254037844387076, 1.000000000000000000, 0.8660254037844387076, 1.000000000000000000, 0.8660254037844387076, 1.000000000000000000, 0.8660254037844387076, 1.000000000000000000, 0.8660254037844387076, 1.000000000000000000, 0.8660254037844387076, 1.000000000000000000, 0.8660254037844387076, 1.000000000000000000, 0.8660254037844387076, 1.000000000000000000, 0.8660254037844387076, 1.000000000000000000, 0.8660254037844387076, 1.000000000000000000, 0.8660254037844387076, 1.000000000000000000, 0.8660254037844387076, 1.000000000000000000, 0.8660254037844387076, 1.000000000000000000, 0.8660254037844387076, 1.000000000000000000, 0.8660254037844387076, 1.000000000000000000, 0.8660254037844387076, 1.000000000000000000, 0.8660254037844387076, 1.000000000000000000, 0.8660254037844387076, 1.000000000000000000, 0.8660254037844387076, 1.000000000000000000, 0.8660254037844387076, 1.000000000000000000, 0.8660254037844387076, 1.000000000000000000, 0.8660254037844387076, 1.000000000000000000, 0.8660254037844387076, 1.000000000000000000, 0.8660254037844387076, 1.000000000000000000, 0.8660254037844387076, 1.000000000000000000, 0.8660254037844387076, 1.000000000000000000, 0.8660254037844387076, 1.000000000000000000, 0.8660254037844387076, 1.000000000000000000, 0.8660254037844387076, 1.000000000000000000, 0.8660254037844387076, 1.000000000000000000, 0.8660254037844387076, 1.000000000000000000, 0.8660254037844387076, 1.000000000000000000, 0.8660254037844387076, 1.000000000000000000, 0.8660254037844387076, 1.000000000000000000, 0.8660254037844387076, 1.000000000000000000, 0.8660254037844387076, 1.000000000000000000, 0.8660254037844387076, 1.000000000000000000, 0.8660254037844387076, 1.000000000000000000, 0.8660254037844387076, 1.000000000000000000, 0.8660254037844387076, 1.000000000000000000, 0.8660254037844387076, 1.000000000000000000, 0.8660254037844387076, 1.000000000000000000, 0.8660254037844387076, 1.000000000000000000, 0.8660254037844387076, 1.000000000000000000, 0.8660254037844387076, 1.000000000000000000, 0.8660254037844387076, 1.000000000000000000, 0.8660254037844387076, 1.000000000000000000, 0.8660254037844387076, 1.000000000000000000, 0.8660254037844387076, 1.000000000000000000, 0.8660254037844387076, 1.000000000000000000, 0.8660254037844387076, 1.000000000000000000, 0.8660254037844387076, 1.000000000000000000, 0.8660254037844387076, 1.000000000000000000, 0.8660254037844387076, 1.000000000000000000, 0.8660254037844387076, 1.000000000000000000, 0.8660254037844387076, 1.000000000000000000, 0.8660254037844387076, 1.000000000000000000, 0.8660254037844387076, 1.000000000000000000, 0.8660254037844387076, 1.000000000000000000, 0.8660254037844387076, 1.000000000000000000, 0.8660254037844387076, 1.000000000000000000, 0.8660254037844387076, 1.000000000000000000, 0.8660254037844387076, 1.000000000000000000, 0.8660254037844387076, 1.000000000000000000, 0.8660254037844387076, 1.000000000000000000, 0.8660254037844387076, 1.000000000000000000, 0.8660254037844387076, 1.000000000000000000, 0.8660254037844387076, 1.000000000000000000, 0.8660254037844387076, 1.000000000000000000, 0.8660254037844387076, 1.000000000000000000, 0.8660254037844387076, 1.000000000000000000, 0.8660254037844387076, 1.000000000000000000, 0.8660254037844387076, 1.000000000000000000, 0.8660254037844387076, 1.000000000000000000, 0.8660254037844387076, 1.000000000000000000, 0.8660254037844387076, 1.000000000000000000, 0.8660254037844387076, 1.000000000000000000, 0.8660254037844387076, 1.000000000000000000, 0.8660254037844387076, 1.000000000000000000, 0.8660254037844387076, 1.000000000000000000, 0.8660254037844387076, 1.000000000000000000, 0.8660254037844387076, 1.000000000000000000, 0.8660254037844387076, 1.000000000000000000, 0.8660254037844387076, 1.000000000000000000, 0.8660254037844387076, 1.000000000000000000, 0.9486992175574315844, 0.9366860366984544051 ) ) 
 REPRESENTATION_ITEM ( '' )  );
#3613 = COORDINATED_UNIVERSAL_TIME_OFFSET ( 6, 0, .AHEAD. ) ;
#3614 = CARTESIAN_POINT ( 'NONE',  ( 10.81189881249999551, -6.242252689847874514, -73.46875000204835260 ) ) ;
#3615 = CARTESIAN_POINT ( 'NONE',  ( -10.00000000000076916, 5.773502691895813221, -104.8749999999999716 ) ) ;
#3616 = CARTESIAN_POINT ( 'NONE',  ( -10.81189881249999729, 6.242252689847871849, -194.2187500020483810 ) ) ;
#3617 = CARTESIAN_POINT ( 'NONE',  ( -2.293366432827344421E-15, -12.48450537969573659, -151.7187500020483810 ) ) ;
#3618 = DIRECTION ( 'NONE',  ( -0.000000000000000000, -0.000000000000000000, 1.000000000000000000 ) ) ;
#3619 = CARTESIAN_POINT ( 'NONE',  ( -9.999999999999998224, 1.224646799147353059E-15, -189.1250000040967905 ) ) ;
#3620 = CARTESIAN_POINT ( 'NONE',  ( 5.405949406249992428, -9.363379034771808662, -148.7812500020483810 ) ) ;
#3621 = CARTESIAN_POINT ( 'NONE',  ( -9.999999999999998224, 5.773502691896259087, -4.750000004096766482 ) ) ;
#3622 = AXIS2_PLACEMENT_3D ( 'NONE', #34855, #7285, #27729 ) ;
#3623 = DIRECTION ( 'NONE',  ( 1.000000000000000000, 0.000000000000000000, 0.000000000000000000 ) ) ;
#3624 = CARTESIAN_POINT ( 'NONE',  ( -10.81189881249999729, 1.324075727343319199E-15, -119.0937500020483810 ) ) ;
#3625 = LINE ( 'NONE', #13933, #25268 ) ;
#3626 = CARTESIAN_POINT ( 'NONE',  ( -10.81189881249999729, 6.242252689847871849, -92.40625000204838102 ) ) ;
#3627 = CARTESIAN_POINT ( 'NONE',  ( 10.81189881249999729, 6.242252689847867408, -107.7187500020483810 ) ) ;
#3628 = CARTESIAN_POINT ( 'NONE',  ( -10.81189881249999729, 1.324075727343319199E-15, -68.09375000204836681 ) ) ;
#3629 = CARTESIAN_POINT ( 'NONE',  ( -5.405949406250003975, -9.363379034771801557, -75.53125000204838102 ) ) ;
#3630 = CARTESIAN_POINT ( 'NONE',  ( 10.00000000000000000, 5.773502691896255534, -159.7500000040967905 ) ) ;
#3631 = CYLINDRICAL_SURFACE ( 'NONE', #11668, 9.999999999999998224 ) ;
#3632 = CARTESIAN_POINT ( 'NONE',  ( -10.81189881249999729, 6.242252689847871849, -161.4062500020483810 ) ) ;
#3633 = CARTESIAN_POINT ( 'NONE',  ( -5.405949406250003975, -9.363379034771801557, -168.5312500020484094 ) ) ;
#3634 = EDGE_CURVE ( 'NONE', #33917, #3910, #37833, .T. ) ;
#3635 = CARTESIAN_POINT ( 'NONE',  ( 0.000000000000000000, 0.000000000000000000, -99.99999999999998579 ) ) ;
#3636 = CARTESIAN_POINT ( 'NONE',  ( 5.405949406249999534, 9.363379034771803333, -2.593750002048367254 ) ) ;
#3637 = LINE ( 'NONE', #20229, #24071 ) ;
#3638 = CARTESIAN_POINT ( 'NONE',  ( -5.405949406250003975, -9.363379034771801557, -105.3437500020483810 ) ) ;
#3639 = CARTESIAN_POINT ( 'NONE',  ( -10.00000000000000000, -5.773502691896251982, -77.62499999999998579 ) ) ;
#3640 = CARTESIAN_POINT ( 'NONE',  ( -10.81189881249999729, 6.242252689847871849, -9.906250002048366810 ) ) ;
#3641 = CARTESIAN_POINT ( 'NONE',  ( 10.00000000000000000, 5.773502691896255534, -93.75000000409677625 ) ) ;
#3642 = CARTESIAN_POINT ( 'NONE',  ( -5.000000000000003553, -8.660254037844383745, -133.3750000040967905 ) ) ;
#3643 = CARTESIAN_POINT ( 'NONE',  ( 10.81189881249999551, -6.242252689847874514, -106.6562500020483952 ) ) ;
#3644 = CARTESIAN_POINT ( 'NONE',  ( 10.81189881249999729, 0.000000000000000000, -87.03125000204838102 ) ) ;
#3645 = ORIENTED_EDGE ( 'NONE', *, *, #22928, .T. ) ;
#3646 = CARTESIAN_POINT ( 'NONE',  ( -2.121150477449813534E-15, -11.54700538379251284, -85.25000000409676204 ) ) ;
#3647 = CARTESIAN_POINT ( 'NONE',  ( -9.999999999999479527, -5.773502691896549521, -141.0000000040967620 ) ) ;
#3648 = CARTESIAN_POINT ( 'NONE',  ( 5.405949406249999534, 9.363379034771803333, -43.09375000204837391 ) ) ;
#3649 = ORIENTED_EDGE ( 'NONE', *, *, #30246, .F. ) ;
#3650 = CARTESIAN_POINT ( 'NONE',  ( -9.999999999999998224, 1.224646799147353059E-15, -10.24999999999995381 ) ) ;
#3651 = CARTESIAN_POINT ( 'NONE',  ( 9.999999999999996447, -5.773502691896262640, -144.6250000000000000 ) ) ;
#3652 = CARTESIAN_POINT ( 'NONE',  ( 0.000000000000000000, 0.000000000000000000, -200.0000000000000000 ) ) ;
#3653 = CARTESIAN_POINT ( 'NONE',  ( -9.999999999999998224, 5.773502691896259087, -10.75000000409676026 ) ) ;
#3654 = EDGE_CURVE ( 'NONE', #9895, #13418, #3294, .T. ) ;
#3655 = CARTESIAN_POINT ( 'NONE',  ( 7.070501591499377789E-16, 11.54700538379251284, -189.1250000000000000 ) ) ;
#3656 = CARTESIAN_POINT ( 'NONE',  ( 9.999999999999998224, 0.000000000000000000, -96.49999999999998579 ) ) ;
#3658 = ORIENTED_EDGE ( 'NONE', *, *, #13010, .T. ) ;
#3657 = CARTESIAN_POINT ( 'NONE',  ( 10.81189881249999729, 0.000000000000000000, -117.0312500020483952 ) ) ;
#3659 = VERTEX_POINT ( 'NONE', #33966 ) ;
#3660 = CARTESIAN_POINT ( 'NONE',  ( -5.405949406250003975, -9.363379034771801557, -47.03125000204838813 ) ) ;
#3661 = PERSON_AND_ORGANIZATION ( #11915, #17965 ) ;
#3662 = CARTESIAN_POINT ( 'NONE',  ( 7.644554776091147741E-16, 12.48450537969573659, -95.46875000204839523 ) ) ;
#3663 = CARTESIAN_POINT ( 'NONE',  ( -5.405949406249996869, 9.363379034771805109, -124.0312500020483952 ) ) ;
#3664 = ORIENTED_EDGE ( 'NONE', *, *, #20347, .T. ) ;
#3665 = DIRECTION ( 'NONE',  ( 1.000000000000000000, 0.000000000000000000, 0.000000000000000000 ) ) ;
#3666 = CARTESIAN_POINT ( 'NONE',  ( 5.000000000000000000, 8.660254037844385522, -128.1250000040967620 ) ) ;
#3667 = CARTESIAN_POINT ( 'NONE',  ( 5.405949406249999534, 9.363379034771803333, -173.7812500020484094 ) ) ;
#3668 = CARTESIAN_POINT ( 'NONE',  ( 9.999999999999998224, 0.000000000000000000, -159.5000000000000000 ) ) ;
#3669 = CARTESIAN_POINT ( 'NONE',  ( 7.644554776091147741E-16, 12.48450537969573659, -135.9687500020483810 ) ) ;
#3670 =( BOUNDED_CURVE ( )  B_SPLINE_CURVE ( 2, ( #710, #40588, #33936, #1342, #17929, #503, #13618 ),
 .UNSPECIFIED., .F., .F. ) 
 B_SPLINE_CURVE_WITH_KNOTS ( ( 3, 2, 2, 3 ),
 ( 0.1007462686567163757, 0.1019900497512437887, 0.1032338308457712017, 0.1044776119402986148 ),
 .UNSPECIFIED. ) 
 CURVE ( )  GEOMETRIC_REPRESENTATION_ITEM ( )  RATIONAL_B_SPLINE_CURVE ( ( 1.000000000000004441, 0.8660254037844342667, 1.000000000000000000, 0.8660254037844387076, 1.000000000000000000, 0.8660254037844267172, 1.000000000000011990 ) ) 
 REPRESENTATION_ITEM ( '' )  );
#3671 = CARTESIAN_POINT ( 'NONE',  ( 10.81189881249999551, -6.242252689847874514, -104.9687500020483810 ) ) ;
#3672 = CARTESIAN_POINT ( 'NONE',  ( 10.00000000000051159, -5.773502691895965988, -44.12499999999996447 ) ) ;
#3673 = CARTESIAN_POINT ( 'NONE',  ( 5.405949406249999534, 9.363379034771803333, -104.7812500020483810 ) ) ;
#3674 = CARTESIAN_POINT ( 'NONE',  ( -2.121150477449813534E-15, -11.54700538379251284, -184.2500000040967905 ) ) ;
#3675 = CARTESIAN_POINT ( 'NONE',  ( -10.81189881249999729, -6.242252689847864744, -114.4687500020483810 ) ) ;
#3676 = CARTESIAN_POINT ( 'NONE',  ( 7.644554776091147741E-16, 12.48450537969573659, -182.6562500020484094 ) ) ;
#3677 = EDGE_CURVE ( 'NONE', #16045, #795, #18788, .T. ) ;
#3678 = FACE_OUTER_BOUND ( 'NONE', #38998, .T. ) ;
#3679 = CARTESIAN_POINT ( 'NONE',  ( -9.999999999999998224, 1.224646799147353059E-15, -184.6250000040967905 ) ) ;
#3680 = CARTESIAN_POINT ( 'NONE',  ( -2.121150477449813534E-15, -11.54700538379251284, -2.374999999999960920 ) ) ;
#3681 = CARTESIAN_POINT ( 'NONE',  ( -10.81189881249999729, -6.242252689847864744, -57.46875000204836681 ) ) ;
#3682 = CARTESIAN_POINT ( 'NONE',  ( -10.81189881249999907, -6.242252689847864744, -40.96875000204834549 ) ) ;
#3683 = CARTESIAN_POINT ( 'NONE',  ( 10.00000000000000000, 5.773502691896255534, -183.7500000040968189 ) ) ;
#3684 = CARTESIAN_POINT ( 'NONE',  ( 10.81189881249999729, 0.000000000000000000, -21.03125000204836326 ) ) ;
#3685 = CARTESIAN_POINT ( 'NONE',  ( 5.405949406249992428, -9.363379034771808662, -27.09375000204835970 ) ) ;
#3686 = CARTESIAN_POINT ( 'NONE',  ( 5.000000000000000000, -20.00000000000000000, -219.9999999999999716 ) ) ;
#3687 = CARTESIAN_POINT ( 'NONE',  ( -10.81189881249999907, -6.242252689847864744, -141.4687500020484094 ) ) ;
#3688 = CARTESIAN_POINT ( 'NONE',  ( -9.999999999999998224, 5.773502691896259087, -109.3750000000000000 ) ) ;
#3689 = CARTESIAN_POINT ( 'NONE',  ( 7.644554776091147741E-16, 12.48450537969573659, -37.15625000204836681 ) ) ;
#3690 = CARTESIAN_POINT ( 'NONE',  ( 9.999999999999227285, 5.773502691896701400, -111.3749999999999432 ) ) ;
#3691 = CARTESIAN_POINT ( 'NONE',  ( -10.00000000000000000, -5.773502691896251982, -58.12499999999997868 ) ) ;
#3692 = CARTESIAN_POINT ( 'NONE',  ( 7.644554776091147741E-16, 12.48450537969573659, -128.6562500020483810 ) ) ;
#3693 = CARTESIAN_POINT ( 'NONE',  ( -10.81189881249999729, 6.242252689847871849, -105.9062500020483810 ) ) ;
#3694 = ORIENTED_EDGE ( 'NONE', *, *, #5638, .T. ) ;
#3695 = CARTESIAN_POINT ( 'NONE',  ( 4.999999999999992006, -8.660254037844389075, -131.2499999999999716 ) ) ;
#3696 = CARTESIAN_POINT ( 'NONE',  ( 5.000000000000000000, 8.660254037844385522, -105.6250000040967763 ) ) ;
#3697 = CARTESIAN_POINT ( 'NONE',  ( 9.999999999999998224, 0.000000000000000000, -200.0000000000000000 ) ) ;
#3698 = CARTESIAN_POINT ( 'NONE',  ( 10.81189881249999551, -6.242252689847874514, -65.96875000204838102 ) ) ;
#3699 = ORIENTED_EDGE ( 'NONE', *, *, #17219, .F. ) ;
#3700 = CARTESIAN_POINT ( 'NONE',  ( -2.121150477449813534E-15, -11.54700538379251284, -30.87499999999995381 ) ) ;
#3701 = CARTESIAN_POINT ( 'NONE',  ( -4.999999999999996447, 8.660254037844387298, -21.37500000409675494 ) ) ;
#3702 = CARTESIAN_POINT ( 'NONE',  ( 5.405949406249992428, -9.363379034771808662, -45.28125000204838102 ) ) ;
#3703 = CARTESIAN_POINT ( 'NONE',  ( 9.999999999999998224, 0.000000000000000000, -200.0000000000000000 ) ) ;
#3704 = CARTESIAN_POINT ( 'NONE',  ( -9.999999999999998224, 1.224646799147353059E-15, -33.12500000409676915 ) ) ;
#3705 = DIRECTION ( 'NONE',  ( -1.000000000000000000, 0.000000000000000000, 0.000000000000000000 ) ) ;
#3706 = CARTESIAN_POINT ( 'NONE',  ( -10.81189881249999729, 6.242252689847871849, -140.4062500020484094 ) ) ;
#3707 = ADVANCED_FACE ( 'NONE', ( #31585 ), #42117, .F. ) ;
#3708 = CARTESIAN_POINT ( 'NONE',  ( 9.999999999999998224, 0.000000000000000000, -200.0000000000000000 ) ) ;
#3709 = ORIENTED_EDGE ( 'NONE', *, *, #5480, .F. ) ;
#3710 = EDGE_LOOP ( 'NONE', ( #40304, #16626, #8914, #34396 ) ) ;
#3711 = VERTEX_POINT ( 'NONE', #18397 ) ;
#3712 = CARTESIAN_POINT ( 'NONE',  ( 7.070501591499376803E-16, 11.54700538379251284, -126.5000000040967763 ) ) ;
#3713 = FACE_OUTER_BOUND ( 'NONE', #41486, .T. ) ;
#3714 =( BOUNDED_CURVE ( )  B_SPLINE_CURVE ( 2, ( #9803, #32493, #3128, #39575, #33126, #13442, #6158 ),
 .UNSPECIFIED., .F., .F. ) 
 B_SPLINE_CURVE_WITH_KNOTS ( ( 3, 2, 2, 3 ),
 ( 0.6305970149253732338, 0.6318407960199006190, 0.6330845771144280043, 0.6343283582089553896 ),
 .UNSPECIFIED. ) 
 CURVE ( )  GEOMETRIC_REPRESENTATION_ITEM ( )  RATIONAL_B_SPLINE_CURVE ( ( 0.9999999999999880096, 0.8660254037844506980, 1.000000000000000000, 0.8660254037844387076, 1.000000000000000000, 0.8660254037844267172, 1.000000000000011990 ) ) 
 REPRESENTATION_ITEM ( '' )  );
#3715 = CARTESIAN_POINT ( 'NONE',  ( 5.405949406249992428, -9.363379034771808662, -171.0937500020484094 ) ) ;
#3716 = CARTESIAN_POINT ( 'NONE',  ( -5.405949406249996869, 9.363379034771805109, -196.0312500020484094 ) ) ;
#3717 = CARTESIAN_POINT ( 'NONE',  ( 10.81189881249999907, 6.242252689847868297, -25.21875000204837036 ) ) ;
#3718 = CARTESIAN_POINT ( 'NONE',  ( -10.00000000000051337, 5.773502691895962435, -144.2500000040967905 ) ) ;
#3719 = CARTESIAN_POINT ( 'NONE',  ( 0.000000000000000000, 0.000000000000000000, -200.0000000000000000 ) ) ;
#3720 = CARTESIAN_POINT ( 'NONE',  ( 5.405949406249999534, 9.363379034771803333, -152.5937500020483810 ) ) ;
#3721 = CARTESIAN_POINT ( 'NONE',  ( 10.81189881249999551, -6.242252689847874514, -136.4687500020483810 ) ) ;
#3722 = CARTESIAN_POINT ( 'NONE',  ( 10.81189881249999907, 6.242252689847868297, -124.2187500020483952 ) ) ;
#3723 = CARTESIAN_POINT ( 'NONE',  ( -10.81189881249999729, 6.242252689847871849, -131.4062500020484094 ) ) ;
#3724 = CARTESIAN_POINT ( 'NONE',  ( -10.81189881249999729, 1.324075727343319199E-15, -14.09375000204834905 ) ) ;
#3725 = CARTESIAN_POINT ( 'NONE',  ( 7.644554776091147741E-16, 12.48450537969573659, -135.9687500020483810 ) ) ;
#3726 = DIRECTION ( 'NONE',  ( -1.000000000000000000, -1.734723475976806848E-16, 0.000000000000000000 ) ) ;
#3727 = CYLINDRICAL_SURFACE ( 'NONE', #28925, 9.999999999999998224 ) ;
#3728 = CARTESIAN_POINT ( 'NONE',  ( -4.999999999999996447, 8.660254037844387298, -153.0000000000000000 ) ) ;
#3729 = CARTESIAN_POINT ( 'NONE',  ( 9.999999999998969713, 5.773502691896851502, -56.25000000409675494 ) ) ;
#3730 = CARTESIAN_POINT ( 'NONE',  ( 10.81189881249999729, 6.242252689847867408, -83.71875000204836681 ) ) ;
#3731 = CARTESIAN_POINT ( 'NONE',  ( -2.293366432827344421E-15, -12.48450537969573659, -75.21875000204839523 ) ) ;
#3732 = CARTESIAN_POINT ( 'NONE',  ( -5.405949406249996869, 9.363379034771805109, -43.03125000204838102 ) ) ;
#3733 = CARTESIAN_POINT ( 'NONE',  ( -2.293366432827344421E-15, -12.48450537969573659, -57.21875000204836681 ) ) ;
#3734 = CARTESIAN_POINT ( 'NONE',  ( -9.999999999999479527, -5.773502691896549521, -139.5000000040967620 ) ) ;
#3735 = CARTESIAN_POINT ( 'NONE',  ( -5.405949406250003975, -9.363379034771801557, -162.3437500020484094 ) ) ;
#3736 = CARTESIAN_POINT ( 'NONE',  ( 9.999999999999998224, 0.000000000000000000, -131.0000000000000000 ) ) ;
#3737 = CARTESIAN_POINT ( 'NONE',  ( -5.405949406249996869, 9.363379034771805109, -140.5312500020484094 ) ) ;
#3738 = LINE ( 'NONE', #6752, #8951 ) ;
#3739 = CARTESIAN_POINT ( 'NONE',  ( 4.999999999999992006, -8.660254037844389075, -83.24999999999997158 ) ) ;
#3740 = EDGE_LOOP ( 'NONE', ( #29551, #84, #2315, #31538 ) ) ;
#3741 = CARTESIAN_POINT ( 'NONE',  ( -5.405949406250003975, -9.363379034771801557, -108.5312500020483810 ) ) ;
#3742 = CARTESIAN_POINT ( 'NONE',  ( -9.999999999999998224, 5.773502691896259087, -135.2500000040967905 ) ) ;
#3743 = CARTESIAN_POINT ( 'NONE',  ( -9.999999999999998224, 1.224646799147353059E-15, -200.0000000000000000 ) ) ;
#3744 = CARTESIAN_POINT ( 'NONE',  ( 5.405949406249999534, 9.363379034771803333, -167.7812500020484094 ) ) ;
#3745 = CARTESIAN_POINT ( 'NONE',  ( 9.999999999999998224, 0.000000000000000000, -44.37500000409677625 ) ) ;
#3746 = DIRECTION ( 'NONE',  ( 1.000000000000000000, 0.000000000000000000, 0.000000000000000000 ) ) ;
#3747 = CARTESIAN_POINT ( 'NONE',  ( 10.81189881249999729, 0.000000000000000000, -52.53125000204835970 ) ) ;
#3748 = CARTESIAN_POINT ( 'NONE',  ( 10.81189881249999551, -6.242252689847874514, -159.1562500020484094 ) ) ;
#3749 = CARTESIAN_POINT ( 'NONE',  ( 5.405949406249992428, -9.363379034771808662, -138.0937500020483810 ) ) ;
#3750 = CARTESIAN_POINT ( 'NONE',  ( -9.999999999999998224, 1.224646799147353059E-15, -200.0000000000000000 ) ) ;
#3752 = EDGE_CURVE ( 'NONE', #37078, #21806, #1412, .T. ) ;
#3751 = CARTESIAN_POINT ( 'NONE',  ( 5.000000000000000000, 8.660254037844385522, -150.2500000000000000 ) ) ;
#3753 = EDGE_LOOP ( 'NONE', ( #37343, #15976, #39421, #31216 ) ) ;
#3754 = EDGE_CURVE ( 'NONE', #16498, #28563, #32224, .T. ) ;
#3755 = CARTESIAN_POINT ( 'NONE',  ( -10.00000000000102496, 5.773502691895664007, -130.7500000040967620 ) ) ;
#3757 = VERTEX_POINT ( 'NONE', #8489 ) ;
#3756 = CARTESIAN_POINT ( 'NONE',  ( -10.81189881249999729, 6.242252689847871849, -72.90625000204838102 ) ) ;
#3758 = APPLICATION_PROTOCOL_DEFINITION ( 'international standard', 'config_control_design', 1994, #15686 ) ;
#3760 = ORIENTED_EDGE ( 'NONE', *, *, #6144, .F. ) ;
#3759 = CARTESIAN_POINT ( 'NONE',  ( -10.81189881249999729, 1.324075727343319199E-15, -116.0937500020483810 ) ) ;
#3761 = CARTESIAN_POINT ( 'NONE',  ( -10.81189881249999729, 1.324075727343319199E-15, -23.09375000204835615 ) ) ;
#3762 = CARTESIAN_POINT ( 'NONE',  ( 10.81189881249999729, 0.000000000000000000, -1.531250002048373249 ) ) ;
#3763 = CARTESIAN_POINT ( 'NONE',  ( -5.405949406249996869, 9.363379034771805109, -50.34375000204835260 ) ) ;
#3764 = DIRECTION ( 'NONE',  ( -1.000000000000000000, 0.000000000000000000, 0.000000000000000000 ) ) ;
#3765 = FACE_OUTER_BOUND ( 'NONE', #29723, .T. ) ;
#3766 = CARTESIAN_POINT ( 'NONE',  ( 5.405949406249992428, -9.363379034771808662, -180.0937500020484094 ) ) ;
#3767 = CARTESIAN_POINT ( 'NONE',  ( 7.644554776091147741E-16, 12.48450537969573659, -170.4687500020483810 ) ) ;
#3768 = CARTESIAN_POINT ( 'NONE',  ( -10.81189881249999729, 1.324075727343319199E-15, -146.0937500020483810 ) ) ;
#3769 = CARTESIAN_POINT ( 'NONE',  ( 7.644554776091147741E-16, 12.48450537969573659, -162.9687500020483810 ) ) ;
#3770 = CARTESIAN_POINT ( 'NONE',  ( 9.999999999999998224, 0.000000000000000000, -146.3750000040967905 ) ) ;
#3771 = CARTESIAN_POINT ( 'NONE',  ( 9.999999999999872102, 5.773502691896329253, -193.8750000000000284 ) ) ;
#3772 = CARTESIAN_POINT ( 'NONE',  ( 9.999999999999996447, -5.773502691896262640, -182.1250000000000000 ) ) ;
#3773 = CARTESIAN_POINT ( 'NONE',  ( -10.81189881249999907, -6.242252689847864744, -97.96875000204838102 ) ) ;
#3774 = CARTESIAN_POINT ( 'NONE',  ( -10.00000000000102496, 5.773502691895664007, -34.37499999999994316 ) ) ;
#3775 = CARTESIAN_POINT ( 'NONE',  ( 10.81189881249999551, -6.242252689847874514, -63.15625000204837391 ) ) ;
#3776 = CARTESIAN_POINT ( 'NONE',  ( 10.81189881249999907, 6.242252689847868297, -188.7187500020484094 ) ) ;
#3777 = ADVANCED_FACE ( 'NONE', ( #12131 ), #31370, .T. ) ;
#3778 = CARTESIAN_POINT ( 'NONE',  ( -10.81189881249999729, 1.324075727343319199E-15, -123.7812500020483952 ) ) ;
#3779 = CARTESIAN_POINT ( 'NONE',  ( -5.405949406250003975, -9.363379034771801557, -159.5312500020484094 ) ) ;
#3780 = CARTESIAN_POINT ( 'NONE',  ( 10.81189881249999907, 6.242252689847868297, -53.90625000204838102 ) ) ;
#3781 = CARTESIAN_POINT ( 'NONE',  ( 4.999999999999992006, -8.660254037844389075, -137.6250000040967620 ) ) ;
#3782 = CARTESIAN_POINT ( 'NONE',  ( 9.999999999999996447, -5.773502691896262640, -119.1249999999999858 ) ) ;
#3783 = ORIENTED_EDGE ( 'NONE', *, *, #13665, .T. ) ;
#3784 = VECTOR ( 'NONE', #4002, 1000.000000000000000 ) ;
#3785 = CARTESIAN_POINT ( 'NONE',  ( -2.293366432827344421E-15, -12.48450537969573659, -132.4062500020483810 ) ) ;
#3786 = CARTESIAN_POINT ( 'NONE',  ( -10.81189881249999729, 6.242252689847871849, -144.9062500020484094 ) ) ;
#3787 = CARTESIAN_POINT ( 'NONE',  ( -10.81189881249999729, 6.242252689847871849, -191.4062500020484094 ) ) ;
#3788 = CARTESIAN_POINT ( 'NONE',  ( 4.999999999999992006, -8.660254037844389075, -125.2500000000000000 ) ) ;
#3789 = CARTESIAN_POINT ( 'NONE',  ( -5.405949406249996869, 9.363379034771805109, -80.34375000204838102 ) ) ;
#3790 = VERTEX_POINT ( 'NONE', #25322 ) ;
#3791 = CARTESIAN_POINT ( 'NONE',  ( 9.999999999999996447, -5.773502691896262640, -54.62499999999996447 ) ) ;
#3792 = CARTESIAN_POINT ( 'NONE',  ( 10.81189881249999729, 0.000000000000000000, -176.8437500020483810 ) ) ;
#3793 = CARTESIAN_POINT ( 'NONE',  ( -5.000000000000003553, -8.660254037844383745, -68.87500000409677625 ) ) ;
#3794 = PLANE ( 'NONE',  #12718 ) ;
#3795 = CARTESIAN_POINT ( 'NONE',  ( -9.999999999999998224, 1.224646799147353059E-15, -135.1250000040967620 ) ) ;
#3796 = CARTESIAN_POINT ( 'NONE',  ( -10.81189881249999907, -6.242252689847864744, -74.15625000204835260 ) ) ;
#3797 = CARTESIAN_POINT ( 'NONE',  ( 10.81189881249999551, -6.242252689847874514, -57.15625000204837391 ) ) ;
#3798 = CARTESIAN_POINT ( 'NONE',  ( 4.999999999999992006, -8.660254037844389075, -55.12500000409675494 ) ) ;
#3799 = CARTESIAN_POINT ( 'NONE',  ( 10.81189881249999907, 6.242252689847868297, -11.71875000204836148 ) ) ;
#3800 = CARTESIAN_POINT ( 'NONE',  ( 10.81189881249999907, 6.242252689847868297, -182.9062500020484094 ) ) ;
#3801 = CARTESIAN_POINT ( 'NONE',  ( 10.81189881249999729, 0.000000000000000000, -6.031250002048377468 ) ) ;
#3802 = CARTESIAN_POINT ( 'NONE',  ( -9.999999999999998224, 1.224646799147353059E-15, -40.24999999999997868 ) ) ;
#3804 = EDGE_CURVE ( 'NONE', #17414, #18914, #11916, .T. ) ;
#3803 = CARTESIAN_POINT ( 'NONE',  ( 0.000000000000000000, 0.000000000000000000, -200.0000000000000000 ) ) ;
#3805 = CARTESIAN_POINT ( 'NONE',  ( -9.999999999999998224, 1.224646799147353059E-15, -116.7499999999999858 ) ) ;
#3806 = CARTESIAN_POINT ( 'NONE',  ( -9.885120488223384072, 1.745261150048159848, -0.000000000000000000 ) ) ;
#3807 = CIRCLE ( 'NONE', #15519, 20.00000000000000355 ) ;
#3808 = ADVANCED_FACE ( 'NONE', ( #21641 ), #22074, .T. ) ;
#3809 = CYLINDRICAL_SURFACE ( 'NONE', #33768, 9.999999999999998224 ) ;
#3810 = ADVANCED_FACE ( 'NONE', ( #1804 ), #25535, .F. ) ;
#3812 = ORIENTED_EDGE ( 'NONE', *, *, #16436, .F. ) ;
#3811 = CARTESIAN_POINT ( 'NONE',  ( -2.293366432827344421E-15, -12.48450537969573659, -96.40625000204839523 ) ) ;
#3813 = CARTESIAN_POINT ( 'NONE',  ( -9.999999999999742428, -5.773502691896402084, -160.5000000040968189 ) ) ;
#3815 = ORIENTED_EDGE ( 'NONE', *, *, #21256, .T. ) ;
#3814 = CARTESIAN_POINT ( 'NONE',  ( -10.81189881249999729, 1.324075727343319199E-15, -102.5937500020483810 ) ) ;
#3816 = VERTEX_POINT ( 'NONE', #28345 ) ;
#3817 = CARTESIAN_POINT ( 'NONE',  ( -10.81189881249999907, -6.242252689847864744, -30.46875000204834549 ) ) ;
#3818 = VECTOR ( 'NONE', #15763, 1000.000000000000000 ) ;
#3819 = CARTESIAN_POINT ( 'NONE',  ( 10.81189881249999907, 6.242252689847868297, -23.90625000204838102 ) ) ;
#3820 = CARTESIAN_POINT ( 'NONE',  ( 10.81189881249999551, -6.242252689847874514, -68.96875000204839523 ) ) ;
#3821 = CARTESIAN_POINT ( 'NONE',  ( -9.999999999999998224, 0.000000000000000000, -99.99999999999998579 ) ) ;
#3822 = CARTESIAN_POINT ( 'NONE',  ( -9.999999999999998224, 5.773502691896259087, -43.37499999999997158 ) ) ;
#3823 = EDGE_CURVE ( 'NONE', #32468, #18020, #32051, .T. ) ;
#3824 = CARTESIAN_POINT ( 'NONE',  ( -10.81189881249999907, -6.242252689847864744, -196.9687500020484379 ) ) ;
#3825 = CARTESIAN_POINT ( 'NONE',  ( -5.405949406249996869, 9.363379034771805109, -153.8437500020483810 ) ) ;
#3826 = EDGE_CURVE ( 'NONE', #8327, #39928, #26234, .T. ) ;
#3827 = CARTESIAN_POINT ( 'NONE',  ( 9.999999999999998224, 0.000000000000000000, -174.8750000040967905 ) ) ;
#3828 = CARTESIAN_POINT ( 'NONE',  ( 0.000000000000000000, 0.000000000000000000, -180.0000000000000000 ) ) ;
#3829 = CARTESIAN_POINT ( 'NONE',  ( 10.81189881249999551, -6.242252689847874514, -145.6562500020484094 ) ) ;
#3830 = CARTESIAN_POINT ( 'NONE',  ( 9.999999999999996447, -5.773502691896262640, -5.500000004096770034 ) ) ;
#3831 = FACE_OUTER_BOUND ( 'NONE', #7684, .T. ) ;
#3832 = CARTESIAN_POINT ( 'NONE',  ( 10.81189881249999551, -6.242252689847874514, -122.9687500020483810 ) ) ;
#3833 = CARTESIAN_POINT ( 'NONE',  ( -4.999999999999996447, 8.660254037844387298, -141.0000000000000000 ) ) ;
#3834 = CARTESIAN_POINT ( 'NONE',  ( 7.644554776091147741E-16, 12.48450537969573659, -89.65625000204839523 ) ) ;
#3835 = CARTESIAN_POINT ( 'NONE',  ( 7.644554776091147741E-16, 12.48450537969573659, -101.4687500020483668 ) ) ;
#3836 = CARTESIAN_POINT ( 'NONE',  ( -5.405949406249996869, 9.363379034771805109, -72.84375000204838102 ) ) ;
#3837 = VECTOR ( 'NONE', #20697, 1000.000000000000000 ) ;
#3838 = CARTESIAN_POINT ( 'NONE',  ( -5.405949406250003975, -9.363379034771801557, -74.03125000204838102 ) ) ;
#3839 = CARTESIAN_POINT ( 'NONE',  ( 10.00000000000000000, 5.773502691896255534, -158.2500000040967905 ) ) ;
#3840 =( BOUNDED_CURVE ( )  B_SPLINE_CURVE ( 2, ( #21959, #18505, #27588, #8387, #25011, #11169, #38153 ),
 .UNSPECIFIED., .F., .F. ) 
 B_SPLINE_CURVE_WITH_KNOTS ( ( 3, 2, 2, 3 ),
 ( 0.4626865671641792743, 0.4639303482587066596, 0.4651741293532339339, 0.4664179104477613191 ),
 .UNSPECIFIED. ) 
 CURVE ( )  GEOMETRIC_REPRESENTATION_ITEM ( )  RATIONAL_B_SPLINE_CURVE ( ( 0.9999999999999820144, 0.8660254037844566932, 1.000000000000000000, 0.8660254037844387076, 1.000000000000000000, 0.8660254037844267172, 1.000000000000011990 ) ) 
 REPRESENTATION_ITEM ( '' )  );
#3841 = CARTESIAN_POINT ( 'NONE',  ( -5.405949406249996869, 9.363379034771805109, -157.0312500020484094 ) ) ;
#3842 = CARTESIAN_POINT ( 'NONE',  ( 5.405949406249999534, 9.363379034771803333, -172.2812500020484094 ) ) ;
#3843 = DIRECTION ( 'NONE',  ( 0.000000000000000000, 0.000000000000000000, -1.000000000000000000 ) ) ;
#3844 = CARTESIAN_POINT ( 'NONE',  ( 4.999999999999992006, -8.660254037844389075, -53.62500000409675494 ) ) ;
#3845 = CARTESIAN_POINT ( 'NONE',  ( 10.81189881249999729, 0.000000000000000000, -109.3437500020483810 ) ) ;
#3846 = CARTESIAN_POINT ( 'NONE',  ( -9.999999999999998224, 5.773502691896259087, -83.87499999999998579 ) ) ;
#3847 = CARTESIAN_POINT ( 'NONE',  ( 7.644554776091147741E-16, 12.48450537969573659, -4.156250002048361480 ) ) ;
#3848 = CARTESIAN_POINT ( 'NONE',  ( -5.000000000000003553, -8.660254037844383745, -88.37500000409677625 ) ) ;
#3849 = AXIS2_PLACEMENT_3D ( 'NONE', #1319, #24205, #10796 ) ;
#3850 = CARTESIAN_POINT ( 'NONE',  ( -5.000000000000003553, -8.660254037844383745, -169.0000000000000000 ) ) ;
#3851 = CARTESIAN_POINT ( 'NONE',  ( -10.81189881249999907, -6.242252689847864744, -96.65625000204839523 ) ) ;
#3852 = CARTESIAN_POINT ( 'NONE',  ( -10.81189881249999729, 1.324075727343319199E-15, -84.78125000204838102 ) ) ;
#3853 = ORIENTED_EDGE ( 'NONE', *, *, #24630, .F. ) ;
#3854 = CARTESIAN_POINT ( 'NONE',  ( -4.999999999999996447, 8.660254037844387298, -78.37500000409677625 ) ) ;
#3855 = CARTESIAN_POINT ( 'NONE',  ( 9.999999999999998224, 0.000000000000000000, -140.3750000040967905 ) ) ;
#3856 = CARTESIAN_POINT ( 'NONE',  ( -5.405949406250003975, -9.363379034771801557, -34.84375000204836681 ) ) ;
#3857 = ORIENTED_EDGE ( 'NONE', *, *, #28973, .F. ) ;
#3858 = CARTESIAN_POINT ( 'NONE',  ( 4.999999999999992006, -8.660254037844389075, -12.74999999999995559 ) ) ;
#3859 = CARTESIAN_POINT ( 'NONE',  ( 10.81189881249999729, 0.000000000000000000, -34.53125000204837391 ) ) ;
#3860 = CARTESIAN_POINT ( 'NONE',  ( -9.999999999999998224, 1.224646799147353059E-15, -148.2500000000000000 ) ) ;
#3861 = DIRECTION ( 'NONE',  ( -0.000000000000000000, -0.000000000000000000, -1.000000000000000000 ) ) ;
#3862 = CARTESIAN_POINT ( 'NONE',  ( 4.999999999999992006, -8.660254037844389075, -10.12500000409674605 ) ) ;
#3863 = CARTESIAN_POINT ( 'NONE',  ( 5.000000000000000000, 8.660254037844385522, -187.7500000000000000 ) ) ;
#3864 = DIRECTION ( 'NONE',  ( -0.000000000000000000, -0.000000000000000000, 1.000000000000000000 ) ) ;
#3865 = APPLICATION_CONTEXT ( 'configuration controlled 3d designs of mechanical parts and assemblies' ) ;
#3867 = VERTEX_POINT ( 'NONE', #8911 ) ;
#3866 = CARTESIAN_POINT ( 'NONE',  ( 7.644554776091147741E-16, 12.48450537969573659, -119.6562500020484094 ) ) ;
#3868 = CARTESIAN_POINT ( 'NONE',  ( 5.000000000000000000, 8.660254037844385522, -36.62500000409676915 ) ) ;
#3869 = ORIENTED_EDGE ( 'NONE', *, *, #4709, .F. ) ;
#3870 = ORIENTED_EDGE ( 'NONE', *, *, #21602, .F. ) ;
#3871 = CARTESIAN_POINT ( 'NONE',  ( 10.81189881249999729, 0.000000000000000000, -43.53125000204838102 ) ) ;
#3872 = DATE_AND_TIME ( #3440, #20081 ) ;
#3873 = EDGE_CURVE ( 'NONE', #31913, #1269, #5826, .T. ) ;
#3874 = CARTESIAN_POINT ( 'NONE',  ( 5.405949406249992428, -9.363379034771808662, -93.09375000204838102 ) ) ;
#3875 = CARTESIAN_POINT ( 'NONE',  ( -10.81189881249999729, -6.242252689847864744, -125.1562500020483810 ) ) ;
#3876 = ORIENTED_EDGE ( 'NONE', *, *, #22021, .T. ) ;
#3877 = VECTOR ( 'NONE', #964, 1000.000000000000000 ) ;
#3878 = CARTESIAN_POINT ( 'NONE',  ( 5.000000000000000000, 8.660254037844385522, -51.62500000409675494 ) ) ;
#3879 = CARTESIAN_POINT ( 'NONE',  ( -2.293366432827344421E-15, -12.48450537969573659, -193.7187500020484094 ) ) ;
#3880 = CARTESIAN_POINT ( 'NONE',  ( -2.293366432827344421E-15, -12.48450537969573659, -172.9062500020484379 ) ) ;
#3881 = DIRECTION ( 'NONE',  ( -1.000000000000000000, 0.000000000000000000, 0.000000000000000000 ) ) ;
#3882 = CARTESIAN_POINT ( 'NONE',  ( 7.644554776091147741E-16, 12.48450537969573659, -129.9687500020483810 ) ) ;
#3883 = CARTESIAN_POINT ( 'NONE',  ( 10.81189881249999729, 0.000000000000000000, -89.84375000204838102 ) ) ;
#3884 = CARTESIAN_POINT ( 'NONE',  ( 10.81189881249999907, 6.242252689847868297, -101.9062500020484094 ) ) ;
#3885 = CARTESIAN_POINT ( 'NONE',  ( 7.070501591499377789E-16, 11.54700538379251284, -189.5000000040968189 ) ) ;
#3886 = CARTESIAN_POINT ( 'NONE',  ( 10.81189881249999729, 0.000000000000000000, -110.8437500020483810 ) ) ;
#3887 = CARTESIAN_POINT ( 'NONE',  ( -10.81189881249999729, 1.324075727343319199E-15, -176.2812500020484094 ) ) ;
#3888 = DIRECTION ( 'NONE',  ( -0.3779644730092261984, 0.6546536707079756434, -0.6546536707079793072 ) ) ;
#3889 = CARTESIAN_POINT ( 'NONE',  ( -1.040834085586084257E-14, 145.0000000000000000, 22.49999999999999289 ) ) ;
#3890 = CARTESIAN_POINT ( 'NONE',  ( -5.405949406250003975, -9.363379034771801557, -195.5312500020484094 ) ) ;
#3891 = CARTESIAN_POINT ( 'NONE',  ( -10.81189881249999729, 1.324075727343319199E-15, -62.09375000204836681 ) ) ;
#3892 = CARTESIAN_POINT ( 'NONE',  ( 5.405949406249992428, -9.363379034771808662, -45.09375000204837391 ) ) ;
#3893 = CARTESIAN_POINT ( 'NONE',  ( 7.070501591499377789E-16, 11.54700538379251284, -170.0000000040967905 ) ) ;
#3894 = CARTESIAN_POINT ( 'NONE',  ( 10.81189881249999907, 6.242252689847868297, -17.90625000204837036 ) ) ;
#3895 = CARTESIAN_POINT ( 'NONE',  ( 5.405949406249992428, -9.363379034771808662, -24.09375000204835970 ) ) ;
#3896 = DIRECTION ( 'NONE',  ( -1.000000000000000000, 0.000000000000000000, 0.000000000000000000 ) ) ;
#3897 = CARTESIAN_POINT ( 'NONE',  ( -10.81189881249999907, -6.242252689847864744, -126.4687500020483810 ) ) ;
#3898 = CARTESIAN_POINT ( 'NONE',  ( 5.000000000000000000, 8.660254037844385522, -106.7499999999999858 ) ) ;
#3899 = CARTESIAN_POINT ( 'NONE',  ( 10.81189881249999729, 0.000000000000000000, -27.03125000204836681 ) ) ;
#3900 = CARTESIAN_POINT ( 'NONE',  ( 10.00000000000051159, -5.773502691895965988, -49.00000000409676204 ) ) ;
#3901 = VECTOR ( 'NONE', #38849, 1000.000000000000000 ) ;
#3902 = CARTESIAN_POINT ( 'NONE',  ( -2.121150477449813534E-15, -11.54700538379251284, -62.37499999999998579 ) ) ;
#3903 = CARTESIAN_POINT ( 'NONE',  ( 10.81189881249999551, -6.242252689847874514, -127.6562500020483952 ) ) ;
#3904 = CARTESIAN_POINT ( 'NONE',  ( -5.405949406249996869, 9.363379034771805109, -107.5312500020483810 ) ) ;
#3905 = ORIENTED_EDGE ( 'NONE', *, *, #24377, .T. ) ;
#3906 = CARTESIAN_POINT ( 'NONE',  ( 10.00000000000025402, -5.773502691896113426, -131.1250000000000000 ) ) ;
#3907 = CARTESIAN_POINT ( 'NONE',  ( -5.000000000000003553, -8.660254037844383745, -104.8750000040967763 ) ) ;
#3908 = DIRECTION ( 'NONE',  ( -0.000000000000000000, -0.000000000000000000, 1.000000000000000000 ) ) ;
#3909 = CARTESIAN_POINT ( 'NONE',  ( 10.81189881249999907, 6.242252689847868297, -58.21875000204838102 ) ) ;
#3910 = VERTEX_POINT ( 'NONE', #23131 ) ;
#3911 = CARTESIAN_POINT ( 'NONE',  ( 4.999999999999992006, -8.660254037844389075, -32.24999999999997158 ) ) ;
#3912 = CARTESIAN_POINT ( 'NONE',  ( -10.81189881249999729, -6.242252689847864744, -35.15625000204836681 ) ) ;
#3913 = DIRECTION ( 'NONE',  ( -1.000000000000000000, 0.000000000000000000, 0.000000000000000000 ) ) ;
#3914 = CARTESIAN_POINT ( 'NONE',  ( 10.00000000000000000, 5.773502691896255534, -39.75000000409675494 ) ) ;
#3915 = CARTESIAN_POINT ( 'NONE',  ( 5.000000000000000000, 8.660254037844385522, -57.62500000409676204 ) ) ;
#3916 = CARTESIAN_POINT ( 'NONE',  ( -10.81189881249999907, -6.242252689847864744, -140.1562500020484094 ) ) ;
#3917 = CARTESIAN_POINT ( 'NONE',  ( -9.999999999999998224, 1.224646799147353059E-15, -97.62500000409677625 ) ) ;
#3918 = ORIENTED_EDGE ( 'NONE', *, *, #9375, .T. ) ;
#3919 = ORIENTED_EDGE ( 'NONE', *, *, #30488, .F. ) ;
#3920 =( BOUNDED_CURVE ( )  B_SPLINE_CURVE ( 2, ( #39230, #29110, #32980, #3409, #25867, #25658, #16327 ),
 .UNSPECIFIED., .F., .F. ) 
 B_SPLINE_CURVE_WITH_KNOTS ( ( 3, 2, 2, 3 ),
 ( 0.5820895522388062071, 0.5833333333333335924, 0.5845771144278607556, 0.5858208955223881409 ),
 .UNSPECIFIED. ) 
 CURVE ( )  GEOMETRIC_REPRESENTATION_ITEM ( )  RATIONAL_B_SPLINE_CURVE ( ( 0.9999999999999761302, 0.8660254037844625774, 1.000000000000000000, 0.8660254037844387076, 1.000000000000000000, 0.8660254037844267172, 1.000000000000011990 ) ) 
 REPRESENTATION_ITEM ( '' )  );
#3921 = CARTESIAN_POINT ( 'NONE',  ( 5.000000000000000000, 8.660254037844385522, -159.2500000000000000 ) ) ;
#3922 = LINE ( 'NONE', #9957, #4940 ) ;
#3923 = CARTESIAN_POINT ( 'NONE',  ( 5.405949406249999534, 9.363379034771803333, -169.0937500020484094 ) ) ;
#3924 = CARTESIAN_POINT ( 'NONE',  ( 5.405949406249999534, 9.363379034771803333, -194.7812500020484094 ) ) ;
#3925 = CARTESIAN_POINT ( 'NONE',  ( -5.405949406249996869, 9.363379034771805109, -20.34375000204835615 ) ) ;
#3926 = DIRECTION ( 'NONE',  ( 0.000000000000000000, 0.000000000000000000, -1.000000000000000000 ) ) ;
#3927 = CARTESIAN_POINT ( 'NONE',  ( -5.405949406250003975, -9.363379034771801557, -159.3437500020484094 ) ) ;
#3928 = CARTESIAN_POINT ( 'NONE',  ( 5.405949406249999534, 9.363379034771803333, -137.5937500020483810 ) ) ;
#3929 = DIRECTION ( 'NONE',  ( -0.000000000000000000, -0.000000000000000000, 1.000000000000000000 ) ) ;
#3930 = CARTESIAN_POINT ( 'NONE',  ( -5.405949406249996869, 9.363379034771805109, -116.3437500020483810 ) ) ;
#3931 = CARTESIAN_POINT ( 'NONE',  ( 4.999999999999992006, -8.660254037844389075, -193.1250000040967905 ) ) ;
#3932 = CARTESIAN_POINT ( 'NONE',  ( -10.81189881249999907, -6.242252689847864744, -125.1562500020483810 ) ) ;
#3933 = CARTESIAN_POINT ( 'NONE',  ( 7.644554776091147741E-16, 12.48450537969573659, -9.968750002048363257 ) ) ;
#3935 = EDGE_CURVE ( 'NONE', #26035, #1967, #2860, .T. ) ;
#3934 = CARTESIAN_POINT ( 'NONE',  ( 5.405949406249992428, -9.363379034771808662, -138.0937500020483810 ) ) ;
#3936 = CARTESIAN_POINT ( 'NONE',  ( 5.000000000000000000, 8.660254037844385522, -5.125000004096769146 ) ) ;
#3937 = CARTESIAN_POINT ( 'NONE',  ( 5.000000000000000000, 8.660254037844385522, -151.7500000000000000 ) ) ;
#3938 = CARTESIAN_POINT ( 'NONE',  ( 5.000000000000000000, 8.660254037844385522, -24.24999999999996447 ) ) ;
#3939 = CARTESIAN_POINT ( 'NONE',  ( -10.81189881249999729, 6.242252689847871849, -86.21875000204836681 ) ) ;
#3940 = CARTESIAN_POINT ( 'NONE',  ( 10.81189881249999907, 6.242252689847868297, -64.21875000204838102 ) ) ;
#3941 = CARTESIAN_POINT ( 'NONE',  ( -5.405949406249996869, 9.363379034771805109, -40.03125000204838102 ) ) ;
#3942 = CARTESIAN_POINT ( 'NONE',  ( 5.405949406249999534, 9.363379034771803333, -50.59375000204835260 ) ) ;
#3943 = LINE ( 'NONE', #17507, #22667 ) ;
#3944 = CARTESIAN_POINT ( 'NONE',  ( 10.81189881249999551, -6.242252689847874514, -152.9687500020484094 ) ) ;
#3945 = CARTESIAN_POINT ( 'NONE',  ( -4.999999999999996447, 8.660254037844387298, -127.5000000000000000 ) ) ;
#3946 = CARTESIAN_POINT ( 'NONE',  ( 5.405949406249992428, -9.363379034771808662, -139.7812500020483810 ) ) ;
#3947 = CARTESIAN_POINT ( 'NONE',  ( 10.00000000000025402, -5.773502691896113426, -187.0000000040967905 ) ) ;
#3948 = CARTESIAN_POINT ( 'NONE',  ( -10.00000000000000000, -5.773502691896251982, -85.12499999999997158 ) ) ;
#3949 = CARTESIAN_POINT ( 'NONE',  ( 10.81189881249999551, -6.242252689847874514, -18.15625000204837036 ) ) ;
#3950 = VERTEX_POINT ( 'NONE', #26157 ) ;
#3951 = CARTESIAN_POINT ( 'NONE',  ( -2.293366432827344421E-15, -12.48450537969573659, -109.9062500020483810 ) ) ;
#3952 = CARTESIAN_POINT ( 'NONE',  ( 9.999999999999996447, -5.773502691896262640, -133.0000000040967905 ) ) ;
#3953 = CARTESIAN_POINT ( 'NONE',  ( 7.070501591499376803E-16, 11.54700538379251284, -39.12499999999995737 ) ) ;
#3954 = CARTESIAN_POINT ( 'NONE',  ( -5.000000000000003553, -8.660254037844383745, -38.87500000409676915 ) ) ;
#3955 = CARTESIAN_POINT ( 'NONE',  ( -5.000000000000003553, -8.660254037844383745, -58.37500000409676204 ) ) ;
#3956 = CARTESIAN_POINT ( 'NONE',  ( -5.405949406249996869, 9.363379034771805109, -52.03125000204835970 ) ) ;
#3957 = CARTESIAN_POINT ( 'NONE',  ( 7.070501591499376803E-16, 11.54700538379251284, -147.1250000000000000 ) ) ;
#3958 = CARTESIAN_POINT ( 'NONE',  ( 5.405949406249992428, -9.363379034771808662, -150.2812500020483810 ) ) ;
#3959 = CARTESIAN_POINT ( 'NONE',  ( 10.81189881249999729, 0.000000000000000000, -133.3437500020484094 ) ) ;
#3960 = CARTESIAN_POINT ( 'NONE',  ( 10.00000000000051159, -5.773502691895965988, -115.0000000040967905 ) ) ;
#3961 = ORIENTED_EDGE ( 'NONE', *, *, #22665, .T. ) ;
#3962 = DIRECTION ( 'NONE',  ( 1.000000000000000000, 0.000000000000000000, 0.000000000000000000 ) ) ;
#3963 =( BOUNDED_CURVE ( )  B_SPLINE_CURVE ( 2, ( #11981, #5308, #1870, #14996, #28195, #41328, #24967 ),
 .UNSPECIFIED., .F., .F. ) 
 B_SPLINE_CURVE_WITH_KNOTS ( ( 3, 2, 2, 3 ),
 ( 0.4328358208955225273, 0.4340796019900499125, 0.4353233830845772978, 0.4365671641791046276 ),
 .UNSPECIFIED. ) 
 CURVE ( )  GEOMETRIC_REPRESENTATION_ITEM ( )  RATIONAL_B_SPLINE_CURVE ( ( 0.9999999999999820144, 0.8660254037844566932, 1.000000000000000000, 0.8660254037844387076, 1.000000000000000000, 0.8660254037844207220, 1.000000000000017986 ) ) 
 REPRESENTATION_ITEM ( '' )  );
#3965 = ORIENTED_EDGE ( 'NONE', *, *, #14049, .F. ) ;
#3964 = CARTESIAN_POINT ( 'NONE',  ( -10.81189881249999907, -6.242252689847864744, -63.65625000204836681 ) ) ;
#3966 = PERSON_AND_ORGANIZATION ( #11915, #17965 ) ;
#3967 = VECTOR ( 'NONE', #4032, 1000.000000000000000 ) ;
#3969 = VERTEX_POINT ( 'NONE', #6724 ) ;
#3968 = CARTESIAN_POINT ( 'NONE',  ( 10.81189881249999907, 6.242252689847868297, -112.2187500020483810 ) ) ;
#3970 = CARTESIAN_POINT ( 'NONE',  ( 5.405949406249999534, 9.363379034771803333, -19.09375000204835260 ) ) ;
#3971 = CARTESIAN_POINT ( 'NONE',  ( -5.405949406250003975, -9.363379034771801557, -190.8437500020484094 ) ) ;
#3972 = CARTESIAN_POINT ( 'NONE',  ( -2.293366432827344421E-15, -12.48450537969573659, -49.71875000204835970 ) ) ;
#3973 = CARTESIAN_POINT ( 'NONE',  ( 8.069781934609757457, -7.195427280628551969, 1.661355961043940754E-14 ) ) ;
#3974 = CARTESIAN_POINT ( 'NONE',  ( 9.999999999998969713, 5.773502691896851502, -0.3749999999999439892 ) ) ;
#3975 = CARTESIAN_POINT ( 'NONE',  ( -5.405949406250003975, -9.363379034771801557, -181.8437500020483810 ) ) ;
#3976 = CARTESIAN_POINT ( 'NONE',  ( 5.405949406249992428, -9.363379034771808662, -160.5937500020484094 ) ) ;
#3977 = CARTESIAN_POINT ( 'NONE',  ( 5.405949406249992428, -9.363379034771808662, -144.0937500020483810 ) ) ;
#3978 = CARTESIAN_POINT ( 'NONE',  ( -5.405949406249996869, 9.363379034771805109, -159.8437500020484094 ) ) ;
#3979 = CARTESIAN_POINT ( 'NONE',  ( -9.999999999999998224, 1.224646799147353059E-15, -128.7499999999999716 ) ) ;
#3980 = CARTESIAN_POINT ( 'NONE',  ( 10.00000000000000000, 5.773502691896255534, -178.8750000000000000 ) ) ;
#3981 = CARTESIAN_POINT ( 'NONE',  ( -2.293366432827344421E-15, -12.48450537969573659, -85.71875000204838102 ) ) ;
#3982 = CARTESIAN_POINT ( 'NONE',  ( 10.81189881249999907, 6.242252689847868297, -67.40625000204839523 ) ) ;
#3983 = FACE_OUTER_BOUND ( 'NONE', #8521, .T. ) ;
#3984 = ADVANCED_FACE ( 'NONE', ( #42327 ), #33062, .T. ) ;
#3985 = CARTESIAN_POINT ( 'NONE',  ( -10.81189881249999729, 6.242252689847871849, -185.2187500020483810 ) ) ;
#3986 = CARTESIAN_POINT ( 'NONE',  ( 5.405949406249999534, 9.363379034771803333, -125.7812500020483668 ) ) ;
#3987 = CARTESIAN_POINT ( 'NONE',  ( -10.81189881249999729, -6.242252689847864744, -165.6562500020483810 ) ) ;
#3988 = CARTESIAN_POINT ( 'NONE',  ( -5.405949406249996869, 9.363379034771805109, -49.03125000204838813 ) ) ;
#3989 = CARTESIAN_POINT ( 'NONE',  ( 9.999999999999998224, 0.000000000000000000, -137.3750000040967905 ) ) ;
#3990 = CARTESIAN_POINT ( 'NONE',  ( -4.999999999999996447, 8.660254037844387298, -106.4999999999999858 ) ) ;
#3991 = ORIENTED_EDGE ( 'NONE', *, *, #36775, .F. ) ;
#3992 = CARTESIAN_POINT ( 'NONE',  ( 10.81189881249999729, 0.000000000000000000, -130.5312500020484094 ) ) ;
#3993 = CARTESIAN_POINT ( 'NONE',  ( -10.81189881249999907, -6.242252689847864744, -149.1562500020483810 ) ) ;
#3994 = CARTESIAN_POINT ( 'NONE',  ( 10.81189881249999729, 0.000000000000000000, -190.5312500020484094 ) ) ;
#3995 = CARTESIAN_POINT ( 'NONE',  ( 7.644554776091147741E-16, 12.48450537969573659, -78.96875000204839523 ) ) ;
#3996 = VECTOR ( 'NONE', #6789, 1000.000000000000000 ) ;
#3997 = ORIENTED_EDGE ( 'NONE', *, *, #41197, .F. ) ;
#3998 = CARTESIAN_POINT ( 'NONE',  ( 7.070501591499377789E-16, 11.54700538379251284, -51.12499999999998579 ) ) ;
#3999 = CARTESIAN_POINT ( 'NONE',  ( 5.405949406249992428, -9.363379034771808662, -180.0937500020484094 ) ) ;
#4000 = CARTESIAN_POINT ( 'NONE',  ( -4.999999999999996447, 8.660254037844387298, -63.37500000409676204 ) ) ;
#4001 = VECTOR ( 'NONE', #14838, 1000.000000000000000 ) ;
#4002 = DIRECTION ( 'NONE',  ( -0.000000000000000000, -0.000000000000000000, 1.000000000000000000 ) ) ;
#4003 = CARTESIAN_POINT ( 'NONE',  ( -10.81189881249999729, 6.242252689847871849, -78.90625000204838102 ) ) ;
#4004 = CARTESIAN_POINT ( 'NONE',  ( 10.81189881249999729, 6.242252689847867408, -58.40625000204838102 ) ) ;
#4005 = CARTESIAN_POINT ( 'NONE',  ( -9.999999999999998224, 1.224646799147353059E-15, -49.62500000409675494 ) ) ;
#4006 = CARTESIAN_POINT ( 'NONE',  ( -5.405949406249996869, 9.363379034771805109, -12.84375000204834905 ) ) ;
#4007 = CARTESIAN_POINT ( 'NONE',  ( 0.000000000000000000, 0.000000000000000000, -99.99999999999998579 ) ) ;
#4008 = CARTESIAN_POINT ( 'NONE',  ( 7.644554776091147741E-16, 12.48450537969573659, -188.6562500020484379 ) ) ;
#4009 = CARTESIAN_POINT ( 'NONE',  ( -2.293366432827344421E-15, -12.48450537969573659, -6.406250002048363257 ) ) ;
#4010 = LINE ( 'NONE', #23874, #23559 ) ;
#4011 = CARTESIAN_POINT ( 'NONE',  ( 8.660254119780192994, -4.999999858083012505, -99.99999999999998579 ) ) ;
#4012 = CARTESIAN_POINT ( 'NONE',  ( 10.00000000000102318, -5.773502691895667560, -89.12499999999994316 ) ) ;
#4013 = DIRECTION ( 'NONE',  ( 1.000000000000000000, 0.000000000000000000, 0.000000000000000000 ) ) ;
#4014 = CARTESIAN_POINT ( 'NONE',  ( 4.999999999999992006, -8.660254037844389075, -122.2500000000000000 ) ) ;
#4016 = ORIENTED_EDGE ( 'NONE', *, *, #38610, .F. ) ;
#4015 = CARTESIAN_POINT ( 'NONE',  ( -5.405949406250003975, -9.363379034771801557, -89.03125000204838102 ) ) ;
#4018 = ORIENTED_EDGE ( 'NONE', *, *, #16822, .T. ) ;
#4017 = DIRECTION ( 'NONE',  ( -0.000000000000000000, -0.000000000000000000, -1.000000000000000000 ) ) ;
#4019 = ORIENTED_EDGE ( 'NONE', *, *, #11969, .F. ) ;
#4020 = CARTESIAN_POINT ( 'NONE',  ( -5.405949406250003975, -9.363379034771801557, -28.84375000204836326 ) ) ;
#4021 = CARTESIAN_POINT ( 'NONE',  ( 5.405949406249992428, -9.363379034771808662, -24.28125000204836681 ) ) ;
#4022 = CALENDAR_DATE ( 2026, 28, 9 ) ;
#4023 = CARTESIAN_POINT ( 'NONE',  ( 10.81189881249999551, -6.242252689847874514, -71.96875000204838102 ) ) ;
#4024 = DIRECTION ( 'NONE',  ( 1.000000000000000000, 0.000000000000000000, 0.000000000000000000 ) ) ;
#4025 = CARTESIAN_POINT ( 'NONE',  ( -2.121150477449813534E-15, -11.54700538379251284, -47.37499999999997868 ) ) ;
#4026 = CARTESIAN_POINT ( 'NONE',  ( 10.81189881249999729, 0.000000000000000000, -182.8437500020483810 ) ) ;
#4027 = CARTESIAN_POINT ( 'NONE',  ( -5.405949406249996869, 9.363379034771805109, -152.3437500020483810 ) ) ;
#4028 = CARTESIAN_POINT ( 'NONE',  ( 10.81189881249999729, 0.000000000000000000, -1.343750002048366143 ) ) ;
#4029 = CARTESIAN_POINT ( 'NONE',  ( -9.999999999999998224, 1.224646799147353059E-15, -200.0000000000000000 ) ) ;
#4030 = CARTESIAN_POINT ( 'NONE',  ( -9.999999999999998224, 1.224646799147353059E-15, -200.0000000000000000 ) ) ;
#4031 = CARTESIAN_POINT ( 'NONE',  ( -9.999999999999998224, 5.773502691896259087, -6.250000004096741613 ) ) ;
#4032 = DIRECTION ( 'NONE',  ( -0.000000000000000000, -0.000000000000000000, 1.000000000000000000 ) ) ;
#4033 = CARTESIAN_POINT ( 'NONE',  ( 5.405949406249999534, 9.363379034771803333, -119.5937500020483810 ) ) ;
#4034 = CARTESIAN_POINT ( 'NONE',  ( -10.00000000000025580, 5.773502691896109873, -160.7500000040967620 ) ) ;
#4035 = CARTESIAN_POINT ( 'NONE',  ( 10.81189881249999907, 6.242252689847868297, -86.90625000204836681 ) ) ;
#4036 = EDGE_CURVE ( 'NONE', #1094, #2019, #33435, .T. ) ;
#4037 = CARTESIAN_POINT ( 'NONE',  ( 10.81189881249999729, 6.242252689847867408, -103.2187500020483810 ) ) ;
#4038 = CARTESIAN_POINT ( 'NONE',  ( -10.81189881249999729, 6.242252689847871849, -71.21875000204839523 ) ) ;
#4039 = EDGE_CURVE ( 'NONE', #318, #26657, #20170, .T. ) ;
#4040 = CARTESIAN_POINT ( 'NONE',  ( -10.81189881249999729, 1.324075727343319199E-15, -72.78125000204838102 ) ) ;
#4041 = CARTESIAN_POINT ( 'NONE',  ( 7.070501591499377789E-16, 11.54700538379251284, -162.5000000040967905 ) ) ;
#4042 = EDGE_CURVE ( 'NONE', #6810, #30574, #37832, .T. ) ;
#4043 = CARTESIAN_POINT ( 'NONE',  ( 7.644554776091147741E-16, 12.48450537969573659, -155.6562500020483810 ) ) ;
#4044 = CARTESIAN_POINT ( 'NONE',  ( -2.293366432827344421E-15, -12.48450537969573659, -175.9062500020483810 ) ) ;
#4045 = CARTESIAN_POINT ( 'NONE',  ( 5.405949406249992428, -9.363379034771808662, -0.09375000204836503315 ) ) ;
#4046 = CARTESIAN_POINT ( 'NONE',  ( 0.000000000000000000, 0.000000000000000000, -99.99999999999998579 ) ) ;
#4047 = CARTESIAN_POINT ( 'NONE',  ( 5.405949406249992428, -9.363379034771808662, -109.5937500020483810 ) ) ;
#4048 = CARTESIAN_POINT ( 'NONE',  ( 9.999999999999612754, 5.773502691896477579, -156.3750000000000000 ) ) ;
#4049 = CARTESIAN_POINT ( 'NONE',  ( -5.000000000000003553, -8.660254037844383745, -75.99999999999998579 ) ) ;
#4050 = CARTESIAN_POINT ( 'NONE',  ( 10.81189881249999907, 6.242252689847868297, -2.906250002048360592 ) ) ;
#4051 = CARTESIAN_POINT ( 'NONE',  ( -2.121150477449813534E-15, -11.54700538379251284, -91.25000000409677625 ) ) ;
#4052 = CARTESIAN_POINT ( 'NONE',  ( -9.999999999999998224, 1.224646799147353059E-15, -96.12500000409677625 ) ) ;
#4053 = CC_DESIGN_PERSON_AND_ORGANIZATION_ASSIGNMENT ( #18777, #36034, ( #21848 ) ) ;
#4054 = CARTESIAN_POINT ( 'NONE',  ( 10.81189881249999551, -6.242252689847874514, -102.1562500020483952 ) ) ;
#4055 = CARTESIAN_POINT ( 'NONE',  ( -5.405949406250003975, -9.363379034771801557, -83.03125000204838102 ) ) ;
#4056 = CARTESIAN_POINT ( 'NONE',  ( 7.070501591499377789E-16, 11.54700538379251284, -80.00000000409679046 ) ) ;
#4057 = CARTESIAN_POINT ( 'NONE',  ( -4.999999999999996447, 8.660254037844387298, -20.99999999999996447 ) ) ;
#4058 = CARTESIAN_POINT ( 'NONE',  ( -5.405949406249996869, 9.363379034771805109, -35.34375000204836681 ) ) ;
#4059 = ORIENTED_EDGE ( 'NONE', *, *, #26989, .T. ) ;
#4060 = CARTESIAN_POINT ( 'NONE',  ( -10.00000000000000000, -5.773502691896251982, -8.624999999999976907 ) ) ;
#4061 = CARTESIAN_POINT ( 'NONE',  ( 5.405949406249992428, -9.363379034771808662, -30.28125000204837036 ) ) ;
#4062 = CARTESIAN_POINT ( 'NONE',  ( -2.121150477449813534E-15, -11.54700538379251284, -143.3750000000000000 ) ) ;
#4063 = CARTESIAN_POINT ( 'NONE',  ( -9.999999999999998224, 1.224646799147353059E-15, -45.12500000409677625 ) ) ;
#4064 = EDGE_CURVE ( 'NONE', #35407, #13549, #40830, .T. ) ;
#4065 = CARTESIAN_POINT ( 'NONE',  ( -9.999999999999998224, 5.773502691896259087, -1.750000004096752271 ) ) ;
#4066 = CARTESIAN_POINT ( 'NONE',  ( -10.81189881249999729, 6.242252689847871849, -135.9062500020484094 ) ) ;
#4067 = ADVANCED_FACE ( 'NONE', ( #29607 ), #6936, .F. ) ;
#4068 = CARTESIAN_POINT ( 'NONE',  ( -9.999999999999998224, 1.224646799147353059E-15, -188.7500000000000000 ) ) ;
#4069 = CARTESIAN_POINT ( 'NONE',  ( 4.999999999999992006, -8.660254037844389075, -184.1250000040967905 ) ) ;
#4070 = VECTOR ( 'NONE', #12003, 1000.000000000000000 ) ;
#4072 = ORIENTED_EDGE ( 'NONE', *, *, #37286, .T. ) ;
#4071 = CARTESIAN_POINT ( 'NONE',  ( 5.405949406249999534, 9.363379034771803333, -116.7812500020483952 ) ) ;
#4073 = CARTESIAN_POINT ( 'NONE',  ( -9.999999999999998224, 1.224646799147353059E-15, -13.24999999999995559 ) ) ;
#4074 = ORIENTED_EDGE ( 'NONE', *, *, #12921, .F. ) ;
#4075 = EDGE_LOOP ( 'NONE', ( #23803, #42412, #28178, #952 ) ) ;
#4076 = AXIS2_PLACEMENT_3D ( 'NONE', #21825, #35005, #15335 ) ;
#4077 = CARTESIAN_POINT ( 'NONE',  ( 10.81189881249999907, 6.242252689847868297, -46.40625000204835970 ) ) ;
#4078 = CALENDAR_DATE ( 2026, 28, 9 ) ;
#4079 = CARTESIAN_POINT ( 'NONE',  ( 10.81189881249999551, -6.242252689847874514, -97.46875000204838102 ) ) ;
#4080 = CARTESIAN_POINT ( 'NONE',  ( -10.81189881249999729, -6.242252689847864744, -126.6562500020483810 ) ) ;
#4081 = ORIENTED_EDGE ( 'NONE', *, *, #7202, .F. ) ;
#4082 = EDGE_CURVE ( 'NONE', #10102, #41485, #6612, .T. ) ;
#4083 = CARTESIAN_POINT ( 'NONE',  ( 7.070501591499376803E-16, 11.54700538379251284, -51.50000000409676204 ) ) ;
#4084 = CARTESIAN_POINT ( 'NONE',  ( -2.293366432827344421E-15, -12.48450537969573659, -196.7187500020484094 ) ) ;
#4085 =( BOUNDED_CURVE ( )  B_SPLINE_CURVE ( 2, ( #10896, #20829, #24089, #17796, #40880, #21258, #4864 ),
 .UNSPECIFIED., .F., .F. ) 
 B_SPLINE_CURVE_WITH_KNOTS ( ( 3, 2, 2, 3 ),
 ( 0.2985074626865671932, 0.2997512437810946340, 0.3009950248756220192, 0.3022388059701494045 ),
 .UNSPECIFIED. ) 
 CURVE ( )  GEOMETRIC_REPRESENTATION_ITEM ( )  RATIONAL_B_SPLINE_CURVE ( ( 0.9999999999999940048, 0.8660254037844447028, 1.000000000000000000, 0.8660254037844387076, 1.000000000000000000, 0.8660254037844207220, 1.000000000000017986 ) ) 
 REPRESENTATION_ITEM ( '' )  );
#4086 = CARTESIAN_POINT ( 'NONE',  ( 7.644554776091147741E-16, 12.48450537969573659, -175.1562500020484094 ) ) ;
#4087 = FACE_OUTER_BOUND ( 'NONE', #33392, .T. ) ;
#4088 = CARTESIAN_POINT ( 'NONE',  ( 7.644554776091147741E-16, 12.48450537969573659, -126.9687500020483952 ) ) ;
#4089 = CARTESIAN_POINT ( 'NONE',  ( 10.81189881249999729, 0.000000000000000000, -94.34375000204838102 ) ) ;
#4090 = CARTESIAN_POINT ( 'NONE',  ( 10.81189881249999551, -6.242252689847874514, -102.1562500020483952 ) ) ;
#4091 = CARTESIAN_POINT ( 'NONE',  ( 9.999999999999996447, -5.773502691896262640, -185.5000000040967905 ) ) ;
#4092 = CARTESIAN_POINT ( 'NONE',  ( -5.405949406249996869, 9.363379034771805109, -108.8437500020483810 ) ) ;
#4093 = CARTESIAN_POINT ( 'NONE',  ( 7.644554776091147741E-16, 12.48450537969573659, -178.1562500020484094 ) ) ;
#4094 = CARTESIAN_POINT ( 'NONE',  ( -5.000000000000003553, -8.660254037844383745, -104.8750000040967763 ) ) ;
#4095 = CARTESIAN_POINT ( 'NONE',  ( -4.999999999999996447, 8.660254037844387298, -121.8750000040967905 ) ) ;
#4096 = CARTESIAN_POINT ( 'NONE',  ( 10.81189881249999551, -6.242252689847874514, -193.6562500020484379 ) ) ;
#4097 = CARTESIAN_POINT ( 'NONE',  ( 10.81189881249999729, 0.000000000000000000, -62.84375000204836681 ) ) ;
#4098 = VECTOR ( 'NONE', #18235, 1000.000000000000000 ) ;
#4099 = CARTESIAN_POINT ( 'NONE',  ( 10.81189881249999907, 6.242252689847868297, -38.71875000204835260 ) ) ;
#4100 = CARTESIAN_POINT ( 'NONE',  ( 4.999999999999992006, -8.660254037844389075, -173.6250000040968189 ) ) ;
#4101 = CARTESIAN_POINT ( 'NONE',  ( -2.293366432827344421E-15, -12.48450537969573659, -13.90625000204836503 ) ) ;
#4102 = CARTESIAN_POINT ( 'NONE',  ( -10.81189881249999729, 1.324075727343319199E-15, -23.09375000204835615 ) ) ;
#4103 = LINE ( 'NONE', #26558, #25431 ) ;
#4104 = CARTESIAN_POINT ( 'NONE',  ( 5.405949406249992428, -9.363379034771808662, -130.5937500020483810 ) ) ;
#4105 = CARTESIAN_POINT ( 'NONE',  ( 10.00000000000000000, 5.773502691896255534, -105.3749999999999858 ) ) ;
#4106 = CARTESIAN_POINT ( 'NONE',  ( -2.293366432827344421E-15, -12.48450537969573659, -28.90625000204835615 ) ) ;
#4107 = CARTESIAN_POINT ( 'NONE',  ( -5.321294541346989426, -5.321294541346989426, -220.0000000000000000 ) ) ;
#4108 = CARTESIAN_POINT ( 'NONE',  ( 9.999999999999998224, 0.000000000000000000, -57.49999999999996447 ) ) ;
#4109 = CARTESIAN_POINT ( 'NONE',  ( 5.405949406249992428, -9.363379034771808662, -127.7812500020483810 ) ) ;
#4110 = CARTESIAN_POINT ( 'NONE',  ( 10.81189881249999729, 6.242252689847867408, -106.4062500020483952 ) ) ;
#4111 = ORIENTED_EDGE ( 'NONE', *, *, #18175, .F. ) ;
#4112 = VECTOR ( 'NONE', #39758, 1000.000000000000000 ) ;
#4113 = CARTESIAN_POINT ( 'NONE',  ( -9.999999999998456346, -5.773502691897145489, -12.00000000409673184 ) ) ;
#4114 = CARTESIAN_POINT ( 'NONE',  ( -10.00000000000000000, -5.773502691896251982, -102.0000000040967905 ) ) ;
#4115 = CARTESIAN_POINT ( 'NONE',  ( -9.999999999999998224, 1.224646799147353059E-15, -195.1250000040967905 ) ) ;
#4116 = CARTESIAN_POINT ( 'NONE',  ( 10.81189881249999907, 6.242252689847868297, -61.21875000204836681 ) ) ;
#4117 = ORIENTED_EDGE ( 'NONE', *, *, #17760, .F. ) ;
#4118 = CARTESIAN_POINT ( 'NONE',  ( -9.999999999999998224, 1.224646799147353059E-15, -34.24999999999997158 ) ) ;
#4119 = EDGE_CURVE ( 'NONE', #36081, #32882, #42477, .T. ) ;
#4120 = CARTESIAN_POINT ( 'NONE',  ( -10.81189881249999729, -6.242252689847864744, -36.65625000204835970 ) ) ;
#4121 = CARTESIAN_POINT ( 'NONE',  ( -9.999999999999998224, 1.224646799147353059E-15, -91.24999999999998579 ) ) ;
#4122 = CARTESIAN_POINT ( 'NONE',  ( 9.999999999999998224, 0.000000000000000000, -26.37500000409676204 ) ) ;
#4123 = CARTESIAN_POINT ( 'NONE',  ( 10.81189881249999551, -6.242252689847874514, -139.6562500020484094 ) ) ;
#4124 = DIRECTION ( 'NONE',  ( -1.000000000000000000, 0.000000000000000000, 0.000000000000000000 ) ) ;
#4125 = ORIENTED_EDGE ( 'NONE', *, *, #4837, .T. ) ;
#4126 = VECTOR ( 'NONE', #34449, 1000.000000000000000 ) ;
#4127 = ORIENTED_EDGE ( 'NONE', *, *, #26163, .T. ) ;
#4128 = DIRECTION ( 'NONE',  ( 1.000000000000000000, 0.000000000000000000, 0.000000000000000000 ) ) ;
#4129 = FACE_OUTER_BOUND ( 'NONE', #33448, .T. ) ;
#4130 = CARTESIAN_POINT ( 'NONE',  ( 10.81189881249999729, 0.000000000000000000, -169.3437500020484094 ) ) ;
#4131 = CARTESIAN_POINT ( 'NONE',  ( 10.81189881249999907, 6.242252689847868297, -197.9062500020484379 ) ) ;
#4132 = CARTESIAN_POINT ( 'NONE',  ( 10.81189881249999729, 0.000000000000000000, -17.84375000204835260 ) ) ;
#4133 = DIRECTION ( 'NONE',  ( 0.4999999999999998335, 0.8660254037844387076, 0.000000000000000000 ) ) ;
#4134 = CARTESIAN_POINT ( 'NONE',  ( -10.81189881249999729, 6.242252689847871849, -144.7187500020484094 ) ) ;
#4135 = CARTESIAN_POINT ( 'NONE',  ( 10.81189881249999551, -6.242252689847874514, -137.9687500020483810 ) ) ;
#4136 = CARTESIAN_POINT ( 'NONE',  ( 5.405949406249999534, 9.363379034771803333, -103.2812500020483952 ) ) ;
#4137 = CARTESIAN_POINT ( 'NONE',  ( 10.81189881249999907, 6.242252689847868297, -118.2187500020483810 ) ) ;
#4138 = CARTESIAN_POINT ( 'NONE',  ( 5.000000000000000000, 8.660254037844385522, -192.6250000040967905 ) ) ;
#4139 = CARTESIAN_POINT ( 'NONE',  ( 10.81189881249999729, 0.000000000000000000, -121.5312500020483952 ) ) ;
#4140 = CARTESIAN_POINT ( 'NONE',  ( 10.81189881249999729, 0.000000000000000000, -7.343750002048343717 ) ) ;
#4141 = CARTESIAN_POINT ( 'NONE',  ( 5.405949406249999534, 9.363379034771803333, -133.0937500020483810 ) ) ;
#4142 = CARTESIAN_POINT ( 'NONE',  ( -9.999999999999998224, 1.224646799147353059E-15, -166.6250000040967905 ) ) ;
#4143 = CARTESIAN_POINT ( 'NONE',  ( -2.121150477449813534E-15, -11.54700538379251284, -96.87500000000000000 ) ) ;
#4144 = CARTESIAN_POINT ( 'NONE',  ( 5.000000000000000000, 8.660254037844385522, -153.2500000000000000 ) ) ;
#4145 = CARTESIAN_POINT ( 'NONE',  ( 10.00000000000000000, 5.773502691896255534, -21.37499999999997868 ) ) ;
#4146 = CARTESIAN_POINT ( 'NONE',  ( 10.81189881249999729, 0.000000000000000000, -80.84375000204838102 ) ) ;
#4147 = CARTESIAN_POINT ( 'NONE',  ( -10.81189881249999907, -6.242252689847864744, -63.46875000204838102 ) ) ;
#4148 = CARTESIAN_POINT ( 'NONE',  ( 0.000000000000000000, 0.000000000000000000, -220.0000000000000000 ) ) ;
#4149 = CARTESIAN_POINT ( 'NONE',  ( -2.293366432827344421E-15, -12.48450537969573659, -39.40625000204835260 ) ) ;
#4150 = CARTESIAN_POINT ( 'NONE',  ( -2.293366432827344421E-15, -12.48450537969573659, -46.71875000204835970 ) ) ;
#4151 = CARTESIAN_POINT ( 'NONE',  ( -9.999999999999479527, -5.773502691896549521, -142.1249999999999716 ) ) ;
#4152 = CARTESIAN_POINT ( 'NONE',  ( -5.405949406249996869, 9.363379034771805109, -153.8437500020483810 ) ) ;
#4153 = CARTESIAN_POINT ( 'NONE',  ( -9.999999999999998224, 5.773502691896259087, -133.3750000000000000 ) ) ;
#4154 = CARTESIAN_POINT ( 'NONE',  ( -2.293366432827344421E-15, -12.48450537969573659, -133.9062500020483810 ) ) ;
#4155 = CARTESIAN_POINT ( 'NONE',  ( 7.070501591499377789E-16, 11.54700538379251284, -84.12499999999997158 ) ) ;
#4156 = CARTESIAN_POINT ( 'NONE',  ( -10.81189881249999729, 1.324075727343319199E-15, -17.28125000204835970 ) ) ;
#4157 = VERTEX_POINT ( 'NONE', #42538 ) ;
#4158 = CARTESIAN_POINT ( 'NONE',  ( 10.81189881249999729, 0.000000000000000000, -114.0312500020483952 ) ) ;
#4159 = CARTESIAN_POINT ( 'NONE',  ( -9.999999999999998224, 1.224646799147353059E-15, -127.6250000040967620 ) ) ;
#4160 = CARTESIAN_POINT ( 'NONE',  ( -5.000000000000003553, -8.660254037844383745, -111.9999999999999858 ) ) ;
#4161 = ADVANCED_FACE ( 'NONE', ( #12961 ), #39308, .T. ) ;
#4162 = CARTESIAN_POINT ( 'NONE',  ( -10.00000000000000000, -5.773502691896251982, -36.00000000409675494 ) ) ;
#4163 = CARTESIAN_POINT ( 'NONE',  ( 9.999999999999998224, 0.000000000000000000, -57.87500000409676204 ) ) ;
#4164 = CARTESIAN_POINT ( 'NONE',  ( -5.405949406249996869, 9.363379034771805109, -53.53125000204836681 ) ) ;
#4165 = CARTESIAN_POINT ( 'NONE',  ( -4.999999999999996447, 8.660254037844387298, -147.0000000000000000 ) ) ;
#4166 = CARTESIAN_POINT ( 'NONE',  ( 5.405949406249992428, -9.363379034771808662, -154.7812500020484094 ) ) ;
#4167 = CARTESIAN_POINT ( 'NONE',  ( -5.405949406249996869, 9.363379034771805109, -132.8437500020484094 ) ) ;
#4168 = CARTESIAN_POINT ( 'NONE',  ( -10.00000000000051337, 5.773502691895962435, -109.3749999999999858 ) ) ;
#4169 = ORIENTED_EDGE ( 'NONE', *, *, #4814, .F. ) ;
#4170 =( BOUNDED_CURVE ( )  B_SPLINE_CURVE ( 2, ( #24476, #28942, #22035, #15951, #11493, #42287, #22452 ),
 .UNSPECIFIED., .F., .F. ) 
 B_SPLINE_CURVE_WITH_KNOTS ( ( 3, 2, 2, 3 ),
 ( 0.3320895522388061516, 0.3333333333333334259, 0.3345771144278607556, 0.3358208955223880854 ),
 .UNSPECIFIED. ) 
 CURVE ( )  GEOMETRIC_REPRESENTATION_ITEM ( )  RATIONAL_B_SPLINE_CURVE ( ( 0.9999999999999820144, 0.8660254037844566932, 1.000000000000000000, 0.8660254037844387076, 1.000000000000000000, 0.8660254037844387076, 1.000000000000000000 ) ) 
 REPRESENTATION_ITEM ( '' )  );
#4171 = CARTESIAN_POINT ( 'NONE',  ( 5.000000000000000000, 8.660254037844385522, -22.74999999999996447 ) ) ;
#4173 = EDGE_CURVE ( 'NONE', #35132, #24959, #17640, .T. ) ;
#4172 = VERTEX_POINT ( 'NONE', #30883 ) ;
#4174 = ORIENTED_EDGE ( 'NONE', *, *, #41905, .T. ) ;
#4175 = APPROVAL_ROLE ( '' ) ;
#4177 = ORIENTED_EDGE ( 'NONE', *, *, #34029, .T. ) ;
#4176 = CARTESIAN_POINT ( 'NONE',  ( 7.644554776091147741E-16, 12.48450537969573659, -113.4687500020483952 ) ) ;
#4178 = LINE ( 'NONE', #14722, #5179 ) ;
#4179 = CARTESIAN_POINT ( 'NONE',  ( -5.405949406250003975, -9.363379034771801557, -192.3437500020484094 ) ) ;
#4180 = CARTESIAN_POINT ( 'NONE',  ( 10.81189881249999729, 0.000000000000000000, -35.84375000204836681 ) ) ;
#4181 = CARTESIAN_POINT ( 'NONE',  ( -9.999999999999998224, 1.224646799147353059E-15, -61.62500000409676204 ) ) ;
#4182 = CARTESIAN_POINT ( 'NONE',  ( -9.999999999999998224, 1.224646799147353059E-15, -151.6250000040967905 ) ) ;
#4183 = VECTOR ( 'NONE', #17096, 1000.000000000000000 ) ;
#4184 = CARTESIAN_POINT ( 'NONE',  ( -10.81189881249999729, -6.242252689847864744, -177.4687500020484094 ) ) ;
#4185 = CARTESIAN_POINT ( 'NONE',  ( -5.405949406250003975, -9.363379034771801557, -159.3437500020484094 ) ) ;
#4186 = CARTESIAN_POINT ( 'NONE',  ( 10.81189881249999729, 0.000000000000000000, -137.8437500020484094 ) ) ;
#4187 = CARTESIAN_POINT ( 'NONE',  ( 7.644554776091147741E-16, 12.48450537969573659, -158.4687500020483810 ) ) ;
#4188 = DIRECTION ( 'NONE',  ( 0.000000000000000000, 1.000000000000000000, 0.000000000000000000 ) ) ;
#4189 = DIRECTION ( 'NONE',  ( 0.08682659386424779191, -0.08682659386424779191, 0.9924325091389669673 ) ) ;
#4190 = CARTESIAN_POINT ( 'NONE',  ( 5.000000000000000000, 8.660254037844385522, -181.7500000000000000 ) ) ;
#4191 = CARTESIAN_POINT ( 'NONE',  ( -10.81189881249999907, -6.242252689847864744, -91.96875000204838102 ) ) ;
#4192 = CARTESIAN_POINT ( 'NONE',  ( 7.070501591499376803E-16, 11.54700538379251284, -151.6250000000000000 ) ) ;
#4193 = CARTESIAN_POINT ( 'NONE',  ( 5.405949406249992428, -9.363379034771808662, -64.78125000204838102 ) ) ;
#4194 = CARTESIAN_POINT ( 'NONE',  ( -5.000000000000003553, -8.660254037844383745, -97.37500000409677625 ) ) ;
#4195 = CARTESIAN_POINT ( 'NONE',  ( -5.405949406250003975, -9.363379034771801557, -177.3437500020483810 ) ) ;
#4196 = CARTESIAN_POINT ( 'NONE',  ( 5.405949406249999534, 9.363379034771803333, -121.2812500020483952 ) ) ;
#4197 = CARTESIAN_POINT ( 'NONE',  ( -5.405949406249996869, 9.363379034771805109, -151.0312500020483810 ) ) ;
#4198 = CARTESIAN_POINT ( 'NONE',  ( 5.405949406249992428, -9.363379034771808662, -52.78125000204836681 ) ) ;
#4199 = CARTESIAN_POINT ( 'NONE',  ( 10.00000000000000000, 5.773502691896255534, -129.7500000040967905 ) ) ;
#4200 = CARTESIAN_POINT ( 'NONE',  ( 7.070501591499377789E-16, 11.54700538379251284, -106.6249999999999716 ) ) ;
#4201 = ADVANCED_FACE ( 'NONE', ( #17479 ), #40565, .T. ) ;
#4202 = VERTEX_POINT ( 'NONE', #27001 ) ;
#4203 = CARTESIAN_POINT ( 'NONE',  ( -2.293366432827344421E-15, -12.48450537969573659, -138.4062500020484094 ) ) ;
#4204 = CARTESIAN_POINT ( 'NONE',  ( 9.999999999999996447, -5.773502691896262640, -158.5000000040968189 ) ) ;
#4205 = CARTESIAN_POINT ( 'NONE',  ( -2.293366432827344421E-15, -12.48450537969573659, -148.9062500020483810 ) ) ;
#4206 = CARTESIAN_POINT ( 'NONE',  ( -5.405949406250003975, -9.363379034771801557, -191.0312500020484094 ) ) ;
#4207 = CARTESIAN_POINT ( 'NONE',  ( -10.81189881249999729, 1.324075727343319199E-15, -84.59375000204836681 ) ) ;
#4208 = ORIENTED_EDGE ( 'NONE', *, *, #37566, .T. ) ;
#4209 = CARTESIAN_POINT ( 'NONE',  ( -5.000000000000003553, -8.660254037844383745, -47.49999999999998579 ) ) ;
#4210 = CARTESIAN_POINT ( 'NONE',  ( -10.81189881249999907, -6.242252689847864744, -180.4687500020484094 ) ) ;
#4211 = CARTESIAN_POINT ( 'NONE',  ( -10.00000000000000000, -5.773502691896251982, -66.00000000409679046 ) ) ;
#4212 = CARTESIAN_POINT ( 'NONE',  ( -9.999999999999998224, 1.224646799147353059E-15, -21.12500000409675494 ) ) ;
#4213 = CARTESIAN_POINT ( 'NONE',  ( 0.000000000000000000, 0.000000000000000000, -99.99999999999998579 ) ) ;
#4214 = CARTESIAN_POINT ( 'NONE',  ( -10.81189881249999907, -6.242252689847864744, -75.65625000204839523 ) ) ;
#4215 = CARTESIAN_POINT ( 'NONE',  ( -10.81189881249999729, -6.242252689847864744, -60.65625000204840234 ) ) ;
#4216 = AXIS2_PLACEMENT_3D ( 'NONE', #4380, #24029, #26828 ) ;
#4217 =( BOUNDED_CURVE ( )  B_SPLINE_CURVE ( 2, ( #8696, #14711, #27686, #15139, #34385, #11050, #28337 ),
 .UNSPECIFIED., .F., .F. ) 
 B_SPLINE_CURVE_WITH_KNOTS ( ( 3, 2, 2, 3 ),
 ( 0.6194029850746269883, 0.6206467661691543736, 0.6218905472636816478, 0.6231343283582090331 ),
 .UNSPECIFIED. ) 
 CURVE ( )  GEOMETRIC_REPRESENTATION_ITEM ( )  RATIONAL_B_SPLINE_CURVE ( ( 0.9999999999999880096, 0.8660254037844506980, 1.000000000000000000, 0.8660254037844387076, 1.000000000000000000, 0.8660254037844267172, 1.000000000000011990 ) ) 
 REPRESENTATION_ITEM ( '' )  );
#4218 = CARTESIAN_POINT ( 'NONE',  ( -5.000000000000003553, -8.660254037844383745, -50.87500000409675494 ) ) ;
#4219 = CARTESIAN_POINT ( 'NONE',  ( -10.81189881249999729, 1.324075727343319199E-15, -12.59375000204834905 ) ) ;
#4220 = CARTESIAN_POINT ( 'NONE',  ( -5.000000000000003553, -8.660254037844383745, -35.49999999999997868 ) ) ;
#4221 = CARTESIAN_POINT ( 'NONE',  ( -5.405949406249996869, 9.363379034771805109, -173.5312500020484094 ) ) ;
#4222 = APPROVAL_PERSON_ORGANIZATION ( #8445, #19877, #15318 ) ;
#4223 = CARTESIAN_POINT ( 'NONE',  ( -5.405949406250003975, -9.363379034771801557, -3.531250002048374803 ) ) ;
#4224 = CARTESIAN_POINT ( 'NONE',  ( 9.999999999999998224, 0.000000000000000000, -72.87500000409677625 ) ) ;
#4225 = CARTESIAN_POINT ( 'NONE',  ( -5.000000000000003553, -8.660254037844383745, -81.99999999999998579 ) ) ;
#4226 = CARTESIAN_POINT ( 'NONE',  ( -5.000000000000003553, -8.660254037844383745, -103.3750000040967763 ) ) ;
#4227 =( BOUNDED_CURVE ( )  B_SPLINE_CURVE ( 2, ( #11797, #8585, #25414, #38559, #34707, #25624, #28227 ),
 .UNSPECIFIED., .F., .F. ) 
 B_SPLINE_CURVE_WITH_KNOTS ( ( 3, 2, 2, 3 ),
 ( 0.6007462686567165422, 0.6019900497512439275, 0.6032338308457712017, 0.6044776119402985870 ),
 .UNSPECIFIED. ) 
 CURVE ( )  GEOMETRIC_REPRESENTATION_ITEM ( )  RATIONAL_B_SPLINE_CURVE ( ( 0.9999999999999880096, 0.8660254037844506980, 1.000000000000000000, 0.8660254037844387076, 1.000000000000000000, 0.8660254037844267172, 1.000000000000011990 ) ) 
 REPRESENTATION_ITEM ( '' )  );
#4228 = LINE ( 'NONE', #26889, #26193 ) ;
#4230 = ORIENTED_EDGE ( 'NONE', *, *, #28859, .T. ) ;
#4229 = CARTESIAN_POINT ( 'NONE',  ( -2.293366432827344421E-15, -12.48450537969573659, -85.90625000204839523 ) ) ;
#4231 = EDGE_CURVE ( 'NONE', #22494, #22182, #33698, .T. ) ;
#4233 = ORIENTED_EDGE ( 'NONE', *, *, #17475, .F. ) ;
#4232 = CARTESIAN_POINT ( 'NONE',  ( 10.00000000000102318, -5.773502691895667560, -69.62499999999995737 ) ) ;
#4234 = ORIENTED_EDGE ( 'NONE', *, *, #24415, .T. ) ;
#4235 = CARTESIAN_POINT ( 'NONE',  ( -2.293366432827344421E-15, -12.48450537969573659, -22.71875000204837747 ) ) ;
#4236 = CARTESIAN_POINT ( 'NONE',  ( 5.405949406249999534, 9.363379034771803333, -10.28125000204835260 ) ) ;
#4237 = CARTESIAN_POINT ( 'NONE',  ( 10.81189881249999729, 0.000000000000000000, -71.84375000204836681 ) ) ;
#4238 = CARTESIAN_POINT ( 'NONE',  ( 7.070501591499376803E-16, 11.54700538379251284, -164.0000000040967905 ) ) ;
#4239 = CARTESIAN_POINT ( 'NONE',  ( 5.000000000000000000, 8.660254037844385522, -43.74999999999998579 ) ) ;
#4240 = CARTESIAN_POINT ( 'NONE',  ( 10.81189881249999551, -6.242252689847874514, -185.9687500020484094 ) ) ;
#4241 = CARTESIAN_POINT ( 'NONE',  ( 10.81189881249999729, 0.000000000000000000, -167.8437500020484094 ) ) ;
#4242 = CONICAL_SURFACE ( 'NONE', #10452, 57.00000000000002132, 0.7853981633974401744 ) ;
#4243 = DIRECTION ( 'NONE',  ( -0.000000000000000000, -0.000000000000000000, 1.000000000000000000 ) ) ;
#4244 = CARTESIAN_POINT ( 'NONE',  ( -9.999999999999998224, 1.224646799147353059E-15, -128.7499999999999716 ) ) ;
#4245 = CARTESIAN_POINT ( 'NONE',  ( 5.000000000000000000, 8.660254037844385522, -141.2500000000000000 ) ) ;
#4246 = CARTESIAN_POINT ( 'NONE',  ( 7.070501591499377789E-16, 11.54700538379251284, 0.9999999959032610519 ) ) ;
#4247 = CARTESIAN_POINT ( 'NONE',  ( 5.000000000000000000, 8.660254037844385522, -60.62500000409676204 ) ) ;
#4248 = APPROVAL_PERSON_ORGANIZATION ( #12499, #26222, #28933 ) ;
#4249 = CARTESIAN_POINT ( 'NONE',  ( -10.81189881249999729, 6.242252689847871849, -116.2187500020483810 ) ) ;
#4250 = CARTESIAN_POINT ( 'NONE',  ( 7.070501591499376803E-16, 11.54700538379251284, -161.0000000040968189 ) ) ;
#4251 = CARTESIAN_POINT ( 'NONE',  ( 10.81189881249999907, 6.242252689847868297, -92.90625000204839523 ) ) ;
#4252 = CARTESIAN_POINT ( 'NONE',  ( -2.293366432827344421E-15, -12.48450537969573659, -96.21875000204838102 ) ) ;
#4253 = CARTESIAN_POINT ( 'NONE',  ( 5.405949406249992428, -9.363379034771808662, -67.59375000204836681 ) ) ;
#4254 = CARTESIAN_POINT ( 'NONE',  ( -5.405949406249996869, 9.363379034771805109, -79.03125000204838102 ) ) ;
#4255 = CARTESIAN_POINT ( 'NONE',  ( -2.121150477449813534E-15, -11.54700538379251284, -152.7500000040967620 ) ) ;
#4256 = CARTESIAN_POINT ( 'NONE',  ( 10.00000000000000000, 5.773502691896255534, -132.3750000000000000 ) ) ;
#4257 = CARTESIAN_POINT ( 'NONE',  ( 10.81189881249999551, -6.242252689847874514, -160.6562500020484094 ) ) ;
#4258 = CARTESIAN_POINT ( 'NONE',  ( 5.405949406249999534, 9.363379034771803333, -175.2812500020484094 ) ) ;
#4259 = AXIS2_PLACEMENT_3D ( 'NONE', #39266, #22879, #32805 ) ;
#4260 = CARTESIAN_POINT ( 'NONE',  ( -10.81189881249999907, -6.242252689847864744, -0.4687500020483514329 ) ) ;
#4261 = DIRECTION ( 'NONE',  ( -1.000000000000000000, 0.000000000000000000, 0.000000000000000000 ) ) ;
#4262 = CARTESIAN_POINT ( 'NONE',  ( 10.81189881249999551, -6.242252689847874514, -106.4687500020483810 ) ) ;
#4263 = CARTESIAN_POINT ( 'NONE',  ( 7.070501591499376803E-16, 11.54700538379251284, -156.1250000000000000 ) ) ;
#4264 = CARTESIAN_POINT ( 'NONE',  ( -9.999999999999998224, 5.773502691896259087, -76.37499999999998579 ) ) ;
#4265 = CARTESIAN_POINT ( 'NONE',  ( -2.293366432827344421E-15, -12.48450537969573659, -6.406250002048363257 ) ) ;
#4266 = CARTESIAN_POINT ( 'NONE',  ( -2.121150477449813534E-15, -11.54700538379251284, -88.25000000409677625 ) ) ;
#4267 = CARTESIAN_POINT ( 'NONE',  ( 9.999999999999998224, 0.000000000000000000, -171.5000000000000000 ) ) ;
#4268 = CARTESIAN_POINT ( 'NONE',  ( 10.81189881249999907, 6.242252689847868297, -98.90625000204839523 ) ) ;
#4269 = CARTESIAN_POINT ( 'NONE',  ( -10.81189881249999729, -6.242252689847864744, -83.15625000204836681 ) ) ;
#4270 = CARTESIAN_POINT ( 'NONE',  ( 5.000000000000000000, 8.660254037844385522, -77.12500000409677625 ) ) ;
#4271 = CARTESIAN_POINT ( 'NONE',  ( 9.999999999999998224, 0.000000000000000000, -168.5000000000000000 ) ) ;
#4272 = CARTESIAN_POINT ( 'NONE',  ( -2.293366432827344421E-15, -12.48450537969573659, -31.71875000204834905 ) ) ;
#4273 = VERTEX_POINT ( 'NONE', #14229 ) ;
#4274 = CARTESIAN_POINT ( 'NONE',  ( -10.81189881249999729, 1.324075727343319199E-15, -197.2812500020484094 ) ) ;
#4275 = CARTESIAN_POINT ( 'NONE',  ( -10.81189881249999729, 6.242252689847871849, -24.90625000204838102 ) ) ;
#4276 = CARTESIAN_POINT ( 'NONE',  ( 5.405949406249992428, -9.363379034771808662, -15.09375000204835082 ) ) ;
#4277 = DIRECTION ( 'NONE',  ( -0.000000000000000000, -0.000000000000000000, 1.000000000000000000 ) ) ;
#4278 = CARTESIAN_POINT ( 'NONE',  ( -10.00000000000000000, -5.773502691896251982, -1.500000004096752271 ) ) ;
#4279 = CARTESIAN_POINT ( 'NONE',  ( -5.405949406250003975, -9.363379034771801557, -138.5312500020484094 ) ) ;
#4280 = CARTESIAN_POINT ( 'NONE',  ( 5.000000000000000000, 8.660254037844385522, -186.2500000000000000 ) ) ;
#4281 = EDGE_CURVE ( 'NONE', #42437, #28218, #36922, .T. ) ;
#4282 = CARTESIAN_POINT ( 'NONE',  ( -9.999999999999742428, -5.773502691896402084, -156.0000000040968473 ) ) ;
#4284 = ORIENTED_EDGE ( 'NONE', *, *, #33039, .F. ) ;
#4283 = CARTESIAN_POINT ( 'NONE',  ( 5.405949406249992428, -9.363379034771808662, -109.7812500020483810 ) ) ;
#4285 = FACE_OUTER_BOUND ( 'NONE', #37764, .T. ) ;
#4286 = EDGE_CURVE ( 'NONE', #31643, #5198, #23206, .T. ) ;
#4287 = VERTEX_POINT ( 'NONE', #3917 ) ;
#4288 = EDGE_CURVE ( 'NONE', #37390, #33430, #36691, .T. ) ;
#4289 = EDGE_LOOP ( 'NONE', ( #3235, #27590, #39153, #22336 ) ) ;
#4290 = CARTESIAN_POINT ( 'NONE',  ( -10.81189881249999729, 1.324075727343319199E-15, -41.28125000204838102 ) ) ;
#4291 = APPROVAL_DATE_TIME ( #7528, #38361 ) ;
#4292 = CARTESIAN_POINT ( 'NONE',  ( 10.81189881249999729, 0.000000000000000000, -92.84375000204838102 ) ) ;
#4293 = FACE_OUTER_BOUND ( 'NONE', #32853, .T. ) ;
#4294 =( BOUNDED_CURVE ( )  B_SPLINE_CURVE ( 2, ( #40816, #20761, #4793, #11256, #11468, #17298, #21189 ),
 .UNSPECIFIED., .F., .F. ) 
 B_SPLINE_CURVE_WITH_KNOTS ( ( 3, 2, 2, 3 ),
 ( 0.6529850746268659467, 0.6542288557213932210, 0.6554726368159206062, 0.6567164179104479915 ),
 .UNSPECIFIED. ) 
 CURVE ( )  GEOMETRIC_REPRESENTATION_ITEM ( )  RATIONAL_B_SPLINE_CURVE ( ( 0.9999999999999761302, 0.8660254037844625774, 1.000000000000000000, 0.8660254037844387076, 1.000000000000000000, 0.8660254037844148378, 1.000000000000023981 ) ) 
 REPRESENTATION_ITEM ( '' )  );
#4295 = CARTESIAN_POINT ( 'NONE',  ( -9.999999999999998224, 1.224646799147353059E-15, -173.7500000000000284 ) ) ;
#4296 = CARTESIAN_POINT ( 'NONE',  ( 10.81189881249999551, -6.242252689847874514, -193.4687500020484094 ) ) ;
#4297 = CARTESIAN_POINT ( 'NONE',  ( -10.81189881249999729, 1.324075727343319199E-15, -170.2812500020484094 ) ) ;
#4298 = EDGE_CURVE ( 'NONE', #25488, #13677, #23467, .T. ) ;
#4299 = CARTESIAN_POINT ( 'NONE',  ( -2.293366432827344421E-15, -12.48450537969573659, -123.2187500020483952 ) ) ;
#4300 = CARTESIAN_POINT ( 'NONE',  ( 5.405949406249992428, -9.363379034771808662, -94.59375000204838102 ) ) ;
#4301 = CARTESIAN_POINT ( 'NONE',  ( 9.999999999999479527, 5.773502691896553074, -113.2500000040967620 ) ) ;
#4302 = CARTESIAN_POINT ( 'NONE',  ( 10.81189881249999907, 6.242252689847868297, -100.4062500020483952 ) ) ;
#4303 = CARTESIAN_POINT ( 'NONE',  ( 7.070501591499377789E-16, 11.54700538379251284, -185.0000000040967905 ) ) ;
#4304 = CARTESIAN_POINT ( 'NONE',  ( -10.81189881249999729, 6.242252689847871849, -110.2187500020483810 ) ) ;
#4305 = CARTESIAN_POINT ( 'NONE',  ( -2.293366432827344421E-15, -12.48450537969573659, -175.9062500020484379 ) ) ;
#4306 = CARTESIAN_POINT ( 'NONE',  ( 9.999999999999998224, 0.000000000000000000, -180.5000000000000000 ) ) ;
#4307 = CARTESIAN_POINT ( 'NONE',  ( 7.070501591499376803E-16, 11.54700538379251284, -122.0000000040967905 ) ) ;
#4308 = CARTESIAN_POINT ( 'NONE',  ( 10.81189881249999729, 0.000000000000000000, -199.5312500020484094 ) ) ;
#4309 = CARTESIAN_POINT ( 'NONE',  ( -5.405949406250003975, -9.363379034771801557, -51.34375000204835260 ) ) ;
#4310 = CARTESIAN_POINT ( 'NONE',  ( 10.81189881249999729, 0.000000000000000000, -43.34375000204837391 ) ) ;
#4311 = CARTESIAN_POINT ( 'NONE',  ( 7.070501591499377789E-16, 11.54700538379251284, -176.0000000040968189 ) ) ;
#4312 = CARTESIAN_POINT ( 'NONE',  ( 5.405949406249992428, -9.363379034771808662, -9.281250002048352599 ) ) ;
#4313 = CARTESIAN_POINT ( 'NONE',  ( 10.81189881249999907, 6.242252689847868297, -19.21875000204836681 ) ) ;
#4314 = CARTESIAN_POINT ( 'NONE',  ( -9.999999999999479527, -5.773502691896549521, -93.00000000409676204 ) ) ;
#4315 = CARTESIAN_POINT ( 'NONE',  ( -5.405949406250003975, -9.363379034771801557, -133.8437500020484094 ) ) ;
#4316 = CARTESIAN_POINT ( 'NONE',  ( 9.999999999999996447, -5.773502691896262640, -93.62499999999998579 ) ) ;
#4317 = CARTESIAN_POINT ( 'NONE',  ( 5.405949406249992428, -9.363379034771808662, -27.28125000204836681 ) ) ;
#4318 = CARTESIAN_POINT ( 'NONE',  ( -5.000000000000003553, -8.660254037844383745, -112.3750000040967763 ) ) ;
#4319 = EDGE_CURVE ( 'NONE', #40567, #29474, #21818, .T. ) ;
#4320 = CARTESIAN_POINT ( 'NONE',  ( 9.999999999999998224, 0.000000000000000000, -158.3750000040967905 ) ) ;
#4321 = CARTESIAN_POINT ( 'NONE',  ( -9.999999999999998224, 5.773502691896259087, -62.87499999999998579 ) ) ;
#4322 = CARTESIAN_POINT ( 'NONE',  ( -5.405949406250003975, -9.363379034771801557, -120.5312500020483952 ) ) ;
#4323 = CARTESIAN_POINT ( 'NONE',  ( -2.293366432827344421E-15, -12.48450537969573659, -108.4062500020483810 ) ) ;
#4324 = EDGE_LOOP ( 'NONE', ( #25882, #24799, #9220, #28023 ) ) ;
#4325 = CARTESIAN_POINT ( 'NONE',  ( 9.999999999999998224, 0.000000000000000000, -8.375000004096744277 ) ) ;
#4326 = CARTESIAN_POINT ( 'NONE',  ( -2.121150477449813534E-15, -11.54700538379251284, -103.2500000040967763 ) ) ;
#4327 = CARTESIAN_POINT ( 'NONE',  ( -9.999999999999998224, 1.224646799147353059E-15, -166.6250000040967905 ) ) ;
#4328 = CARTESIAN_POINT ( 'NONE',  ( 10.81189881249999729, 0.000000000000000000, -59.84375000204835970 ) ) ;
#4329 = VERTEX_POINT ( 'NONE', #37127 ) ;
#4330 = CARTESIAN_POINT ( 'NONE',  ( 5.000000000000000000, 8.660254037844385522, -27.24999999999996803 ) ) ;
#4331 = CARTESIAN_POINT ( 'NONE',  ( 7.644554776091147741E-16, 12.48450537969573659, -32.65625000204835970 ) ) ;
#4332 = CARTESIAN_POINT ( 'NONE',  ( -9.999999999999998224, 5.773502691896259087, -160.3749999999999716 ) ) ;
#4333 = CARTESIAN_POINT ( 'NONE',  ( 4.999999999999992006, -8.660254037844389075, -26.62500000409676204 ) ) ;
#4334 = CARTESIAN_POINT ( 'NONE',  ( 10.81189881249999729, 0.000000000000000000, -133.5312500020484094 ) ) ;
#4335 = ADVANCED_FACE ( 'NONE', ( #4336 ), #17908, .F. ) ;
#4336 = FACE_OUTER_BOUND ( 'NONE', #32090, .T. ) ;
#4337 = ORIENTED_EDGE ( 'NONE', *, *, #2216, .F. ) ;
#4338 =( BOUNDED_CURVE ( )  B_SPLINE_CURVE ( 2, ( #38895, #32012, #28559, #9323, #35667, #41691, #41260 ),
 .UNSPECIFIED., .F., .F. ) 
 B_SPLINE_CURVE_WITH_KNOTS ( ( 3, 2, 2, 3 ),
 ( 0.6940298507462688837, 0.6952736318407962690, 0.6965174129353237653, 0.6977611940298510396 ),
 .UNSPECIFIED. ) 
 CURVE ( )  GEOMETRIC_REPRESENTATION_ITEM ( )  RATIONAL_B_SPLINE_CURVE ( ( 0.9999999999999761302, 0.8660254037844625774, 1.000000000000000000, 0.8660254037844387076, 1.000000000000000000, 0.8660254037844028474, 1.000000000000035971 ) ) 
 REPRESENTATION_ITEM ( '' )  );
#4339 = EDGE_CURVE ( 'NONE', #32487, #3490, #1538, .T. ) ;
#4340 = EDGE_CURVE ( 'NONE', #30728, #18233, #34772, .T. ) ;
#4342 = VERTEX_POINT ( 'NONE', #5413 ) ;
#4341 = VERTEX_POINT ( 'NONE', #15094 ) ;
#4343 = CARTESIAN_POINT ( 'NONE',  ( -9.999999999999742428, -5.773502691896402084, -121.1250000000000000 ) ) ;
#4344 = CC_DESIGN_PERSON_AND_ORGANIZATION_ASSIGNMENT ( #13434, #10000, ( #19626 ) ) ;
#4345 = CARTESIAN_POINT ( 'NONE',  ( 4.999999999999992006, -8.660254037844389075, -134.2499999999999716 ) ) ;
#4346 = CARTESIAN_POINT ( 'NONE',  ( -2.293366432827344421E-15, -12.48450537969573659, -163.7187500020483810 ) ) ;
#4347 = CARTESIAN_POINT ( 'NONE',  ( -2.293366432827344421E-15, -12.48450537969573659, -193.9062500020484094 ) ) ;
#4348 = CARTESIAN_POINT ( 'NONE',  ( -2.293366432827344421E-15, -12.48450537969573659, -18.21875000204837036 ) ) ;
#4349 = DIRECTION ( 'NONE',  ( 1.000000000000000000, 0.000000000000000000, 0.000000000000000000 ) ) ;
#4350 = CARTESIAN_POINT ( 'NONE',  ( -10.81189881249999729, 1.324075727343319199E-15, -149.0937500020483810 ) ) ;
#4351 = CARTESIAN_POINT ( 'NONE',  ( -10.81189881249999729, 6.242252689847871849, -135.7187500020483810 ) ) ;
#4352 = CARTESIAN_POINT ( 'NONE',  ( 5.405949406249999534, 9.363379034771803333, -109.2812500020483810 ) ) ;
#4353 = CARTESIAN_POINT ( 'NONE',  ( 10.81189881249999551, -6.242252689847874514, -116.9687500020483952 ) ) ;
#4354 = CARTESIAN_POINT ( 'NONE',  ( 5.405949406249992428, -9.363379034771808662, -0.09375000204836503315 ) ) ;
#4355 = CARTESIAN_POINT ( 'NONE',  ( 5.405949406249992428, -9.363379034771808662, -127.7812500020483810 ) ) ;
#4356 = CARTESIAN_POINT ( 'NONE',  ( -5.405949406249996869, 9.363379034771805109, -12.84375000204834905 ) ) ;
#4358 = EDGE_CURVE ( 'NONE', #35303, #32901, #36921, .T. ) ;
#4357 = CARTESIAN_POINT ( 'NONE',  ( 10.81189881249999729, 6.242252689847867408, -130.2187500020483810 ) ) ;
#4359 = DIRECTION ( 'NONE',  ( 0.000000000000000000, 0.000000000000000000, 1.000000000000000000 ) ) ;
#4360 = CARTESIAN_POINT ( 'NONE',  ( 9.999999999999998224, 0.000000000000000000, -96.49999999999998579 ) ) ;
#4361 = CARTESIAN_POINT ( 'NONE',  ( -2.121150477449813534E-15, -11.54700538379251284, -152.3750000000000000 ) ) ;
#4362 = CARTESIAN_POINT ( 'NONE',  ( -9.999999999999998224, 5.773502691896259087, -17.87499999999997513 ) ) ;
#4363 = CARTESIAN_POINT ( 'NONE',  ( -10.81189881249999729, 6.242252689847871849, -77.21875000204838102 ) ) ;
#4364 = CARTESIAN_POINT ( 'NONE',  ( 10.81189881249999729, 0.000000000000000000, -68.84375000204836681 ) ) ;
#4365 = CARTESIAN_POINT ( 'NONE',  ( -9.999999999999998224, 1.224646799147353059E-15, -167.7500000000000000 ) ) ;
#4366 = CARTESIAN_POINT ( 'NONE',  ( -10.81189881249999729, 1.324075727343319199E-15, -35.28125000204837391 ) ) ;
#4367 = CARTESIAN_POINT ( 'NONE',  ( -10.81189881249999729, 1.324075727343319199E-15, -47.09375000204838102 ) ) ;
#4368 = CARTESIAN_POINT ( 'NONE',  ( -9.999999999999998224, 1.224646799147353059E-15, -171.1250000040968189 ) ) ;
#4369 = CARTESIAN_POINT ( 'NONE',  ( -2.293366432827344421E-15, -12.48450537969573659, -154.7187500020483810 ) ) ;
#4370 = CARTESIAN_POINT ( 'NONE',  ( -9.999999999999998224, 5.773502691896259087, -118.3750000000000000 ) ) ;
#4371 = CARTESIAN_POINT ( 'NONE',  ( -10.81189881249999729, 1.324075727343319199E-15, -134.2812500020483810 ) ) ;
#4372 = DIRECTION ( 'NONE',  ( 0.000000000000000000, -0.000000000000000000, 1.000000000000000000 ) ) ;
#4373 = CARTESIAN_POINT ( 'NONE',  ( 10.00000000000000000, 5.773502691896255534, -81.37499999999998579 ) ) ;
#4374 = CARTESIAN_POINT ( 'NONE',  ( -10.81189881249999729, -6.242252689847864744, -15.65625000204837569 ) ) ;
#4375 = EDGE_LOOP ( 'NONE', ( #6883, #24316, #26270, #14560 ) ) ;
#4376 = LINE ( 'NONE', #5024, #2453 ) ;
#4377 = CARTESIAN_POINT ( 'NONE',  ( 9.999999999999996447, -5.773502691896262640, -122.5000000040967905 ) ) ;
#4378 = CARTESIAN_POINT ( 'NONE',  ( 5.000000000000000000, 8.660254037844385522, -9.249999999999952038 ) ) ;
#4379 = CARTESIAN_POINT ( 'NONE',  ( 7.070501591499377789E-16, 11.54700538379251284, -35.00000000409674783 ) ) ;
#4380 = CARTESIAN_POINT ( 'NONE',  ( 0.000000000000000000, 0.000000000000000000, -99.99999999999998579 ) ) ;
#4381 = CARTESIAN_POINT ( 'NONE',  ( -10.81189881249999907, -6.242252689847864744, -54.65625000204838102 ) ) ;
#4382 = CARTESIAN_POINT ( 'NONE',  ( -9.999999999999998224, 1.224646799147353059E-15, -136.2499999999999716 ) ) ;
#4383 = CARTESIAN_POINT ( 'NONE',  ( 10.81189881249999551, -6.242252689847874514, -150.1562500020484094 ) ) ;
#4384 = CARTESIAN_POINT ( 'NONE',  ( 5.405949406249992428, -9.363379034771808662, -132.0937500020483810 ) ) ;
#4385 = CARTESIAN_POINT ( 'NONE',  ( -9.999999999999996447, 5.773502691896259975, -165.2500000040967905 ) ) ;
#4386 = ORIENTED_EDGE ( 'NONE', *, *, #20247, .F. ) ;
#4387 = VERTEX_POINT ( 'NONE', #31752 ) ;
#4388 = VERTEX_POINT ( 'NONE', #41429 ) ;
#4390 = EDGE_LOOP ( 'NONE', ( #40997, #15151, #31808, #25816 ) ) ;
#4389 = CARTESIAN_POINT ( 'NONE',  ( -10.81189881249999907, -6.242252689847864744, -109.9687500020483668 ) ) ;
#4391 = FACE_OUTER_BOUND ( 'NONE', #42616, .T. ) ;
#4392 = CARTESIAN_POINT ( 'NONE',  ( 10.81189881249999551, -6.242252689847874514, -187.4687500020484094 ) ) ;
#4394 = EDGE_CURVE ( 'NONE', #16041, #33493, #11865, .T. ) ;
#4393 = CARTESIAN_POINT ( 'NONE',  ( -10.81189881249999907, -6.242252689847864744, -42.46875000204835260 ) ) ;
#4395 = CARTESIAN_POINT ( 'NONE',  ( 0.000000000000000000, 0.000000000000000000, -99.99999999999998579 ) ) ;
#4396 = CARTESIAN_POINT ( 'NONE',  ( -5.000000000000003553, -8.660254037844383745, -10.37500000409674605 ) ) ;
#4397 = CARTESIAN_POINT ( 'NONE',  ( -2.293366432827344421E-15, -12.48450537969573659, -169.7187500020483810 ) ) ;
#4398 = CARTESIAN_POINT ( 'NONE',  ( -5.405949406250003975, -9.363379034771801557, -157.8437500020483810 ) ) ;
#4399 = CARTESIAN_POINT ( 'NONE',  ( -2.121150477449813534E-15, -11.54700538379251284, -25.25000000409676559 ) ) ;
#4400 = CARTESIAN_POINT ( 'NONE',  ( 5.405949406249992428, -9.363379034771808662, -138.0937500020483810 ) ) ;
#4401 = CARTESIAN_POINT ( 'NONE',  ( 10.81189881249999551, -6.242252689847874514, -157.4687500020484379 ) ) ;
#4402 = CARTESIAN_POINT ( 'NONE',  ( -2.121150477449813534E-15, -11.54700538379251284, -42.87499999999997868 ) ) ;
#4403 = CARTESIAN_POINT ( 'NONE',  ( 4.999999999999992006, -8.660254037844389075, -139.1250000040967905 ) ) ;
#4404 = CARTESIAN_POINT ( 'NONE',  ( -10.00000000000000000, -5.773502691896251982, -179.6250000000000284 ) ) ;
#4405 = CARTESIAN_POINT ( 'NONE',  ( 5.405949406249992428, -9.363379034771808662, -85.59375000204836681 ) ) ;
#4406 = CARTESIAN_POINT ( 'NONE',  ( -2.520757610592990083, 10.51993215483609490, -99.99999999999995737 ) ) ;
#4407 = CARTESIAN_POINT ( 'NONE',  ( 10.81189881249999907, 6.242252689847868297, -55.40625000204837391 ) ) ;
#4408 = CARTESIAN_POINT ( 'NONE',  ( -4.999999999999996447, 8.660254037844387298, -87.37500000409677625 ) ) ;
#4409 = CARTESIAN_POINT ( 'NONE',  ( 10.81189881249999551, -6.242252689847874514, -175.4687500020484094 ) ) ;
#4410 = CARTESIAN_POINT ( 'NONE',  ( 10.81189881249999729, 0.000000000000000000, -120.0312500020483952 ) ) ;
#4411 = CARTESIAN_POINT ( 'NONE',  ( -2.293366432827344421E-15, -12.48450537969573659, -156.4062500020484379 ) ) ;
#4412 = FACE_OUTER_BOUND ( 'NONE', #14165, .T. ) ;
#4413 = CARTESIAN_POINT ( 'NONE',  ( -2.293366432827344421E-15, -12.48450537969573659, -54.40625000204838102 ) ) ;
#4414 = CARTESIAN_POINT ( 'NONE',  ( 10.00000000000000000, 5.773502691896255534, -131.2500000040967905 ) ) ;
#4415 = CARTESIAN_POINT ( 'NONE',  ( -9.999999999999998224, 5.773502691896259087, -109.3750000000000000 ) ) ;
#4416 = ORIENTED_EDGE ( 'NONE', *, *, #19816, .F. ) ;
#4417 = CARTESIAN_POINT ( 'NONE',  ( 10.81189881249999729, 6.242252689847867408, -134.9062500020483810 ) ) ;
#4418 = CARTESIAN_POINT ( 'NONE',  ( -4.999999999999996447, 8.660254037844387298, -150.3750000040967905 ) ) ;
#4419 = CARTESIAN_POINT ( 'NONE',  ( 5.405949406249992428, -9.363379034771808662, -148.7812500020483810 ) ) ;
#4420 = CARTESIAN_POINT ( 'NONE',  ( 5.405949406249992428, -9.363379034771808662, -189.2812500020484094 ) ) ;
#4421 = ORIENTED_EDGE ( 'NONE', *, *, #40051, .T. ) ;
#4422 = CARTESIAN_POINT ( 'NONE',  ( 7.070501591499377789E-16, 11.54700538379251284, -52.62499999999997868 ) ) ;
#4423 = CARTESIAN_POINT ( 'NONE',  ( -10.81189881249999729, 1.324075727343319199E-15, -179.0937500020484094 ) ) ;
#4424 = CARTESIAN_POINT ( 'NONE',  ( -4.999999999999996447, 8.660254037844387298, -55.87500000409676204 ) ) ;
#4425 = CARTESIAN_POINT ( 'NONE',  ( 9.999999999999998224, 0.000000000000000000, -108.8750000040967763 ) ) ;
#4426 =( BOUNDED_CURVE ( )  B_SPLINE_CURVE ( 2, ( #11234, #41003, #4771, #6006, #9026, #18946, #2769 ),
 .UNSPECIFIED., .F., .F. ) 
 B_SPLINE_CURVE_WITH_KNOTS ( ( 3, 2, 2, 3 ),
 ( 0.3507462686567164867, 0.3519900497512438720, 0.3532338308457712572, 0.3544776119402986980 ),
 .UNSPECIFIED. ) 
 CURVE ( )  GEOMETRIC_REPRESENTATION_ITEM ( )  RATIONAL_B_SPLINE_CURVE ( ( 0.9999999999999940048, 0.8660254037844447028, 1.000000000000000000, 0.8660254037844387076, 1.000000000000000000, 0.8660254037844207220, 1.000000000000017986 ) ) 
 REPRESENTATION_ITEM ( '' )  );
#4427 = CARTESIAN_POINT ( 'NONE',  ( -11.54700538379250574, -20.00000000000000355, 45.00000000000009237 ) ) ;
#4428 = CARTESIAN_POINT ( 'NONE',  ( 5.405949406249992428, -9.363379034771808662, -78.28125000204838102 ) ) ;
#4429 = CARTESIAN_POINT ( 'NONE',  ( 5.405949406249999534, 9.363379034771803333, -53.78125000204836681 ) ) ;
#4430 = CARTESIAN_POINT ( 'NONE',  ( -9.999999999999998224, 1.224646799147353059E-15, -55.62500000409676204 ) ) ;
#4431 = CARTESIAN_POINT ( 'NONE',  ( 5.405949406249999534, 9.363379034771803333, -10.09375000204834549 ) ) ;
#4432 = DIRECTION ( 'NONE',  ( -0.000000000000000000, -0.000000000000000000, 1.000000000000000000 ) ) ;
#4433 = CARTESIAN_POINT ( 'NONE',  ( 10.81189881249999729, 0.000000000000000000, -175.5312500020483810 ) ) ;
#4434 = CARTESIAN_POINT ( 'NONE',  ( 5.405949406249999534, 9.363379034771803333, -5.781250002048377468 ) ) ;
#4435 = CARTESIAN_POINT ( 'NONE',  ( -9.999999999999998224, 1.224646799147353059E-15, -200.0000000000000000 ) ) ;
#4436 = DIRECTION ( 'NONE',  ( 0.000000000000000000, 0.000000000000000000, 1.000000000000000000 ) ) ;
#4437 = CARTESIAN_POINT ( 'NONE',  ( -2.121150477449813534E-15, -11.54700538379251284, -89.37499999999997158 ) ) ;
#4438 = CARTESIAN_POINT ( 'NONE',  ( -10.00000000000051337, 5.773502691895962435, -105.2500000040967620 ) ) ;
#4439 = CARTESIAN_POINT ( 'NONE',  ( 7.070501591499376803E-16, 11.54700538379251284, -39.50000000409675494 ) ) ;
#4441 = EDGE_LOOP ( 'NONE', ( #28605, #21906, #40386, #26571 ) ) ;
#4440 = CARTESIAN_POINT ( 'NONE',  ( -5.405949406250003975, -9.363379034771801557, -83.03125000204838102 ) ) ;
#4443 = ORIENTED_EDGE ( 'NONE', *, *, #8828, .T. ) ;
#4442 = CARTESIAN_POINT ( 'NONE',  ( 0.000000000000000000, 0.000000000000000000, -99.99999999999998579 ) ) ;
#4444 = EDGE_LOOP ( 'NONE', ( #4635, #2340, #108, #23454 ) ) ;
#4445 = EDGE_CURVE ( 'NONE', #6420, #18833, #38084, .T. ) ;
#4446 = CARTESIAN_POINT ( 'NONE',  ( 10.81189881249999551, -6.242252689847874514, -35.96875000204835260 ) ) ;
#4447 = CARTESIAN_POINT ( 'NONE',  ( 10.81189881249999551, -6.242252689847874514, -25.46875000204837391 ) ) ;
#4448 = CARTESIAN_POINT ( 'NONE',  ( -2.293366432827344421E-15, -12.48450537969573659, -15.40625000204837391 ) ) ;
#4449 = CARTESIAN_POINT ( 'NONE',  ( -10.81189881249999729, 6.242252689847871849, -66.71875000204838102 ) ) ;
#4450 = CARTESIAN_POINT ( 'NONE',  ( 10.00000000000000000, 5.773502691896255534, -45.37499999999997158 ) ) ;
#4451 = CARTESIAN_POINT ( 'NONE',  ( 5.405949406249992428, -9.363379034771808662, -181.5937500020483810 ) ) ;
#4452 = CARTESIAN_POINT ( 'NONE',  ( 7.644554776091147741E-16, 12.48450537969573659, -162.9687500020483810 ) ) ;
#4453 = LINE ( 'NONE', #15001, #32376 ) ;
#4454 = DIRECTION ( 'NONE',  ( -0.000000000000000000, -0.000000000000000000, 1.000000000000000000 ) ) ;
#4455 = CARTESIAN_POINT ( 'NONE',  ( -9.999999999999998224, 1.224646799147353059E-15, -65.74999999999997158 ) ) ;
#4456 = CYLINDRICAL_SURFACE ( 'NONE', #14879, 9.750000000000003553 ) ;
#4457 = CARTESIAN_POINT ( 'NONE',  ( 0.000000000000000000, 0.000000000000000000, -200.0000000000000000 ) ) ;
#4458 = CARTESIAN_POINT ( 'NONE',  ( -10.81189881249999729, 6.242252689847871849, -110.2187500020483810 ) ) ;
#4459 = LINE ( 'NONE', #20218, #28719 ) ;
#4460 = CARTESIAN_POINT ( 'NONE',  ( 5.405949406249992428, -9.363379034771808662, -93.28125000204838102 ) ) ;
#4461 = CARTESIAN_POINT ( 'NONE',  ( -10.81189881249999729, 1.324075727343319199E-15, -102.5937500020483810 ) ) ;
#4462 = EDGE_CURVE ( 'NONE', #7311, #33113, #34555, .T. ) ;
#4463 = CARTESIAN_POINT ( 'NONE',  ( -10.81189881249999907, -6.242252689847864744, -72.46875000204835260 ) ) ;
#4464 = CARTESIAN_POINT ( 'NONE',  ( 10.81189881249999729, 0.000000000000000000, -76.53125000204838102 ) ) ;
#4465 = CARTESIAN_POINT ( 'NONE',  ( 9.999999999999996447, -5.773502691896262640, -152.5000000040967905 ) ) ;
#4466 = CARTESIAN_POINT ( 'NONE',  ( 7.070501591499377789E-16, 11.54700538379251284, -135.1250000000000000 ) ) ;
#4467 =( BOUNDED_CURVE ( )  B_SPLINE_CURVE ( 2, ( #20196, #3174, #9845, #29926, #367, #19766, #15878 ),
 .UNSPECIFIED., .F., .F. ) 
 B_SPLINE_CURVE_WITH_KNOTS ( ( 3, 2, 2, 3 ),
 ( 0.7649253731343285123, 0.7661691542288557866, 0.7674129353233831718, 0.7686567164179105571 ),
 .UNSPECIFIED. ) 
 CURVE ( )  GEOMETRIC_REPRESENTATION_ITEM ( )  RATIONAL_B_SPLINE_CURVE ( ( 0.9999999999999880096, 0.8660254037844506980, 1.000000000000000000, 0.8660254037844387076, 1.000000000000000000, 0.8660254037844267172, 1.000000000000011990 ) ) 
 REPRESENTATION_ITEM ( '' )  );
#4468 = CARTESIAN_POINT ( 'NONE',  ( 10.81189881249999551, -6.242252689847874514, -159.1562500020484094 ) ) ;
#4469 = CARTESIAN_POINT ( 'NONE',  ( 5.405949406249992428, -9.363379034771808662, -174.2812500020484094 ) ) ;
#4470 = CARTESIAN_POINT ( 'NONE',  ( -4.999999999999996447, 8.660254037844387298, -153.3750000040967905 ) ) ;
#4471 = DIRECTION ( 'NONE',  ( 0.000000000000000000, 0.000000000000000000, -1.000000000000000000 ) ) ;
#4472 = CARTESIAN_POINT ( 'NONE',  ( -5.405949406250003975, -9.363379034771801557, -108.3437500020483810 ) ) ;
#4473 = CARTESIAN_POINT ( 'NONE',  ( -9.999999999999998224, 1.224646799147353059E-15, -130.6250000040967620 ) ) ;
#4474 = CARTESIAN_POINT ( 'NONE',  ( -4.999999999999996447, 8.660254037844387298, -73.49999999999998579 ) ) ;
#4475 = CARTESIAN_POINT ( 'NONE',  ( 7.644554776091147741E-16, 12.48450537969573659, -1.156250002048359038 ) ) ;
#4476 = CARTESIAN_POINT ( 'NONE',  ( -5.000000000000003553, -8.660254037844383745, -80.87500000409677625 ) ) ;
#4477 = CARTESIAN_POINT ( 'NONE',  ( 10.00000000000051159, -5.773502691895965988, -95.50000000409676204 ) ) ;
#4478 = CARTESIAN_POINT ( 'NONE',  ( 7.644554776091147741E-16, 12.48450537969573659, -98.65625000204838102 ) ) ;
#4479 = CARTESIAN_POINT ( 'NONE',  ( -10.81189881249999729, 1.324075727343319199E-15, -80.28125000204838102 ) ) ;
#4480 =( BOUNDED_CURVE ( )  B_SPLINE_CURVE ( 2, ( #4327, #40343, #14658, #11423, #37766, #17465, #1742 ),
 .UNSPECIFIED., .F., .F. ) 
 B_SPLINE_CURVE_WITH_KNOTS ( ( 3, 2, 2, 3 ),
 ( 0.1604477611940298698, 0.1616915422885572551, 0.1629353233830845848, 0.1641791044776119424 ),
 .UNSPECIFIED. ) 
 CURVE ( )  GEOMETRIC_REPRESENTATION_ITEM ( )  RATIONAL_B_SPLINE_CURVE ( ( 0.9999999999999970024, 0.8660254037844417052, 1.000000000000000000, 0.8660254037844387076, 1.000000000000000000, 0.8660254037844387076, 1.000000000000000000 ) ) 
 REPRESENTATION_ITEM ( '' )  );
#4481 = CARTESIAN_POINT ( 'NONE',  ( -5.000000000000003553, -8.660254037844383745, -73.37500000409677625 ) ) ;
#4482 = CARTESIAN_POINT ( 'NONE',  ( -9.999999999999998224, 1.224646799147353059E-15, -167.7500000000000000 ) ) ;
#4483 = CARTESIAN_POINT ( 'NONE',  ( -10.81189881249999907, -6.242252689847864744, -37.96875000204835970 ) ) ;
#4484 = EDGE_LOOP ( 'NONE', ( #27084, #12915, #33120, #2907 ) ) ;
#4485 = CARTESIAN_POINT ( 'NONE',  ( -5.000000000000003553, -8.660254037844383745, -2.499999999999974243 ) ) ;
#4486 = CARTESIAN_POINT ( 'NONE',  ( 10.81189881249999907, 6.242252689847868297, -26.90625000204838813 ) ) ;
#4487 = CARTESIAN_POINT ( 'NONE',  ( 5.405949406249999534, 9.363379034771803333, -11.59375000204834727 ) ) ;
#4488 = CARTESIAN_POINT ( 'NONE',  ( -5.000000000000003553, -8.660254037844383745, -176.8750000040967905 ) ) ;
#4489 = CARTESIAN_POINT ( 'NONE',  ( -5.000000000000003553, -8.660254037844383745, -1.375000004096765815 ) ) ;
#4490 = CARTESIAN_POINT ( 'NONE',  ( 10.81189881249999907, 6.242252689847868297, -128.9062500020483810 ) ) ;
#4491 = CARTESIAN_POINT ( 'NONE',  ( -4.999999999999996447, 8.660254037844387298, -181.5000000000000000 ) ) ;
#4492 = CARTESIAN_POINT ( 'NONE',  ( 0.000000000000000000, 0.000000000000000000, -200.0000000000000000 ) ) ;
#4494 = ORIENTED_EDGE ( 'NONE', *, *, #38620, .F. ) ;
#4493 = CARTESIAN_POINT ( 'NONE',  ( 10.81189881249999551, -6.242252689847874514, -108.1562500020483810 ) ) ;
#4495 = CARTESIAN_POINT ( 'NONE',  ( -4.999999999999996447, 8.660254037844387298, -138.3750000040967905 ) ) ;
#4496 = ORIENTED_EDGE ( 'NONE', *, *, #2895, .F. ) ;
#4497 = ORIENTED_EDGE ( 'NONE', *, *, #37845, .F. ) ;
#4498 = CARTESIAN_POINT ( 'NONE',  ( 5.405949406249992428, -9.363379034771808662, -37.78125000204838102 ) ) ;
#4499 = PERSON_AND_ORGANIZATION ( #11915, #17965 ) ;
#4500 = CARTESIAN_POINT ( 'NONE',  ( 10.81189881249999551, -6.242252689847874514, -89.96875000204838102 ) ) ;
#4501 = CARTESIAN_POINT ( 'NONE',  ( 9.999999999999998224, 0.000000000000000000, -167.0000000000000000 ) ) ;
#4502 = CARTESIAN_POINT ( 'NONE',  ( 0.000000000000000000, 0.000000000000000000, -200.0000000000000000 ) ) ;
#4503 = AXIS2_PLACEMENT_3D ( 'NONE', #31678, #8996, #7561 ) ;
#4504 = CARTESIAN_POINT ( 'NONE',  ( 10.81189881249999551, -6.242252689847874514, -172.6562500020484379 ) ) ;
#4505 = CARTESIAN_POINT ( 'NONE',  ( 9.999999999999998224, 1.224646799147353059E-15, -99.99999999999998579 ) ) ;
#4506 = CARTESIAN_POINT ( 'NONE',  ( -10.81189881249999729, 1.324075727343319199E-15, -122.0937500020483952 ) ) ;
#4507 = CARTESIAN_POINT ( 'NONE',  ( 7.644554776091147741E-16, 12.48450537969573659, -92.46875000204838102 ) ) ;
#4508 = CARTESIAN_POINT ( 'NONE',  ( 10.81189881249999551, -6.242252689847874514, -0.1562500020483646446 ) ) ;
#4509 = CARTESIAN_POINT ( 'NONE',  ( 7.070501591499376803E-16, 11.54700538379251284, -154.6250000000000284 ) ) ;
#4510 = CARTESIAN_POINT ( 'NONE',  ( -10.81189881249999729, 6.242252689847871849, -96.90625000204838102 ) ) ;
#4511 = CARTESIAN_POINT ( 'NONE',  ( -9.999999999999998224, 5.773502691896259087, -178.7500000040967905 ) ) ;
#4512 = CARTESIAN_POINT ( 'NONE',  ( -5.405949406250003975, -9.363379034771801557, -106.8437500020483810 ) ) ;
#4513 = CARTESIAN_POINT ( 'NONE',  ( -5.405949406250003975, -9.363379034771801557, -177.5312500020483810 ) ) ;
#4514 = CYLINDRICAL_SURFACE ( 'NONE', #40311, 5.500000000000003553 ) ;
#4515 = CARTESIAN_POINT ( 'NONE',  ( 10.81189881249999551, -6.242252689847874514, -195.1562500020484379 ) ) ;
#4516 = CARTESIAN_POINT ( 'NONE',  ( -5.405949406249996869, 9.363379034771805109, -48.84375000204838102 ) ) ;
#4517 = CARTESIAN_POINT ( 'NONE',  ( -10.81189881249999907, -6.242252689847864744, -43.96875000204835970 ) ) ;
#4518 = CARTESIAN_POINT ( 'NONE',  ( 9.999999999999998224, 0.000000000000000000, -170.3750000040968189 ) ) ;
#4519 = CARTESIAN_POINT ( 'NONE',  ( -10.81189881249999907, -6.242252689847864744, -12.65625000204835970 ) ) ;
#4520 = CARTESIAN_POINT ( 'NONE',  ( -5.405949406249996869, 9.363379034771805109, -20.34375000204835615 ) ) ;
#4521 = CARTESIAN_POINT ( 'NONE',  ( -5.000000000000003553, -8.660254037844383745, -164.8750000040967905 ) ) ;
#4522 = CARTESIAN_POINT ( 'NONE',  ( 5.405949406249992428, -9.363379034771808662, -127.5937500020483668 ) ) ;
#4523 = EDGE_CURVE ( 'NONE', #10167, #38258, #24610, .T. ) ;
#4524 = CARTESIAN_POINT ( 'NONE',  ( 4.999999999999992006, -8.660254037844389075, -96.74999999999998579 ) ) ;
#4525 = CARTESIAN_POINT ( 'NONE',  ( 5.405949406249999534, 9.363379034771803333, -31.28125000204837036 ) ) ;
#4526 = CARTESIAN_POINT ( 'NONE',  ( 9.999999999999998224, 0.000000000000000000, -102.8750000040967763 ) ) ;
#4527 = CARTESIAN_POINT ( 'NONE',  ( -5.000000000000003553, -8.660254037844383745, -169.0000000000000000 ) ) ;
#4528 = CARTESIAN_POINT ( 'NONE',  ( 10.00000000000000000, 5.773502691896255534, -58.87499999999997868 ) ) ;
#4529 = CARTESIAN_POINT ( 'NONE',  ( -5.405949406250003975, -9.363379034771801557, -128.0312500020484094 ) ) ;
#4530 = CARTESIAN_POINT ( 'NONE',  ( 10.81189881249999551, -6.242252689847874514, -111.1562500020483952 ) ) ;
#4531 = ORIENTED_EDGE ( 'NONE', *, *, #30417, .F. ) ;
#4532 = CARTESIAN_POINT ( 'NONE',  ( 10.00000000000025402, -5.773502691896113426, -117.6250000000000142 ) ) ;
#4533 = CARTESIAN_POINT ( 'NONE',  ( 9.999999999999996447, -5.773502691896262640, -101.5000000040967905 ) ) ;
#4534 = CYLINDRICAL_SURFACE ( 'NONE', #8465, 9.999999999999998224 ) ;
#4535 = CARTESIAN_POINT ( 'NONE',  ( -5.405949406250003975, -9.363379034771801557, -168.5312500020484094 ) ) ;
#4536 = CARTESIAN_POINT ( 'NONE',  ( -10.81189881249999729, 1.324075727343319199E-15, -59.09375000204835970 ) ) ;
#4537 = ORIENTED_EDGE ( 'NONE', *, *, #19813, .F. ) ;
#4538 = CARTESIAN_POINT ( 'NONE',  ( 9.999999999999996447, -5.773502691896262640, -24.62499999999998934 ) ) ;
#4539 = CARTESIAN_POINT ( 'NONE',  ( -5.405949406249996869, 9.363379034771805109, -37.03125000204837391 ) ) ;
#4540 = CARTESIAN_POINT ( 'NONE',  ( 4.999999999999992006, -8.660254037844389075, -162.7500000000000000 ) ) ;
#4541 = LINE ( 'NONE', #1098, #26277 ) ;
#4542 = CARTESIAN_POINT ( 'NONE',  ( -9.999999999999998224, 1.224646799147353059E-15, -30.12500000409676204 ) ) ;
#4543 = VECTOR ( 'NONE', #28297, 1000.000000000000000 ) ;
#4544 = AXIS2_PLACEMENT_3D ( 'NONE', #28875, #16090, #9215 ) ;
#4545 = CARTESIAN_POINT ( 'NONE',  ( -9.999999999999998224, 1.224646799147353059E-15, -34.24999999999997158 ) ) ;
#4546 = CARTESIAN_POINT ( 'NONE',  ( -10.81189881249999729, 1.324075727343319199E-15, -137.2812500020483810 ) ) ;
#4547 = CARTESIAN_POINT ( 'NONE',  ( -1.880502898556992042, 9.996614838207573683, 4.524943085473207639E-15 ) ) ;
#4548 = AXIS2_PLACEMENT_3D ( 'NONE', #17327, #40410, #39788 ) ;
#4549 =( BOUNDED_CURVE ( )  B_SPLINE_CURVE ( 2, ( #18402, #41487, #11923, #21860, #18616, #12135, #31813 ),
 .UNSPECIFIED., .F., .F. ) 
 B_SPLINE_CURVE_WITH_KNOTS ( ( 3, 2, 2, 3 ),
 ( 0.9514925373134331954, 0.9527363184079605807, 0.9539800995024879660, 0.9552238805970153512 ),
 .UNSPECIFIED. ) 
 CURVE ( )  GEOMETRIC_REPRESENTATION_ITEM ( )  RATIONAL_B_SPLINE_CURVE ( ( 0.9999999999999641398, 0.8660254037844745678, 1.000000000000000000, 0.8660254037844387076, 1.000000000000000000, 0.8660254037843908570, 1.000000000000047740 ) ) 
 REPRESENTATION_ITEM ( '' )  );
#4550 = CARTESIAN_POINT ( 'NONE',  ( 5.000000000000000000, 8.660254037844385522, -167.1250000040967905 ) ) ;
#4551 = ORIENTED_EDGE ( 'NONE', *, *, #36139, .T. ) ;
#4553 = EDGE_LOOP ( 'NONE', ( #1161, #17163, #11750, #29234 ) ) ;
#4552 = ORIENTED_EDGE ( 'NONE', *, *, #6442, .F. ) ;
#4554 = CARTESIAN_POINT ( 'NONE',  ( 7.070501591499376803E-16, 11.54700538379251284, -182.0000000040967905 ) ) ;
#4555 = CARTESIAN_POINT ( 'NONE',  ( -2.121150477449813534E-15, -11.54700538379251284, -146.7500000040967905 ) ) ;
#4556 = CARTESIAN_POINT ( 'NONE',  ( -10.81189881249999729, 1.324075727343319199E-15, -168.5937500020484094 ) ) ;
#4557 = CARTESIAN_POINT ( 'NONE',  ( -5.405949406249996869, 9.363379034771805109, -199.0312500020484094 ) ) ;
#4558 = CARTESIAN_POINT ( 'NONE',  ( 10.81189881249999729, 0.000000000000000000, -14.84375000204835082 ) ) ;
#4559 = FACE_OUTER_BOUND ( 'NONE', #30726, .T. ) ;
#4560 = CARTESIAN_POINT ( 'NONE',  ( 5.405949406249992428, -9.363379034771808662, -148.5937500020483810 ) ) ;
#4561 = CARTESIAN_POINT ( 'NONE',  ( -5.405949406249996869, 9.363379034771805109, -140.3437500020484094 ) ) ;
#4562 = CARTESIAN_POINT ( 'NONE',  ( -5.405949406249996869, 9.363379034771805109, -107.5312500020483810 ) ) ;
#4563 = CARTESIAN_POINT ( 'NONE',  ( 5.405949406249992428, -9.363379034771808662, -115.5937500020483810 ) ) ;
#4564 = CARTESIAN_POINT ( 'NONE',  ( -9.999999999999998224, 1.224646799147353059E-15, -195.1250000040967905 ) ) ;
#4565 = CARTESIAN_POINT ( 'NONE',  ( 10.81189881249999907, 6.242252689847868297, -127.4062500020483810 ) ) ;
#4566 = CARTESIAN_POINT ( 'NONE',  ( -5.405949406250003975, -9.363379034771801557, -3.343750002048367698 ) ) ;
#4567 = CARTESIAN_POINT ( 'NONE',  ( -5.405949406249996869, 9.363379034771805109, -134.3437500020484094 ) ) ;
#4568 = CARTESIAN_POINT ( 'NONE',  ( -9.999999999999998224, 1.224646799147353059E-15, -152.7500000000000000 ) ) ;
#4569 = CARTESIAN_POINT ( 'NONE',  ( -4.999999999999996447, 8.660254037844387298, -4.875000004096769146 ) ) ;
#4570 = CARTESIAN_POINT ( 'NONE',  ( 9.999999999999998224, 0.000000000000000000, -158.0000000000000000 ) ) ;
#4571 = CARTESIAN_POINT ( 'NONE',  ( 5.000000000000000000, 8.660254037844385522, -16.74999999999996092 ) ) ;
#4572 = CARTESIAN_POINT ( 'NONE',  ( 5.405949406249999534, 9.363379034771803333, -76.09375000204838102 ) ) ;
#4573 = CARTESIAN_POINT ( 'NONE',  ( -10.81189881249999907, -6.242252689847864744, -64.96875000204838102 ) ) ;
#4574 = CARTESIAN_POINT ( 'NONE',  ( -9.999999999999998224, 1.224646799147353059E-15, -170.7500000000000000 ) ) ;
#4575 = CARTESIAN_POINT ( 'NONE',  ( -5.405949406249996869, 9.363379034771805109, -35.53125000204837391 ) ) ;
#4576 = CARTESIAN_POINT ( 'NONE',  ( -2.293366432827344421E-15, -12.48450537969573659, -49.71875000204836681 ) ) ;
#4577 = CARTESIAN_POINT ( 'NONE',  ( 0.000000000000000000, 0.000000000000000000, -200.0000000000000000 ) ) ;
#4578 = EDGE_CURVE ( 'NONE', #28777, #34758, #42226, .T. ) ;
#4579 = CARTESIAN_POINT ( 'NONE',  ( -5.405949406249996869, 9.363379034771805109, -155.3437500020483810 ) ) ;
#4580 = EDGE_CURVE ( 'NONE', #19402, #25691, #27872, .T. ) ;
#4581 = CARTESIAN_POINT ( 'NONE',  ( -9.999999999999998224, 1.224646799147353059E-15, -124.2500000000000000 ) ) ;
#4582 = CARTESIAN_POINT ( 'NONE',  ( 10.81189881249999729, 6.242252689847867408, -131.9062500020483810 ) ) ;
#4583 = CARTESIAN_POINT ( 'NONE',  ( 1.498518790203807738, 10.17864512702100832, -179.9999999999998863 ) ) ;
#4584 = CARTESIAN_POINT ( 'NONE',  ( 9.999999999999996447, -5.773502691896262640, -80.12500000000000000 ) ) ;
#4585 = CARTESIAN_POINT ( 'NONE',  ( -10.81189881249999729, 1.324075727343319199E-15, -14.28125000204835615 ) ) ;
#4586 = ADVANCED_FACE ( 'NONE', ( #24347 ), #10722, .F. ) ;
#4587 = ORIENTED_EDGE ( 'NONE', *, *, #42588, .F. ) ;
#4588 = CARTESIAN_POINT ( 'NONE',  ( 7.644554776091147741E-16, 12.48450537969573659, -104.6562500020483810 ) ) ;
#4589 = CARTESIAN_POINT ( 'NONE',  ( 10.00000000000000000, 5.773502691896255534, -123.7500000040967905 ) ) ;
#4590 = CARTESIAN_POINT ( 'NONE',  ( 7.070501591499377789E-16, 11.54700538379251284, -38.00000000409676204 ) ) ;
#4591 = CARTESIAN_POINT ( 'NONE',  ( -10.00000000000051337, 5.773502691895962435, -148.3749999999999716 ) ) ;
#4592 = CC_DESIGN_PERSON_AND_ORGANIZATION_ASSIGNMENT ( #11816, #1919, ( #28392 ) ) ;
#4593 = CARTESIAN_POINT ( 'NONE',  ( -10.81189881249999729, 6.242252689847871849, -47.40625000204836681 ) ) ;
#4594 =( BOUNDED_CURVE ( )  B_SPLINE_CURVE ( 2, ( #8254, #37808, #18157, #15124, #34801, #35014, #12107 ),
 .UNSPECIFIED., .F., .F. ) 
 B_SPLINE_CURVE_WITH_KNOTS ( ( 3, 2, 2, 3 ),
 ( 0.3134328358208955390, 0.3146766169154229242, 0.3159203980099503650, 0.3171641791044778058 ),
 .UNSPECIFIED. ) 
 CURVE ( )  GEOMETRIC_REPRESENTATION_ITEM ( )  RATIONAL_B_SPLINE_CURVE ( ( 1.000000000000000000, 0.8660254037844387076, 1.000000000000000000, 0.8660254037844387076, 1.000000000000000000, 0.8660254037844207220, 1.000000000000017986 ) ) 
 REPRESENTATION_ITEM ( '' )  );
#4595 = CARTESIAN_POINT ( 'NONE',  ( -9.999999999999998224, 1.224646799147353059E-15, -191.7500000000000000 ) ) ;
#4596 = CARTESIAN_POINT ( 'NONE',  ( -2.293366432827344421E-15, -12.48450537969573659, -156.4062500020483810 ) ) ;
#4597 = CARTESIAN_POINT ( 'NONE',  ( 5.405949406249992428, -9.363379034771808662, -126.0937500020483668 ) ) ;
#4598 = CARTESIAN_POINT ( 'NONE',  ( 5.000000000000000000, 8.660254037844385522, -190.7500000000000000 ) ) ;
#4599 = VERTEX_POINT ( 'NONE', #1031 ) ;
#4600 = CARTESIAN_POINT ( 'NONE',  ( 7.070501591499376803E-16, 11.54700538379251284, -22.62499999999997868 ) ) ;
#4601 = ORIENTED_EDGE ( 'NONE', *, *, #32446, .F. ) ;
#4602 = ORGANIZATION ( 'NAUO-ORG5', 'UNSPECIFIED', 'UNSPECIFIED' ) ;
#4603 = EDGE_CURVE ( 'NONE', #27698, #42437, #8601, .T. ) ;
#4604 = ORIENTED_EDGE ( 'NONE', *, *, #19687, .F. ) ;
#4606 = VERTEX_POINT ( 'NONE', #34270 ) ;
#4605 = CARTESIAN_POINT ( 'NONE',  ( -5.405949406250003975, -9.363379034771801557, -109.8437500020483810 ) ) ;
#4607 = CARTESIAN_POINT ( 'NONE',  ( -5.321294541346989426, -5.321294541346989426, -219.9999999999999716 ) ) ;
#4608 = CARTESIAN_POINT ( 'NONE',  ( 10.81189881249999551, -6.242252689847874514, -185.9687500020484094 ) ) ;
#4609 = CARTESIAN_POINT ( 'NONE',  ( -5.405949406249996869, 9.363379034771805109, -41.34375000204837391 ) ) ;
#4610 = CARTESIAN_POINT ( 'NONE',  ( 0.3998884125188737482, -10.45061954883015254, 8.157905031340238759E-16 ) ) ;
#4611 = CARTESIAN_POINT ( 'NONE',  ( -9.999999999999998224, 1.224646799147353059E-15, -174.1250000040968189 ) ) ;
#4612 = CARTESIAN_POINT ( 'NONE',  ( 10.81189881249999729, 6.242252689847867408, -175.2187500020484094 ) ) ;
#4613 = CARTESIAN_POINT ( 'NONE',  ( -10.81189881249999907, -6.242252689847864744, -163.9687500020484094 ) ) ;
#4614 = CARTESIAN_POINT ( 'NONE',  ( 10.81189881249999907, 6.242252689847868297, -140.7187500020483810 ) ) ;
#4615 = CARTESIAN_POINT ( 'NONE',  ( 10.81189881249999729, 0.000000000000000000, -148.5312500020483810 ) ) ;
#4616 = CARTESIAN_POINT ( 'NONE',  ( 5.405949406249999534, 9.363379034771803333, -151.0937500020483810 ) ) ;
#4617 = CARTESIAN_POINT ( 'NONE',  ( 9.999999999999998224, 0.000000000000000000, -74.37500000409677625 ) ) ;
#4618 = CARTESIAN_POINT ( 'NONE',  ( -2.121150477449813534E-15, -11.54700538379251284, -182.3750000000000000 ) ) ;
#4619 = CARTESIAN_POINT ( 'NONE',  ( -5.405949406249996869, 9.363379034771805109, -87.84375000204836681 ) ) ;
#4620 = CARTESIAN_POINT ( 'NONE',  ( 10.00000000000025402, -5.773502691896113426, -135.6250000000000000 ) ) ;
#4621 = CARTESIAN_POINT ( 'NONE',  ( 5.405949406249999534, 9.363379034771803333, -61.28125000204837391 ) ) ;
#4622 = CARTESIAN_POINT ( 'NONE',  ( 9.999999999999872102, 5.773502691896329253, -168.7500000040967905 ) ) ;
#4623 = CARTESIAN_POINT ( 'NONE',  ( 10.81189881249999729, 0.000000000000000000, -175.3437500020483810 ) ) ;
#4624 = CARTESIAN_POINT ( 'NONE',  ( 5.405949406249999534, 9.363379034771803333, -112.2812500020483952 ) ) ;
#4625 = CARTESIAN_POINT ( 'NONE',  ( -10.81189881249999729, 1.324075727343319199E-15, -150.7812500020483810 ) ) ;
#4626 = DIRECTION ( 'NONE',  ( -1.000000000000000000, 0.000000000000000000, 0.000000000000000000 ) ) ;
#4627 = CARTESIAN_POINT ( 'NONE',  ( -10.81189881249999729, 1.324075727343319199E-15, -44.28125000204838102 ) ) ;
#4628 = CARTESIAN_POINT ( 'NONE',  ( 7.070501591499377789E-16, 11.54700538379251284, -126.5000000040967905 ) ) ;
#4629 = CARTESIAN_POINT ( 'NONE',  ( 9.999999999999996447, -5.773502691896262640, -107.1249999999999858 ) ) ;
#4630 = ORIENTED_EDGE ( 'NONE', *, *, #41333, .T. ) ;
#4631 = CARTESIAN_POINT ( 'NONE',  ( -2.293366432827344421E-15, -12.48450537969573659, -127.9062500020483952 ) ) ;
#4632 = CARTESIAN_POINT ( 'NONE',  ( 5.000000000000000000, 8.660254037844385522, -144.6250000040967905 ) ) ;
#4633 = FACE_OUTER_BOUND ( 'NONE', #42222, .T. ) ;
#4634 = CARTESIAN_POINT ( 'NONE',  ( 5.405949406249999534, 9.363379034771803333, -184.2812500020484094 ) ) ;
#4635 = ORIENTED_EDGE ( 'NONE', *, *, #18426, .F. ) ;
#4636 = CARTESIAN_POINT ( 'NONE',  ( -4.999999999999996447, 8.660254037844387298, -52.49999999999996447 ) ) ;
#4637 = CARTESIAN_POINT ( 'NONE',  ( -5.405949406250003975, -9.363379034771801557, -169.8437500020484094 ) ) ;
#4638 = CARTESIAN_POINT ( 'NONE',  ( -10.00000000000000000, -5.773502691896251982, -55.50000000409678336 ) ) ;
#4639 = CARTESIAN_POINT ( 'NONE',  ( -9.999999999999998224, 1.224646799147353059E-15, -49.62500000409675494 ) ) ;
#4640 = CARTESIAN_POINT ( 'NONE',  ( 9.999999999999998224, 0.000000000000000000, -171.8750000040968189 ) ) ;
#4641 = CARTESIAN_POINT ( 'NONE',  ( 5.405949406249992428, -9.363379034771808662, -64.78125000204838102 ) ) ;
#4642 = CARTESIAN_POINT ( 'NONE',  ( -10.81189881249999729, 1.324075727343319199E-15, -53.28125000204836681 ) ) ;
#4643 = CARTESIAN_POINT ( 'NONE',  ( 9.999999999999998224, 0.000000000000000000, -50.37500000409675494 ) ) ;
#4644 = CARTESIAN_POINT ( 'NONE',  ( 10.81189881249999907, 6.242252689847868297, -2.718750002048353043 ) ) ;
#4645 = CARTESIAN_POINT ( 'NONE',  ( 7.070501591499376803E-16, 11.54700538379251284, -158.0000000040968189 ) ) ;
#4646 = CARTESIAN_POINT ( 'NONE',  ( -10.81189881249999729, 1.324075727343319199E-15, -180.7812500020484094 ) ) ;
#4647 = ADVANCED_FACE ( 'NONE', ( #37488 ), #40281, .T. ) ;
#4648 = DIRECTION ( 'NONE',  ( -1.000000000000000000, 0.000000000000000000, 0.000000000000000000 ) ) ;
#4649 = CARTESIAN_POINT ( 'NONE',  ( 4.999999999999992006, -8.660254037844389075, -103.1250000040967763 ) ) ;
#4650 = CARTESIAN_POINT ( 'NONE',  ( 7.071067811865472841, 7.071067811865472841, -200.0000000000000000 ) ) ;
#4651 = CARTESIAN_POINT ( 'NONE',  ( 9.999999999999998224, 0.000000000000000000, -162.8750000040967905 ) ) ;
#4653 = ORIENTED_EDGE ( 'NONE', *, *, #41203, .T. ) ;
#4652 = CARTESIAN_POINT ( 'NONE',  ( 10.81189881249999907, 6.242252689847868297, -88.40625000204839523 ) ) ;
#4655 = VERTEX_POINT ( 'NONE', #14154 ) ;
#4654 = CARTESIAN_POINT ( 'NONE',  ( -7.071067811865477282, -7.071067811865472841, -200.0000000000000000 ) ) ;
#4656 = ORIENTED_EDGE ( 'NONE', *, *, #17738, .F. ) ;
#4657 = CARTESIAN_POINT ( 'NONE',  ( 10.81189881249999729, 6.242252689847867408, -35.71875000204835260 ) ) ;
#4658 = CARTESIAN_POINT ( 'NONE',  ( -5.405949406250003975, -9.363379034771801557, -24.34375000204835970 ) ) ;
#4659 = CARTESIAN_POINT ( 'NONE',  ( 7.644554776091147741E-16, 12.48450537969573659, -16.15625000204837747 ) ) ;
#4660 = CARTESIAN_POINT ( 'NONE',  ( 5.405949406249999534, 9.363379034771803333, -65.59375000204836681 ) ) ;
#4661 = DIRECTION ( 'NONE',  ( -0.000000000000000000, -0.000000000000000000, 1.000000000000000000 ) ) ;
#4662 = CARTESIAN_POINT ( 'NONE',  ( -9.999999999999998224, 5.773502691896259087, -46.37499999999996447 ) ) ;
#4663 = CARTESIAN_POINT ( 'NONE',  ( 10.81189881249999907, 6.242252689847868297, -185.7187500020483810 ) ) ;
#4664 = CARTESIAN_POINT ( 'NONE',  ( 10.81189881249999551, -6.242252689847874514, -164.9687500020484094 ) ) ;
#4665 = CARTESIAN_POINT ( 'NONE',  ( 8.614196012144985204, -6.533971456632194474, -179.9999999999999716 ) ) ;
#4666 = CARTESIAN_POINT ( 'NONE',  ( 5.000000000000000000, 8.660254037844385522, -199.7500000000000000 ) ) ;
#4667 = CYLINDRICAL_SURFACE ( 'NONE', #25390, 9.999999999999998224 ) ;
#4668 = FACE_OUTER_BOUND ( 'NONE', #38926, .T. ) ;
#4669 = CARTESIAN_POINT ( 'NONE',  ( -9.999999999999998224, 1.224646799147353059E-15, -175.2500000000000284 ) ) ;
#4670 = CARTESIAN_POINT ( 'NONE',  ( 5.405949406249999534, 9.363379034771803333, -113.5937500020483810 ) ) ;
#4671 = CARTESIAN_POINT ( 'NONE',  ( 9.999999999999998224, 0.000000000000000000, -18.87500000409675494 ) ) ;
#4672 = VECTOR ( 'NONE', #37576, 1000.000000000000114 ) ;
#4673 = CARTESIAN_POINT ( 'NONE',  ( -10.81189881249999729, 1.324075727343319199E-15, -86.28125000204838102 ) ) ;
#4674 = CARTESIAN_POINT ( 'NONE',  ( 10.81189881249999551, -6.242252689847874514, -100.4687500020483952 ) ) ;
#4675 = VECTOR ( 'NONE', #26378, 1000.000000000000000 ) ;
#4676 =( BOUNDED_CURVE ( )  B_SPLINE_CURVE ( 2, ( #18230, #37670, #17798, #17368, #27319, #4438, #21475 ),
 .UNSPECIFIED., .F., .F. ) 
 B_SPLINE_CURVE_WITH_KNOTS ( ( 3, 2, 2, 3 ),
 ( 0.4626865671641792743, 0.4639303482587066596, 0.4651741293532339339, 0.4664179104477613191 ),
 .UNSPECIFIED. ) 
 CURVE ( )  GEOMETRIC_REPRESENTATION_ITEM ( )  RATIONAL_B_SPLINE_CURVE ( ( 0.9999999999999820144, 0.8660254037844566932, 1.000000000000000000, 0.8660254037844387076, 1.000000000000000000, 0.8660254037844267172, 1.000000000000011990 ) ) 
 REPRESENTATION_ITEM ( '' )  );
#4677 = CARTESIAN_POINT ( 'NONE',  ( -10.81189881249999907, -6.242252689847864744, -63.46875000204838102 ) ) ;
#4678 = CARTESIAN_POINT ( 'NONE',  ( 10.81189881249999729, 0.000000000000000000, -67.53125000204838102 ) ) ;
#4679 = CARTESIAN_POINT ( 'NONE',  ( 5.000000000000000000, 8.660254037844385522, -150.6250000040967905 ) ) ;
#4680 = CARTESIAN_POINT ( 'NONE',  ( -4.999999999999996447, 8.660254037844387298, -130.5000000000000000 ) ) ;
#4681 = CARTESIAN_POINT ( 'NONE',  ( 10.81189881249999729, 0.000000000000000000, -147.0312500020483810 ) ) ;
#4682 = CARTESIAN_POINT ( 'NONE',  ( -10.81189881249999907, -6.242252689847864744, -161.1562500020484094 ) ) ;
#4683 = DIRECTION ( 'NONE',  ( -1.000000000000000000, 0.000000000000000000, 0.000000000000000000 ) ) ;
#4684 = CARTESIAN_POINT ( 'NONE',  ( -4.999999999999996447, 8.660254037844387298, -172.5000000000000284 ) ) ;
#4685 = CARTESIAN_POINT ( 'NONE',  ( 10.81189881249999729, 0.000000000000000000, -101.8437500020483810 ) ) ;
#4686 = CARTESIAN_POINT ( 'NONE',  ( 4.999999999999992006, -8.660254037844389075, -77.24999999999998579 ) ) ;
#4687 = CARTESIAN_POINT ( 'NONE',  ( 5.405949406249992428, -9.363379034771808662, -7.781250002048350822 ) ) ;
#4688 = CARTESIAN_POINT ( 'NONE',  ( -9.999999999999998224, 5.773502691896259087, -81.25000000409677625 ) ) ;
#4689 = CARTESIAN_POINT ( 'NONE',  ( 8.614196012144985204, -6.533971456632194474, -180.0000000000000000 ) ) ;
#4690 = CARTESIAN_POINT ( 'NONE',  ( -10.81189881249999907, -6.242252689847864744, -99.65625000204839523 ) ) ;
#4691 = CARTESIAN_POINT ( 'NONE',  ( -2.293366432827344421E-15, -12.48450537969573659, -78.40625000204838102 ) ) ;
#4692 = CARTESIAN_POINT ( 'NONE',  ( 9.999999999999998224, 0.000000000000000000, -75.87500000409677625 ) ) ;
#4693 = CARTESIAN_POINT ( 'NONE',  ( 9.999999999999479527, 5.773502691896553074, -118.8749999999999858 ) ) ;
#4694 = CARTESIAN_POINT ( 'NONE',  ( -5.405949406249996869, 9.363379034771805109, -36.84375000204836681 ) ) ;
#4695 = VERTEX_POINT ( 'NONE', #23915 ) ;
#4696 = CARTESIAN_POINT ( 'NONE',  ( 5.000000000000000000, 8.660254037844385522, -1.749999999999973799 ) ) ;
#4697 = CARTESIAN_POINT ( 'NONE',  ( -10.81189881249999729, 1.324075727343319199E-15, -27.78125000204837036 ) ) ;
#4698 = CARTESIAN_POINT ( 'NONE',  ( 5.405949406249992428, -9.363379034771808662, -12.09375000204834727 ) ) ;
#4699 = CARTESIAN_POINT ( 'NONE',  ( -4.999999999999996447, 8.660254037844387298, -7.875000004096744277 ) ) ;
#4700 = CARTESIAN_POINT ( 'NONE',  ( 10.81189881249999907, 6.242252689847868297, -131.9062500020484094 ) ) ;
#4701 = CARTESIAN_POINT ( 'NONE',  ( 9.999999999999996447, -5.773502691896262640, -182.1250000000000000 ) ) ;
#4702 = DIRECTION ( 'NONE',  ( -0.000000000000000000, -0.000000000000000000, 1.000000000000000000 ) ) ;
#4704 = ORIENTED_EDGE ( 'NONE', *, *, #10791, .T. ) ;
#4703 = CARTESIAN_POINT ( 'NONE',  ( -5.405949406250003975, -9.363379034771801557, -108.5312500020483810 ) ) ;
#4705 = CARTESIAN_POINT ( 'NONE',  ( 5.000000000000000000, 8.660254037844385522, -138.6250000040967905 ) ) ;
#4706 = AXIS2_PLACEMENT_3D ( 'NONE', #9135, #12566, #5260 ) ;
#4707 = ORIENTED_EDGE ( 'NONE', *, *, #1065, .F. ) ;
#4708 = ORIENTED_EDGE ( 'NONE', *, *, #42274, .F. ) ;
#4709 = EDGE_CURVE ( 'NONE', #22217, #29348, #22078, .T. ) ;
#4710 = CARTESIAN_POINT ( 'NONE',  ( 5.405949406249992428, -9.363379034771808662, -36.28125000204837391 ) ) ;
#4711 = PERSON_AND_ORGANIZATION_ROLE ( 'classification_officer' ) ;
#4712 = CARTESIAN_POINT ( 'NONE',  ( -5.405949406250003975, -9.363379034771801557, -84.34375000204836681 ) ) ;
#4713 = DIRECTION ( 'NONE',  ( -0.000000000000000000, -0.000000000000000000, 1.000000000000000000 ) ) ;
#4714 = CYLINDRICAL_SURFACE ( 'NONE', #464, 9.999999999999998224 ) ;
#4715 =( BOUNDED_CURVE ( )  B_SPLINE_CURVE ( 2, ( #31853, #8328, #28606, #35082, #38094, #14766, #27962 ),
 .UNSPECIFIED., .F., .F. ) 
 B_SPLINE_CURVE_WITH_KNOTS ( ( 3, 2, 2, 3 ),
 ( 0.9029850746268659467, 0.9042288557213932210, 0.9054726368159207173, 0.9067164179104481025 ),
 .UNSPECIFIED. ) 
 CURVE ( )  GEOMETRIC_REPRESENTATION_ITEM ( )  RATIONAL_B_SPLINE_CURVE ( ( 0.9999999999999761302, 0.8660254037844625774, 1.000000000000000000, 0.8660254037844387076, 1.000000000000000000, 0.8660254037844028474, 1.000000000000035971 ) ) 
 REPRESENTATION_ITEM ( '' )  );
#4716 = CARTESIAN_POINT ( 'NONE',  ( -9.999999999999998224, 1.224646799147353059E-15, -167.7500000000000000 ) ) ;
#4717 = CARTESIAN_POINT ( 'NONE',  ( 5.405949406249999534, 9.363379034771803333, -167.7812500020484094 ) ) ;
#4718 = CARTESIAN_POINT ( 'NONE',  ( 10.00000000000102318, -5.773502691895667560, -68.12499999999995737 ) ) ;
#4719 = CARTESIAN_POINT ( 'NONE',  ( -5.405949406250003975, -9.363379034771801557, -126.3437500020483952 ) ) ;
#4720 = CARTESIAN_POINT ( 'NONE',  ( 7.644554776091147741E-16, 12.48450537969573659, -89.46875000204838102 ) ) ;
#4721 = CARTESIAN_POINT ( 'NONE',  ( -2.293366432827344421E-15, -12.48450537969573659, -0.4062500020483658103 ) ) ;
#4722 = CARTESIAN_POINT ( 'NONE',  ( -10.81189881249999729, 6.242252689847871849, -197.2187500020484379 ) ) ;
#4723 = CARTESIAN_POINT ( 'NONE',  ( -10.81189881249999729, 1.324075727343319199E-15, -104.2812500020483810 ) ) ;
#4724 = CARTESIAN_POINT ( 'NONE',  ( -2.121150477449813534E-15, -11.54700538379251284, -176.7500000040967620 ) ) ;
#4725 = CARTESIAN_POINT ( 'NONE',  ( -10.81189881249999729, -6.242252689847864744, -103.9687500020483810 ) ) ;
#4726 = CARTESIAN_POINT ( 'NONE',  ( -10.81189881249999729, -6.242252689847864744, -179.1562500020484094 ) ) ;
#4727 =( BOUNDED_CURVE ( )  B_SPLINE_CURVE ( 2, ( #9062, #42480, #9266, #3015, #35822, #2387, #19399 ),
 .UNSPECIFIED., .F., .F. ) 
 B_SPLINE_CURVE_WITH_KNOTS ( ( 3, 2, 2, 3 ),
 ( 0.3917910447761194792, 0.3930348258706468090, 0.3942786069651742498, 0.3955223880597015795 ),
 .UNSPECIFIED. ) 
 CURVE ( )  GEOMETRIC_REPRESENTATION_ITEM ( )  RATIONAL_B_SPLINE_CURVE ( ( 0.9999999999999940048, 0.8660254037844447028, 1.000000000000000000, 0.8660254037844387076, 1.000000000000000000, 0.8660254037844267172, 1.000000000000011990 ) ) 
 REPRESENTATION_ITEM ( '' )  );
#4728 = CARTESIAN_POINT ( 'NONE',  ( -9.999999999999998224, 1.224646799147353059E-15, -70.62500000409677625 ) ) ;
#4729 = CARTESIAN_POINT ( 'NONE',  ( -9.999999999999998224, 1.224646799147353059E-15, -124.6250000040967763 ) ) ;
#4730 = CARTESIAN_POINT ( 'NONE',  ( -10.81189881249999729, 6.242252689847871849, -194.4062500020484094 ) ) ;
#4731 = CARTESIAN_POINT ( 'NONE',  ( -2.293366432827344421E-15, -12.48450537969573659, -48.21875000204836681 ) ) ;
#4732 = EDGE_CURVE ( 'NONE', #35021, #13374, #8855, .T. ) ;
#4733 = CARTESIAN_POINT ( 'NONE',  ( 10.00000000000000000, 5.773502691896255534, -170.2500000040967905 ) ) ;
#4734 = CARTESIAN_POINT ( 'NONE',  ( 5.405949406249999534, 9.363379034771803333, -13.28125000204835615 ) ) ;
#4735 = CARTESIAN_POINT ( 'NONE',  ( -2.293366432827344421E-15, -12.48450537969573659, -25.71875000204837391 ) ) ;
#4736 = CARTESIAN_POINT ( 'NONE',  ( 9.999999999999998224, 0.000000000000000000, -192.8750000040967905 ) ) ;
#4737 = CARTESIAN_POINT ( 'NONE',  ( 10.81189881249999729, 0.000000000000000000, -128.8437500020484094 ) ) ;
#4738 = CARTESIAN_POINT ( 'NONE',  ( 9.999999999999998224, 0.000000000000000000, -97.99999999999998579 ) ) ;
#4739 = CARTESIAN_POINT ( 'NONE',  ( 5.405949406249992428, -9.363379034771808662, -25.78125000204836681 ) ) ;
#4740 = CARTESIAN_POINT ( 'NONE',  ( -9.999999999999998224, 1.224646799147353059E-15, -109.6250000040967763 ) ) ;
#4741 = FACE_OUTER_BOUND ( 'NONE', #36183, .T. ) ;
#4742 = CARTESIAN_POINT ( 'NONE',  ( -9.999999999999998224, 1.224646799147353059E-15, -52.24999999999996447 ) ) ;
#4743 = CARTESIAN_POINT ( 'NONE',  ( -10.81189881249999729, 1.324075727343319199E-15, -122.2812500020483952 ) ) ;
#4744 = CARTESIAN_POINT ( 'NONE',  ( -5.405949406249996869, 9.363379034771805109, -103.0312500020483952 ) ) ;
#4745 = VERTEX_POINT ( 'NONE', #30602 ) ;
#4746 = CARTESIAN_POINT ( 'NONE',  ( -10.00000000000000000, -5.773502691896251982, -100.5000000040967905 ) ) ;
#4747 = CARTESIAN_POINT ( 'NONE',  ( -5.000000000000003553, -8.660254037844383745, -113.4999999999999858 ) ) ;
#4748 = CARTESIAN_POINT ( 'NONE',  ( -10.81189881249999907, -6.242252689847864744, -165.6562500020483810 ) ) ;
#4749 = CARTESIAN_POINT ( 'NONE',  ( -10.81189881249999729, 6.242252689847871849, -54.71875000204837391 ) ) ;
#4750 = VERTEX_POINT ( 'NONE', #7719 ) ;
#4751 = CARTESIAN_POINT ( 'NONE',  ( 7.070501591499377789E-16, 11.54700538379251284, -22.62499999999997868 ) ) ;
#4752 = CARTESIAN_POINT ( 'NONE',  ( -5.405949406250003975, -9.363379034771801557, -35.03125000204837391 ) ) ;
#4753 = CARTESIAN_POINT ( 'NONE',  ( 9.999999999999998224, 0.000000000000000000, -165.5000000000000000 ) ) ;
#4754 = DIRECTION ( 'NONE',  ( -0.000000000000000000, -0.000000000000000000, 1.000000000000000000 ) ) ;
#4755 = CARTESIAN_POINT ( 'NONE',  ( -4.999999999999996447, 8.660254037844387298, -28.87500000409676204 ) ) ;
#4756 = CARTESIAN_POINT ( 'NONE',  ( 9.999999999999998224, 0.000000000000000000, -168.5000000000000000 ) ) ;
#4757 = CARTESIAN_POINT ( 'NONE',  ( 7.644554776091147741E-16, 12.48450537969573659, -130.1562500020483810 ) ) ;
#4758 = CARTESIAN_POINT ( 'NONE',  ( 5.000000000000000000, 8.660254037844385522, -46.74999999999998579 ) ) ;
#4759 = CARTESIAN_POINT ( 'NONE',  ( -5.000000000000003553, -8.660254037844383745, -119.8750000040967905 ) ) ;
#4760 = VERTEX_POINT ( 'NONE', #17615 ) ;
#4761 = CARTESIAN_POINT ( 'NONE',  ( 10.81189881249999729, 0.000000000000000000, -61.53125000204837391 ) ) ;
#4762 = EDGE_CURVE ( 'NONE', #24456, #35132, #10210, .T. ) ;
#4764 = VERTEX_POINT ( 'NONE', #4473 ) ;
#4763 = ORIENTED_EDGE ( 'NONE', *, *, #9324, .F. ) ;
#4765 = DIRECTION ( 'NONE',  ( -0.000000000000000000, -0.000000000000000000, -1.000000000000000000 ) ) ;
#4766 = CARTESIAN_POINT ( 'NONE',  ( 9.999999999999998224, 0.000000000000000000, -174.8750000040967905 ) ) ;
#4767 = CARTESIAN_POINT ( 'NONE',  ( 7.644554776091147741E-16, 12.48450537969573659, -168.9687500020483810 ) ) ;
#4768 = CARTESIAN_POINT ( 'NONE',  ( -5.405949406250003975, -9.363379034771801557, -188.0312500020484094 ) ) ;
#4769 = CARTESIAN_POINT ( 'NONE',  ( 5.405949406249999534, 9.363379034771803333, -11.59375000204834727 ) ) ;
#4770 = AXIS2_PLACEMENT_3D ( 'NONE', #7078, #13730, #17401 ) ;
#4771 = CARTESIAN_POINT ( 'NONE',  ( 5.000000000000000000, 8.660254037844385522, -129.2499999999999716 ) ) ;
#4772 = CARTESIAN_POINT ( 'NONE',  ( -5.405949406250003975, -9.363379034771801557, -151.8437500020483810 ) ) ;
#4773 = CARTESIAN_POINT ( 'NONE',  ( -5.405949406249996869, 9.363379034771805109, -125.3437500020483952 ) ) ;
#4774 = CARTESIAN_POINT ( 'NONE',  ( 5.405949406249999534, 9.363379034771803333, -107.7812500020483810 ) ) ;
#4775 = CARTESIAN_POINT ( 'NONE',  ( -2.293366432827344421E-15, -12.48450537969573659, -121.7187500020483952 ) ) ;
#4776 = CARTESIAN_POINT ( 'NONE',  ( 7.644554776091147741E-16, 12.48450537969573659, 0.5312499979516493998 ) ) ;
#4777 = CARTESIAN_POINT ( 'NONE',  ( 5.405949406249992428, -9.363379034771808662, -126.2812500020483668 ) ) ;
#4778 = CARTESIAN_POINT ( 'NONE',  ( 10.81189881249999551, -6.242252689847874514, 0.03124999795165228286 ) ) ;
#4779 = CARTESIAN_POINT ( 'NONE',  ( -5.405949406250003975, -9.363379034771801557, -130.8437500020484094 ) ) ;
#4780 = CARTESIAN_POINT ( 'NONE',  ( -99.99999999999994316, 19.99999999999998934, -160.0000000000000000 ) ) ;
#4781 = CARTESIAN_POINT ( 'NONE',  ( 10.00000000000006040, -5.773502691896226224, -196.0000000040968473 ) ) ;
#4782 = CARTESIAN_POINT ( 'NONE',  ( -4.999999999999996447, 8.660254037844387298, -150.0000000000000000 ) ) ;
#4783 = CARTESIAN_POINT ( 'NONE',  ( -4.999999999999996447, 8.660254037844387298, -20.99999999999996447 ) ) ;
#4784 = CARTESIAN_POINT ( 'NONE',  ( -5.405949406250003975, -9.363379034771801557, -75.34375000204838102 ) ) ;
#4785 = CARTESIAN_POINT ( 'NONE',  ( -10.81189881249999729, 6.242252689847871849, -65.21875000204838102 ) ) ;
#4786 = CARTESIAN_POINT ( 'NONE',  ( 4.999999999999992006, -8.660254037844389075, -170.2500000000000000 ) ) ;
#4787 = CARTESIAN_POINT ( 'NONE',  ( -10.81189881249999907, -6.242252689847864744, -32.15625000204835970 ) ) ;
#4788 = CARTESIAN_POINT ( 'NONE',  ( 5.405949406249992428, -9.363379034771808662, -43.59375000204837391 ) ) ;
#4789 = DIRECTION ( 'NONE',  ( -0.000000000000000000, -0.000000000000000000, -1.000000000000000000 ) ) ;
#4790 = CARTESIAN_POINT ( 'NONE',  ( 10.81189881249999729, 0.000000000000000000, -154.3437500020483810 ) ) ;
#4791 = CARTESIAN_POINT ( 'NONE',  ( 10.00000000000000000, 5.773502691896255534, -123.3749999999999858 ) ) ;
#4792 = CARTESIAN_POINT ( 'NONE',  ( 10.81189881249999729, 6.242252689847867408, -130.4062500020483810 ) ) ;
#4793 = CARTESIAN_POINT ( 'NONE',  ( -5.000000000000003553, -8.660254037844383745, -67.37500000409676204 ) ) ;
#4794 = CARTESIAN_POINT ( 'NONE',  ( 7.070501591499377789E-16, 11.54700538379251284, -76.62499999999997158 ) ) ;
#4795 = CARTESIAN_POINT ( 'NONE',  ( 10.81189881249999551, -6.242252689847874514, -21.15625000204836681 ) ) ;
#4796 = EDGE_LOOP ( 'NONE', ( #13179, #1194, #23884, #1624 ) ) ;
#4797 = CARTESIAN_POINT ( 'NONE',  ( 10.81189881249999729, 0.000000000000000000, -102.0312500020483952 ) ) ;
#4798 = CARTESIAN_POINT ( 'NONE',  ( 7.070501591499377789E-16, 11.54700538379251284, -122.0000000040967905 ) ) ;
#4799 = CARTESIAN_POINT ( 'NONE',  ( 4.999999999999992006, -8.660254037844389075, -154.1250000040967905 ) ) ;
#4800 = CARTESIAN_POINT ( 'NONE',  ( -5.000000000000003553, -8.660254037844383745, -34.37500000409676915 ) ) ;
#4801 =( BOUNDED_CURVE ( )  B_SPLINE_CURVE ( 2, ( #14104, #23437, #7451, #7237, #10250, #16929, #4425 ),
 .UNSPECIFIED., .F., .F. ) 
 B_SPLINE_CURVE_WITH_KNOTS ( ( 3, 2, 2, 3 ),
 ( 0.4440298507462688282, 0.4452736318407962135, 0.4465174129353234878, 0.4477611940298508730 ),
 .UNSPECIFIED. ) 
 CURVE ( )  GEOMETRIC_REPRESENTATION_ITEM ( )  RATIONAL_B_SPLINE_CURVE ( ( 0.9999999999999820144, 0.8660254037844566932, 1.000000000000000000, 0.8660254037844387076, 1.000000000000000000, 0.8660254037844267172, 1.000000000000011990 ) ) 
 REPRESENTATION_ITEM ( '' )  );
#4802 = CARTESIAN_POINT ( 'NONE',  ( 9.999999999999998224, 0.000000000000000000, -149.0000000000000000 ) ) ;
#4803 = CARTESIAN_POINT ( 'NONE',  ( 7.644554776091147741E-16, 12.48450537969573659, -44.65625000204836681 ) ) ;
#4804 = CARTESIAN_POINT ( 'NONE',  ( 9.999999999999998224, 0.000000000000000000, -191.0000000000000000 ) ) ;
#4805 = CARTESIAN_POINT ( 'NONE',  ( -10.81189881249999907, -6.242252689847864744, -153.6562500020484094 ) ) ;
#4806 = AXIS2_PLACEMENT_3D ( 'NONE', #42161, #19286, #18654 ) ;
#4807 = CARTESIAN_POINT ( 'NONE',  ( -5.405949406250003975, -9.363379034771801557, -126.3437500020483952 ) ) ;
#4808 = CARTESIAN_POINT ( 'NONE',  ( -4.999999999999996447, 8.660254037844387298, -109.4999999999999858 ) ) ;
#4809 = ORIENTED_EDGE ( 'NONE', *, *, #22059, .T. ) ;
#4810 = DIRECTION ( 'NONE',  ( -0.000000000000000000, -0.000000000000000000, 1.000000000000000000 ) ) ;
#4811 = ORIENTED_EDGE ( 'NONE', *, *, #24808, .T. ) ;
#4812 = EDGE_CURVE ( 'NONE', #31374, #5830, #27784, .T. ) ;
#4813 = ORIENTED_EDGE ( 'NONE', *, *, #14906, .T. ) ;
#4814 = EDGE_CURVE ( 'NONE', #6986, #3969, #27624, .T. ) ;
#4815 = ORIENTED_EDGE ( 'NONE', *, *, #26459, .T. ) ;
#4816 = EDGE_CURVE ( 'NONE', #28591, #27752, #8695, .T. ) ;
#4817 = ADVANCED_FACE ( 'NONE', ( #36770 ), #7003, .T. ) ;
#4818 = CARTESIAN_POINT ( 'NONE',  ( -10.81189881249999907, -6.242252689847864744, -190.9687500020484379 ) ) ;
#4819 = CARTESIAN_POINT ( 'NONE',  ( -10.81189881249999729, 6.242252689847871849, -38.21875000204836681 ) ) ;
#4820 = CARTESIAN_POINT ( 'NONE',  ( 4.168882320602625313, -9.758565647681585631, 6.544024882825217862E-15 ) ) ;
#4821 = CARTESIAN_POINT ( 'NONE',  ( 7.070501591499376803E-16, 11.54700538379251284, -139.6250000000000000 ) ) ;
#4822 = CARTESIAN_POINT ( 'NONE',  ( -5.405949406250003975, -9.363379034771801557, -174.3437500020484094 ) ) ;
#4823 = CARTESIAN_POINT ( 'NONE',  ( 10.81189881249999907, 6.242252689847868297, -164.7187500020483810 ) ) ;
#4824 = CC_DESIGN_PERSON_AND_ORGANIZATION_ASSIGNMENT ( #14625, #11389, ( #18005 ) ) ;
#4825 = DIRECTION ( 'NONE',  ( -0.000000000000000000, -1.000000000000000000, -0.000000000000000000 ) ) ;
#4826 = CARTESIAN_POINT ( 'NONE',  ( 10.81189881249999729, 0.000000000000000000, -145.3437500020483810 ) ) ;
#4827 = CARTESIAN_POINT ( 'NONE',  ( -5.405949406249996869, 9.363379034771805109, -145.0312500020483810 ) ) ;
#4828 = CARTESIAN_POINT ( 'NONE',  ( 10.81189881249999729, 0.000000000000000000, -154.3437500020483810 ) ) ;
#4829 = CARTESIAN_POINT ( 'NONE',  ( 5.000000000000000000, 8.660254037844385522, -87.24999999999998579 ) ) ;
#4830 = DIRECTION ( 'NONE',  ( 0.000000000000000000, 0.000000000000000000, -1.000000000000000000 ) ) ;
#4831 = CARTESIAN_POINT ( 'NONE',  ( -9.999999999999998224, 5.773502691896259087, -175.3750000000000000 ) ) ;
#4832 = CARTESIAN_POINT ( 'NONE',  ( -5.405949406250003975, -9.363379034771801557, -91.84375000204838102 ) ) ;
#4833 = CARTESIAN_POINT ( 'NONE',  ( 4.999999999999992006, -8.660254037844389075, -82.12500000409676204 ) ) ;
#4834 = CARTESIAN_POINT ( 'NONE',  ( -10.81189881249999907, -6.242252689847864744, -56.15625000204837391 ) ) ;
#4835 = CARTESIAN_POINT ( 'NONE',  ( -8.865618880899917897, 5.969117493042149114, -99.99999999999998579 ) ) ;
#4836 = CARTESIAN_POINT ( 'NONE',  ( -5.405949406249996869, 9.363379034771805109, -176.3437500020483810 ) ) ;
#4837 = EDGE_CURVE ( 'NONE', #33095, #42590, #11595, .T. ) ;
#4838 = CARTESIAN_POINT ( 'NONE',  ( 7.644554776091147741E-16, 12.48450537969573659, -112.1562500020483810 ) ) ;
#4839 = CARTESIAN_POINT ( 'NONE',  ( 10.81189881249999729, 0.000000000000000000, -153.0312500020484094 ) ) ;
#4840 = DIRECTION ( 'NONE',  ( -0.000000000000000000, -0.000000000000000000, 1.000000000000000000 ) ) ;
#4841 = CARTESIAN_POINT ( 'NONE',  ( -10.81189881249999729, 1.324075727343319199E-15, -41.28125000204838102 ) ) ;
#4842 = CARTESIAN_POINT ( 'NONE',  ( -4.999999999999996447, 8.660254037844387298, -130.8750000040967905 ) ) ;
#4843 = CARTESIAN_POINT ( 'NONE',  ( 9.999999999999998224, 0.000000000000000000, -105.4999999999999858 ) ) ;
#4844 =( BOUNDED_CURVE ( )  B_SPLINE_CURVE ( 2, ( #28752, #36059, #28958, #29370, #9515, #15760, #16175 ),
 .UNSPECIFIED., .F., .F. ) 
 B_SPLINE_CURVE_WITH_KNOTS ( ( 3, 2, 2, 3 ),
 ( 0.9514925373134331954, 0.9527363184079605807, 0.9539800995024879660, 0.9552238805970153512 ),
 .UNSPECIFIED. ) 
 CURVE ( )  GEOMETRIC_REPRESENTATION_ITEM ( )  RATIONAL_B_SPLINE_CURVE ( ( 0.9999999999999641398, 0.8660254037844745678, 1.000000000000000000, 0.8660254037844387076, 1.000000000000000000, 0.8660254037843908570, 1.000000000000047740 ) ) 
 REPRESENTATION_ITEM ( '' )  );
#4845 = VERTEX_POINT ( 'NONE', #16898 ) ;
#4846 = CARTESIAN_POINT ( 'NONE',  ( -10.81189881249999729, 6.242252689847871849, -128.4062500020483810 ) ) ;
#4847 = CARTESIAN_POINT ( 'NONE',  ( -9.999999999999998224, 5.773502691896259087, -145.7500000040967905 ) ) ;
#4848 = CARTESIAN_POINT ( 'NONE',  ( 4.999999999999992006, -8.660254037844389075, -167.2500000000000000 ) ) ;
#4849 = EDGE_CURVE ( 'NONE', #33599, #11060, #30655, .T. ) ;
#4850 = CARTESIAN_POINT ( 'NONE',  ( 7.644554776091147741E-16, 12.48450537969573659, -184.1562500020484094 ) ) ;
#4851 = ORIENTED_EDGE ( 'NONE', *, *, #29617, .T. ) ;
#4852 = CARTESIAN_POINT ( 'NONE',  ( 10.81189881249999907, 6.242252689847868297, -172.2187500020483810 ) ) ;
#4853 = CARTESIAN_POINT ( 'NONE',  ( 9.999999999999996447, -5.773502691896262640, -59.50000000409676915 ) ) ;
#4854 = EDGE_CURVE ( 'NONE', #38736, #35715, #39464, .T. ) ;
#4855 = CARTESIAN_POINT ( 'NONE',  ( -9.999999999999998224, 1.224646799147353059E-15, -109.6250000040967763 ) ) ;
#4856 = CARTESIAN_POINT ( 'NONE',  ( 10.00000000000012790, 5.773502691896179151, -171.7500000040967620 ) ) ;
#4857 = CARTESIAN_POINT ( 'NONE',  ( 7.644554776091147741E-16, 12.48450537969573659, -71.65625000204836681 ) ) ;
#4858 = CARTESIAN_POINT ( 'NONE',  ( 10.81189881249999729, 6.242252689847867408, -49.40625000204837391 ) ) ;
#4859 = CARTESIAN_POINT ( 'NONE',  ( -2.121150477449813534E-15, -11.54700538379251284, -44.75000000409676204 ) ) ;
#4860 = CARTESIAN_POINT ( 'NONE',  ( -2.293366432827344421E-15, -12.48450537969573659, -4.718750002048355263 ) ) ;
#4861 = CARTESIAN_POINT ( 'NONE',  ( 31.99999999999997158, 0.000000000000000000, -180.0000000000000000 ) ) ;
#4862 = CARTESIAN_POINT ( 'NONE',  ( 5.405949406249992428, -9.363379034771808662, -175.7812500020484094 ) ) ;
#4863 = CARTESIAN_POINT ( 'NONE',  ( 9.999999999999479527, 5.773502691896553074, -147.7500000040967620 ) ) ;
#4864 = CARTESIAN_POINT ( 'NONE',  ( -9.999999999999998224, 1.224646799147353059E-15, -138.1250000040967620 ) ) ;
#4865 = ORIENTED_EDGE ( 'NONE', *, *, #21422, .T. ) ;
#4866 = DIRECTION ( 'NONE',  ( 0.000000000000000000, 0.000000000000000000, -1.000000000000000000 ) ) ;
#4867 = CARTESIAN_POINT ( 'NONE',  ( -9.999999999999998224, 1.224646799147353059E-15, -154.2500000000000000 ) ) ;
#4868 = CARTESIAN_POINT ( 'NONE',  ( -9.999999999999998224, 1.224646799147353059E-15, -1.249999999999973355 ) ) ;
#4870 = ORIENTED_EDGE ( 'NONE', *, *, #929, .F. ) ;
#4869 = CARTESIAN_POINT ( 'NONE',  ( -5.405949406250003975, -9.363379034771801557, -86.03125000204838102 ) ) ;
#4871 = AXIS2_PLACEMENT_3D ( 'NONE', #37827, #8698, #2434 ) ;
#4873 = VERTEX_POINT ( 'NONE', #1166 ) ;
#4872 = DIRECTION ( 'NONE',  ( -0.000000000000000000, -0.000000000000000000, 1.000000000000000000 ) ) ;
#4874 = ORIENTED_EDGE ( 'NONE', *, *, #35749, .T. ) ;
#4875 = EDGE_CURVE ( 'NONE', #39779, #4966, #14621, .T. ) ;
#4876 = CARTESIAN_POINT ( 'NONE',  ( -2.293366432827344421E-15, -12.48450537969573659, -34.71875000204835260 ) ) ;
#4877 = CARTESIAN_POINT ( 'NONE',  ( 10.81189881249999729, 0.000000000000000000, -23.84375000204835970 ) ) ;
#4878 = CARTESIAN_POINT ( 'NONE',  ( 10.81189881249999907, 6.242252689847868297, -14.90625000204837036 ) ) ;
#4881 = ADVANCED_FACE ( 'NONE', ( #3765 ), #40002, .T. ) ;
#4880 = VERTEX_POINT ( 'NONE', #24267 ) ;
#4879 = CARTESIAN_POINT ( 'NONE',  ( -5.405949406250003975, -9.363379034771801557, -63.34375000204836681 ) ) ;
#4882 = CARTESIAN_POINT ( 'NONE',  ( -9.999999999998969713, -5.773502691896847949, -131.6250000000000000 ) ) ;
#4883 = CARTESIAN_POINT ( 'NONE',  ( -9.999999999999998224, 1.224646799147353059E-15, -34.24999999999997158 ) ) ;
#4884 = CARTESIAN_POINT ( 'NONE',  ( 5.405949406249992428, -9.363379034771808662, -184.5937500020483810 ) ) ;
#4885 = CARTESIAN_POINT ( 'NONE',  ( -5.405949406249996869, 9.363379034771805109, -168.8437500020484094 ) ) ;
#4886 = CARTESIAN_POINT ( 'NONE',  ( 5.405949406249999534, 9.363379034771803333, -176.5937500020484094 ) ) ;
#4887 = CARTESIAN_POINT ( 'NONE',  ( 9.999999999999998224, 0.000000000000000000, -182.3750000040967905 ) ) ;
#4888 = CARTESIAN_POINT ( 'NONE',  ( -2.121150477449813534E-15, -11.54700538379251284, -167.7500000040968189 ) ) ;
#4889 = CARTESIAN_POINT ( 'NONE',  ( -10.00000000000076916, 5.773502691895813221, -103.7500000040967763 ) ) ;
#4890 = CARTESIAN_POINT ( 'NONE',  ( 0.000000000000000000, 0.000000000000000000, -200.0000000000000000 ) ) ;
#4891 = CARTESIAN_POINT ( 'NONE',  ( -10.81189881249999907, -6.242252689847864744, -115.9687500020483810 ) ) ;
#4892 = DIRECTION ( 'NONE',  ( -0.000000000000000000, -0.000000000000000000, 1.000000000000000000 ) ) ;
#4893 = CARTESIAN_POINT ( 'NONE',  ( -2.293366432827344421E-15, -12.48450537969573659, -84.40625000204838102 ) ) ;
#4894 = CARTESIAN_POINT ( 'NONE',  ( 10.81189881249999551, -6.242252689847874514, -88.46875000204836681 ) ) ;
#4895 = CARTESIAN_POINT ( 'NONE',  ( 5.405949406249992428, -9.363379034771808662, -61.59375000204836681 ) ) ;
#4896 = CARTESIAN_POINT ( 'NONE',  ( -5.405949406250003975, -9.363379034771801557, -69.53125000204838102 ) ) ;
#4897 = CARTESIAN_POINT ( 'NONE',  ( 9.999999999999998224, 0.000000000000000000, -156.8750000040967905 ) ) ;
#4898 = CARTESIAN_POINT ( 'NONE',  ( -5.000000000000003553, -8.660254037844383745, -128.5000000000000000 ) ) ;
#4899 = ADVANCED_FACE ( 'NONE', ( #37413 ), #14075, .T. ) ;
#4900 = CARTESIAN_POINT ( 'NONE',  ( 7.644554776091147741E-16, 12.48450537969573659, -154.1562500020484094 ) ) ;
#4901 = CARTESIAN_POINT ( 'NONE',  ( 5.405949406249999534, 9.363379034771803333, -161.7812500020484094 ) ) ;
#4902 = CC_DESIGN_APPROVAL ( #19877, ( #10394 ) ) ;
#4903 = CARTESIAN_POINT ( 'NONE',  ( -9.999999999999998224, 1.224646799147353059E-15, -157.6250000040967905 ) ) ;
#4904 = CARTESIAN_POINT ( 'NONE',  ( 5.000000000000000000, 8.660254037844385522, -159.6250000040967905 ) ) ;
#4905 = CARTESIAN_POINT ( 'NONE',  ( 10.81189881249999551, -6.242252689847874514, -98.96875000204838102 ) ) ;
#4906 = CARTESIAN_POINT ( 'NONE',  ( -9.999999999999998224, 1.224646799147353059E-15, -10.24999999999995381 ) ) ;
#4907 = CARTESIAN_POINT ( 'NONE',  ( 4.999999999999992006, -8.660254037844389075, -72.74999999999998579 ) ) ;
#4908 = CARTESIAN_POINT ( 'NONE',  ( -5.405949406249996869, 9.363379034771805109, -195.8437500020484094 ) ) ;
#4909 = CARTESIAN_POINT ( 'NONE',  ( -9.999999999999998224, 1.224646799147353059E-15, -85.62500000409677625 ) ) ;
#4910 = CARTESIAN_POINT ( 'NONE',  ( 2.933915056720935777, -10.14638297711852388, -180.0000000000000284 ) ) ;
#4911 = CARTESIAN_POINT ( 'NONE',  ( 10.81189881249999907, 6.242252689847868297, -92.90625000204839523 ) ) ;
#4912 = CARTESIAN_POINT ( 'NONE',  ( 7.644554776091147741E-16, 12.48450537969573659, -79.15625000204838102 ) ) ;
#4913 = CARTESIAN_POINT ( 'NONE',  ( -9.999999999999998224, 1.224646799147353059E-15, -72.12500000409677625 ) ) ;
#4914 = CARTESIAN_POINT ( 'NONE',  ( 7.070501591499376803E-16, 11.54700538379251284, -118.6250000000000142 ) ) ;
#4915 = CARTESIAN_POINT ( 'NONE',  ( -2.293366432827344421E-15, -12.48450537969573659, -27.21875000204837747 ) ) ;
#4916 = VERTEX_POINT ( 'NONE', #33549 ) ;
#4917 = CARTESIAN_POINT ( 'NONE',  ( 9.999999999999998224, 0.000000000000000000, -3.499999999999975131 ) ) ;
#4918 = CARTESIAN_POINT ( 'NONE',  ( 7.644554776091147741E-16, 12.48450537969573659, -28.15625000204838102 ) ) ;
#4919 = CARTESIAN_POINT ( 'NONE',  ( 10.81189881249999729, 6.242252689847867408, -16.21875000204836326 ) ) ;
#4920 = DIRECTION ( 'NONE',  ( 0.000000000000000000, 0.000000000000000000, -1.000000000000000000 ) ) ;
#4921 = CARTESIAN_POINT ( 'NONE',  ( -9.999999999999998224, 1.224646799147353059E-15, -4.625000004096769146 ) ) ;
#4922 = DIRECTION ( 'NONE',  ( 0.000000000000000000, -0.9961946980917455452, -0.08715574274765837404 ) ) ;
#4923 = CARTESIAN_POINT ( 'NONE',  ( -5.405949406250003975, -9.363379034771801557, -131.0312500020484094 ) ) ;
#4924 = CARTESIAN_POINT ( 'NONE',  ( 5.000000000000000000, 8.660254037844385522, -184.7500000000000000 ) ) ;
#4925 = CARTESIAN_POINT ( 'NONE',  ( 9.999999999999998224, 0.000000000000000000, -200.0000000000000000 ) ) ;
#4927 = ORIENTED_EDGE ( 'NONE', *, *, #11221, .F. ) ;
#4926 = CARTESIAN_POINT ( 'NONE',  ( 7.644554776091147741E-16, 12.48450537969573659, -112.1562500020483810 ) ) ;
#4928 = DIRECTION ( 'NONE',  ( 0.000000000000000000, 0.000000000000000000, 1.000000000000000000 ) ) ;
#4929 = ORIENTED_EDGE ( 'NONE', *, *, #1611, .T. ) ;
#4930 = ORIENTED_EDGE ( 'NONE', *, *, #40243, .F. ) ;
#4931 = CARTESIAN_POINT ( 'NONE',  ( 10.81189881249999729, 0.000000000000000000, -36.03125000204837391 ) ) ;
#4932 = PERSON_AND_ORGANIZATION ( #11915, #17965 ) ;
#4933 = SECURITY_CLASSIFICATION ( '', '', #6675 ) ;
#4934 = CARTESIAN_POINT ( 'NONE',  ( 10.81189881249999551, -6.242252689847874514, -86.96875000204838102 ) ) ;
#4935 = DIRECTION ( 'NONE',  ( -0.000000000000000000, -0.000000000000000000, -1.000000000000000000 ) ) ;
#4936 = DIRECTION ( 'NONE',  ( -0.000000000000000000, -0.000000000000000000, 1.000000000000000000 ) ) ;
#4937 =( BOUNDED_CURVE ( )  B_SPLINE_CURVE ( 2, ( #32059, #25579, #31854, #2288, #18448, #2908, #28607 ),
 .UNSPECIFIED., .F., .F. ) 
 B_SPLINE_CURVE_WITH_KNOTS ( ( 3, 2, 2, 3 ),
 ( 0.1268656716417910224, 0.1281094527363183799, 0.1293532338308457652, 0.1305970149253731227 ),
 .UNSPECIFIED. ) 
 CURVE ( )  GEOMETRIC_REPRESENTATION_ITEM ( )  RATIONAL_B_SPLINE_CURVE ( ( 1.000000000000003109, 0.8660254037844358210, 1.000000000000000000, 0.8660254037844387076, 1.000000000000000000, 0.8660254037844387076, 1.000000000000000000 ) ) 
 REPRESENTATION_ITEM ( '' )  );
#4938 = LINE ( 'NONE', #39949, #28819 ) ;
#4939 = CARTESIAN_POINT ( 'NONE',  ( 10.81189881249999551, -6.242252689847874514, -168.1562500020484094 ) ) ;
#4940 = VECTOR ( 'NONE', #20305, 1000.000000000000000 ) ;
#4941 = LINE ( 'NONE', #4505, #26734 ) ;
#4942 = ADVANCED_FACE ( 'NONE', ( #27271 ), #13443, .F. ) ;
#4943 = CARTESIAN_POINT ( 'NONE',  ( 10.81189881249999729, 6.242252689847867408, -121.2187500020483952 ) ) ;
#4944 = CARTESIAN_POINT ( 'NONE',  ( 10.81189881249999907, 6.242252689847868297, -88.21875000204838102 ) ) ;
#4945 = CARTESIAN_POINT ( 'NONE',  ( 9.999999999999998224, 0.000000000000000000, -102.5000000000000000 ) ) ;
#4946 = CARTESIAN_POINT ( 'NONE',  ( -10.81189881249999729, 1.324075727343319199E-15, -192.5937500020484094 ) ) ;
#4947 = CARTESIAN_POINT ( 'NONE',  ( 5.405949406249992428, -9.363379034771808662, -93.28125000204838102 ) ) ;
#4948 = CARTESIAN_POINT ( 'NONE',  ( -4.999999999999996447, 8.660254037844387298, -178.8750000040967905 ) ) ;
#4949 = CARTESIAN_POINT ( 'NONE',  ( 7.644554776091147741E-16, 12.48450537969573659, -169.1562500020484094 ) ) ;
#4950 = CARTESIAN_POINT ( 'NONE',  ( 9.999999999999998224, 0.000000000000000000, -103.9999999999999858 ) ) ;
#4951 = CARTESIAN_POINT ( 'NONE',  ( 10.81189881249999551, -6.242252689847874514, -175.6562500020484094 ) ) ;
#4952 = CARTESIAN_POINT ( 'NONE',  ( 7.644554776091147741E-16, 12.48450537969573659, -187.1562500020484094 ) ) ;
#4953 = CARTESIAN_POINT ( 'NONE',  ( 5.405949406249992428, -9.363379034771808662, -54.09375000204835970 ) ) ;
#4954 = CARTESIAN_POINT ( 'NONE',  ( -9.999999999999998224, 1.224646799147353059E-15, -165.1250000040967905 ) ) ;
#4955 = CARTESIAN_POINT ( 'NONE',  ( -10.81189881249999907, -6.242252689847864744, -9.656250002048379244 ) ) ;
#4956 = CARTESIAN_POINT ( 'NONE',  ( 7.644554776091147741E-16, 12.48450537969573659, -9.968750002048359704 ) ) ;
#4957 = DIRECTION ( 'NONE',  ( -0.000000000000000000, -0.000000000000000000, 1.000000000000000000 ) ) ;
#4958 = CARTESIAN_POINT ( 'NONE',  ( -10.81189881249999729, 6.242252689847871849, -122.2187500020483810 ) ) ;
#4959 = CARTESIAN_POINT ( 'NONE',  ( -2.121150477449813534E-15, -11.54700538379251284, -101.3750000000000000 ) ) ;
#4960 = CARTESIAN_POINT ( 'NONE',  ( 7.644554776091147741E-16, 12.48450537969573659, -20.65625000204837747 ) ) ;
#4961 = CARTESIAN_POINT ( 'NONE',  ( 9.999999999999998224, 0.000000000000000000, -108.8750000040967763 ) ) ;
#4962 = CARTESIAN_POINT ( 'NONE',  ( 10.00000000000000000, 5.773502691896255534, -52.87499999999997868 ) ) ;
#4963 = CARTESIAN_POINT ( 'NONE',  ( 5.405949406249999534, 9.363379034771803333, -116.7812500020483952 ) ) ;
#4964 = CARTESIAN_POINT ( 'NONE',  ( -10.81189881249999729, 6.242252689847871849, -102.9062500020483952 ) ) ;
#4965 = EDGE_CURVE ( 'NONE', #3711, #41596, #38331, .T. ) ;
#4966 = VERTEX_POINT ( 'NONE', #4182 ) ;
#4967 = AXIS2_PLACEMENT_3D ( 'NONE', #8535, #35295, #34656 ) ;
#4968 = CARTESIAN_POINT ( 'NONE',  ( 9.999999999999996447, -5.773502691896262640, -97.00000000409677625 ) ) ;
#4969 = CARTESIAN_POINT ( 'NONE',  ( 5.000000000000000000, 8.660254037844385522, -141.6250000040967905 ) ) ;
#4970 = CARTESIAN_POINT ( 'NONE',  ( 5.405949406249999534, 9.363379034771803333, -161.7812500020484094 ) ) ;
#4971 = CARTESIAN_POINT ( 'NONE',  ( -10.81189881249999907, -6.242252689847864744, -46.96875000204835970 ) ) ;
#4972 = ORIENTED_EDGE ( 'NONE', *, *, #30168, .F. ) ;
#4973 = CARTESIAN_POINT ( 'NONE',  ( 4.999999999999992006, -8.660254037844389075, -21.74999999999996447 ) ) ;
#4974 = CARTESIAN_POINT ( 'NONE',  ( -10.81189881249999729, -6.242252689847864744, -26.15625000204837391 ) ) ;
#4975 = CARTESIAN_POINT ( 'NONE',  ( 10.00000000000000000, 5.773502691896255534, -165.3749999999999716 ) ) ;
#4976 = CARTESIAN_POINT ( 'NONE',  ( -5.000000000000003553, -8.660254037844383745, -103.0000000000000000 ) ) ;
#4977 = CARTESIAN_POINT ( 'NONE',  ( -9.999999999999998224, 5.773502691896259087, -28.75000000409674783 ) ) ;
#4978 =( BOUNDED_CURVE ( )  B_SPLINE_CURVE ( 2, ( #40932, #14387, #1904, #34499, #31689, #11374, #28016 ),
 .UNSPECIFIED., .F., .F. ) 
 B_SPLINE_CURVE_WITH_KNOTS ( ( 3, 2, 2, 3 ),
 ( 0.6679104477611942370, 0.6691542288557216223, 0.6703980099502490075, 0.6716417910447763928 ),
 .UNSPECIFIED. ) 
 CURVE ( )  GEOMETRIC_REPRESENTATION_ITEM ( )  RATIONAL_B_SPLINE_CURVE ( ( 0.9999999999999761302, 0.8660254037844625774, 1.000000000000000000, 0.8660254037844387076, 1.000000000000000000, 0.8660254037844148378, 1.000000000000023981 ) ) 
 REPRESENTATION_ITEM ( '' )  );
#4979 = AXIS2_PLACEMENT_3D ( 'NONE', #16034, #39562, #42584 ) ;
#4980 = DIRECTION ( 'NONE',  ( 0.000000000000000000, 0.000000000000000000, 1.000000000000000000 ) ) ;
#4981 = CARTESIAN_POINT ( 'NONE',  ( 10.81189881249999729, 0.000000000000000000, -135.0312500020484094 ) ) ;
#4982 = CARTESIAN_POINT ( 'NONE',  ( 7.547620300323909959, 7.372587587660208719, -7.434655202704447971E-15 ) ) ;
#4983 = DIRECTION ( 'NONE',  ( -0.000000000000000000, -0.000000000000000000, -1.000000000000000000 ) ) ;
#4984 = ORIENTED_EDGE ( 'NONE', *, *, #20639, .F. ) ;
#4985 =( BOUNDED_SURFACE ( )  B_SPLINE_SURFACE ( 1, 2, ( 
 ( #8815, #35151, #29096, #38163, #12659, #5575, #9446, #15477, #18729, #35786, #39008, #12246, #22611, #25438, #35363, #5791, #18944, #32128, #39630, #3824, #22827, #26484, #7060, #35991, #13504, #16531, #596, #10278, #10070, #26693, #12871, #10489, #30156, #23465, #39845, #13295, #20210, #36612, #6425, #33399, #23247, #3616, #16315, #19568, #16743, #39217, #29513, #16960, #36825, #386, #42444, #13713, #3188, #29943, #29728, #32752, #39429, #26902, #174, #40058, #23678, #19363, #42655, #23037, #9655, #26067, #32548, #2978, #32967, #16103, #13080, #26276, #9864, #36193, #6630, #19781, #29297, #3394, #36407, #6840, #19993, #33184, #20628, #21277, #27761, #8124, #34250, #40898, #37684, #24755, #37468, #33817, #1226, #20420, #11547, #10699, #11340, #14783, #40262, #24535, #24325, #7267, #10915, #30582, #33608, #23893, #14572, #4240, #20847, #4663, #17814, #7479, #7912, #40467, #27550, #13926, #21059, #24108, #4884, #18031, #37246, #37041, #34462, #17382, #1012, #30792, #802, #27979, #7693, #31009, #1438, #31228, #4026, #41107, #1653, #14132, #30372, #14352, #17171, #27333, #27121, #34031, #4451, #17593, #40684, #11122, #15428, #1873, #41967, #18464, #28626, #28415, #2710, #19104, #35312, #8972, #31652, #2302, #41553, #22349, #25180, #21496, #41757, #2086, #38530, #14999, #15842, #18674, #11984, #34888, #32286, #38322, #41331, #8763, #5312, #35525, #21919, #38112, #5954, #22138, #31871, #8556, #5742, #35099, #12192, #15216, #5524, #25594, #21706, #28198, #29042, #9178, #31437, #25383, #18895, #15634, #11769, #32075, #24970, #2510, #28836, #42180, #12401, #38749, #12607, #37902, #8345, #34678, #5100, #18246, #16054, #33346, #19940, #6372, #16690, #35931, #30102, #26012, #23410, #38957, #9806, #39164, #10223, #20156, #39790, #42602, #29245, #32910, #36142, #326, #16901, #3767, #36352, #19302, #42389, #33129, #22556, #541, #6785, #3343, #29886, #6162, #16475, #26427, #12821, #22985, #32700, #19516, #39578, #32496, #13446, #9596, #25801, #6573, #35732, #9391, #10014, #13028, #3556, #19729, #26641, #29674, #2924, #22771, #118, #36559, #3131, #13240, #7005, #16260, #29459, #23191, #26221, #39370, #20788, #7857, #7209, #4823, #24478, #17754, #34195, #7638, #1382, #4613, #751, #14512, #33977, #40626, #10643, #13873, #11068, #33551, #23835, #30949, #31170, #37415, #36772, #27706, #40211, #24269, #24048, #27068, #33762, #21219, #10857, #21006, #17970, #13659, #36986, #17329, #3976, #20362, #40844, #8069, #27275, #26850, #7422, #20572, #17116, #30316, #4185, #30532, #11283, #959, #14077, #40412, #37630, #23627, #37189, #34404, #40005, #10436, #4398, #17537, #30739, #1169, #14292, #27492, #38265, #14728, #1816, #18189, #14942, #12140, #41702, #31381, #21433, #28356, #22084, #31596, #41494, #25545, #35259, #8712, #38478, #37844, #35471, #12346, #5693, #18842, #21866, #32023, #2450, #28142, #15583, #35045, #28572, #41275, #11711, #25333, #34618, #24910, #28784, #19051, #8922, #24698, #41915, #38057, #38695, #11928, #8497, #21650, #9129, #25121, #22299, #5895, #1599, #34831, #5255, #5044, #8286, #27920, #41052, #15158, #11495, #18407, #2029, #5472, #18622, #31818, #2252, #15372, #16002, #35680, #9336, #13187, #42128, #2872, #3498, #9962, #33072, #16421, #23140, #19889, #6949, #19675, #29197, #26170, #2659, #32445, #6108, #42337, #62, #29619, #19255, #22505, #16207, #36304, #19467, #16637, #26589, #29839, #6320, #12767, #39317, #42549, #6735, #23360, #39740, #26380, #25754, #25961, #39531, #28989, #32233, #276, #9756, #13397, #12560, #22937, #32862, #39109, #29409, #9546, #22720, #3293, #38907, #10175, #35885, #36512, #12973, #32652, #15793, #3080, #36090, #6525, #910, #11021, #27220, #39952, #36720, #40365, #4561, #23573, #10806, #7809, #7159, #14241, #17066, #13821, #24215, #10384, #27654, #27444, #702, #37366, #30263, #24435, #20311, #17702, #33295, #4135, #33504, #37578, #3928, #20957, #40795, #27014, #40580, #37139, #20104, #23779, #40161, #3721, #10592, #34143, #36932, #33710, #17492, #4351, #7376, #7587, #20522, #23999, #26802, #20740, #17276, #30897, #1333, #30481, #14025, #14464, #33927, #30685, #1116, #13610, #11236, #16850, #30048, #495, #38808, #8023, #16109, #42240, #15482, #31118, #15696, #2773, #24649, #14684, #22195, #29305, #21167, #25652, #9235, #28895, #27871, #12665, #31927, #42028, #41814, #42451, #32556, #6010, #22404, #2355, #12459, #12252, #35793, #38590, #34356, #35581, #28686, #19159, #41005, #12878, #32136, #25444, #5581, #2985, #9031, #11449, #35370, #18735, #6224, #5797, #8820, #19369, #32349, #2567, #21977, #15899, #18949, #29104, #25860, #39015, #9452, #35156, #37792, #26073, #22618, #1551, #4773, #17921, #16968, #29520, #33193, #3195, #392, #20217, #7275, #30163, #604, #26700, #13719, #26909, #13932, #183, #19787, #39224, #13086, #3832, #23042, #10078, #36621, #23473, #39436, #39852, #29737, #16751, #16321, #10286, #13303, #36832, #20429, #26492, #26286, #40066, #9869, #32974, #20001, #32758, #17180, #39637, #13511, #7068, #33407, #9662, #4033, #10497, #3403, #19575, #3624, #22835, #42662, #23685, #6431, #36200, #33615, #30378, #810, #35997, #6637, #16538, #23255, #36414, #6848, #29952, #40269, #27340, #1019, #40474, #37692, #24541, #14139, #4249, #11132, #4891, #14359, #11554, #21503, #41115, #1233, #30588, #34257, #37475, #1659, #18252, #34685, #8133, #20636, #17391, #34469, #23903, #1878, #21283, #4670, #31235, #7485, #17821, #27768, #10922, #24334, #34038, #37252, #40906, #33825, #14791, #24116, #5105, #7919, #37048, #31443, #11348, #27557, #18039, #21066, #27986, #31016, #7704, #20854, #1446, #24764, #4458, #14581, #37908, #17601, #8352, #27126, #10706, #30797, #40691, #9184, #8563, #6168, #25807, #19110, #35531, #8978, #2717, #5960, #2093, #15848, #35319, #29048, #41975, #32293, #42187, #32501, #2516, #28422, #22145, #28204, #15223, #31659, #41558, #25600, #12407, #11991, #34894, #41765, #12614, #2309, #38964, #9398, #22562, #31878, #18471, #5748, #25388, #35740, #19308, #15006, #38758, #21713, #5318, #22355, #11775, #41338, #24977, #18901, #38118, #25187, #32082, #15641, #38327, #12198, #21925, #8769, #28841, #35106, #5531, #18680, #15435, #38537, #28633, #7216, #16697, #32916, #23417, #26433, #36565, #10020, #22777, #19522, #23198, #30108, #6379, #36358, #33353, #32706, #39796, #125, #26858, #7011, #6791, #10229, #39170, #36780, #13664, #20163, #3773, #39584, #16907, #547, #3139, #40012, #19947, #29893, #42607, #16266, #333, #35938, #13035, #10442, #20368, #26647, #26018, #23634, #29465, #13452, #13246, #26228, #22990, #2931, #33135, #16060, #29252, #42396, #39376, #6579, #9812, #9604, #12827, #36147, #16482, #19736, #3349, #29681, #3563, #13878, #36993, #14084, #7428, #14737, #8297, #10651, #14521, #757, #4191, #4832, #11291, #23843, #17544, #24486, #20796, #17978, #27930, #31178, #7645, #20579, #40634, #1178, #8077, #24706, #41060, #1391, #27074, #33769, #40852, #30324, #33557, #27714, #11074, #37638, #40217, #24277, #34203, #17336, #30746, #40420, #966, #4619, #30539, #21228, #27284, #11504, #14299, #10864, #37852, #17765, #33984, #34414, #27499, #1607, #37422, #24055, #37197, #7865, #3981, #4405, #21013, #17122, #30959, #15592, #18631, #2668, #12356, #28580, #28793, #14951, #12570, #32241, #25554, #41924, #15382, #9139, #38705, #8505, #22307, #41710, #5702, #18415, #21659, #18853, #41283, #31605, #35480, #38916, #2461, #1824, #5907, #5263, #32033, #31825, #34839, #41504, #28998, #2261, #19060, #25763, #21441, #2037, #25128, #11722, #28149, #15802, #42139, #35053, #34625, #15168, #28365, #24920, #38064, #11936, #38274, #8720, #5052, #18198, #21875, #31389, #5481, #12148, #25340, #38487, #8931, #22095, #35269, #39751, #26814, #39541, #22730, #3303, #22516, #9556, #25971, #35896, #19899, #6746, #39122, #29849, #39327, #36521, #3731, #23371, #26180, #12779, #16431, #19688, #26601, #506, #16861, #33083, #2882, #42347, #16648, #6118, #9347, #3511, #29630, #13408, #32456, #73, #9972, #6333, #36101, #16219, #19476, #23152, #16012, #10186, #32662, #30064, #6535, #19263, #13622, #36314, #9767, #287, #32872, #6961, #13197, #29208, #3092, #26390, #20118, #29419, #33306, #35689, #42559, #12983, #22947, #21179, #30910, #4364, #34155, #33517, #31132, #8035, #1346, #17715, #33942, #27670, #14475, #27028, #40808, #17503, #24228, #36946, #40173, #37379, #17078, #7388, #11248, #14695, #20969, #20323, #24446, #23791, #7822, #7599, #10604, #17291, #4785, #37153, #4573, #1565, #39966, #20535, #922, #30276, #3940, #37591, #34369, #10818, #10396, #33724, #4147, #715, #13834, #30495, #14037, #27233, #17933, #23586, #40376, #36733, #7171, #24011, #20754, #30698, #1130, #14253, #27456, #40592, #11034, #15339, #41235, #21830, #41017, #28107, #1778, #11673, #38441, #25298, #14908, #5012, #11891, #11461, #25086, #24873, #32197, #31348, #31988, #35430, #18153, #5652, #2207, #2624, #31562, #8467, #27884, #38023, #35221, #21618, #41456, #8885, #12103, #34797, #28536, #18373, #5439, #34582, #41668, #1995, #25509, #38657, #15120, #5217, #18800, #28315, #38231, #8676, #21397, #5858, #35009, #22048, #2414, #15546, #24662, #19012, #28748, #37804, #41874, #12311, #18591, #31777, #9094, #22261, #8250, #28954, #32822, #16379, #36054, #22465, #19848, #39071, #6490, #6282, #23318, #39702, #13147, #29580, #9510, #22898, #19428, #240, #3043, #42091, #19638, #22680, #24, #35642, #36473, #39283, #32618, #12722, #10138, #16171, #19219, #29366, #25920, #13362, #42506, #15965, #26554, #26342, #9716, #29161, #39494, #12933, #3252, #35849, #26129, #3462, #42301, #6070, #6907, #29800, #9295, #9925, #23104, #36266, #32409, #6697, #2831, #33033, #16597, #20061, #33256, #15756, #12524, #25717, #38866, #3892, #666, #30645, #23533, #20913, #33888, #30226, #17449, #17027, #4517, #20278, #10981, #1076, #30440, #4310, #26762, #34096, #24176, #14201, #27401, #17240, #40537, #37323, #7123, #7770, #871, #23959, #13784, #33466, #37103, #10345, #26967, #17661, #3682, #16810, #39915, #30009, #40125, #455, #13987, #10555, #36894, #13571, #10770, #36683, #23741, #7338, #20487, #33673, #7547, #27184, #4099, #40328, #20700, #12655, #22822, #6421, #2971, #22604, #16099, #35985, #29291, #23460, #16952, #19357, #23242, #9439, #12866, #13500, #19988, #379, #26478, #33179, #29939, #42229, #29724, #26061, #36186, #25848, #42439, #39212, #9649, #10064, #39625, #19561, #32543, #26271, #3610, #29506, #26688, #36607, #39841, #16311, #32747, #6624, #9857, #16739, #33394, #7055, #36401, #35780, #3184, #6834, #39003, #6212, #10273, #19776, #20205, #42649, #32961, #169, #13076, #39424, #23033, #3389, #13291, #16526, #3817, #13920, #8118, #14126, #40052, #34456, #1221, #17377, #7906, #10910, #21054, #37240, #7261, #4020, #7687, #14566, #33601, #20842, #17808, #17164, #24319, #27328, #11334, #1008, #30366, #40891, #14346, #24101, #796, #30787, #30577, #34025, #27114, #40462, #31004, #40256, #20413, #27755, #1433, #23673, #4447, #10692, #34244, #23888, #17588, #36820, #27544, #11117, #24528, #4658, #37678, #40678, #21270, #4877, #37036, #7472, #30150, #20621, #588, #37463, #33811, #13706, #4235, #26897, #10483, #29413, #36308, #13191, #6529, #22941, #39115, #32866, #36095, #32237, #3298, #22724, #42553, #42133, #2663, #12977, #22303, #12564, #19680, #19893, #26174, #25549, #16425, #28993, #39320, #12772, #15797, #22510, #9966, #42341, #9760, #6739, #2456, #25758, #6112, #35475, #9133, #29623, #39536, #16006, #15587, #38911, #9342, #5901, #38699, #19055, #35684, #19259, #26384, #28788, #32450, #66, #12351, #2876, #23145, #41919, #29201, #25965, #9550, #35889, #6326, #32656, #19471, #3084, #16212, #33299, #6953, #3724, #915, #30486, #20109, #10179, #17071, #10811, #20316, #17497, #27449, #4356, #7164, #36516, #40166, #707, #7592, #24220, #40585, #14030, #37371, #16854, #37144, #11026, #23364, #24004, #7381, #7814, #36725, #13615, #33077, #30056, #40370, #500, #3933, #27226, #17281, #26807, #20527, #23578, #10598, #39744, #33715, #33510, #30690, #1123, #30268, #39958, #20746, #10389, #13826, #27020, #26594, #3503, #23784, #4140, #33933, #14246, #16641, #29843, #281, #13402, #36939, #34789, #21390, #37583, #27659, #34573, #41661, #34148, #38014, #21610, #41228, #40800, #25079, #1556, #11665, #11454, #28529, #2198, #18366, #5210, #14688, #28100, #24654, #5431, #8242, #4566, #24866, #27877, #31554, #11241, #12097, #1771, #37797, #17926, #15332, #5004, #24440, #18145, #31123, #18582, #31341, #21172, #31770, #1987, #14901, #34362, #15113, #8459, #28308, #41009, #41447, #8668, #4778, #8028, #25290, #35002, #14469, #11883 ),
 ( #38224, #21822, #38435, #20962, #17708, #30903, #1338, #18792, #22253, #22888, #29359, #9709, #35842, #42498, #39275, #26334, #39064, #35423, #2824, #22041, #9085, #25501, #5850, #19420, #6274, #38650, #28740, #35635, #12926, #38859, #36047, #3245, #6483, #25709, #12304, #15957, #19212, #26121, #16, #16371, #32611, #2407, #41866, #16163, #5643, #8878, #3036, #29154, #19630, #31981, #42293, #9502, #19005, #6062, #15748, #32190, #22671, #15538, #32814, #2617, #29571, #32401, #28947, #13139, #35213, #9286, #42084, #12715, #12516, #25912, #22458, #13354, #17020, #23952, #232, #3885, #27177, #26545, #33667, #36675, #20693, #23095, #30219, #20053, #23734, #30638, #7539, #864, #17233, #33458, #40320, #30434, #39694, #10761, #658, #36885, #36464, #10130, #7331, #16589, #6900, #13980, #14194, #20480, #19839, #37096, #23309, #4091, #7116, #33247, #16802, #4303, #20270, #33881, #13776, #39486, #447, #3674, #9919, #30001, #17442, #13564, #10338, #1070, #36258, #26755, #26960, #39907, #40116, #3453, #10549, #23526, #6688, #33024, #29791, #14415, #34739, #27609, #7971, #8189, #20906, #5376, #1503, #1719, #14848, #28044, #27393, #34951, #18313, #18527, #41171, #11610, #27825, #1286, #34088, #40959, #31716, #40530, #24818, #37963, #4948, #4511, #31503, #21120, #18095, #17873, #2147, #8617, #8408, #21559, #34309, #34525, #31069, #11830, #14637, #10973, #31290, #4724, #5161, #17654, #24169, #21336, #11402, #24389, #21773, #24596, #30849, #37745, #37530, #25030, #1933, #40749, #38173, #15060, #28258, #11191, #41395, #37316, #7762, #12256, #15700, #2990, #41818, #35161, #42456, #29311, #8826, #12463, #25449, #35798, #5587, #9240, #21983, #19165, #39021, #26078, #6229, #19375, #2779, #32562, #16115, #38595, #9035, #12883, #18740, #22840, #9457, #22200, #39229, #35374, #35587, #32141, #9667, #28480, #42033, #28691, #19580, #31932, #36003, #6437, #2359, #22409, #32764, #15282, #15486, #41611, #6015, #42245, #5801, #18953, #12670, #2571, #28899, #12045, #25241, #22623, #38385, #25656, #38812, #25866, #32354, #15905, #29109, #10714, #398, #610, #7491, #3200, #13309, #6854, #36206, #9875, #13726, #40275, #16758, #16326, #26499, #10084, #6642, #26291, #19792, #39644, #32979, #27132, #20644, #23048, #26915, #13091, #16543, #17186, #23691, #4041, #30171, #36838, #33620, #29525, #33413, #29742, #39858, #42667, #3408, #189, #23260, #40073, #10503, #36420, #20007, #29958, #7282, #33199, #30384, #23909, #816, #3630, #13518, #10292, #26706, #20435, #37054, #39441, #13939, #23479, #36627, #7074, #20223, #3839, #16974, #11354, #37914, #14146, #40912, #34475, #7711, #17827, #40697, #1241, #4897, #27346, #21509, #17607, #11780, #31022, #1025, #38123, #18045, #21074, #11562, #14587, #24770, #24548, #10928, #20860, #37699, #18260, #37261, #8141, #34691, #34044, #27993, #1452, #15012, #17397, #21289, #14365, #31241, #24982, #1883, #8358, #5111, #4255, #27776, #4465, #8568, #30803, #31449, #41344, #24122, #28209, #1668, #33831, #37481, #27563, #30595, #11140, #41122, #24340, #4679, #14797, #40481, #7925, #34263, #12203, #41982, #28427, #22360, #25396, #19315, #32509, #38542, #8776, #29054, #21932, #2313, #2521, #15228, #42403, #8983, #38763, #9189, #35536, #21718, #29260, #12620, #12835, #5965, #19116, #22150, #38333, #41563, #35325, #26025, #34901, #32302, #2723, #12412, #11996, #25813, #15440, #25605, #5753, #39178, #2938, #15856, #42193, #28638, #28847, #18906, #6175, #32087, #5323, #38969, #41771, #9405, #25192, #18477, #15647, #22568, #18685, #16067, #35747, #35111, #31664, #31883, #2098, #5536, #9818, #20376, #23424, #3571, #22999, #10237, #10027, #29902, #6587, #23208, #40020, #36154, #29472, #36788, #23642, #3146, #6801, #19743, #30117, #42614, #16705, #16273, #13462, #33361, #33565, #554, #13674, #39805, #26866, #10450, #32923, #3357, #7225, #13041, #17132, #3781, #16489, #3989, #29688, #340, #26441, #30333, #763, #131, #26236, #13886, #27082, #39385, #19955, #13254, #9611, #39593, #26655, #36366, #36573, #16915, #22785, #35945, #6388, #7019, #19529, #32713, #33143, #20172, #31187, #30546, #5061, #34423, #20805, #1617, #33993, #17774, #14309, #17987, #10659, #24286, #10872, #1832, #974, #14746, #18208, #14092, #27939, #14530, #14960, #1187, #4414, #40225, #27293, #4842, #24065, #11085, #37647, #24494, #40429, #27724, #30754, #30970, #4199, #40860, #27509, #37861, #8306, #40643, #37207, #41068, #7654, #17553, #21021, #33777, #31398, #37431, #11300, #8087, #21237, #23852, #37001, #11513, #7436, #24715, #21451, #7874, #34212, #17343, #4628, #20589, #1400, #34634, #28803, #5711, #34849, #32250, #8730, #18862, #18640, #35698, #9355, #25564, #41935, #21884, #35278, #31834, #12578, #15392, #11731, #32043, #35062, #12366, #5272, #6126, #8940, #2270, #25137, #22525, #28589, #31614, #41720, #38283, #25771, #12157, #28374, #38924, #38716, #22104, #41514, #9149, #25350, #2472, #5490, #38496, #15601, #22317, #5918, #41292, #35490, #11946, #32465, #2047, #2677, #19270, #18424, #19069, #15811, #2890, #29007, #42147, #28158, #15177, #24930, #38074, #8514, #21667, #295, #16228, #3520, #6543, #36322, #22738, #16656, #19697, #14210, #27409, #32880, #3099, #23379, #29427, #39336, #39549, #9564, #37331, #3311, #33092, #29857, #13416, #16020, #24184, #7555, #7778, #26611, #39759, #16440, #32671, #35904, #29639, #20921, #29216, #10194, #36529, #6753, #6341, #20708, #9775, #19907, #82, #34103, #40545, #33896, #4318, #22955, #23159, #13205, #1084, #26398, #42355, #17457, #36109, #30654, #19484, #12788, #9980, #10989, #12992, #25979, #39131, #42568, #26188, #1517, #2161, #18108, #4740, #15295, #18327, #41184, #17886, #5173, #4961, #24831, #14651, #31303, #34966, #31084, #24403, #31731, #18540, #40763, #1735, #27840, #25044, #37544, #11624, #11205, #8421, #28273, #28492, #38186, #8630, #34753, #21786, #5389, #40972, #11415, #41624, #7984, #12058, #41409, #24609, #25254, #37758, #17669, #8202, #21351, #21135, #27623, #34323, #34537, #14861, #38399, #21997, #28058, #11843, #14430, #37977, #8841, #4526, #30863, #31516, #1299, #21572, #1946, #15071, #5813, #29120, #5600, #35389, #9048, #18966, #3001, #32575, #22213, #12268, #19177, #12895, #22421, #19592, #29536, #6450, #9252, #38609, #42256, #2790, #9678, #26303, #42678, #16126, #28704, #25464, #42467, #31944, #9887, #29323, #12681, #39240, #15498, #25878, #35809, #32153, #32366, #42048, #2583, #6241, #41831, #22851, #15712, #13104, #15919, #2372, #39452, #19385, #35599, #26089, #39032, #36013, #9467, #28911, #12474, #22636, #32775, #25669, #3211, #16338, #38823, #35175, #18754, #6027, #6653, #619, #3641, #7292, #14157, #33840, #27141, #827, #16983, #10725, #13948, #10093, #23918, #13735, #20444, #20017, #23271, #33629, #199, #33210, #40284, #40492, #4051, #3419, #37062, #6866, #17195, #33422, #36430, #408, #30605, #20233, #30394, #27357, #23061, #16768, #26716, #13320, #29754, #7501, #17407, #36637, #36849, #10302, #20653, #3848, #4266, #30181, #26509, #39656, #26924, #1034, #29968, #40082, #36217, #13529, #19803, #10513, #32991, #16556, #23700, #39868, #23489, #7083, #21728, #15022, #31459, #4909, #41354, #1893, #40708, #11791, #31251, #37924, #7935, #11151, #8370, #30813, #21085, #28221, #28439, #34701, #34054, #24993, #37491, #21520, #21299, #24350, #31032, #18488, #8151, #5121, #15241, #10938, #34273, #14597, #1252, #17618, #18270, #5333, #24559, #24131, #4688, #17837, #14376, #4476, #27573, #1464, #27787, #34911, #37273, #40921, #38135, #20870, #11364, #8578, #31676, #2110, #7722, #37709, #34487, #18056, #41133, #1679, #14807, #28003, #11573, #24779, #41780, #9416, #38980, #15452, #18699, #25617, #19326, #28858, #26038, #35958, #12846, #15658, #2323, #5977, #9201, #16078, #32724, #6399, #22581, #35123, #31895, #6187, #38344, #16286, #35759, #19128, #2950, #21943, #32313, #42205, #28650, #38775, #5764, #8994, #12631, #5547, #29271, #25407, #19540, #22370, #8786, #3157, #12214, #32521, #15866, #41575, #2533, #22162, #12008, #38553, #42415, #35337, #12423, #39190, #25825, #18917, #29067, #32100, #2736, #41994, #9624, #35547, #22796, #25203, #3584, #16501, #36798, #29699, #10038, #10248, #23011, #7448, #16718, #3793, #16927, #30128, #29484, #37012, #20386, #20601, #565, #13685, #29913, #3368, #36165, #352, #33788, #42624, #26876, #40031, #7031, #6598, #33577, #23220, #20183, #19968, #4211, #10670, #10461, #23652, #36378, #36584, #33154, #13899, #13474, #13054, #33373, #6813, #7236, #19754, #26248, #23436, #26666, #26452, #23864, #39816, #32936, #4000, #39604, #27092, #17143, #145, #40235, #30344, #773, #13266, #39397, #9829, #37656, #14321, #17784, #5070, #1197, #37217, #1843, #31408, #10884, #14540, #27520, #37870, #7664, #11311, #24076, #21247, #41077, #28167, #8315, #21460, #4853, #34644, #18218, #40652, #11094, #14969, #20817, #24939, #11522, #24297, #41302, #37441, #8096, #34222, #11740, #30558, #1410, #30764, #21676, #34003, #38082, #8523, #34859, #17996, #17354, #985, #7884, #21032, #14103, #4424, #27304, #24724, #4638, #40440, #30981, #34433, #27734, #17564, #40870, #24504, #31196, #1626, #14755, #27950, #12795, #38293, #25778, #22324, #22745, #8948, #28597, #5281, #21893, #12585, #31842, #18870, #2684, #32257, #5498, #35499, #38505, #25571, #11955, #5925, #22111, #2897, #16027, #35285, #35071, #38931, #18648, #41728, #28810, #41525, #25988, #5718, #19076, #15819, #29015, #18434, #39139, #9363, #9571, #42154, #22532, #32050, #2279, #25146, #35705, #38723, #19277, #6134, #32473, #29223, #42362, #31623, #2057, #15187, #15400, #41942, #28384, #12165, #25357, #2479, #8739, #15608, #12375, #9156, #19914, #13635, #23166, #20339, #30292, #7185, #9987, #39343, #302, #3527, #10411, #27045, #731, #3745, #29435, #26195, #521, #32678, #10619, #16875, #13422, #39981, #16235, #26618, #36537, #9782, #33103, #90, #3317, #6978, #42577, #23604, #19704, #13849, #16663, #3107, #40190, #20132, #36329, #26827, #29864, #39556, #16449, #35911, #22962, #36748, #32887, #6760, #33320, #30080, #36117, #23387, #26406, #39767, #12998, #33531, #10201, #3954, #17092, #6348, #6550, #19492, #29647, #13212, #4590, #17306, #1795, #40605, #40823, #11264, #24460, #23807, #31363, #14710, #14924, #37607, #8049, #24244, #10833, #24027, #4162, #41033, #36961, #21197, #34384, #1360, #30510, #27901, #4379, #14491, #14269, #28123, #5028, #4800, #17949, #17518, #30925, #27470, #8265, #11049, #7403, #27685, #30718, #31148, #937, #41251, #17730, #37395, #20769, #18169, #7837, #27248, #20985, #33957, #21412, #34171, #37167, #34598, #1580, #11476, #7615, #24677, #37823, #20551, #1145, #33740, #14055, #40389, #31578, #38884, #25734, #5236, #8902, #8694, #32214, #2010, #5669, #18389, #15565, #35450, #22483, #2642, #15773, #41894, #28970, #42109, #21847, #5456, #12543, #15137, #19237, #5876, #35027, #9315, #18606, #32005, #28553, #35659, #24890, #38460, #25102, #15984, #28335, #6090, #32425, #41473, #2850, #28766, #29179, #11693, #38676, #38039, #8481, #21635, #12328, #38249, #18821, #34813, #11907, #31795, #2228, #22278, #9110, #15355, #41685, #22066, #12123, #25315, #35239, #2430, #25527, #19030, #19445, #26362, #29601, #39723, #475, #3701, #3481, #22699, #6301, #260, #39090, #13591, #16617, #39514, #26573, #9529, #9943, #6717, #32637, #16401, #9737, #12953, #19869, #35868, #10158, #29385, #30029, #44, #3063, #42318, #33055, #32843, #13381, #13168, #23340, #23123, #16188, #42528, #36287, #6928, #26148, #29820, #36491, #39299, #20082, #33276, #16830, #25941, #12741, #22918, #36072, #6509, #19658, #3271, #15896, #32134, #25858, #29101, #25233, #39013, #15694, #22402, #35154, #38379, #35579, #15275, #5579, #42238, #12876, #19156, #18521, #12663, #21975, #6008, #5795, #8818, #15480, #2983, #35368, #32347, #42449, #38165, #18732, #41812, #28474, #2140, #2771, #32553, #9028, #8611, #31925, #2353, #41605, #31710, #12038, #28683, #12250, #19367, #21765, #25442, #34943, #9233, #28893, #9450, #22616, #16107, #35790, #38588, #22194, #6222, #5368, #18948, #29303, #42026, #2564, #12456, #25649, #38806, #42660, #10077, #32972, #36198, #39850, #6429, #13717, #9867, #4031, #23253, #35995, #30376, #10284, #13301, #3830, #6846, #16966, #33190, #3193, #13084, #3621, #10495, #29518, #16748, #26907, #26282, #20216, #36412, #7272, #9659, #29950, #6635, #23471, #17178, #36830, #30161, #602, #19999, #40063, #23683, #39434, #20427, #391, #36618, #23040, #19785, #7065, #16319, #3401, #33613, #807, #33404, #19573, #26071, #16536, #39222, #13509, #29734, #179, #22832, #26699, #32756, #26490, #39635, #24114, #17599, #4246, #20634 ) ),
 .UNSPECIFIED., .F., .F., .F. ) 
 B_SPLINE_SURFACE_WITH_KNOTS ( ( 2, 2 ),
 ( 3, 2, 2, 2, 2, 2, 2, 2, 2, 2, 2, 2, 2, 2, 2, 2, 2, 2, 2, 2, 2, 2, 2, 2, 2, 2, 2, 2, 2, 2, 2, 2, 2, 2, 2, 2, 2, 2, 2, 2, 2, 2, 2, 2, 2, 2, 2, 2, 2, 2, 2, 2, 2, 2, 2, 2, 2, 2, 2, 2, 2, 2, 2, 2, 2, 2, 2, 2, 2, 2, 2, 2, 2, 2, 2, 2, 2, 2, 2, 2, 2, 2, 2, 2, 2, 2, 2, 2, 2, 2, 2, 2, 2, 2, 2, 2, 2, 2, 2, 2, 2, 2, 2, 2, 2, 2, 2, 2, 2, 2, 2, 2, 2, 2, 2, 2, 2, 2, 2, 2, 2, 2, 2, 2, 2, 2, 2, 2, 2, 2, 2, 2, 2, 2, 2, 2, 2, 2, 2, 2, 2, 2, 2, 2, 2, 2, 2, 2, 2, 2, 2, 2, 2, 2, 2, 2, 2, 2, 2, 2, 2, 2, 2, 2, 2, 2, 2, 2, 2, 2, 2, 2, 2, 2, 2, 2, 2, 2, 2, 2, 2, 2, 2, 2, 2, 2, 2, 2, 2, 2, 2, 2, 2, 2, 2, 2, 2, 2, 2, 2, 2, 2, 2, 2, 2, 2, 2, 2, 2, 2, 2, 2, 2, 2, 2, 2, 2, 2, 2, 2, 2, 2, 2, 2, 2, 2, 2, 2, 2, 2, 2, 2, 2, 2, 2, 2, 2, 2, 2, 2, 2, 2, 2, 2, 2, 2, 2, 2, 2, 2, 2, 2, 2, 2, 2, 2, 2, 2, 2, 2, 2, 2, 2, 2, 2, 2, 2, 2, 2, 2, 2, 2, 2, 2, 2, 2, 2, 2, 2, 2, 2, 2, 2, 2, 2, 2, 2, 2, 2, 2, 2, 2, 2, 2, 2, 2, 2, 2, 2, 2, 2, 2, 2, 2, 2, 2, 2, 2, 2, 2, 2, 2, 2, 2, 2, 2, 2, 2, 2, 2, 2, 2, 2, 2, 2, 2, 2, 2, 2, 2, 2, 2, 2, 2, 2, 2, 2, 2, 2, 2, 2, 2, 2, 2, 2, 2, 2, 2, 2, 2, 2, 2, 2, 2, 2, 2, 2, 2, 2, 2, 2, 2, 2, 2, 2, 2, 2, 2, 2, 2, 2, 2, 2, 2, 2, 2, 2, 2, 2, 2, 2, 2, 2, 2, 2, 2, 2, 2, 2, 2, 2, 2, 2, 2, 2, 2, 2, 2, 2, 2, 2, 2, 2, 2, 2, 2, 2, 2, 2, 2, 2, 2, 2, 2, 2, 2, 2, 2, 2, 2, 2, 2, 2, 2, 2, 2, 2, 2, 2, 2, 2, 2, 2, 2, 2, 2, 2, 2, 2, 2, 2, 2, 2, 2, 2, 2, 2, 2, 2, 2, 2, 2, 2, 2, 2, 2, 2, 2, 2, 2, 2, 2, 2, 2, 2, 2, 2, 2, 2, 2, 2, 2, 2, 2, 2, 2, 2, 2, 2, 2, 2, 2, 2, 2, 2, 2, 2, 2, 2, 2, 2, 2, 2, 2, 2, 2, 2, 2, 2, 2, 2, 2, 2, 2, 2, 2, 2, 2, 2, 2, 2, 2, 2, 2, 2, 2, 2, 2, 2, 2, 2, 2, 2, 2, 2, 2, 2, 2, 2, 2, 2, 2, 2, 2, 2, 2, 2, 2, 2, 2, 2, 2, 2, 2, 2, 2, 2, 2, 2, 2, 2, 2, 2, 2, 2, 2, 2, 2, 2, 2, 2, 2, 2, 2, 2, 2, 2, 2, 2, 2, 2, 2, 2, 2, 2, 2, 2, 2, 2, 2, 2, 2, 2, 2, 2, 2, 2, 2, 2, 2, 2, 2, 2, 2, 2, 2, 2, 2, 2, 2, 2, 2, 2, 2, 2, 2, 2, 2, 2, 2, 2, 2, 2, 2, 2, 2, 2, 2, 2, 2, 2, 2, 2, 2, 2, 2, 2, 2, 2, 2, 2, 2, 2, 2, 2, 2, 2, 2, 2, 2, 2, 2, 2, 2, 2, 2, 2, 2, 2, 2, 2, 2, 2, 2, 2, 2, 2, 2, 2, 2, 2, 2, 2, 2, 2, 2, 2, 2, 2, 2, 2, 2, 2, 2, 2, 2, 2, 2, 2, 2, 2, 2, 2, 2, 2, 2, 2, 2, 2, 2, 2, 2, 2, 2, 2, 2, 2, 2, 2, 2, 2, 2, 2, 2, 2, 2, 2, 2, 2, 2, 2, 2, 2, 2, 2, 2, 2, 2, 2, 2, 2, 2, 2, 2, 2, 2, 2, 2, 2, 2, 2, 2, 2, 2, 2, 2, 2, 2, 2, 2, 2, 2, 2, 2, 2, 2, 2, 2, 2, 2, 2, 2, 2, 2, 2, 2, 2, 2, 2, 2, 2, 2, 2, 2, 2, 2, 2, 2, 2, 2, 2, 2, 2, 2, 2, 2, 2, 2, 2, 2, 2, 2, 2, 2, 2, 2, 2, 2, 2, 2, 2, 2, 2, 2, 2, 2, 2, 2, 2, 2, 3 ),
 ( 0.000000000000000000, 1.000000000000000000 ),
 ( 0.000000000000000000, 0.001243781094527363160, 0.002487562189054726321, 0.003731343283582089481, 0.004975124378109452641, 0.006218905472636816235, 0.007462686567164178962, 0.008706467661691542556, 0.009950248756218905283, 0.01119402985074626801, 0.01243781094527363247, 0.01368159203980099520, 0.01492537313432835792, 0.01616915422885572065, 0.01741293532338308511, 0.01865671641791044610, 0.01990049751243781057, 0.02114427860696517503, 0.02238805970149253602, 0.02363184079601990048, 0.02487562189054726494, 0.02611940298507462593, 0.02736318407960199039, 0.02860696517412935486, 0.02985074626865671585, 0.03109452736318408031, 0.03233830845771144130, 0.03358208955223880576, 0.03482587064676617022, 0.03606965174129353469, 0.03731343283582089221, 0.03855721393034825667, 0.03980099502487562113, 0.04104477611940298559, 0.04228855721393035005, 0.04353233830845771452, 0.04477611940298507204, 0.04601990049751243650, 0.04726368159203980096, 0.04850746268656716542, 0.04975124378109452988, 0.05099502487562188741, 0.05223880597014925187, 0.05348258706467661633, 0.05472636815920398079, 0.05597014925373134525, 0.05721393034825870971, 0.05845771144278606724, 0.05970149253731343170, 0.06094527363184079616, 0.06218905472636816062, 0.06343283582089552508, 0.06467661691542288260, 0.06592039800995025400, 0.06716417910447761153, 0.06840796019900496905, 0.06965174129353234045, 0.07089552238805969797, 0.07213930348258706937, 0.07338308457711442689, 0.07462686567164178442, 0.07587064676616915582, 0.07711442786069651334, 0.07835820895522388474, 0.07960199004975124226, 0.08084577114427861366, 0.08208955223880597118, 0.08333333333333332871, 0.08457711442786070011, 0.08582089552238805763, 0.08706467661691542903, 0.08830845771144278655, 0.08955223880597014408, 0.09079601990049751548, 0.09203980099502487300, 0.09328358208955224440, 0.09452736318407960192, 0.09577114427860695944, 0.09701492537313433084, 0.09825870646766168837, 0.09950248756218905977, 0.1007462686567164173, 0.1019900497512437748, 0.1032338308457711462, 0.1044776119402985037, 0.1057213930348258751, 0.1069651741293532327, 0.1082089552238805902, 0.1094527363184079616, 0.1106965174129353191, 0.1119402985074626905, 0.1131840796019900480, 0.1144278606965174194, 0.1156716417910447769, 0.1169154228855721345, 0.1181592039800995059, 0.1194029850746268634, 0.1206467661691542348, 0.1218905472636815923, 0.1231343283582089498, 0.1243781094527363212, 0.1256218905472636926, 0.1268656716417910502, 0.1281094527363184077, 0.1293532338308457652, 0.1305970149253731227, 0.1318407960199005080, 0.1330845771144278655, 0.1343283582089552231, 0.1355721393034825806, 0.1368159203980099381, 0.1380597014925373234, 0.1393034825870646809, 0.1405472636815920384, 0.1417910447761193959, 0.1430348258706467535, 0.1442786069651741387, 0.1455223880597014963, 0.1467661691542288538, 0.1480099502487562113, 0.1492537313432835688, 0.1504975124378109541, 0.1517412935323383116, 0.1529850746268656692, 0.1542288557213930267, 0.1554726368159203842, 0.1567164179104477695, 0.1579601990049751270, 0.1592039800995024845, 0.1604477611940298420, 0.1616915422885572273, 0.1629353233830845848, 0.1641791044776119424, 0.1654228855721392999, 0.1666666666666666574, 0.1679104477611940427, 0.1691542288557214002, 0.1703980099502487577, 0.1716417910447761153, 0.1728855721393034728, 0.1741293532338308581, 0.1753731343283582156, 0.1766169154228855731, 0.1778606965174129306, 0.1791044776119402882, 0.1803482587064676734, 0.1815920398009950310, 0.1828358208955223885, 0.1840796019900497460, 0.1853233830845771035, 0.1865671641791044888, 0.1878109452736318463, 0.1890547263681592038, 0.1902985074626865614, 0.1915422885572139189, 0.1927860696517413042, 0.1940298507462686617, 0.1952736318407960192, 0.1965174129353233767, 0.1977611940298507343, 0.1990049751243781195, 0.2002487562189054771, 0.2014925373134328346, 0.2027363184079601921, 0.2039800995024875496, 0.2052238805970149349, 0.2064676616915422924, 0.2077114427860696499, 0.2089552238805970075, 0.2101990049751243650, 0.2114427860696517503, 0.2126865671641791078, 0.2139303482587064653, 0.2151741293532338228, 0.2164179104477611804, 0.2176616915422885656, 0.2189054726368159232, 0.2201492537313432807, 0.2213930348258706382, 0.2226368159203980235, 0.2238805970149253810, 0.2251243781094527385, 0.2263681592039800961, 0.2276119402985074536, 0.2288557213930348389, 0.2300995024875621964, 0.2313432835820895539, 0.2325870646766169114, 0.2338308457711442689, 0.2350746268656716542, 0.2363184079601990117, 0.2375621890547263693, 0.2388059701492537268, 0.2400497512437810843, 0.2412935323383084696, 0.2425373134328358271, 0.2437810945273631846, 0.2450248756218905422, 0.2462686567164178997, 0.2475124378109452850, 0.2487562189054726425, 0.2500000000000000000, 0.2512437810945273853, 0.2524875621890547150, 0.2537313432835821003, 0.2549751243781094301, 0.2562189054726368154, 0.2574626865671642006, 0.2587064676616915304, 0.2599502487562189157, 0.2611940298507462455, 0.2624378109452736307, 0.2636815920398010160, 0.2649253731343283458, 0.2661691542288557311, 0.2674129353233830608, 0.2686567164179104461, 0.2699004975124378314, 0.2711442786069651611, 0.2723880597014925464, 0.2736318407960198762, 0.2748756218905472615, 0.2761194029850746468, 0.2773631840796019765, 0.2786069651741293618, 0.2798507462686566916, 0.2810945273631840768, 0.2823383084577114621, 0.2835820895522387919, 0.2848258706467661772, 0.2860696517412935069, 0.2873134328358208922, 0.2885572139303482775, 0.2898009950248756073, 0.2910447761194029925, 0.2922885572139303223, 0.2935323383084577076, 0.2947761194029850929, 0.2960199004975124226, 0.2972636815920398079, 0.2985074626865671377, 0.2997512437810945229, 0.3009950248756219082, 0.3022388059701492380, 0.3034825870646766233, 0.3047263681592039530, 0.3059701492537313383, 0.3072139303482587236, 0.3084577114427860534, 0.3097014925373134386, 0.3109452736318407684, 0.3121890547263681537, 0.3134328358208955390, 0.3146766169154228687, 0.3159203980099502540, 0.3171641791044776393, 0.3184079601990049690, 0.3196517412935323543, 0.3208955223880596841, 0.3221393034825870694, 0.3233830845771144546, 0.3246268656716417844, 0.3258706467661691697, 0.3271144278606964995, 0.3283582089552238847, 0.3296019900497512700, 0.3308457711442785998, 0.3320895522388059851, 0.3333333333333333148, 0.3345771144278607001, 0.3358208955223880854, 0.3370646766169154152, 0.3383084577114428004, 0.3395522388059701302, 0.3407960199004975155, 0.3420398009950249008, 0.3432835820895522305, 0.3445273631840796158, 0.3457711442786069456, 0.3470149253731343308, 0.3482587064676617161, 0.3495024875621890459, 0.3507462686567164312, 0.3519900497512437609, 0.3532338308457711462, 0.3544776119402985315, 0.3557213930348258613, 0.3569651741293532465, 0.3582089552238805763, 0.3594527363184079616, 0.3606965174129353469, 0.3619402985074626766, 0.3631840796019900619, 0.3644278606965173917, 0.3656716417910447769, 0.3669154228855721622, 0.3681592039800994920, 0.3694029850746268773, 0.3706467661691542070, 0.3718905472636815923, 0.3731343283582089776, 0.3743781094527363074, 0.3756218905472636926, 0.3768656716417910224, 0.3781094527363184077, 0.3793532338308457930, 0.3805970149253731227, 0.3818407960199005080, 0.3830845771144278378, 0.3843283582089552231, 0.3855721393034826083, 0.3868159203980099381, 0.3880597014925373234, 0.3893034825870646531, 0.3905472636815920384, 0.3917910447761194237, 0.3930348258706467535, 0.3942786069651741387, 0.3955223880597014685, 0.3967661691542288538, 0.3980099502487562391, 0.3992537313432835688, 0.4004975124378109541, 0.4017412935323382839, 0.4029850746268656692, 0.4042288557213930544, 0.4054726368159203842, 0.4067164179104477695, 0.4079601990049750992, 0.4092039800995024845, 0.4104477611940298698, 0.4116915422885571996, 0.4129353233830845848, 0.4141791044776119146, 0.4154228855721392999, 0.4166666666666666852, 0.4179104477611940149, 0.4191542288557214002, 0.4203980099502487300, 0.4216417910447761153, 0.4228855721393035005, 0.4241293532338308303, 0.4253731343283582156, 0.4266169154228855454, 0.4278606965174129306, 0.4291044776119403159, 0.4303482587064676457, 0.4315920398009950310, 0.4328358208955223607, 0.4340796019900497460, 0.4353233830845771313, 0.4365671641791044610, 0.4378109452736318463, 0.4390547263681592316, 0.4402985074626865614, 0.4415422885572139466, 0.4427860696517412764, 0.4440298507462686617, 0.4452736318407960470, 0.4465174129353233767, 0.4477611940298507620, 0.4490049751243780918, 0.4502487562189054771, 0.4514925373134328623, 0.4527363184079601921, 0.4539800995024875774, 0.4552238805970149071, 0.4564676616915422924, 0.4577114427860696777, 0.4589552238805970075, 0.4601990049751243927, 0.4614427860696517225, 0.4626865671641791078, 0.4639303482587064931, 0.4651741293532338228, 0.4664179104477612081, 0.4676616915422885379, 0.4689054726368159232, 0.4701492537313433084, 0.4713930348258706382, 0.4726368159203980235, 0.4738805970149253532, 0.4751243781094527385, 0.4763681592039801238, 0.4776119402985074536, 0.4788557213930348389, 0.4800995024875621686, 0.4813432835820895539, 0.4825870646766169392, 0.4838308457711442689, 0.4850746268656716542, 0.4863184079601989840, 0.4875621890547263693, 0.4888059701492537545, 0.4900497512437810843, 0.4912935323383084696, 0.4925373134328357994, 0.4937810945273631846, 0.4950248756218905699, 0.4962686567164178997, 0.4975124378109452850, 0.4987562189054726147, 0.5000000000000000000, 0.5012437810945273853, 0.5024875621890547706, 0.5037313432835820448, 0.5049751243781094301, 0.5062189054726368154, 0.5074626865671642006, 0.5087064676616915859, 0.5099502487562188602, 0.5111940298507462455, 0.5124378109452736307, 0.5136815920398010160, 0.5149253731343284013, 0.5161691542288556755, 0.5174129353233830608, 0.5186567164179104461, 0.5199004975124378314, 0.5211442786069652167, 0.5223880597014924909, 0.5236318407960198762, 0.5248756218905472615, 0.5261194029850746468, 0.5273631840796020320, 0.5286069651741293063, 0.5298507462686566916, 0.5310945273631840768, 0.5323383084577114621, 0.5335820895522388474, 0.5348258706467661217, 0.5360696517412935069, 0.5373134328358208922, 0.5385572139303482775, 0.5398009950248756628, 0.5410447761194029370, 0.5422885572139303223, 0.5435323383084577076, 0.5447761194029850929, 0.5460199004975124781, 0.5472636815920397524, 0.5485074626865671377, 0.5497512437810945229, 0.5509950248756219082, 0.5522388059701492935, 0.5534825870646765678, 0.5547263681592039530, 0.5559701492537313383, 0.5572139303482587236, 0.5584577114427861089, 0.5597014925373133831, 0.5609452736318407684, 0.5621890547263681537, 0.5634328358208955390, 0.5646766169154229242, 0.5659203980099501985, 0.5671641791044775838, 0.5684079601990049690, 0.5696517412935323543, 0.5708955223880597396, 0.5721393034825870139, 0.5733830845771143991, 0.5746268656716417844, 0.5758706467661691697, 0.5771144278606965550, 0.5783582089552238292, 0.5796019900497512145, 0.5808457711442785998, 0.5820895522388059851, 0.5833333333333333703, 0.5845771144278606446, 0.5858208955223880299, 0.5870646766169154152, 0.5883084577114428004, 0.5895522388059701857, 0.5907960199004974600, 0.5920398009950248452, 0.5932835820895522305, 0.5945273631840796158, 0.5957711442786070011, 0.5970149253731342753, 0.5982587064676616606, 0.5995024875621890459, 0.6007462686567164312, 0.6019900497512438164, 0.6032338308457710907, 0.6044776119402984760, 0.6057213930348258613, 0.6069651741293532465, 0.6082089552238806318, 0.6094527363184079061, 0.6106965174129352913, 0.6119402985074626766, 0.6131840796019900619, 0.6144278606965174472, 0.6156716417910447214, 0.6169154228855721067, 0.6181592039800994920, 0.6194029850746268773, 0.6206467661691542625, 0.6218905472636815368, 0.6231343283582089221, 0.6243781094527363074, 0.6256218905472636926, 0.6268656716417910779, 0.6281094527363184632, 0.6293532338308457375, 0.6305970149253731227, 0.6318407960199005080, 0.6330845771144278933, 0.6343283582089552786, 0.6355721393034825528, 0.6368159203980099381, 0.6380597014925373234, 0.6393034825870647087, 0.6405472636815920939, 0.6417910447761193682, 0.6430348258706467535, 0.6442786069651741387, 0.6455223880597015240, 0.6467661691542289093, 0.6480099502487561836, 0.6492537313432835688, 0.6504975124378109541, 0.6517412935323383394, 0.6529850746268657247, 0.6542288557213929989, 0.6554726368159203842, 0.6567164179104477695, 0.6579601990049751548, 0.6592039800995025400, 0.6604477611940298143, 0.6616915422885571996, 0.6629353233830845848, 0.6641791044776119701, 0.6654228855721393554, 0.6666666666666666297, 0.6679104477611940149, 0.6691542288557214002, 0.6703980099502487855, 0.6716417910447761708, 0.6728855721393034450, 0.6741293532338308303, 0.6753731343283582156, 0.6766169154228856009, 0.6778606965174129861, 0.6791044776119402604, 0.6803482587064676457, 0.6815920398009950310, 0.6828358208955224162, 0.6840796019900498015, 0.6853233830845770758, 0.6865671641791044610, 0.6878109452736318463, 0.6890547263681592316, 0.6902985074626866169, 0.6915422885572138911, 0.6927860696517412764, 0.6940298507462686617, 0.6952736318407960470, 0.6965174129353234322, 0.6977611940298507065, 0.6990049751243780918, 0.7002487562189054771, 0.7014925373134328623, 0.7027363184079602476, 0.7039800995024875219, 0.7052238805970149071, 0.7064676616915422924, 0.7077114427860696777, 0.7089552238805970630, 0.7101990049751243372, 0.7114427860696517225, 0.7126865671641791078, 0.7139303482587064931, 0.7151741293532338783, 0.7164179104477611526, 0.7176616915422885379, 0.7189054726368159232, 0.7201492537313433084, 0.7213930348258706937, 0.7226368159203979680, 0.7238805970149253532, 0.7251243781094527385, 0.7263681592039801238, 0.7276119402985075091, 0.7288557213930347833, 0.7300995024875621686, 0.7313432835820895539, 0.7325870646766169392, 0.7338308457711443245, 0.7350746268656715987, 0.7363184079601989840, 0.7375621890547263693, 0.7388059701492537545, 0.7400497512437811398, 0.7412935323383084141, 0.7425373134328357994, 0.7437810945273631846, 0.7450248756218905699, 0.7462686567164179552, 0.7475124378109452294, 0.7487562189054726147, 0.7500000000000000000, 0.7512437810945273853, 0.7524875621890547706, 0.7537313432835820448, 0.7549751243781094301, 0.7562189054726368154, 0.7574626865671642006, 0.7587064676616915859, 0.7599502487562188602, 0.7611940298507462455, 0.7624378109452736307, 0.7636815920398010160, 0.7649253731343284013, 0.7661691542288556755, 0.7674129353233830608, 0.7686567164179104461, 0.7699004975124378314, 0.7711442786069652167, 0.7723880597014924909, 0.7736318407960198762, 0.7748756218905472615, 0.7761194029850746468, 0.7773631840796020320, 0.7786069651741293063, 0.7798507462686566916, 0.7810945273631840768, 0.7823383084577114621, 0.7835820895522388474, 0.7848258706467661217, 0.7860696517412935069, 0.7873134328358208922, 0.7885572139303482775, 0.7898009950248756628, 0.7910447761194029370, 0.7922885572139303223, 0.7935323383084577076, 0.7947761194029850929, 0.7960199004975124781, 0.7972636815920397524, 0.7985074626865671377, 0.7997512437810945229, 0.8009950248756219082, 0.8022388059701492935, 0.8034825870646765678, 0.8047263681592039530, 0.8059701492537313383, 0.8072139303482587236, 0.8084577114427861089, 0.8097014925373133831, 0.8109452736318407684, 0.8121890547263681537, 0.8134328358208955390, 0.8146766169154229242, 0.8159203980099501985, 0.8171641791044775838, 0.8184079601990049690, 0.8196517412935323543, 0.8208955223880597396, 0.8221393034825870139, 0.8233830845771143991, 0.8246268656716417844, 0.8258706467661691697, 0.8271144278606965550, 0.8283582089552238292, 0.8296019900497512145, 0.8308457711442785998, 0.8320895522388059851, 0.8333333333333333703, 0.8345771144278606446, 0.8358208955223880299, 0.8370646766169154152, 0.8383084577114428004, 0.8395522388059701857, 0.8407960199004974600, 0.8420398009950248452, 0.8432835820895522305, 0.8445273631840796158, 0.8457711442786070011, 0.8470149253731342753, 0.8482587064676616606, 0.8495024875621890459, 0.8507462686567164312, 0.8519900497512438164, 0.8532338308457710907, 0.8544776119402984760, 0.8557213930348258613, 0.8569651741293532465, 0.8582089552238806318, 0.8594527363184079061, 0.8606965174129352913, 0.8619402985074626766, 0.8631840796019900619, 0.8644278606965174472, 0.8656716417910447214, 0.8669154228855721067, 0.8681592039800994920, 0.8694029850746268773, 0.8706467661691542625, 0.8718905472636815368, 0.8731343283582089221, 0.8743781094527363074, 0.8756218905472636926, 0.8768656716417910779, 0.8781094527363184632, 0.8793532338308457375, 0.8805970149253731227, 0.8818407960199005080, 0.8830845771144278933, 0.8843283582089552786, 0.8855721393034825528, 0.8868159203980099381, 0.8880597014925373234, 0.8893034825870647087, 0.8905472636815920939, 0.8917910447761193682, 0.8930348258706467535, 0.8942786069651741387, 0.8955223880597015240, 0.8967661691542289093, 0.8980099502487561836, 0.8992537313432835688, 0.9004975124378109541, 0.9017412935323383394, 0.9029850746268657247, 0.9042288557213929989, 0.9054726368159203842, 0.9067164179104477695, 0.9079601990049751548, 0.9092039800995025400, 0.9104477611940298143, 0.9116915422885571996, 0.9129353233830845848, 0.9141791044776119701, 0.9154228855721393554, 0.9166666666666666297, 0.9179104477611940149, 0.9191542288557214002, 0.9203980099502487855, 0.9216417910447761708, 0.9228855721393034450, 0.9241293532338308303, 0.9253731343283582156, 0.9266169154228856009, 0.9278606965174129861, 0.9291044776119402604, 0.9303482587064676457, 0.9315920398009950310, 0.9328358208955224162, 0.9340796019900498015, 0.9353233830845770758, 0.9365671641791044610, 0.9378109452736318463, 0.9390547263681592316, 0.9402985074626866169, 0.9415422885572138911, 0.9427860696517412764, 0.9440298507462686617, 0.9452736318407960470, 0.9465174129353234322, 0.9477611940298507065, 0.9490049751243780918, 0.9502487562189054771, 0.9514925373134328623, 0.9527363184079602476, 0.9539800995024875219, 0.9552238805970149071, 0.9564676616915422924, 0.9577114427860696777, 0.9589552238805970630, 0.9601990049751243372, 0.9614427860696517225, 0.9626865671641791078, 0.9639303482587064931, 0.9651741293532338783, 0.9664179104477611526, 0.9676616915422885379, 0.9689054726368159232, 0.9701492537313433084, 0.9713930348258706937, 0.9726368159203979680, 0.9738805970149253532, 0.9751243781094527385, 0.9763681592039801238, 0.9776119402985075091, 0.9788557213930347833, 0.9800995024875621686, 0.9813432835820895539, 0.9825870646766169392, 0.9838308457711443245, 0.9850746268656715987, 0.9863184079601989840, 0.9875621890547263693, 0.9888059701492537545, 0.9900497512437811398, 0.9912935323383084141, 0.9925373134328357994, 0.9937810945273631846, 0.9950248756218905699 ),
 .UNSPECIFIED. ) 
 GEOMETRIC_REPRESENTATION_ITEM ( )  RATIONAL_B_SPLINE_SURFACE ( (
 ( 1.000000000000000000, 0.8660254037844387076, 1.000000000000000000, 0.8660254037844387076, 1.000000000000000000, 0.8660254037844387076, 1.000000000000000000, 0.8660254037844387076, 1.000000000000000000, 0.8660254037844387076, 1.000000000000000000, 0.8660254037844387076, 1.000000000000000000, 0.8660254037844387076, 1.000000000000000000, 0.8660254037844387076, 1.000000000000000000, 0.8660254037844387076, 1.000000000000000000, 0.8660254037844387076, 1.000000000000000000, 0.8660254037844387076, 1.000000000000000000, 0.8660254037844387076, 1.000000000000000000, 0.8660254037844387076, 1.000000000000000000, 0.8660254037844387076, 1.000000000000000000, 0.8660254037844387076, 1.000000000000000000, 0.8660254037844387076, 1.000000000000000000, 0.8660254037844387076, 1.000000000000000000, 0.8660254037844387076, 1.000000000000000000, 0.8660254037844387076, 1.000000000000000000, 0.8660254037844387076, 1.000000000000000000, 0.8660254037844387076, 1.000000000000000000, 0.8660254037844387076, 1.000000000000000000, 0.8660254037844387076, 1.000000000000000000, 0.8660254037844387076, 1.000000000000000000, 0.8660254037844387076, 1.000000000000000000, 0.8660254037844387076, 1.000000000000000000, 0.8660254037844387076, 1.000000000000000000, 0.8660254037844387076, 1.000000000000000000, 0.8660254037844387076, 1.000000000000000000, 0.8660254037844387076, 1.000000000000000000, 0.8660254037844387076, 1.000000000000000000, 0.8660254037844387076, 1.000000000000000000, 0.8660254037844387076, 1.000000000000000000, 0.8660254037844387076, 1.000000000000000000, 0.8660254037844387076, 1.000000000000000000, 0.8660254037844387076, 1.000000000000000000, 0.8660254037844387076, 1.000000000000000000, 0.8660254037844387076, 1.000000000000000000, 0.8660254037844387076, 1.000000000000000000, 0.8660254037844387076, 1.000000000000000000, 0.8660254037844387076, 1.000000000000000000, 0.8660254037844387076, 1.000000000000000000, 0.8660254037844387076, 1.000000000000000000, 0.8660254037844387076, 1.000000000000000000, 0.8660254037844387076, 1.000000000000000000, 0.8660254037844387076, 1.000000000000000000, 0.8660254037844387076, 1.000000000000000000, 0.8660254037844387076, 1.000000000000000000, 0.8660254037844387076, 1.000000000000000000, 0.8660254037844387076, 1.000000000000000000, 0.8660254037844387076, 1.000000000000000000, 0.8660254037844387076, 1.000000000000000000, 0.8660254037844387076, 1.000000000000000000, 0.8660254037844387076, 1.000000000000000000, 0.8660254037844387076, 1.000000000000000000, 0.8660254037844387076, 1.000000000000000000, 0.8660254037844387076, 1.000000000000000000, 0.8660254037844387076, 1.000000000000000000, 0.8660254037844387076, 1.000000000000000000, 0.8660254037844387076, 1.000000000000000000, 0.8660254037844387076, 1.000000000000000000, 0.8660254037844387076, 1.000000000000000000, 0.8660254037844387076, 1.000000000000000000, 0.8660254037844387076, 1.000000000000000000, 0.8660254037844387076, 1.000000000000000000, 0.8660254037844387076, 1.000000000000000000, 0.8660254037844387076, 1.000000000000000000, 0.8660254037844387076, 1.000000000000000000, 0.8660254037844387076, 1.000000000000000000, 0.8660254037844387076, 1.000000000000000000, 0.8660254037844387076, 1.000000000000000000, 0.8660254037844387076, 1.000000000000000000, 0.8660254037844387076, 1.000000000000000000, 0.8660254037844387076, 1.000000000000000000, 0.8660254037844387076, 1.000000000000000000, 0.8660254037844387076, 1.000000000000000000, 0.8660254037844387076, 1.000000000000000000, 0.8660254037844387076, 1.000000000000000000, 0.8660254037844387076, 1.000000000000000000, 0.8660254037844387076, 1.000000000000000000, 0.8660254037844387076, 1.000000000000000000, 0.8660254037844387076, 1.000000000000000000, 0.8660254037844387076, 1.000000000000000000, 0.8660254037844387076, 1.000000000000000000, 0.8660254037844387076, 1.000000000000000000, 0.8660254037844387076, 1.000000000000000000, 0.8660254037844387076, 1.000000000000000000, 0.8660254037844387076, 1.000000000000000000, 0.8660254037844387076, 1.000000000000000000, 0.8660254037844387076, 1.000000000000000000, 0.8660254037844387076, 1.000000000000000000, 0.8660254037844387076, 1.000000000000000000, 0.8660254037844387076, 1.000000000000000000, 0.8660254037844387076, 1.000000000000000000, 0.8660254037844387076, 1.000000000000000000, 0.8660254037844387076, 1.000000000000000000, 0.8660254037844387076, 1.000000000000000000, 0.8660254037844387076, 1.000000000000000000, 0.8660254037844387076, 1.000000000000000000, 0.8660254037844387076, 1.000000000000000000, 0.8660254037844387076, 1.000000000000000000, 0.8660254037844387076, 1.000000000000000000, 0.8660254037844387076, 1.000000000000000000, 0.8660254037844387076, 1.000000000000000000, 0.8660254037844387076, 1.000000000000000000, 0.8660254037844387076, 1.000000000000000000, 0.8660254037844387076, 1.000000000000000000, 0.8660254037844387076, 1.000000000000000000, 0.8660254037844387076, 1.000000000000000000, 0.8660254037844387076, 1.000000000000000000, 0.8660254037844387076, 1.000000000000000000, 0.8660254037844387076, 1.000000000000000000, 0.8660254037844387076, 1.000000000000000000, 0.8660254037844387076, 1.000000000000000000, 0.8660254037844387076, 1.000000000000000000, 0.8660254037844387076, 1.000000000000000000, 0.8660254037844387076, 1.000000000000000000, 0.8660254037844387076, 1.000000000000000000, 0.8660254037844387076, 1.000000000000000000, 0.8660254037844387076, 1.000000000000000000, 0.8660254037844387076, 1.000000000000000000, 0.8660254037844387076, 1.000000000000000000, 0.8660254037844387076, 1.000000000000000000, 0.8660254037844387076, 1.000000000000000000, 0.8660254037844387076, 1.000000000000000000, 0.8660254037844387076, 1.000000000000000000, 0.8660254037844387076, 1.000000000000000000, 0.8660254037844387076, 1.000000000000000000, 0.8660254037844387076, 1.000000000000000000, 0.8660254037844387076, 1.000000000000000000, 0.8660254037844387076, 1.000000000000000000, 0.8660254037844387076, 1.000000000000000000, 0.8660254037844387076, 1.000000000000000000, 0.8660254037844387076, 1.000000000000000000, 0.8660254037844387076, 1.000000000000000000, 0.8660254037844387076, 1.000000000000000000, 0.8660254037844387076, 1.000000000000000000, 0.8660254037844387076, 1.000000000000000000, 0.8660254037844387076, 1.000000000000000000, 0.8660254037844387076, 1.000000000000000000, 0.8660254037844387076, 1.000000000000000000, 0.8660254037844387076, 1.000000000000000000, 0.8660254037844387076, 1.000000000000000000, 0.8660254037844387076, 1.000000000000000000, 0.8660254037844387076, 1.000000000000000000, 0.8660254037844387076, 1.000000000000000000, 0.8660254037844387076, 1.000000000000000000, 0.8660254037844387076, 1.000000000000000000, 0.8660254037844387076, 1.000000000000000000, 0.8660254037844387076, 1.000000000000000000, 0.8660254037844387076, 1.000000000000000000, 0.8660254037844387076, 1.000000000000000000, 0.8660254037844387076, 1.000000000000000000, 0.8660254037844387076, 1.000000000000000000, 0.8660254037844387076, 1.000000000000000000, 0.8660254037844387076, 1.000000000000000000, 0.8660254037844387076, 1.000000000000000000, 0.8660254037844387076, 1.000000000000000000, 0.8660254037844387076, 1.000000000000000000, 0.8660254037844387076, 1.000000000000000000, 0.8660254037844387076, 1.000000000000000000, 0.8660254037844387076, 1.000000000000000000, 0.8660254037844387076, 1.000000000000000000, 0.8660254037844387076, 1.000000000000000000, 0.8660254037844387076, 1.000000000000000000, 0.8660254037844387076, 1.000000000000000000, 0.8660254037844387076, 1.000000000000000000, 0.8660254037844387076, 1.000000000000000000, 0.8660254037844387076, 1.000000000000000000, 0.8660254037844387076, 1.000000000000000000, 0.8660254037844387076, 1.000000000000000000, 0.8660254037844387076, 1.000000000000000000, 0.8660254037844387076, 1.000000000000000000, 0.8660254037844387076, 1.000000000000000000, 0.8660254037844387076, 1.000000000000000000, 0.8660254037844387076, 1.000000000000000000, 0.8660254037844387076, 1.000000000000000000, 0.8660254037844387076, 1.000000000000000000, 0.8660254037844387076, 1.000000000000000000, 0.8660254037844387076, 1.000000000000000000, 0.8660254037844387076, 1.000000000000000000, 0.8660254037844387076, 1.000000000000000000, 0.8660254037844387076, 1.000000000000000000, 0.8660254037844387076, 1.000000000000000000, 0.8660254037844387076, 1.000000000000000000, 0.8660254037844387076, 1.000000000000000000, 0.8660254037844387076, 1.000000000000000000, 0.8660254037844387076, 1.000000000000000000, 0.8660254037844387076, 1.000000000000000000, 0.8660254037844387076, 1.000000000000000000, 0.8660254037844387076, 1.000000000000000000, 0.8660254037844387076, 1.000000000000000000, 0.8660254037844387076, 1.000000000000000000, 0.8660254037844387076, 1.000000000000000000, 0.8660254037844387076, 1.000000000000000000, 0.8660254037844387076, 1.000000000000000000, 0.8660254037844387076, 1.000000000000000000, 0.8660254037844387076, 1.000000000000000000, 0.8660254037844387076, 1.000000000000000000, 0.8660254037844387076, 1.000000000000000000, 0.8660254037844387076, 1.000000000000000000, 0.8660254037844387076, 1.000000000000000000, 0.8660254037844387076, 1.000000000000000000, 0.8660254037844387076, 1.000000000000000000, 0.8660254037844387076, 1.000000000000000000, 0.8660254037844387076, 1.000000000000000000, 0.8660254037844387076, 1.000000000000000000, 0.8660254037844387076, 1.000000000000000000, 0.8660254037844387076, 1.000000000000000000, 0.8660254037844387076, 1.000000000000000000, 0.8660254037844387076, 1.000000000000000000, 0.8660254037844387076, 1.000000000000000000, 0.8660254037844387076, 1.000000000000000000, 0.8660254037844387076, 1.000000000000000000, 0.8660254037844387076, 1.000000000000000000, 0.8660254037844387076, 1.000000000000000000, 0.8660254037844387076, 1.000000000000000000, 0.8660254037844387076, 1.000000000000000000, 0.8660254037844387076, 1.000000000000000000, 0.8660254037844387076, 1.000000000000000000, 0.8660254037844387076, 1.000000000000000000, 0.8660254037844387076, 1.000000000000000000, 0.8660254037844387076, 1.000000000000000000, 0.8660254037844387076, 1.000000000000000000, 0.8660254037844387076, 1.000000000000000000, 0.8660254037844387076, 1.000000000000000000, 0.8660254037844387076, 1.000000000000000000, 0.8660254037844387076, 1.000000000000000000, 0.8660254037844387076, 1.000000000000000000, 0.8660254037844387076, 1.000000000000000000, 0.8660254037844387076, 1.000000000000000000, 0.8660254037844387076, 1.000000000000000000, 0.8660254037844387076, 1.000000000000000000, 0.8660254037844387076, 1.000000000000000000, 0.8660254037844387076, 1.000000000000000000, 0.8660254037844387076, 1.000000000000000000, 0.8660254037844387076, 1.000000000000000000, 0.8660254037844387076, 1.000000000000000000, 0.8660254037844387076, 1.000000000000000000, 0.8660254037844387076, 1.000000000000000000, 0.8660254037844387076, 1.000000000000000000, 0.8660254037844387076, 1.000000000000000000, 0.8660254037844387076, 1.000000000000000000, 0.8660254037844387076, 1.000000000000000000, 0.8660254037844387076, 1.000000000000000000, 0.8660254037844387076, 1.000000000000000000, 0.8660254037844387076, 1.000000000000000000, 0.8660254037844387076, 1.000000000000000000, 0.8660254037844387076, 1.000000000000000000, 0.8660254037844387076, 1.000000000000000000, 0.8660254037844387076, 1.000000000000000000, 0.8660254037844387076, 1.000000000000000000, 0.8660254037844387076, 1.000000000000000000, 0.8660254037844387076, 1.000000000000000000, 0.8660254037844387076, 1.000000000000000000, 0.8660254037844387076, 1.000000000000000000, 0.8660254037844387076, 1.000000000000000000, 0.8660254037844387076, 1.000000000000000000, 0.8660254037844387076, 1.000000000000000000, 0.8660254037844387076, 1.000000000000000000, 0.8660254037844387076, 1.000000000000000000, 0.8660254037844387076, 1.000000000000000000, 0.8660254037844387076, 1.000000000000000000, 0.8660254037844387076, 1.000000000000000000, 0.8660254037844387076, 1.000000000000000000, 0.8660254037844387076, 1.000000000000000000, 0.8660254037844387076, 1.000000000000000000, 0.8660254037844387076, 1.000000000000000000, 0.8660254037844387076, 1.000000000000000000, 0.8660254037844387076, 1.000000000000000000, 0.8660254037844387076, 1.000000000000000000, 0.8660254037844387076, 1.000000000000000000, 0.8660254037844387076, 1.000000000000000000, 0.8660254037844387076, 1.000000000000000000, 0.8660254037844387076, 1.000000000000000000, 0.8660254037844387076, 1.000000000000000000, 0.8660254037844387076, 1.000000000000000000, 0.8660254037844387076, 1.000000000000000000, 0.8660254037844387076, 1.000000000000000000, 0.8660254037844387076, 1.000000000000000000, 0.8660254037844387076, 1.000000000000000000, 0.8660254037844387076, 1.000000000000000000, 0.8660254037844387076, 1.000000000000000000, 0.8660254037844387076, 1.000000000000000000, 0.8660254037844387076, 1.000000000000000000, 0.8660254037844387076, 1.000000000000000000, 0.8660254037844387076, 1.000000000000000000, 0.8660254037844387076, 1.000000000000000000, 0.8660254037844387076, 1.000000000000000000, 0.8660254037844387076, 1.000000000000000000, 0.8660254037844387076, 1.000000000000000000, 0.8660254037844387076, 1.000000000000000000, 0.8660254037844387076, 1.000000000000000000, 0.8660254037844387076, 1.000000000000000000, 0.8660254037844387076, 1.000000000000000000, 0.8660254037844387076, 1.000000000000000000, 0.8660254037844387076, 1.000000000000000000, 0.8660254037844387076, 1.000000000000000000, 0.8660254037844387076, 1.000000000000000000, 0.8660254037844387076, 1.000000000000000000, 0.8660254037844387076, 1.000000000000000000, 0.8660254037844387076, 1.000000000000000000, 0.8660254037844387076, 1.000000000000000000, 0.8660254037844387076, 1.000000000000000000, 0.8660254037844387076, 1.000000000000000000, 0.8660254037844387076, 1.000000000000000000, 0.8660254037844387076, 1.000000000000000000, 0.8660254037844387076, 1.000000000000000000, 0.8660254037844387076, 1.000000000000000000, 0.8660254037844387076, 1.000000000000000000, 0.8660254037844387076, 1.000000000000000000, 0.8660254037844387076, 1.000000000000000000, 0.8660254037844387076, 1.000000000000000000, 0.8660254037844387076, 1.000000000000000000, 0.8660254037844387076, 1.000000000000000000, 0.8660254037844387076, 1.000000000000000000, 0.8660254037844387076, 1.000000000000000000, 0.8660254037844387076, 1.000000000000000000, 0.8660254037844387076, 1.000000000000000000, 0.8660254037844387076, 1.000000000000000000, 0.8660254037844387076, 1.000000000000000000, 0.8660254037844387076, 1.000000000000000000, 0.8660254037844387076, 1.000000000000000000, 0.8660254037844387076, 1.000000000000000000, 0.8660254037844387076, 1.000000000000000000, 0.8660254037844387076, 1.000000000000000000, 0.8660254037844387076, 1.000000000000000000, 0.8660254037844387076, 1.000000000000000000, 0.8660254037844387076, 1.000000000000000000, 0.8660254037844387076, 1.000000000000000000, 0.8660254037844387076, 1.000000000000000000, 0.8660254037844387076, 1.000000000000000000, 0.8660254037844387076, 1.000000000000000000, 0.8660254037844387076, 1.000000000000000000, 0.8660254037844387076, 1.000000000000000000, 0.8660254037844387076, 1.000000000000000000, 0.8660254037844387076, 1.000000000000000000, 0.8660254037844387076, 1.000000000000000000, 0.8660254037844387076, 1.000000000000000000, 0.8660254037844387076, 1.000000000000000000, 0.8660254037844387076, 1.000000000000000000, 0.8660254037844387076, 1.000000000000000000, 0.8660254037844387076, 1.000000000000000000, 0.8660254037844387076, 1.000000000000000000, 0.8660254037844387076, 1.000000000000000000, 0.8660254037844387076, 1.000000000000000000, 0.8660254037844387076, 1.000000000000000000, 0.8660254037844387076, 1.000000000000000000, 0.8660254037844387076, 1.000000000000000000, 0.8660254037844387076, 1.000000000000000000, 0.8660254037844387076, 1.000000000000000000, 0.8660254037844387076, 1.000000000000000000, 0.8660254037844387076, 1.000000000000000000, 0.8660254037844387076, 1.000000000000000000, 0.8660254037844387076, 1.000000000000000000, 0.8660254037844387076, 1.000000000000000000, 0.8660254037844387076, 1.000000000000000000, 0.8660254037844387076, 1.000000000000000000, 0.8660254037844387076, 1.000000000000000000, 0.8660254037844387076, 1.000000000000000000, 0.8660254037844387076, 1.000000000000000000, 0.8660254037844387076, 1.000000000000000000, 0.8660254037844387076, 1.000000000000000000, 0.8660254037844387076, 1.000000000000000000, 0.8660254037844387076, 1.000000000000000000, 0.8660254037844387076, 1.000000000000000000, 0.8660254037844387076, 1.000000000000000000, 0.8660254037844387076, 1.000000000000000000, 0.8660254037844387076, 1.000000000000000000, 0.8660254037844387076, 1.000000000000000000, 0.8660254037844387076, 1.000000000000000000, 0.8660254037844387076, 1.000000000000000000, 0.8660254037844387076, 1.000000000000000000, 0.8660254037844387076, 1.000000000000000000, 0.8660254037844387076, 1.000000000000000000, 0.8660254037844387076, 1.000000000000000000, 0.8660254037844387076, 1.000000000000000000, 0.8660254037844387076, 1.000000000000000000, 0.8660254037844387076, 1.000000000000000000, 0.8660254037844387076, 1.000000000000000000, 0.8660254037844387076, 1.000000000000000000, 0.8660254037844387076, 1.000000000000000000, 0.8660254037844387076, 1.000000000000000000, 0.8660254037844387076, 1.000000000000000000, 0.8660254037844387076, 1.000000000000000000, 0.8660254037844387076, 1.000000000000000000, 0.8660254037844387076, 1.000000000000000000, 0.8660254037844387076, 1.000000000000000000, 0.8660254037844387076, 1.000000000000000000, 0.8660254037844387076, 1.000000000000000000, 0.8660254037844387076, 1.000000000000000000, 0.8660254037844387076, 1.000000000000000000, 0.8660254037844387076, 1.000000000000000000, 0.8660254037844387076, 1.000000000000000000, 0.8660254037844387076, 1.000000000000000000, 0.8660254037844387076, 1.000000000000000000, 0.8660254037844387076, 1.000000000000000000, 0.8660254037844387076, 1.000000000000000000, 0.8660254037844387076, 1.000000000000000000, 0.8660254037844387076, 1.000000000000000000, 0.8660254037844387076, 1.000000000000000000, 0.8660254037844387076, 1.000000000000000000, 0.8660254037844387076, 1.000000000000000000, 0.8660254037844387076, 1.000000000000000000, 0.8660254037844387076, 1.000000000000000000, 0.8660254037844387076, 1.000000000000000000, 0.8660254037844387076, 1.000000000000000000, 0.8660254037844387076, 1.000000000000000000, 0.8660254037844387076, 1.000000000000000000, 0.8660254037844387076, 1.000000000000000000, 0.8660254037844387076, 1.000000000000000000, 0.8660254037844387076, 1.000000000000000000, 0.8660254037844387076, 1.000000000000000000, 0.8660254037844387076, 1.000000000000000000, 0.8660254037844387076, 1.000000000000000000, 0.8660254037844387076, 1.000000000000000000, 0.8660254037844387076, 1.000000000000000000, 0.8660254037844387076, 1.000000000000000000, 0.8660254037844387076, 1.000000000000000000, 0.8660254037844387076, 1.000000000000000000, 0.8660254037844387076, 1.000000000000000000, 0.8660254037844387076, 1.000000000000000000, 0.8660254037844387076, 1.000000000000000000, 0.8660254037844387076, 1.000000000000000000, 0.8660254037844387076, 1.000000000000000000, 0.8660254037844387076, 1.000000000000000000, 0.8660254037844387076, 1.000000000000000000, 0.8660254037844387076, 1.000000000000000000, 0.8660254037844387076, 1.000000000000000000, 0.8660254037844387076, 1.000000000000000000, 0.8660254037844387076, 1.000000000000000000, 0.8660254037844387076, 1.000000000000000000, 0.8660254037844387076, 1.000000000000000000, 0.8660254037844387076, 1.000000000000000000, 0.8660254037844387076, 1.000000000000000000, 0.8660254037844387076, 1.000000000000000000, 0.8660254037844387076, 1.000000000000000000, 0.8660254037844387076, 1.000000000000000000, 0.8660254037844387076, 1.000000000000000000, 0.8660254037844387076, 1.000000000000000000, 0.8660254037844387076, 1.000000000000000000, 0.8660254037844387076, 1.000000000000000000, 0.8660254037844387076, 1.000000000000000000, 0.8660254037844387076, 1.000000000000000000, 0.8660254037844387076, 1.000000000000000000, 0.8660254037844387076, 1.000000000000000000, 0.8660254037844387076, 1.000000000000000000, 0.8660254037844387076, 1.000000000000000000, 0.8660254037844387076, 1.000000000000000000, 0.8660254037844387076, 1.000000000000000000, 0.8660254037844387076, 1.000000000000000000, 0.8660254037844387076, 1.000000000000000000, 0.8660254037844387076, 1.000000000000000000, 0.8660254037844387076, 1.000000000000000000, 0.8660254037844387076, 1.000000000000000000, 0.8660254037844387076, 1.000000000000000000, 0.8660254037844387076, 1.000000000000000000, 0.8660254037844387076, 1.000000000000000000, 0.8660254037844387076, 1.000000000000000000, 0.8660254037844387076, 1.000000000000000000, 0.8660254037844387076, 1.000000000000000000, 0.8660254037844387076, 1.000000000000000000, 0.8660254037844387076, 1.000000000000000000, 0.8660254037844387076, 1.000000000000000000, 0.8660254037844387076, 1.000000000000000000, 0.8660254037844387076, 1.000000000000000000, 0.8660254037844387076, 1.000000000000000000, 0.8660254037844387076, 1.000000000000000000, 0.8660254037844387076, 1.000000000000000000, 0.8660254037844387076, 1.000000000000000000, 0.8660254037844387076, 1.000000000000000000, 0.8660254037844387076, 1.000000000000000000, 0.8660254037844387076, 1.000000000000000000, 0.8660254037844387076, 1.000000000000000000, 0.8660254037844387076, 1.000000000000000000, 0.8660254037844387076, 1.000000000000000000, 0.8660254037844387076, 1.000000000000000000, 0.8660254037844387076, 1.000000000000000000, 0.8660254037844387076, 1.000000000000000000, 0.8660254037844387076, 1.000000000000000000, 0.8660254037844387076, 1.000000000000000000, 0.8660254037844387076, 1.000000000000000000, 0.8660254037844387076, 1.000000000000000000, 0.8660254037844387076, 1.000000000000000000, 0.8660254037844387076, 1.000000000000000000, 0.8660254037844387076, 1.000000000000000000, 0.8660254037844387076, 1.000000000000000000, 0.8660254037844387076, 1.000000000000000000, 0.8660254037844387076, 1.000000000000000000, 0.8660254037844387076, 1.000000000000000000, 0.8660254037844387076, 1.000000000000000000, 0.8660254037844387076, 1.000000000000000000, 0.8660254037844387076, 1.000000000000000000, 0.8660254037844387076, 1.000000000000000000, 0.8660254037844387076, 1.000000000000000000, 0.8660254037844387076, 1.000000000000000000, 0.8660254037844387076, 1.000000000000000000, 0.8660254037844387076, 1.000000000000000000, 0.8660254037844387076, 1.000000000000000000, 0.8660254037844387076, 1.000000000000000000, 0.8660254037844387076, 1.000000000000000000, 0.8660254037844387076, 1.000000000000000000, 0.8660254037844387076, 1.000000000000000000, 0.8660254037844387076, 1.000000000000000000, 0.8660254037844387076, 1.000000000000000000, 0.8660254037844387076, 1.000000000000000000, 0.8660254037844387076, 1.000000000000000000, 0.8660254037844387076, 1.000000000000000000, 0.8660254037844387076, 1.000000000000000000, 0.8660254037844387076, 1.000000000000000000, 0.8660254037844387076, 1.000000000000000000, 0.8660254037844387076, 1.000000000000000000, 0.8660254037844387076, 1.000000000000000000, 0.8660254037844387076, 1.000000000000000000, 0.8660254037844387076, 1.000000000000000000, 0.8660254037844387076, 1.000000000000000000, 0.8660254037844387076, 1.000000000000000000, 0.8660254037844387076, 1.000000000000000000, 0.8660254037844387076, 1.000000000000000000, 0.8660254037844387076, 1.000000000000000000, 0.8660254037844387076, 1.000000000000000000, 0.8660254037844387076, 1.000000000000000000, 0.8660254037844387076, 1.000000000000000000, 0.8660254037844387076, 1.000000000000000000, 0.8660254037844387076, 1.000000000000000000, 0.8660254037844387076, 1.000000000000000000, 0.8660254037844387076, 1.000000000000000000, 0.8660254037844387076, 1.000000000000000000, 0.8660254037844387076, 1.000000000000000000, 0.8660254037844387076, 1.000000000000000000, 0.8660254037844387076, 1.000000000000000000, 0.8660254037844387076, 1.000000000000000000, 0.8660254037844387076, 1.000000000000000000, 0.8660254037844387076, 1.000000000000000000, 0.8660254037844387076, 1.000000000000000000, 0.8660254037844387076, 1.000000000000000000, 0.8660254037844387076, 1.000000000000000000, 0.8660254037844387076, 1.000000000000000000, 0.8660254037844387076, 1.000000000000000000, 0.8660254037844387076, 1.000000000000000000, 0.8660254037844387076, 1.000000000000000000, 0.8660254037844387076, 1.000000000000000000, 0.8660254037844387076, 1.000000000000000000, 0.8660254037844387076, 1.000000000000000000, 0.8660254037844387076, 1.000000000000000000, 0.8660254037844387076, 1.000000000000000000, 0.8660254037844387076, 1.000000000000000000, 0.8660254037844387076, 1.000000000000000000, 0.8660254037844387076, 1.000000000000000000, 0.8660254037844387076, 1.000000000000000000, 0.8660254037844387076, 1.000000000000000000, 0.8660254037844387076, 1.000000000000000000, 0.8660254037844387076, 1.000000000000000000, 0.8660254037844387076, 1.000000000000000000, 0.8660254037844387076, 1.000000000000000000, 0.8660254037844387076, 1.000000000000000000, 0.8660254037844387076, 1.000000000000000000, 0.8660254037844387076, 1.000000000000000000, 0.8660254037844387076, 1.000000000000000000, 0.8660254037844387076, 1.000000000000000000, 0.8660254037844387076, 1.000000000000000000, 0.8660254037844387076, 1.000000000000000000, 0.8660254037844387076, 1.000000000000000000, 0.8660254037844387076, 1.000000000000000000, 0.8660254037844387076, 1.000000000000000000, 0.8660254037844387076, 1.000000000000000000, 0.8660254037844387076, 1.000000000000000000, 0.8660254037844387076, 1.000000000000000000, 0.8660254037844387076, 1.000000000000000000, 0.8660254037844387076, 1.000000000000000000, 0.8660254037844387076, 1.000000000000000000, 0.8660254037844387076, 1.000000000000000000, 0.8660254037844387076, 1.000000000000000000, 0.8660254037844387076, 1.000000000000000000, 0.8660254037844387076, 1.000000000000000000, 0.8660254037844387076, 1.000000000000000000, 0.8660254037844387076, 1.000000000000000000, 0.8660254037844387076, 1.000000000000000000, 0.8660254037844387076, 1.000000000000000000, 0.8660254037844387076, 1.000000000000000000, 0.8660254037844387076, 1.000000000000000000, 0.8660254037844387076, 1.000000000000000000, 0.8660254037844387076, 1.000000000000000000, 0.8660254037844387076, 1.000000000000000000, 0.8660254037844387076, 1.000000000000000000, 0.8660254037844387076, 1.000000000000000000, 0.8660254037844387076, 1.000000000000000000, 0.8660254037844387076, 1.000000000000000000, 0.8660254037844387076, 1.000000000000000000, 0.8660254037844387076, 1.000000000000000000, 0.8660254037844387076, 1.000000000000000000, 0.8660254037844387076, 1.000000000000000000, 0.8660254037844387076, 1.000000000000000000, 0.8660254037844387076, 1.000000000000000000, 0.8660254037844387076, 1.000000000000000000, 0.8660254037844387076, 1.000000000000000000, 0.8660254037844387076, 1.000000000000000000, 0.8660254037844387076, 1.000000000000000000, 0.8660254037844387076, 1.000000000000000000, 0.8660254037844387076, 1.000000000000000000, 0.8660254037844387076, 1.000000000000000000, 0.8660254037844387076, 1.000000000000000000, 0.8660254037844387076, 1.000000000000000000, 0.8660254037844387076, 1.000000000000000000, 0.8660254037844387076, 1.000000000000000000, 0.8660254037844387076, 1.000000000000000000, 0.8660254037844387076, 1.000000000000000000, 0.8660254037844387076, 1.000000000000000000, 0.8660254037844387076, 1.000000000000000000, 0.8660254037844387076, 1.000000000000000000, 0.8660254037844387076, 1.000000000000000000, 0.8660254037844387076, 1.000000000000000000, 0.8660254037844387076, 1.000000000000000000, 0.8660254037844387076, 1.000000000000000000, 0.8660254037844387076, 1.000000000000000000, 0.8660254037844387076, 1.000000000000000000, 0.8660254037844387076, 1.000000000000000000, 0.8660254037844387076, 1.000000000000000000, 0.8660254037844387076, 1.000000000000000000, 0.8660254037844387076, 1.000000000000000000, 0.8660254037844387076, 1.000000000000000000, 0.8660254037844387076, 1.000000000000000000, 0.8660254037844387076, 1.000000000000000000, 0.8660254037844387076, 1.000000000000000000, 0.8660254037844387076, 1.000000000000000000, 0.8660254037844387076, 1.000000000000000000, 0.8660254037844387076, 1.000000000000000000, 0.8660254037844387076, 1.000000000000000000, 0.8660254037844387076, 1.000000000000000000, 0.8660254037844387076, 1.000000000000000000, 0.8660254037844387076, 1.000000000000000000, 0.8660254037844387076, 1.000000000000000000, 0.8660254037844387076, 1.000000000000000000, 0.8660254037844387076, 1.000000000000000000, 0.8660254037844387076, 1.000000000000000000, 0.8660254037844387076, 1.000000000000000000, 0.8660254037844387076, 1.000000000000000000, 0.8660254037844387076, 1.000000000000000000, 0.8660254037844387076, 1.000000000000000000, 0.8660254037844387076, 1.000000000000000000, 0.8660254037844387076, 1.000000000000000000, 0.8660254037844387076, 1.000000000000000000, 0.8660254037844387076, 1.000000000000000000, 0.8660254037844387076, 1.000000000000000000, 0.8660254037844387076, 1.000000000000000000, 0.8660254037844387076, 1.000000000000000000, 0.8660254037844387076, 1.000000000000000000, 0.8660254037844387076, 1.000000000000000000, 0.8660254037844387076, 1.000000000000000000, 0.8660254037844387076, 1.000000000000000000, 0.8660254037844387076, 1.000000000000000000, 0.8660254037844387076, 1.000000000000000000, 0.8660254037844387076, 1.000000000000000000, 0.8660254037844387076, 1.000000000000000000, 0.8660254037844387076, 1.000000000000000000, 0.8660254037844387076, 1.000000000000000000, 0.8660254037844387076, 1.000000000000000000, 0.8660254037844387076, 1.000000000000000000, 0.8660254037844387076, 1.000000000000000000, 0.8660254037844387076, 1.000000000000000000, 0.8660254037844387076, 1.000000000000000000, 0.8660254037844387076, 1.000000000000000000, 0.8660254037844387076, 1.000000000000000000, 0.8660254037844387076, 1.000000000000000000, 0.8660254037844387076, 1.000000000000000000, 0.8660254037844387076, 1.000000000000000000, 0.8660254037844387076, 1.000000000000000000, 0.8660254037844387076, 1.000000000000000000, 0.8660254037844387076, 1.000000000000000000, 0.8660254037844387076, 1.000000000000000000, 0.8660254037844387076, 1.000000000000000000, 0.8660254037844387076, 1.000000000000000000, 0.8660254037844387076, 1.000000000000000000, 0.8660254037844387076, 1.000000000000000000, 0.8660254037844387076, 1.000000000000000000, 0.8660254037844387076, 1.000000000000000000, 0.8660254037844387076, 1.000000000000000000, 0.8660254037844387076, 1.000000000000000000, 0.8660254037844387076, 1.000000000000000000, 0.8660254037844387076, 1.000000000000000000, 0.8660254037844387076, 1.000000000000000000, 0.8660254037844387076, 1.000000000000000000, 0.8660254037844387076, 1.000000000000000000, 0.8660254037844387076, 1.000000000000000000, 0.8660254037844387076, 1.000000000000000000, 0.8660254037844387076, 1.000000000000000000, 0.8660254037844387076, 1.000000000000000000, 0.8660254037844387076, 1.000000000000000000, 0.8660254037844387076, 1.000000000000000000, 0.8660254037844387076, 1.000000000000000000, 0.8660254037844387076, 1.000000000000000000, 0.8660254037844387076, 1.000000000000000000, 0.8660254037844387076, 1.000000000000000000, 0.8660254037844387076, 1.000000000000000000, 0.8660254037844387076, 1.000000000000000000, 0.8660254037844387076, 1.000000000000000000, 0.8660254037844387076, 1.000000000000000000, 0.8660254037844387076, 1.000000000000000000, 0.8660254037844387076, 1.000000000000000000, 0.8660254037844387076, 1.000000000000000000, 0.8660254037844387076, 1.000000000000000000, 0.8660254037844387076, 1.000000000000000000, 0.8660254037844387076, 1.000000000000000000, 0.8660254037844387076, 1.000000000000000000, 0.8660254037844387076, 1.000000000000000000, 0.8660254037844387076, 1.000000000000000000, 0.8660254037844387076, 1.000000000000000000, 0.8660254037844387076, 1.000000000000000000, 0.8660254037844387076, 1.000000000000000000, 0.8660254037844387076, 1.000000000000000000, 0.8660254037844387076, 1.000000000000000000, 0.8660254037844387076, 1.000000000000000000, 0.8660254037844387076, 1.000000000000000000, 0.8660254037844387076, 1.000000000000000000, 0.8660254037844387076, 1.000000000000000000, 0.8660254037844387076, 1.000000000000000000, 0.8660254037844387076, 1.000000000000000000, 0.8660254037844387076, 1.000000000000000000, 0.8660254037844387076, 1.000000000000000000, 0.8660254037844387076, 1.000000000000000000, 0.8660254037844387076, 1.000000000000000000, 0.8660254037844387076, 1.000000000000000000, 0.8660254037844387076, 1.000000000000000000, 0.8660254037844387076, 1.000000000000000000, 0.8660254037844387076, 1.000000000000000000, 0.8660254037844387076, 1.000000000000000000, 0.8660254037844387076, 1.000000000000000000, 0.8660254037844387076, 1.000000000000000000, 0.8660254037844387076, 1.000000000000000000, 0.8660254037844387076, 1.000000000000000000, 0.8660254037844387076, 1.000000000000000000, 0.8660254037844387076, 1.000000000000000000, 0.8660254037844387076, 1.000000000000000000, 0.8660254037844387076, 1.000000000000000000, 0.8660254037844387076, 1.000000000000000000, 0.8660254037844387076, 1.000000000000000000, 0.8660254037844387076, 1.000000000000000000, 0.8660254037844387076, 1.000000000000000000, 0.8660254037844387076, 1.000000000000000000, 0.8660254037844387076, 1.000000000000000000, 0.8660254037844387076, 1.000000000000000000, 0.8660254037844387076, 1.000000000000000000, 0.8660254037844387076, 1.000000000000000000, 0.8660254037844387076, 1.000000000000000000, 0.8660254037844387076, 1.000000000000000000, 0.8660254037844387076, 1.000000000000000000, 0.8660254037844387076, 1.000000000000000000, 0.8660254037844387076, 1.000000000000000000, 0.8660254037844387076, 1.000000000000000000, 0.8660254037844387076, 1.000000000000000000, 0.8660254037844387076, 1.000000000000000000, 0.8660254037844387076, 1.000000000000000000, 0.8660254037844387076, 1.000000000000000000, 0.8660254037844387076, 1.000000000000000000, 0.8660254037844387076, 1.000000000000000000, 0.8660254037844387076, 1.000000000000000000, 0.8660254037844387076, 1.000000000000000000, 0.8660254037844387076, 1.000000000000000000, 0.8660254037844387076, 1.000000000000000000, 0.8660254037844387076, 1.000000000000000000, 0.8660254037844387076, 1.000000000000000000, 0.8660254037844387076, 1.000000000000000000, 0.8660254037844387076, 1.000000000000000000, 0.8660254037844387076, 1.000000000000000000, 0.8660254037844387076, 1.000000000000000000, 0.8660254037844387076, 1.000000000000000000, 0.8660254037844387076, 1.000000000000000000, 0.8660254037844387076, 1.000000000000000000, 0.8660254037844387076, 1.000000000000000000, 0.8660254037844387076, 1.000000000000000000, 0.8660254037844387076, 1.000000000000000000, 0.8660254037844387076, 1.000000000000000000, 0.8660254037844387076, 1.000000000000000000, 0.8660254037844387076, 1.000000000000000000, 0.8660254037844387076, 1.000000000000000000, 0.8660254037844387076, 1.000000000000000000, 0.8660254037844387076, 1.000000000000000000, 0.8660254037844387076, 1.000000000000000000, 0.8660254037844387076, 1.000000000000000000, 0.8660254037844387076, 1.000000000000000000, 0.8660254037844387076, 1.000000000000000000, 0.8660254037844387076, 1.000000000000000000, 0.8660254037844387076, 1.000000000000000000, 0.8660254037844387076, 1.000000000000000000, 0.8660254037844387076, 1.000000000000000000, 0.8660254037844387076, 1.000000000000000000, 0.8660254037844387076, 1.000000000000000000, 0.8660254037844387076, 1.000000000000000000, 0.8660254037844387076, 1.000000000000000000, 0.8660254037844387076, 1.000000000000000000, 0.8660254037844387076, 1.000000000000000000, 0.8660254037844387076, 1.000000000000000000, 0.8660254037844387076, 1.000000000000000000, 0.8660254037844387076, 1.000000000000000000, 0.8660254037844387076, 1.000000000000000000, 0.8660254037844387076, 1.000000000000000000, 0.8660254037844387076, 1.000000000000000000, 0.8660254037844387076, 1.000000000000000000, 0.8660254037844387076, 1.000000000000000000, 0.8660254037844387076, 1.000000000000000000),
 ( 1.000000000000000000, 0.8660254037844387076, 1.000000000000000000, 0.8660254037844387076, 1.000000000000000000, 0.8660254037844387076, 1.000000000000000000, 0.8660254037844387076, 1.000000000000000000, 0.8660254037844387076, 1.000000000000000000, 0.8660254037844387076, 1.000000000000000000, 0.8660254037844387076, 1.000000000000000000, 0.8660254037844387076, 1.000000000000000000, 0.8660254037844387076, 1.000000000000000000, 0.8660254037844387076, 1.000000000000000000, 0.8660254037844387076, 1.000000000000000000, 0.8660254037844387076, 1.000000000000000000, 0.8660254037844387076, 1.000000000000000000, 0.8660254037844387076, 1.000000000000000000, 0.8660254037844387076, 1.000000000000000000, 0.8660254037844387076, 1.000000000000000000, 0.8660254037844387076, 1.000000000000000000, 0.8660254037844387076, 1.000000000000000000, 0.8660254037844387076, 1.000000000000000000, 0.8660254037844387076, 1.000000000000000000, 0.8660254037844387076, 1.000000000000000000, 0.8660254037844387076, 1.000000000000000000, 0.8660254037844387076, 1.000000000000000000, 0.8660254037844387076, 1.000000000000000000, 0.8660254037844387076, 1.000000000000000000, 0.8660254037844387076, 1.000000000000000000, 0.8660254037844387076, 1.000000000000000000, 0.8660254037844387076, 1.000000000000000000, 0.8660254037844387076, 1.000000000000000000, 0.8660254037844387076, 1.000000000000000000, 0.8660254037844387076, 1.000000000000000000, 0.8660254037844387076, 1.000000000000000000, 0.8660254037844387076, 1.000000000000000000, 0.8660254037844387076, 1.000000000000000000, 0.8660254037844387076, 1.000000000000000000, 0.8660254037844387076, 1.000000000000000000, 0.8660254037844387076, 1.000000000000000000, 0.8660254037844387076, 1.000000000000000000, 0.8660254037844387076, 1.000000000000000000, 0.8660254037844387076, 1.000000000000000000, 0.8660254037844387076, 1.000000000000000000, 0.8660254037844387076, 1.000000000000000000, 0.8660254037844387076, 1.000000000000000000, 0.8660254037844387076, 1.000000000000000000, 0.8660254037844387076, 1.000000000000000000, 0.8660254037844387076, 1.000000000000000000, 0.8660254037844387076, 1.000000000000000000, 0.8660254037844387076, 1.000000000000000000, 0.8660254037844387076, 1.000000000000000000, 0.8660254037844387076, 1.000000000000000000, 0.8660254037844387076, 1.000000000000000000, 0.8660254037844387076, 1.000000000000000000, 0.8660254037844387076, 1.000000000000000000, 0.8660254037844387076, 1.000000000000000000, 0.8660254037844387076, 1.000000000000000000, 0.8660254037844387076, 1.000000000000000000, 0.8660254037844387076, 1.000000000000000000, 0.8660254037844387076, 1.000000000000000000, 0.8660254037844387076, 1.000000000000000000, 0.8660254037844387076, 1.000000000000000000, 0.8660254037844387076, 1.000000000000000000, 0.8660254037844387076, 1.000000000000000000, 0.8660254037844387076, 1.000000000000000000, 0.8660254037844387076, 1.000000000000000000, 0.8660254037844387076, 1.000000000000000000, 0.8660254037844387076, 1.000000000000000000, 0.8660254037844387076, 1.000000000000000000, 0.8660254037844387076, 1.000000000000000000, 0.8660254037844387076, 1.000000000000000000, 0.8660254037844387076, 1.000000000000000000, 0.8660254037844387076, 1.000000000000000000, 0.8660254037844387076, 1.000000000000000000, 0.8660254037844387076, 1.000000000000000000, 0.8660254037844387076, 1.000000000000000000, 0.8660254037844387076, 1.000000000000000000, 0.8660254037844387076, 1.000000000000000000, 0.8660254037844387076, 1.000000000000000000, 0.8660254037844387076, 1.000000000000000000, 0.8660254037844387076, 1.000000000000000000, 0.8660254037844387076, 1.000000000000000000, 0.8660254037844387076, 1.000000000000000000, 0.8660254037844387076, 1.000000000000000000, 0.8660254037844387076, 1.000000000000000000, 0.8660254037844387076, 1.000000000000000000, 0.8660254037844387076, 1.000000000000000000, 0.8660254037844387076, 1.000000000000000000, 0.8660254037844387076, 1.000000000000000000, 0.8660254037844387076, 1.000000000000000000, 0.8660254037844387076, 1.000000000000000000, 0.8660254037844387076, 1.000000000000000000, 0.8660254037844387076, 1.000000000000000000, 0.8660254037844387076, 1.000000000000000000, 0.8660254037844387076, 1.000000000000000000, 0.8660254037844387076, 1.000000000000000000, 0.8660254037844387076, 1.000000000000000000, 0.8660254037844387076, 1.000000000000000000, 0.8660254037844387076, 1.000000000000000000, 0.8660254037844387076, 1.000000000000000000, 0.8660254037844387076, 1.000000000000000000, 0.8660254037844387076, 1.000000000000000000, 0.8660254037844387076, 1.000000000000000000, 0.8660254037844387076, 1.000000000000000000, 0.8660254037844387076, 1.000000000000000000, 0.8660254037844387076, 1.000000000000000000, 0.8660254037844387076, 1.000000000000000000, 0.8660254037844387076, 1.000000000000000000, 0.8660254037844387076, 1.000000000000000000, 0.8660254037844387076, 1.000000000000000000, 0.8660254037844387076, 1.000000000000000000, 0.8660254037844387076, 1.000000000000000000, 0.8660254037844387076, 1.000000000000000000, 0.8660254037844387076, 1.000000000000000000, 0.8660254037844387076, 1.000000000000000000, 0.8660254037844387076, 1.000000000000000000, 0.8660254037844387076, 1.000000000000000000, 0.8660254037844387076, 1.000000000000000000, 0.8660254037844387076, 1.000000000000000000, 0.8660254037844387076, 1.000000000000000000, 0.8660254037844387076, 1.000000000000000000, 0.8660254037844387076, 1.000000000000000000, 0.8660254037844387076, 1.000000000000000000, 0.8660254037844387076, 1.000000000000000000, 0.8660254037844387076, 1.000000000000000000, 0.8660254037844387076, 1.000000000000000000, 0.8660254037844387076, 1.000000000000000000, 0.8660254037844387076, 1.000000000000000000, 0.8660254037844387076, 1.000000000000000000, 0.8660254037844387076, 1.000000000000000000, 0.8660254037844387076, 1.000000000000000000, 0.8660254037844387076, 1.000000000000000000, 0.8660254037844387076, 1.000000000000000000, 0.8660254037844387076, 1.000000000000000000, 0.8660254037844387076, 1.000000000000000000, 0.8660254037844387076, 1.000000000000000000, 0.8660254037844387076, 1.000000000000000000, 0.8660254037844387076, 1.000000000000000000, 0.8660254037844387076, 1.000000000000000000, 0.8660254037844387076, 1.000000000000000000, 0.8660254037844387076, 1.000000000000000000, 0.8660254037844387076, 1.000000000000000000, 0.8660254037844387076, 1.000000000000000000, 0.8660254037844387076, 1.000000000000000000, 0.8660254037844387076, 1.000000000000000000, 0.8660254037844387076, 1.000000000000000000, 0.8660254037844387076, 1.000000000000000000, 0.8660254037844387076, 1.000000000000000000, 0.8660254037844387076, 1.000000000000000000, 0.8660254037844387076, 1.000000000000000000, 0.8660254037844387076, 1.000000000000000000, 0.8660254037844387076, 1.000000000000000000, 0.8660254037844387076, 1.000000000000000000, 0.8660254037844387076, 1.000000000000000000, 0.8660254037844387076, 1.000000000000000000, 0.8660254037844387076, 1.000000000000000000, 0.8660254037844387076, 1.000000000000000000, 0.8660254037844387076, 1.000000000000000000, 0.8660254037844387076, 1.000000000000000000, 0.8660254037844387076, 1.000000000000000000, 0.8660254037844387076, 1.000000000000000000, 0.8660254037844387076, 1.000000000000000000, 0.8660254037844387076, 1.000000000000000000, 0.8660254037844387076, 1.000000000000000000, 0.8660254037844387076, 1.000000000000000000, 0.8660254037844387076, 1.000000000000000000, 0.8660254037844387076, 1.000000000000000000, 0.8660254037844387076, 1.000000000000000000, 0.8660254037844387076, 1.000000000000000000, 0.8660254037844387076, 1.000000000000000000, 0.8660254037844387076, 1.000000000000000000, 0.8660254037844387076, 1.000000000000000000, 0.8660254037844387076, 1.000000000000000000, 0.8660254037844387076, 1.000000000000000000, 0.8660254037844387076, 1.000000000000000000, 0.8660254037844387076, 1.000000000000000000, 0.8660254037844387076, 1.000000000000000000, 0.8660254037844387076, 1.000000000000000000, 0.8660254037844387076, 1.000000000000000000, 0.8660254037844387076, 1.000000000000000000, 0.8660254037844387076, 1.000000000000000000, 0.8660254037844387076, 1.000000000000000000, 0.8660254037844387076, 1.000000000000000000, 0.8660254037844387076, 1.000000000000000000, 0.8660254037844387076, 1.000000000000000000, 0.8660254037844387076, 1.000000000000000000, 0.8660254037844387076, 1.000000000000000000, 0.8660254037844387076, 1.000000000000000000, 0.8660254037844387076, 1.000000000000000000, 0.8660254037844387076, 1.000000000000000000, 0.8660254037844387076, 1.000000000000000000, 0.8660254037844387076, 1.000000000000000000, 0.8660254037844387076, 1.000000000000000000, 0.8660254037844387076, 1.000000000000000000, 0.8660254037844387076, 1.000000000000000000, 0.8660254037844387076, 1.000000000000000000, 0.8660254037844387076, 1.000000000000000000, 0.8660254037844387076, 1.000000000000000000, 0.8660254037844387076, 1.000000000000000000, 0.8660254037844387076, 1.000000000000000000, 0.8660254037844387076, 1.000000000000000000, 0.8660254037844387076, 1.000000000000000000, 0.8660254037844387076, 1.000000000000000000, 0.8660254037844387076, 1.000000000000000000, 0.8660254037844387076, 1.000000000000000000, 0.8660254037844387076, 1.000000000000000000, 0.8660254037844387076, 1.000000000000000000, 0.8660254037844387076, 1.000000000000000000, 0.8660254037844387076, 1.000000000000000000, 0.8660254037844387076, 1.000000000000000000, 0.8660254037844387076, 1.000000000000000000, 0.8660254037844387076, 1.000000000000000000, 0.8660254037844387076, 1.000000000000000000, 0.8660254037844387076, 1.000000000000000000, 0.8660254037844387076, 1.000000000000000000, 0.8660254037844387076, 1.000000000000000000, 0.8660254037844387076, 1.000000000000000000, 0.8660254037844387076, 1.000000000000000000, 0.8660254037844387076, 1.000000000000000000, 0.8660254037844387076, 1.000000000000000000, 0.8660254037844387076, 1.000000000000000000, 0.8660254037844387076, 1.000000000000000000, 0.8660254037844387076, 1.000000000000000000, 0.8660254037844387076, 1.000000000000000000, 0.8660254037844387076, 1.000000000000000000, 0.8660254037844387076, 1.000000000000000000, 0.8660254037844387076, 1.000000000000000000, 0.8660254037844387076, 1.000000000000000000, 0.8660254037844387076, 1.000000000000000000, 0.8660254037844387076, 1.000000000000000000, 0.8660254037844387076, 1.000000000000000000, 0.8660254037844387076, 1.000000000000000000, 0.8660254037844387076, 1.000000000000000000, 0.8660254037844387076, 1.000000000000000000, 0.8660254037844387076, 1.000000000000000000, 0.8660254037844387076, 1.000000000000000000, 0.8660254037844387076, 1.000000000000000000, 0.8660254037844387076, 1.000000000000000000, 0.8660254037844387076, 1.000000000000000000, 0.8660254037844387076, 1.000000000000000000, 0.8660254037844387076, 1.000000000000000000, 0.8660254037844387076, 1.000000000000000000, 0.8660254037844387076, 1.000000000000000000, 0.8660254037844387076, 1.000000000000000000, 0.8660254037844387076, 1.000000000000000000, 0.8660254037844387076, 1.000000000000000000, 0.8660254037844387076, 1.000000000000000000, 0.8660254037844387076, 1.000000000000000000, 0.8660254037844387076, 1.000000000000000000, 0.8660254037844387076, 1.000000000000000000, 0.8660254037844387076, 1.000000000000000000, 0.8660254037844387076, 1.000000000000000000, 0.8660254037844387076, 1.000000000000000000, 0.8660254037844387076, 1.000000000000000000, 0.8660254037844387076, 1.000000000000000000, 0.8660254037844387076, 1.000000000000000000, 0.8660254037844387076, 1.000000000000000000, 0.8660254037844387076, 1.000000000000000000, 0.8660254037844387076, 1.000000000000000000, 0.8660254037844387076, 1.000000000000000000, 0.8660254037844387076, 1.000000000000000000, 0.8660254037844387076, 1.000000000000000000, 0.8660254037844387076, 1.000000000000000000, 0.8660254037844387076, 1.000000000000000000, 0.8660254037844387076, 1.000000000000000000, 0.8660254037844387076, 1.000000000000000000, 0.8660254037844387076, 1.000000000000000000, 0.8660254037844387076, 1.000000000000000000, 0.8660254037844387076, 1.000000000000000000, 0.8660254037844387076, 1.000000000000000000, 0.8660254037844387076, 1.000000000000000000, 0.8660254037844387076, 1.000000000000000000, 0.8660254037844387076, 1.000000000000000000, 0.8660254037844387076, 1.000000000000000000, 0.8660254037844387076, 1.000000000000000000, 0.8660254037844387076, 1.000000000000000000, 0.8660254037844387076, 1.000000000000000000, 0.8660254037844387076, 1.000000000000000000, 0.8660254037844387076, 1.000000000000000000, 0.8660254037844387076, 1.000000000000000000, 0.8660254037844387076, 1.000000000000000000, 0.8660254037844387076, 1.000000000000000000, 0.8660254037844387076, 1.000000000000000000, 0.8660254037844387076, 1.000000000000000000, 0.8660254037844387076, 1.000000000000000000, 0.8660254037844387076, 1.000000000000000000, 0.8660254037844387076, 1.000000000000000000, 0.8660254037844387076, 1.000000000000000000, 0.8660254037844387076, 1.000000000000000000, 0.8660254037844387076, 1.000000000000000000, 0.8660254037844387076, 1.000000000000000000, 0.8660254037844387076, 1.000000000000000000, 0.8660254037844387076, 1.000000000000000000, 0.8660254037844387076, 1.000000000000000000, 0.8660254037844387076, 1.000000000000000000, 0.8660254037844387076, 1.000000000000000000, 0.8660254037844387076, 1.000000000000000000, 0.8660254037844387076, 1.000000000000000000, 0.8660254037844387076, 1.000000000000000000, 0.8660254037844387076, 1.000000000000000000, 0.8660254037844387076, 1.000000000000000000, 0.8660254037844387076, 1.000000000000000000, 0.8660254037844387076, 1.000000000000000000, 0.8660254037844387076, 1.000000000000000000, 0.8660254037844387076, 1.000000000000000000, 0.8660254037844387076, 1.000000000000000000, 0.8660254037844387076, 1.000000000000000000, 0.8660254037844387076, 1.000000000000000000, 0.8660254037844387076, 1.000000000000000000, 0.8660254037844387076, 1.000000000000000000, 0.8660254037844387076, 1.000000000000000000, 0.8660254037844387076, 1.000000000000000000, 0.8660254037844387076, 1.000000000000000000, 0.8660254037844387076, 1.000000000000000000, 0.8660254037844387076, 1.000000000000000000, 0.8660254037844387076, 1.000000000000000000, 0.8660254037844387076, 1.000000000000000000, 0.8660254037844387076, 1.000000000000000000, 0.8660254037844387076, 1.000000000000000000, 0.8660254037844387076, 1.000000000000000000, 0.8660254037844387076, 1.000000000000000000, 0.8660254037844387076, 1.000000000000000000, 0.8660254037844387076, 1.000000000000000000, 0.8660254037844387076, 1.000000000000000000, 0.8660254037844387076, 1.000000000000000000, 0.8660254037844387076, 1.000000000000000000, 0.8660254037844387076, 1.000000000000000000, 0.8660254037844387076, 1.000000000000000000, 0.8660254037844387076, 1.000000000000000000, 0.8660254037844387076, 1.000000000000000000, 0.8660254037844387076, 1.000000000000000000, 0.8660254037844387076, 1.000000000000000000, 0.8660254037844387076, 1.000000000000000000, 0.8660254037844387076, 1.000000000000000000, 0.8660254037844387076, 1.000000000000000000, 0.8660254037844387076, 1.000000000000000000, 0.8660254037844387076, 1.000000000000000000, 0.8660254037844387076, 1.000000000000000000, 0.8660254037844387076, 1.000000000000000000, 0.8660254037844387076, 1.000000000000000000, 0.8660254037844387076, 1.000000000000000000, 0.8660254037844387076, 1.000000000000000000, 0.8660254037844387076, 1.000000000000000000, 0.8660254037844387076, 1.000000000000000000, 0.8660254037844387076, 1.000000000000000000, 0.8660254037844387076, 1.000000000000000000, 0.8660254037844387076, 1.000000000000000000, 0.8660254037844387076, 1.000000000000000000, 0.8660254037844387076, 1.000000000000000000, 0.8660254037844387076, 1.000000000000000000, 0.8660254037844387076, 1.000000000000000000, 0.8660254037844387076, 1.000000000000000000, 0.8660254037844387076, 1.000000000000000000, 0.8660254037844387076, 1.000000000000000000, 0.8660254037844387076, 1.000000000000000000, 0.8660254037844387076, 1.000000000000000000, 0.8660254037844387076, 1.000000000000000000, 0.8660254037844387076, 1.000000000000000000, 0.8660254037844387076, 1.000000000000000000, 0.8660254037844387076, 1.000000000000000000, 0.8660254037844387076, 1.000000000000000000, 0.8660254037844387076, 1.000000000000000000, 0.8660254037844387076, 1.000000000000000000, 0.8660254037844387076, 1.000000000000000000, 0.8660254037844387076, 1.000000000000000000, 0.8660254037844387076, 1.000000000000000000, 0.8660254037844387076, 1.000000000000000000, 0.8660254037844387076, 1.000000000000000000, 0.8660254037844387076, 1.000000000000000000, 0.8660254037844387076, 1.000000000000000000, 0.8660254037844387076, 1.000000000000000000, 0.8660254037844387076, 1.000000000000000000, 0.8660254037844387076, 1.000000000000000000, 0.8660254037844387076, 1.000000000000000000, 0.8660254037844387076, 1.000000000000000000, 0.8660254037844387076, 1.000000000000000000, 0.8660254037844387076, 1.000000000000000000, 0.8660254037844387076, 1.000000000000000000, 0.8660254037844387076, 1.000000000000000000, 0.8660254037844387076, 1.000000000000000000, 0.8660254037844387076, 1.000000000000000000, 0.8660254037844387076, 1.000000000000000000, 0.8660254037844387076, 1.000000000000000000, 0.8660254037844387076, 1.000000000000000000, 0.8660254037844387076, 1.000000000000000000, 0.8660254037844387076, 1.000000000000000000, 0.8660254037844387076, 1.000000000000000000, 0.8660254037844387076, 1.000000000000000000, 0.8660254037844387076, 1.000000000000000000, 0.8660254037844387076, 1.000000000000000000, 0.8660254037844387076, 1.000000000000000000, 0.8660254037844387076, 1.000000000000000000, 0.8660254037844387076, 1.000000000000000000, 0.8660254037844387076, 1.000000000000000000, 0.8660254037844387076, 1.000000000000000000, 0.8660254037844387076, 1.000000000000000000, 0.8660254037844387076, 1.000000000000000000, 0.8660254037844387076, 1.000000000000000000, 0.8660254037844387076, 1.000000000000000000, 0.8660254037844387076, 1.000000000000000000, 0.8660254037844387076, 1.000000000000000000, 0.8660254037844387076, 1.000000000000000000, 0.8660254037844387076, 1.000000000000000000, 0.8660254037844387076, 1.000000000000000000, 0.8660254037844387076, 1.000000000000000000, 0.8660254037844387076, 1.000000000000000000, 0.8660254037844387076, 1.000000000000000000, 0.8660254037844387076, 1.000000000000000000, 0.8660254037844387076, 1.000000000000000000, 0.8660254037844387076, 1.000000000000000000, 0.8660254037844387076, 1.000000000000000000, 0.8660254037844387076, 1.000000000000000000, 0.8660254037844387076, 1.000000000000000000, 0.8660254037844387076, 1.000000000000000000, 0.8660254037844387076, 1.000000000000000000, 0.8660254037844387076, 1.000000000000000000, 0.8660254037844387076, 1.000000000000000000, 0.8660254037844387076, 1.000000000000000000, 0.8660254037844387076, 1.000000000000000000, 0.8660254037844387076, 1.000000000000000000, 0.8660254037844387076, 1.000000000000000000, 0.8660254037844387076, 1.000000000000000000, 0.8660254037844387076, 1.000000000000000000, 0.8660254037844387076, 1.000000000000000000, 0.8660254037844387076, 1.000000000000000000, 0.8660254037844387076, 1.000000000000000000, 0.8660254037844387076, 1.000000000000000000, 0.8660254037844387076, 1.000000000000000000, 0.8660254037844387076, 1.000000000000000000, 0.8660254037844387076, 1.000000000000000000, 0.8660254037844387076, 1.000000000000000000, 0.8660254037844387076, 1.000000000000000000, 0.8660254037844387076, 1.000000000000000000, 0.8660254037844387076, 1.000000000000000000, 0.8660254037844387076, 1.000000000000000000, 0.8660254037844387076, 1.000000000000000000, 0.8660254037844387076, 1.000000000000000000, 0.8660254037844387076, 1.000000000000000000, 0.8660254037844387076, 1.000000000000000000, 0.8660254037844387076, 1.000000000000000000, 0.8660254037844387076, 1.000000000000000000, 0.8660254037844387076, 1.000000000000000000, 0.8660254037844387076, 1.000000000000000000, 0.8660254037844387076, 1.000000000000000000, 0.8660254037844387076, 1.000000000000000000, 0.8660254037844387076, 1.000000000000000000, 0.8660254037844387076, 1.000000000000000000, 0.8660254037844387076, 1.000000000000000000, 0.8660254037844387076, 1.000000000000000000, 0.8660254037844387076, 1.000000000000000000, 0.8660254037844387076, 1.000000000000000000, 0.8660254037844387076, 1.000000000000000000, 0.8660254037844387076, 1.000000000000000000, 0.8660254037844387076, 1.000000000000000000, 0.8660254037844387076, 1.000000000000000000, 0.8660254037844387076, 1.000000000000000000, 0.8660254037844387076, 1.000000000000000000, 0.8660254037844387076, 1.000000000000000000, 0.8660254037844387076, 1.000000000000000000, 0.8660254037844387076, 1.000000000000000000, 0.8660254037844387076, 1.000000000000000000, 0.8660254037844387076, 1.000000000000000000, 0.8660254037844387076, 1.000000000000000000, 0.8660254037844387076, 1.000000000000000000, 0.8660254037844387076, 1.000000000000000000, 0.8660254037844387076, 1.000000000000000000, 0.8660254037844387076, 1.000000000000000000, 0.8660254037844387076, 1.000000000000000000, 0.8660254037844387076, 1.000000000000000000, 0.8660254037844387076, 1.000000000000000000, 0.8660254037844387076, 1.000000000000000000, 0.8660254037844387076, 1.000000000000000000, 0.8660254037844387076, 1.000000000000000000, 0.8660254037844387076, 1.000000000000000000, 0.8660254037844387076, 1.000000000000000000, 0.8660254037844387076, 1.000000000000000000, 0.8660254037844387076, 1.000000000000000000, 0.8660254037844387076, 1.000000000000000000, 0.8660254037844387076, 1.000000000000000000, 0.8660254037844387076, 1.000000000000000000, 0.8660254037844387076, 1.000000000000000000, 0.8660254037844387076, 1.000000000000000000, 0.8660254037844387076, 1.000000000000000000, 0.8660254037844387076, 1.000000000000000000, 0.8660254037844387076, 1.000000000000000000, 0.8660254037844387076, 1.000000000000000000, 0.8660254037844387076, 1.000000000000000000, 0.8660254037844387076, 1.000000000000000000, 0.8660254037844387076, 1.000000000000000000, 0.8660254037844387076, 1.000000000000000000, 0.8660254037844387076, 1.000000000000000000, 0.8660254037844387076, 1.000000000000000000, 0.8660254037844387076, 1.000000000000000000, 0.8660254037844387076, 1.000000000000000000, 0.8660254037844387076, 1.000000000000000000, 0.8660254037844387076, 1.000000000000000000, 0.8660254037844387076, 1.000000000000000000, 0.8660254037844387076, 1.000000000000000000, 0.8660254037844387076, 1.000000000000000000, 0.8660254037844387076, 1.000000000000000000, 0.8660254037844387076, 1.000000000000000000, 0.8660254037844387076, 1.000000000000000000, 0.8660254037844387076, 1.000000000000000000, 0.8660254037844387076, 1.000000000000000000, 0.8660254037844387076, 1.000000000000000000, 0.8660254037844387076, 1.000000000000000000, 0.8660254037844387076, 1.000000000000000000, 0.8660254037844387076, 1.000000000000000000, 0.8660254037844387076, 1.000000000000000000, 0.8660254037844387076, 1.000000000000000000, 0.8660254037844387076, 1.000000000000000000, 0.8660254037844387076, 1.000000000000000000, 0.8660254037844387076, 1.000000000000000000, 0.8660254037844387076, 1.000000000000000000, 0.8660254037844387076, 1.000000000000000000, 0.8660254037844387076, 1.000000000000000000, 0.8660254037844387076, 1.000000000000000000, 0.8660254037844387076, 1.000000000000000000, 0.8660254037844387076, 1.000000000000000000, 0.8660254037844387076, 1.000000000000000000, 0.8660254037844387076, 1.000000000000000000, 0.8660254037844387076, 1.000000000000000000, 0.8660254037844387076, 1.000000000000000000, 0.8660254037844387076, 1.000000000000000000, 0.8660254037844387076, 1.000000000000000000, 0.8660254037844387076, 1.000000000000000000, 0.8660254037844387076, 1.000000000000000000, 0.8660254037844387076, 1.000000000000000000, 0.8660254037844387076, 1.000000000000000000, 0.8660254037844387076, 1.000000000000000000, 0.8660254037844387076, 1.000000000000000000, 0.8660254037844387076, 1.000000000000000000, 0.8660254037844387076, 1.000000000000000000, 0.8660254037844387076, 1.000000000000000000, 0.8660254037844387076, 1.000000000000000000, 0.8660254037844387076, 1.000000000000000000, 0.8660254037844387076, 1.000000000000000000, 0.8660254037844387076, 1.000000000000000000, 0.8660254037844387076, 1.000000000000000000, 0.8660254037844387076, 1.000000000000000000, 0.8660254037844387076, 1.000000000000000000, 0.8660254037844387076, 1.000000000000000000, 0.8660254037844387076, 1.000000000000000000, 0.8660254037844387076, 1.000000000000000000, 0.8660254037844387076, 1.000000000000000000, 0.8660254037844387076, 1.000000000000000000, 0.8660254037844387076, 1.000000000000000000, 0.8660254037844387076, 1.000000000000000000, 0.8660254037844387076, 1.000000000000000000, 0.8660254037844387076, 1.000000000000000000, 0.8660254037844387076, 1.000000000000000000, 0.8660254037844387076, 1.000000000000000000, 0.8660254037844387076, 1.000000000000000000, 0.8660254037844387076, 1.000000000000000000, 0.8660254037844387076, 1.000000000000000000, 0.8660254037844387076, 1.000000000000000000, 0.8660254037844387076, 1.000000000000000000, 0.8660254037844387076, 1.000000000000000000, 0.8660254037844387076, 1.000000000000000000, 0.8660254037844387076, 1.000000000000000000, 0.8660254037844387076, 1.000000000000000000, 0.8660254037844387076, 1.000000000000000000, 0.8660254037844387076, 1.000000000000000000, 0.8660254037844387076, 1.000000000000000000, 0.8660254037844387076, 1.000000000000000000, 0.8660254037844387076, 1.000000000000000000, 0.8660254037844387076, 1.000000000000000000, 0.8660254037844387076, 1.000000000000000000, 0.8660254037844387076, 1.000000000000000000, 0.8660254037844387076, 1.000000000000000000, 0.8660254037844387076, 1.000000000000000000, 0.8660254037844387076, 1.000000000000000000, 0.8660254037844387076, 1.000000000000000000, 0.8660254037844387076, 1.000000000000000000, 0.8660254037844387076, 1.000000000000000000, 0.8660254037844387076, 1.000000000000000000, 0.8660254037844387076, 1.000000000000000000, 0.8660254037844387076, 1.000000000000000000, 0.8660254037844387076, 1.000000000000000000, 0.8660254037844387076, 1.000000000000000000, 0.8660254037844387076, 1.000000000000000000, 0.8660254037844387076, 1.000000000000000000, 0.8660254037844387076, 1.000000000000000000, 0.8660254037844387076, 1.000000000000000000, 0.8660254037844387076, 1.000000000000000000, 0.8660254037844387076, 1.000000000000000000, 0.8660254037844387076, 1.000000000000000000, 0.8660254037844387076, 1.000000000000000000, 0.8660254037844387076, 1.000000000000000000, 0.8660254037844387076, 1.000000000000000000, 0.8660254037844387076, 1.000000000000000000, 0.8660254037844387076, 1.000000000000000000, 0.8660254037844387076, 1.000000000000000000, 0.8660254037844387076, 1.000000000000000000, 0.8660254037844387076, 1.000000000000000000, 0.8660254037844387076, 1.000000000000000000, 0.8660254037844387076, 1.000000000000000000, 0.8660254037844387076, 1.000000000000000000, 0.8660254037844387076, 1.000000000000000000, 0.8660254037844387076, 1.000000000000000000, 0.8660254037844387076, 1.000000000000000000, 0.8660254037844387076, 1.000000000000000000, 0.8660254037844387076, 1.000000000000000000, 0.8660254037844387076, 1.000000000000000000, 0.8660254037844387076, 1.000000000000000000, 0.8660254037844387076, 1.000000000000000000, 0.8660254037844387076, 1.000000000000000000, 0.8660254037844387076, 1.000000000000000000, 0.8660254037844387076, 1.000000000000000000, 0.8660254037844387076, 1.000000000000000000, 0.8660254037844387076, 1.000000000000000000, 0.8660254037844387076, 1.000000000000000000, 0.8660254037844387076, 1.000000000000000000, 0.8660254037844387076, 1.000000000000000000, 0.8660254037844387076, 1.000000000000000000, 0.8660254037844387076, 1.000000000000000000, 0.8660254037844387076, 1.000000000000000000, 0.8660254037844387076, 1.000000000000000000, 0.8660254037844387076, 1.000000000000000000, 0.8660254037844387076, 1.000000000000000000, 0.8660254037844387076, 1.000000000000000000, 0.8660254037844387076, 1.000000000000000000, 0.8660254037844387076, 1.000000000000000000, 0.8660254037844387076, 1.000000000000000000, 0.8660254037844387076, 1.000000000000000000, 0.8660254037844387076, 1.000000000000000000, 0.8660254037844387076, 1.000000000000000000, 0.8660254037844387076, 1.000000000000000000, 0.8660254037844387076, 1.000000000000000000, 0.8660254037844387076, 1.000000000000000000, 0.8660254037844387076, 1.000000000000000000, 0.8660254037844387076, 1.000000000000000000, 0.8660254037844387076, 1.000000000000000000, 0.8660254037844387076, 1.000000000000000000, 0.8660254037844387076, 1.000000000000000000, 0.8660254037844387076, 1.000000000000000000, 0.8660254037844387076, 1.000000000000000000, 0.8660254037844387076, 1.000000000000000000, 0.8660254037844387076, 1.000000000000000000, 0.8660254037844387076, 1.000000000000000000, 0.8660254037844387076, 1.000000000000000000, 0.8660254037844387076, 1.000000000000000000, 0.8660254037844387076, 1.000000000000000000, 0.8660254037844387076, 1.000000000000000000, 0.8660254037844387076, 1.000000000000000000, 0.8660254037844387076, 1.000000000000000000, 0.8660254037844387076, 1.000000000000000000, 0.8660254037844387076, 1.000000000000000000, 0.8660254037844387076, 1.000000000000000000, 0.8660254037844387076, 1.000000000000000000, 0.8660254037844387076, 1.000000000000000000, 0.8660254037844387076, 1.000000000000000000, 0.8660254037844387076, 1.000000000000000000, 0.8660254037844387076, 1.000000000000000000, 0.8660254037844387076, 1.000000000000000000, 0.8660254037844387076, 1.000000000000000000, 0.8660254037844387076, 1.000000000000000000, 0.8660254037844387076, 1.000000000000000000, 0.8660254037844387076, 1.000000000000000000, 0.8660254037844387076, 1.000000000000000000, 0.8660254037844387076, 1.000000000000000000, 0.8660254037844387076, 1.000000000000000000, 0.8660254037844387076, 1.000000000000000000, 0.8660254037844387076, 1.000000000000000000, 0.8660254037844387076, 1.000000000000000000, 0.8660254037844387076, 1.000000000000000000, 0.8660254037844387076, 1.000000000000000000, 0.8660254037844387076, 1.000000000000000000, 0.8660254037844387076, 1.000000000000000000, 0.8660254037844387076, 1.000000000000000000, 0.8660254037844387076, 1.000000000000000000, 0.8660254037844387076, 1.000000000000000000, 0.8660254037844387076, 1.000000000000000000, 0.8660254037844387076, 1.000000000000000000, 0.8660254037844387076, 1.000000000000000000, 0.8660254037844387076, 1.000000000000000000, 0.8660254037844387076, 1.000000000000000000, 0.8660254037844387076, 1.000000000000000000, 0.8660254037844387076, 1.000000000000000000, 0.8660254037844387076, 1.000000000000000000, 0.8660254037844387076, 1.000000000000000000, 0.8660254037844387076, 1.000000000000000000, 0.8660254037844387076, 1.000000000000000000, 0.8660254037844387076, 1.000000000000000000, 0.8660254037844387076, 1.000000000000000000, 0.8660254037844387076, 1.000000000000000000, 0.8660254037844387076, 1.000000000000000000, 0.8660254037844387076, 1.000000000000000000, 0.8660254037844387076, 1.000000000000000000, 0.8660254037844387076, 1.000000000000000000, 0.8660254037844387076, 1.000000000000000000, 0.8660254037844387076, 1.000000000000000000, 0.8660254037844387076, 1.000000000000000000, 0.8660254037844387076, 1.000000000000000000, 0.8660254037844387076, 1.000000000000000000, 0.8660254037844387076, 1.000000000000000000, 0.8660254037844387076, 1.000000000000000000, 0.8660254037844387076, 1.000000000000000000, 0.8660254037844387076, 1.000000000000000000, 0.8660254037844387076, 1.000000000000000000, 0.8660254037844387076, 1.000000000000000000, 0.8660254037844387076, 1.000000000000000000, 0.8660254037844387076, 1.000000000000000000, 0.8660254037844387076, 1.000000000000000000, 0.8660254037844387076, 1.000000000000000000, 0.8660254037844387076, 1.000000000000000000, 0.8660254037844387076, 1.000000000000000000, 0.8660254037844387076, 1.000000000000000000, 0.8660254037844387076, 1.000000000000000000, 0.8660254037844387076, 1.000000000000000000, 0.8660254037844387076, 1.000000000000000000, 0.8660254037844387076, 1.000000000000000000, 0.8660254037844387076, 1.000000000000000000, 0.8660254037844387076, 1.000000000000000000, 0.8660254037844387076, 1.000000000000000000, 0.8660254037844387076, 1.000000000000000000, 0.8660254037844387076, 1.000000000000000000, 0.8660254037844387076, 1.000000000000000000, 0.8660254037844387076, 1.000000000000000000, 0.8660254037844387076, 1.000000000000000000, 0.8660254037844387076, 1.000000000000000000, 0.8660254037844387076, 1.000000000000000000, 0.8660254037844387076, 1.000000000000000000, 0.8660254037844387076, 1.000000000000000000, 0.8660254037844387076, 1.000000000000000000, 0.8660254037844387076, 1.000000000000000000, 0.8660254037844387076, 1.000000000000000000, 0.8660254037844387076, 1.000000000000000000, 0.8660254037844387076, 1.000000000000000000, 0.8660254037844387076, 1.000000000000000000, 0.8660254037844387076, 1.000000000000000000, 0.8660254037844387076, 1.000000000000000000, 0.8660254037844387076, 1.000000000000000000, 0.8660254037844387076, 1.000000000000000000, 0.8660254037844387076, 1.000000000000000000, 0.8660254037844387076, 1.000000000000000000, 0.8660254037844387076, 1.000000000000000000, 0.8660254037844387076, 1.000000000000000000, 0.8660254037844387076, 1.000000000000000000, 0.8660254037844387076, 1.000000000000000000, 0.8660254037844387076, 1.000000000000000000, 0.8660254037844387076, 1.000000000000000000, 0.8660254037844387076, 1.000000000000000000, 0.8660254037844387076, 1.000000000000000000, 0.8660254037844387076, 1.000000000000000000, 0.8660254037844387076, 1.000000000000000000, 0.8660254037844387076, 1.000000000000000000, 0.8660254037844387076, 1.000000000000000000, 0.8660254037844387076, 1.000000000000000000, 0.8660254037844387076, 1.000000000000000000, 0.8660254037844387076, 1.000000000000000000, 0.8660254037844387076, 1.000000000000000000, 0.8660254037844387076, 1.000000000000000000, 0.8660254037844387076, 1.000000000000000000, 0.8660254037844387076, 1.000000000000000000, 0.8660254037844387076, 1.000000000000000000, 0.8660254037844387076, 1.000000000000000000, 0.8660254037844387076, 1.000000000000000000, 0.8660254037844387076, 1.000000000000000000, 0.8660254037844387076, 1.000000000000000000, 0.8660254037844387076, 1.000000000000000000, 0.8660254037844387076, 1.000000000000000000, 0.8660254037844387076, 1.000000000000000000, 0.8660254037844387076, 1.000000000000000000, 0.8660254037844387076, 1.000000000000000000, 0.8660254037844387076, 1.000000000000000000, 0.8660254037844387076, 1.000000000000000000, 0.8660254037844387076, 1.000000000000000000, 0.8660254037844387076, 1.000000000000000000, 0.8660254037844387076, 1.000000000000000000, 0.8660254037844387076, 1.000000000000000000, 0.8660254037844387076, 1.000000000000000000, 0.8660254037844387076, 1.000000000000000000, 0.8660254037844387076, 1.000000000000000000, 0.8660254037844387076, 1.000000000000000000, 0.8660254037844387076, 1.000000000000000000, 0.8660254037844387076, 1.000000000000000000, 0.8660254037844387076, 1.000000000000000000, 0.8660254037844387076, 1.000000000000000000, 0.8660254037844387076, 1.000000000000000000, 0.8660254037844387076, 1.000000000000000000, 0.8660254037844387076, 1.000000000000000000, 0.8660254037844387076, 1.000000000000000000, 0.8660254037844387076, 1.000000000000000000, 0.8660254037844387076, 1.000000000000000000, 0.8660254037844387076, 1.000000000000000000, 0.8660254037844387076, 1.000000000000000000, 0.8660254037844387076, 1.000000000000000000, 0.8660254037844387076, 1.000000000000000000, 0.8660254037844387076, 1.000000000000000000, 0.8660254037844387076, 1.000000000000000000, 0.8660254037844387076, 1.000000000000000000, 0.8660254037844387076, 1.000000000000000000, 0.8660254037844387076, 1.000000000000000000, 0.8660254037844387076, 1.000000000000000000, 0.8660254037844387076, 1.000000000000000000, 0.8660254037844387076, 1.000000000000000000, 0.8660254037844387076, 1.000000000000000000, 0.8660254037844387076, 1.000000000000000000, 0.8660254037844387076, 1.000000000000000000, 0.8660254037844387076, 1.000000000000000000, 0.8660254037844387076, 1.000000000000000000) ) ) 
 REPRESENTATION_ITEM ( '' )  SURFACE ( )  );
#4986 = CARTESIAN_POINT ( 'NONE',  ( -2.293366432827344421E-15, -12.48450537969573659, -61.90625000204838813 ) ) ;
#4987 = DATE_TIME_ROLE ( 'creation_date' ) ;
#4989 = ORIENTED_EDGE ( 'NONE', *, *, #41755, .F. ) ;
#4988 = ORIENTED_EDGE ( 'NONE', *, *, #16390, .T. ) ;
#4990 = DIRECTION ( 'NONE',  ( -1.000000000000000000, 0.000000000000000000, 0.000000000000000000 ) ) ;
#4991 = VECTOR ( 'NONE', #5574, 1000.000000000000000 ) ;
#4992 = CARTESIAN_POINT ( 'NONE',  ( -9.999999999998969713, -5.773502691896847949, -55.50000000409676204 ) ) ;
#4994 = ADVANCED_FACE ( 'NONE', ( #748 ), #20154, .T. ) ;
#4993 = CARTESIAN_POINT ( 'NONE',  ( 10.81189881249999729, 0.000000000000000000, -158.8437500020483810 ) ) ;
#4995 =( BOUNDED_CURVE ( )  B_SPLINE_CURVE ( 2, ( #40822, #24242, #14268, #7836, #17948, #14922, #31146 ),
 .UNSPECIFIED., .F., .F. ) 
 B_SPLINE_CURVE_WITH_KNOTS ( ( 3, 2, 2, 3 ),
 ( 0.7052238805970151292, 0.7064676616915425145, 0.7077114427860698997, 0.7089552238805972850 ),
 .UNSPECIFIED. ) 
 CURVE ( )  GEOMETRIC_REPRESENTATION_ITEM ( )  RATIONAL_B_SPLINE_CURVE ( ( 0.9999999999999761302, 0.8660254037844625774, 1.000000000000000000, 0.8660254037844387076, 1.000000000000000000, 0.8660254037844148378, 1.000000000000023981 ) ) 
 REPRESENTATION_ITEM ( '' )  );
#4996 = CARTESIAN_POINT ( 'NONE',  ( 5.405949406249992428, -9.363379034771808662, -187.7812500020484094 ) ) ;
#4997 = CARTESIAN_POINT ( 'NONE',  ( 10.81189881249999551, -6.242252689847874514, -16.46875000204836326 ) ) ;
#4998 = CARTESIAN_POINT ( 'NONE',  ( -10.00000000000102496, 5.773502691895664007, -30.25000000409673007 ) ) ;
#4999 = CARTESIAN_POINT ( 'NONE',  ( 10.81189881249999729, 0.000000000000000000, -146.8437500020483810 ) ) ;
#5000 = CARTESIAN_POINT ( 'NONE',  ( -2.293366432827344421E-15, -12.48450537969573659, -105.4062500020483810 ) ) ;
#5001 = CARTESIAN_POINT ( 'NONE',  ( 5.405949406249999534, 9.363379034771803333, -109.0937500020483810 ) ) ;
#5002 = CARTESIAN_POINT ( 'NONE',  ( -2.121150477449813534E-15, -11.54700538379251284, -161.3750000000000000 ) ) ;
#5003 = CARTESIAN_POINT ( 'NONE',  ( 10.81189881249999907, 6.242252689847868297, -116.9062500020483952 ) ) ;
#5004 = CARTESIAN_POINT ( 'NONE',  ( -10.81189881249999729, 1.324075727343319199E-15, -2.093750002048366810 ) ) ;
#5005 = CARTESIAN_POINT ( 'NONE',  ( 10.81189881249999729, 6.242252689847867408, -127.2187500020483810 ) ) ;
#5006 = CARTESIAN_POINT ( 'NONE',  ( 7.644554776091147741E-16, 12.48450537969573659, -197.6562500020484094 ) ) ;
#5007 = CARTESIAN_POINT ( 'NONE',  ( -9.999999999999998224, 1.224646799147353059E-15, -165.1250000040967905 ) ) ;
#5008 = CARTESIAN_POINT ( 'NONE',  ( -10.00000000000000000, -5.773502691896251982, -151.1250000000000284 ) ) ;
#5009 = CARTESIAN_POINT ( 'NONE',  ( -4.999999999999996447, 8.660254037844387298, -16.49999999999995737 ) ) ;
#5010 = AXIS2_PLACEMENT_3D ( 'NONE', #18603, #2639, #41891 ) ;
#5011 = CARTESIAN_POINT ( 'NONE',  ( -10.81189881249999729, -6.242252689847864744, -73.96875000204836681 ) ) ;
#5012 = CARTESIAN_POINT ( 'NONE',  ( 10.81189881249999729, 0.000000000000000000, -59.84375000204835970 ) ) ;
#5013 = CARTESIAN_POINT ( 'NONE',  ( 10.00000000000025402, -5.773502691896113426, -116.5000000040967763 ) ) ;
#5014 = CARTESIAN_POINT ( 'NONE',  ( 10.81189881249999729, 0.000000000000000000, -37.53125000204838102 ) ) ;
#5015 = CARTESIAN_POINT ( 'NONE',  ( -2.293366432827344421E-15, -12.48450537969573659, -45.21875000204835970 ) ) ;
#5016 = CARTESIAN_POINT ( 'NONE',  ( 9.999999999999998224, 0.000000000000000000, -53.37500000409675494 ) ) ;
#5017 = CARTESIAN_POINT ( 'NONE',  ( 7.644554776091147741E-16, 12.48450537969573659, -149.4687500020484094 ) ) ;
#5018 = CARTESIAN_POINT ( 'NONE',  ( 10.00000000000000000, 5.773502691896255534, -121.8750000000000000 ) ) ;
#5019 = ADVANCED_FACE ( 'NONE', ( #29148 ), #2612, .T. ) ;
#5020 = DIRECTION ( 'NONE',  ( -0.000000000000000000, -0.000000000000000000, 1.000000000000000000 ) ) ;
#5021 = CARTESIAN_POINT ( 'NONE',  ( -9.999999999999998224, 5.773502691896259087, -77.87499999999998579 ) ) ;
#5022 = CARTESIAN_POINT ( 'NONE',  ( -10.81189881249999729, -6.242252689847864744, -8.156250002048370362 ) ) ;
#5023 = VERTEX_POINT ( 'NONE', #6056 ) ;
#5024 = CARTESIAN_POINT ( 'NONE',  ( -9.999999999999998224, 1.224646799147353059E-15, -200.0000000000000000 ) ) ;
#5025 = CARTESIAN_POINT ( 'NONE',  ( -2.121150477449813534E-15, -11.54700538379251284, -121.2500000040967905 ) ) ;
#5026 = CARTESIAN_POINT ( 'NONE',  ( -5.000000000000003553, -8.660254037844383745, -154.3750000040967905 ) ) ;
#5027 = CARTESIAN_POINT ( 'NONE',  ( 7.644554776091147741E-16, 12.48450537969573659, -84.96875000204835260 ) ) ;
#5028 = CARTESIAN_POINT ( 'NONE',  ( -10.00000000000000000, -5.773502691896251982, -34.50000000409674783 ) ) ;
#5029 = EDGE_CURVE ( 'NONE', #23394, #24472, #32300, .T. ) ;
#5030 = CARTESIAN_POINT ( 'NONE',  ( -9.999999999999998224, 1.224646799147353059E-15, -131.7499999999999716 ) ) ;
#5031 = CARTESIAN_POINT ( 'NONE',  ( 5.405949406249999534, 9.363379034771803333, -47.78125000204838813 ) ) ;
#5032 = CARTESIAN_POINT ( 'NONE',  ( 9.999999999999998224, 0.000000000000000000, -99.49999999999998579 ) ) ;
#5033 = CARTESIAN_POINT ( 'NONE',  ( -5.405949406249996869, 9.363379034771805109, -146.5312500020483810 ) ) ;
#5034 = CARTESIAN_POINT ( 'NONE',  ( 5.405949406249992428, -9.363379034771808662, -124.5937500020483952 ) ) ;
#5035 = DIRECTION ( 'NONE',  ( -0.9961946980917455452, 0.000000000000000000, -0.08715574274765837404 ) ) ;
#5036 = VERTEX_POINT ( 'NONE', #11281 ) ;
#5037 = ORIENTED_EDGE ( 'NONE', *, *, #19605, .F. ) ;
#5038 = ORIENTED_EDGE ( 'NONE', *, *, #10150, .F. ) ;
#5039 = FACE_BOUND ( 'NONE', #22654, .T. ) ;
#5040 = CARTESIAN_POINT ( 'NONE',  ( -5.405949406249996869, 9.363379034771805109, -185.3437500020483810 ) ) ;
#5041 = CARTESIAN_POINT ( 'NONE',  ( 7.644554776091147741E-16, 12.48450537969573659, -41.46875000204835260 ) ) ;
#5042 = CARTESIAN_POINT ( 'NONE',  ( -9.999999999998969713, -5.773502691896847949, -130.5000000040967905 ) ) ;
#5043 = CARTESIAN_POINT ( 'NONE',  ( 7.644554776091147741E-16, 12.48450537969573659, -173.4687500020483810 ) ) ;
#5044 = CARTESIAN_POINT ( 'NONE',  ( -10.81189881249999729, 6.242252689847871849, -150.7187500020483810 ) ) ;
#5045 = CARTESIAN_POINT ( 'NONE',  ( -9.999999999999998224, 1.224646799147353059E-15, -76.62500000409677625 ) ) ;
#5046 = CARTESIAN_POINT ( 'NONE',  ( -5.405949406249996869, 9.363379034771805109, -129.8437500020484094 ) ) ;
#5047 = CARTESIAN_POINT ( 'NONE',  ( 10.81189881249999907, 6.242252689847868297, -139.4062500020484094 ) ) ;
#5048 = CARTESIAN_POINT ( 'NONE',  ( -5.405949406250003975, -9.363379034771801557, -153.3437500020483810 ) ) ;
#5049 = CARTESIAN_POINT ( 'NONE',  ( -2.121150477449813534E-15, -11.54700538379251284, -155.3750000000000000 ) ) ;
#5050 = CARTESIAN_POINT ( 'NONE',  ( 9.999999999999998224, 0.000000000000000000, -170.0000000000000000 ) ) ;
#5051 = CARTESIAN_POINT ( 'NONE',  ( -9.999999999999998224, 1.224646799147353059E-15, -170.7500000000000000 ) ) ;
#5052 = CARTESIAN_POINT ( 'NONE',  ( -10.81189881249999907, -6.242252689847864744, -78.46875000204838102 ) ) ;
#5053 = CARTESIAN_POINT ( 'NONE',  ( -5.405949406250003975, -9.363379034771801557, -60.53125000204836681 ) ) ;
#5054 = CARTESIAN_POINT ( 'NONE',  ( -9.564224651208778738, -3.791567223145488885, -99.99999999999998579 ) ) ;
#5055 = CARTESIAN_POINT ( 'NONE',  ( 7.644554776091147741E-16, 12.48450537969573659, -179.4687500020483810 ) ) ;
#5056 = CARTESIAN_POINT ( 'NONE',  ( 10.81189881249999729, 0.000000000000000000, -111.0312500020483810 ) ) ;
#5057 = CARTESIAN_POINT ( 'NONE',  ( -10.81189881249999729, 1.324075727343319199E-15, -158.2812500020484094 ) ) ;
#5058 =( BOUNDED_CURVE ( )  B_SPLINE_CURVE ( 2, ( #13780, #36890, #451, #13567, #10341, #27612, #26758 ),
 .UNSPECIFIED., .F., .F. ) 
 B_SPLINE_CURVE_WITH_KNOTS ( ( 3, 2, 2, 3 ),
 ( 0.9776119402985076201, 0.9788557213930348944, 0.9800995024875623907, 0.9813432835820897759 ),
 .UNSPECIFIED. ) 
 CURVE ( )  GEOMETRIC_REPRESENTATION_ITEM ( )  RATIONAL_B_SPLINE_CURVE ( ( 0.9999999999999880096, 0.8660254037844506980, 1.000000000000000000, 0.8660254037844387076, 1.000000000000000000, 0.8660254037844148378, 1.000000000000023981 ) ) 
 REPRESENTATION_ITEM ( '' )  );
#5059 = CARTESIAN_POINT ( 'NONE',  ( 9.999999999999998224, 0.000000000000000000, -10.99999999999995381 ) ) ;
#5060 = CARTESIAN_POINT ( 'NONE',  ( -10.81189881249999729, 6.242252689847871849, -47.40625000204836681 ) ) ;
#5061 = CARTESIAN_POINT ( 'NONE',  ( -9.999999999999998224, 5.773502691896259087, -133.7500000040967905 ) ) ;
#5062 = CARTESIAN_POINT ( 'NONE',  ( -5.000000000000003553, -8.660254037844383745, -95.49999999999998579 ) ) ;
#5063 = ORIENTED_EDGE ( 'NONE', *, *, #21137, .F. ) ;
#5064 = CARTESIAN_POINT ( 'NONE',  ( -5.405949406249996869, 9.363379034771805109, -128.5312500020484094 ) ) ;
#5065 = CARTESIAN_POINT ( 'NONE',  ( 9.999999999999998224, 0.000000000000000000, -149.3750000040967905 ) ) ;
#5066 = DIRECTION ( 'NONE',  ( -0.000000000000000000, -0.000000000000000000, -1.000000000000000000 ) ) ;
#5067 = CARTESIAN_POINT ( 'NONE',  ( 10.81189881249999729, 0.000000000000000000, -183.0312500020484094 ) ) ;
#5068 = VERTEX_POINT ( 'NONE', #12709 ) ;
#5069 = CARTESIAN_POINT ( 'NONE',  ( -5.405949406249996869, 9.363379034771805109, -171.8437500020484094 ) ) ;
#5070 = CARTESIAN_POINT ( 'NONE',  ( -9.999999999999998224, 1.224646799147353059E-15, -61.62500000409676204 ) ) ;
#5071 = ADVANCED_FACE ( 'NONE', ( #2402 ), #5637, .F. ) ;
#5072 = CARTESIAN_POINT ( 'NONE',  ( 9.999999999999998224, 0.000000000000000000, -200.0000000000000000 ) ) ;
#5073 = CYLINDRICAL_SURFACE ( 'NONE', #24222, 9.999999999999998224 ) ;
#5074 = ADVANCED_FACE ( 'NONE', ( #25496 ), #27918, .T. ) ;
#5075 = CARTESIAN_POINT ( 'NONE',  ( 10.81189881249999551, -6.242252689847874514, -70.65625000204839523 ) ) ;
#5076 = CARTESIAN_POINT ( 'NONE',  ( -4.999999999999996447, 8.660254037844387298, -40.87500000409677625 ) ) ;
#5077 = CARTESIAN_POINT ( 'NONE',  ( -10.81189881249999729, 1.324075727343319199E-15, -5.093750002048369474 ) ) ;
#5078 = FACE_OUTER_BOUND ( 'NONE', #6755, .T. ) ;
#5079 = CARTESIAN_POINT ( 'NONE',  ( -2.293366432827344421E-15, -12.48450537969573659, -168.4062500020483810 ) ) ;
#5080 = CARTESIAN_POINT ( 'NONE',  ( 9.999999999999998224, 0.000000000000000000, -135.8750000040967905 ) ) ;
#5081 = CARTESIAN_POINT ( 'NONE',  ( 9.999999999999479527, 5.773502691896553074, -148.8749999999999432 ) ) ;
#5082 = ORIENTED_EDGE ( 'NONE', *, *, #6833, .F. ) ;
#5083 = CARTESIAN_POINT ( 'NONE',  ( -9.999999999999998224, 1.224646799147353059E-15, -115.2499999999999858 ) ) ;
#5084 = FACE_OUTER_BOUND ( 'NONE', #35114, .T. ) ;
#5085 = FACE_OUTER_BOUND ( 'NONE', #29481, .T. ) ;
#5087 = VERTEX_POINT ( 'NONE', #41049 ) ;
#5086 = CARTESIAN_POINT ( 'NONE',  ( -2.293366432827344421E-15, -12.48450537969573659, -76.90625000204839523 ) ) ;
#5088 = FACE_OUTER_BOUND ( 'NONE', #29859, .T. ) ;
#5090 = ORIENTED_EDGE ( 'NONE', *, *, #35509, .T. ) ;
#5089 = CARTESIAN_POINT ( 'NONE',  ( -9.999999999999998224, 1.224646799147353059E-15, -200.0000000000000000 ) ) ;
#5091 = ORIENTED_EDGE ( 'NONE', *, *, #14781, .F. ) ;
#5092 = CARTESIAN_POINT ( 'NONE',  ( -10.81189881249999729, 1.324075727343319199E-15, -41.09375000204837391 ) ) ;
#5093 = CARTESIAN_POINT ( 'NONE',  ( -9.999999999999998224, 1.224646799147353059E-15, -53.74999999999996447 ) ) ;
#5094 = CARTESIAN_POINT ( 'NONE',  ( 10.81189881249999551, -6.242252689847874514, -10.65625000204838280 ) ) ;
#5096 = VERTEX_POINT ( 'NONE', #5843 ) ;
#5095 = CARTESIAN_POINT ( 'NONE',  ( 7.644554776091147741E-16, 12.48450537969573659, -62.46875000204839523 ) ) ;
#5097 = DIRECTION ( 'NONE',  ( -0.000000000000000000, -0.000000000000000000, 1.000000000000000000 ) ) ;
#5098 = CARTESIAN_POINT ( 'NONE',  ( -9.999999999999998224, 5.773502691896259087, -40.37499999999997158 ) ) ;
#5099 = CARTESIAN_POINT ( 'NONE',  ( -2.293366432827344421E-15, -12.48450537969573659, -192.2187500020484379 ) ) ;
#5100 = CARTESIAN_POINT ( 'NONE',  ( -5.405949406249996869, 9.363379034771805109, -173.3437500020484094 ) ) ;
#5101 = CARTESIAN_POINT ( 'NONE',  ( -5.405949406249996869, 9.363379034771805109, -164.3437500020484094 ) ) ;
#5102 =( BOUNDED_CURVE ( )  B_SPLINE_CURVE ( 2, ( #28540, #5443, #41672, #21834, #24666, #5656, #38235 ),
 .UNSPECIFIED., .F., .F. ) 
 B_SPLINE_CURVE_WITH_KNOTS ( ( 3, 2, 2, 3 ),
 ( 0.5149253731343285123, 0.5161691542288557866, 0.5174129353233831718, 0.5186567164179105571 ),
 .UNSPECIFIED. ) 
 CURVE ( )  GEOMETRIC_REPRESENTATION_ITEM ( )  RATIONAL_B_SPLINE_CURVE ( ( 0.9999999999999880096, 0.8660254037844506980, 1.000000000000000000, 0.8660254037844387076, 1.000000000000000000, 0.8660254037844267172, 1.000000000000011990 ) ) 
 REPRESENTATION_ITEM ( '' )  );
#5103 = CARTESIAN_POINT ( 'NONE',  ( -5.405949406249996869, 9.363379034771805109, -177.8437500020483810 ) ) ;
#5104 = CARTESIAN_POINT ( 'NONE',  ( -4.999999999999996447, 8.660254037844387298, -192.0000000000000000 ) ) ;
#5105 = CARTESIAN_POINT ( 'NONE',  ( 7.644554776091147741E-16, 12.48450537969573659, -111.9687500020483952 ) ) ;
#5106 = DIRECTION ( 'NONE',  ( 1.000000000000000000, 0.000000000000000000, 0.000000000000000000 ) ) ;
#5107 = CARTESIAN_POINT ( 'NONE',  ( -2.293366432827344421E-15, -12.48450537969573659, -81.40625000204838102 ) ) ;
#5108 = CARTESIAN_POINT ( 'NONE',  ( 5.405949406249992428, -9.363379034771808662, -94.59375000204838102 ) ) ;
#5109 = CARTESIAN_POINT ( 'NONE',  ( 5.405949406249999534, 9.363379034771803333, -65.59375000204836681 ) ) ;
#5110 = CARTESIAN_POINT ( 'NONE',  ( 5.405949406249992428, -9.363379034771808662, -70.78125000204838102 ) ) ;
#5111 = CARTESIAN_POINT ( 'NONE',  ( -5.000000000000003553, -8.660254037844383745, -152.8750000040967905 ) ) ;
#5112 = CARTESIAN_POINT ( 'NONE',  ( -2.121150477449813534E-15, -11.54700538379251284, -126.8749999999999858 ) ) ;
#5113 = CARTESIAN_POINT ( 'NONE',  ( 5.405949406249999534, 9.363379034771803333, -148.2812500020483810 ) ) ;
#5114 = CARTESIAN_POINT ( 'NONE',  ( 10.81189881249999729, 0.000000000000000000, -160.5312500020484094 ) ) ;
#5115 = FACE_OUTER_BOUND ( 'NONE', #23717, .T. ) ;
#5116 = CARTESIAN_POINT ( 'NONE',  ( -9.999999999999941380, -5.773502691896284844, -197.6250000000000000 ) ) ;
#5117 = CARTESIAN_POINT ( 'NONE',  ( -10.81189881249999729, 6.242252689847871849, -96.71875000204838102 ) ) ;
#5118 = ORIENTED_EDGE ( 'NONE', *, *, #17487, .T. ) ;
#5119 = CARTESIAN_POINT ( 'NONE',  ( -10.00000000000000000, -5.773502691896251982, -64.12499999999998579 ) ) ;
#5120 = CARTESIAN_POINT ( 'NONE',  ( 10.81189881249999551, -6.242252689847874514, -197.9687500020484094 ) ) ;
#5121 = CARTESIAN_POINT ( 'NONE',  ( -9.999999999999998224, 1.224646799147353059E-15, -82.62500000409676204 ) ) ;
#5122 = EDGE_CURVE ( 'NONE', #24722, #41312, #4170, .T. ) ;
#5123 = CARTESIAN_POINT ( 'NONE',  ( 9.999999999999998224, 0.000000000000000000, -150.5000000000000000 ) ) ;
#5124 = CARTESIAN_POINT ( 'NONE',  ( -10.81189881249999907, -6.242252689847864744, -93.65625000204840944 ) ) ;
#5125 = CARTESIAN_POINT ( 'NONE',  ( 5.405949406249999534, 9.363379034771803333, -71.78125000204838102 ) ) ;
#5126 = EDGE_CURVE ( 'NONE', #6299, #18722, #28688, .T. ) ;
#5127 = CARTESIAN_POINT ( 'NONE',  ( 5.000000000000000000, 8.660254037844385522, -65.12500000409676204 ) ) ;
#5128 = DIRECTION ( 'NONE',  ( 1.000000000000000000, 0.000000000000000000, 0.000000000000000000 ) ) ;
#5129 = CARTESIAN_POINT ( 'NONE',  ( 5.405949406249999534, 9.363379034771803333, -25.09375000204835970 ) ) ;
#5130 = ORIENTED_EDGE ( 'NONE', *, *, #6833, .T. ) ;
#5131 = CARTESIAN_POINT ( 'NONE',  ( 9.999999999999998224, 0.000000000000000000, -0.4999999999999726885 ) ) ;
#5132 = ADVANCED_FACE ( 'NONE', ( #9281 ), #35418, .T. ) ;
#5133 = CARTESIAN_POINT ( 'NONE',  ( -10.81189881249999729, 1.324075727343319199E-15, -23.28125000204836326 ) ) ;
#5134 = CARTESIAN_POINT ( 'NONE',  ( 10.81189881249999729, 6.242252689847867408, -10.21875000204836326 ) ) ;
#5135 = CARTESIAN_POINT ( 'NONE',  ( -9.999999999999479527, -5.773502691896549521, -94.50000000409676204 ) ) ;
#5136 = CARTESIAN_POINT ( 'NONE',  ( 5.405949406249999534, 9.363379034771803333, -142.0937500020483810 ) ) ;
#5137 = DIRECTION ( 'NONE',  ( 0.000000000000000000, 0.000000000000000000, -1.000000000000000000 ) ) ;
#5138 = CC_DESIGN_PERSON_AND_ORGANIZATION_ASSIGNMENT ( #20679, #30206, ( #14057 ) ) ;
#5139 = CARTESIAN_POINT ( 'NONE',  ( -4.999999999999996447, 8.660254037844387298, -160.8750000040967905 ) ) ;
#5140 = CARTESIAN_POINT ( 'NONE',  ( -10.81189881249999907, -6.242252689847864744, -129.6562500020483810 ) ) ;
#5141 = CARTESIAN_POINT ( 'NONE',  ( -10.00000000000000000, -5.773502691896251982, -181.1249999999999716 ) ) ;
#5142 = DIRECTION ( 'NONE',  ( -0.000000000000000000, -0.000000000000000000, 1.000000000000000000 ) ) ;
#5144 = ORIENTED_EDGE ( 'NONE', *, *, #23603, .F. ) ;
#5143 = CARTESIAN_POINT ( 'NONE',  ( -5.405949406249996869, 9.363379034771805109, -110.5312500020483810 ) ) ;
#5145 = CARTESIAN_POINT ( 'NONE',  ( -9.999999999999998224, 1.224646799147353059E-15, -183.1250000040967905 ) ) ;
#5146 = ORIENTED_EDGE ( 'NONE', *, *, #5790, .T. ) ;
#5147 = VERTEX_POINT ( 'NONE', #35630 ) ;
#5148 = CARTESIAN_POINT ( 'NONE',  ( -5.405949406249996869, 9.363379034771805109, -41.53125000204838102 ) ) ;
#5149 = APPROVAL_ROLE ( '' ) ;
#5150 = CARTESIAN_POINT ( 'NONE',  ( -10.81189881249999729, 1.324075727343319199E-15, -89.09375000204838102 ) ) ;
#5151 = DIRECTION ( 'NONE',  ( -0.000000000000000000, -0.000000000000000000, 1.000000000000000000 ) ) ;
#5152 = CARTESIAN_POINT ( 'NONE',  ( 1.776448412236305119, 10.65631784354585498, -99.99999999999995737 ) ) ;
#5153 = CARTESIAN_POINT ( 'NONE',  ( 7.070501591499376803E-16, 11.54700538379251284, -156.5000000040968189 ) ) ;
#5154 = CARTESIAN_POINT ( 'NONE',  ( 5.405949406249992428, -9.363379034771808662, -166.7812500020484094 ) ) ;
#5155 = DIRECTION ( 'NONE',  ( 0.000000000000000000, 0.000000000000000000, 1.000000000000000000 ) ) ;
#5156 = CARTESIAN_POINT ( 'NONE',  ( 5.405949406249999534, 9.363379034771803333, -116.5937500020483810 ) ) ;
#5157 = CARTESIAN_POINT ( 'NONE',  ( -10.81189881249999907, -6.242252689847864744, -88.96875000204836681 ) ) ;
#5158 = CYLINDRICAL_SURFACE ( 'NONE', #31624, 9.999999999999998224 ) ;
#5159 = CARTESIAN_POINT ( 'NONE',  ( 7.644554776091147741E-16, 12.48450537969573659, -192.9687500020483810 ) ) ;
#5160 = CARTESIAN_POINT ( 'NONE',  ( -5.405949406249996869, 9.363379034771805109, -94.03125000204838102 ) ) ;
#5161 = CARTESIAN_POINT ( 'NONE',  ( 4.999999999999992006, -8.660254037844389075, -176.6250000040968189 ) ) ;
#5162 = CARTESIAN_POINT ( 'NONE',  ( 5.405949406249999534, 9.363379034771803333, -169.2812500020484094 ) ) ;
#5163 = CARTESIAN_POINT ( 'NONE',  ( -10.00000000000051337, 5.773502691895962435, -102.2500000040967905 ) ) ;
#5164 = CARTESIAN_POINT ( 'NONE',  ( -10.81189881249999729, -6.242252689847864744, -176.1562500020484094 ) ) ;
#5165 = CARTESIAN_POINT ( 'NONE',  ( 10.81189881249999907, 6.242252689847868297, -187.4062500020484379 ) ) ;
#5166 = CARTESIAN_POINT ( 'NONE',  ( -10.81189881249999729, 6.242252689847871849, -47.21875000204836681 ) ) ;
#5167 = CARTESIAN_POINT ( 'NONE',  ( 9.999999999999996447, -5.773502691896262640, -167.5000000040968189 ) ) ;
#5168 = CARTESIAN_POINT ( 'NONE',  ( 7.644554776091147741E-16, 12.48450537969573659, -15.96875000204836503 ) ) ;
#5169 = CARTESIAN_POINT ( 'NONE',  ( 0.000000000000000000, 0.000000000000000000, -200.0000000000000000 ) ) ;
#5170 = CARTESIAN_POINT ( 'NONE',  ( -5.405949406250003975, -9.363379034771801557, -120.3437500020483952 ) ) ;
#5171 = CARTESIAN_POINT ( 'NONE',  ( -5.000000000000003553, -8.660254037844383745, -98.49999999999998579 ) ) ;
#5172 = CARTESIAN_POINT ( 'NONE',  ( 10.81189881249999729, 0.000000000000000000, -18.03125000204835970 ) ) ;
#5173 = CARTESIAN_POINT ( 'NONE',  ( 9.999999999999996447, -5.773502691896262640, -109.0000000040967763 ) ) ;
#5174 = CARTESIAN_POINT ( 'NONE',  ( 9.999999999999994671, -5.773502691896262640, -136.0000000040967905 ) ) ;
#5175 = CARTESIAN_POINT ( 'NONE',  ( -5.000000000000003553, -8.660254037844383745, -53.49999999999996447 ) ) ;
#5176 = CARTESIAN_POINT ( 'NONE',  ( 10.81189881249999907, 6.242252689847868297, -118.4062500020484094 ) ) ;
#5177 = CARTESIAN_POINT ( 'NONE',  ( 7.644554776091147741E-16, 12.48450537969573659, -103.1562500020483952 ) ) ;
#5178 = VERTEX_POINT ( 'NONE', #22664 ) ;
#5179 = VECTOR ( 'NONE', #24692, 1000.000000000000000 ) ;
#5180 = CARTESIAN_POINT ( 'NONE',  ( 9.999999999999998224, 0.000000000000000000, -89.37500000409677625 ) ) ;
#5181 = CARTESIAN_POINT ( 'NONE',  ( 9.999999999999998224, 0.000000000000000000, -91.99999999999998579 ) ) ;
#5182 = CARTESIAN_POINT ( 'NONE',  ( 7.644554776091147741E-16, 12.48450537969573659, -155.6562500020484094 ) ) ;
#5183 = CARTESIAN_POINT ( 'NONE',  ( 5.405949406249992428, -9.363379034771808662, -52.59375000204835260 ) ) ;
#5184 = ORIENTED_EDGE ( 'NONE', *, *, #31977, .T. ) ;
#5185 = CARTESIAN_POINT ( 'NONE',  ( 7.070501591499377789E-16, 11.54700538379251284, -28.62499999999997513 ) ) ;
#5186 = CARTESIAN_POINT ( 'NONE',  ( 5.405949406249999534, 9.363379034771803333, -28.28125000204837036 ) ) ;
#5187 = CARTESIAN_POINT ( 'NONE',  ( -4.999999999999996447, 8.660254037844387298, -160.5000000000000000 ) ) ;
#5188 = CARTESIAN_POINT ( 'NONE',  ( 9.999999999999998224, 0.000000000000000000, -102.5000000000000000 ) ) ;
#5189 = CARTESIAN_POINT ( 'NONE',  ( 9.999999999999996447, -5.773502691896262640, -19.00000000409676915 ) ) ;
#5190 = EDGE_CURVE ( 'NONE', #2132, #31273, #19207, .T. ) ;
#5191 = CARTESIAN_POINT ( 'NONE',  ( -5.405949406249996869, 9.363379034771805109, -137.5312500020484094 ) ) ;
#5192 = CARTESIAN_POINT ( 'NONE',  ( -5.000020801129981152, 8.660290040615111096, 0.000000000000000000 ) ) ;
#5193 = CARTESIAN_POINT ( 'NONE',  ( -5.000000000000003553, -8.660254037844383745, -68.87500000409677625 ) ) ;
#5194 = ORIENTED_EDGE ( 'NONE', *, *, #11704, .F. ) ;
#5195 = CARTESIAN_POINT ( 'NONE',  ( 10.81189881249999907, 6.242252689847868297, -58.40625000204838102 ) ) ;
#5196 = DATE_AND_TIME ( #38000, #13860 ) ;
#5198 = VERTEX_POINT ( 'NONE', #4611 ) ;
#5197 = VERTEX_POINT ( 'NONE', #9497 ) ;
#5199 = DIRECTION ( 'NONE',  ( -1.000000000000000000, 0.000000000000000000, 0.000000000000000000 ) ) ;
#5200 = CARTESIAN_POINT ( 'NONE',  ( 4.999999999999992006, -8.660254037844389075, -183.7500000000000000 ) ) ;
#5201 = CARTESIAN_POINT ( 'NONE',  ( -10.81189881249999907, -6.242252689847864744, -154.9687500020484094 ) ) ;
#5202 = VECTOR ( 'NONE', #34967, 1000.000000000000000 ) ;
#5203 = CARTESIAN_POINT ( 'NONE',  ( 10.81189881249999907, 6.242252689847868297, -187.4062500020484379 ) ) ;
#5204 = CARTESIAN_POINT ( 'NONE',  ( 10.81189881249999729, 0.000000000000000000, -10.34375000204834549 ) ) ;
#5205 = CARTESIAN_POINT ( 'NONE',  ( 5.405949406249992428, -9.363379034771808662, -136.5937500020483810 ) ) ;
#5206 = CARTESIAN_POINT ( 'NONE',  ( 5.405949406249992428, -9.363379034771808662, -96.28125000204838102 ) ) ;
#5207 = CARTESIAN_POINT ( 'NONE',  ( -10.81189881249999729, 6.242252689847871849, -110.2187500020483810 ) ) ;
#5208 = CARTESIAN_POINT ( 'NONE',  ( 5.000000000000000000, 8.660254037844385522, -55.74999999999996447 ) ) ;
#5209 = CARTESIAN_POINT ( 'NONE',  ( 5.405949406249992428, -9.363379034771808662, -120.2812500020483952 ) ) ;
#5210 = CARTESIAN_POINT ( 'NONE',  ( 5.405949406249999534, 9.363379034771803333, -4.093750002048368586 ) ) ;
#5211 = CARTESIAN_POINT ( 'NONE',  ( 5.405949406249992428, -9.363379034771808662, -124.5937500020483952 ) ) ;
#5212 = CARTESIAN_POINT ( 'NONE',  ( -5.405949406249996869, 9.363379034771805109, -197.5312500020484094 ) ) ;
#5213 = CARTESIAN_POINT ( 'NONE',  ( -10.00000000000154188, 5.773502691895366468, -11.87499999999992006 ) ) ;
#5214 = CARTESIAN_POINT ( 'NONE',  ( 9.999999999999998224, 0.000000000000000000, -144.5000000000000000 ) ) ;
#5215 = CARTESIAN_POINT ( 'NONE',  ( 9.999999999999998224, 0.000000000000000000, -10.99999999999995381 ) ) ;
#5216 = CARTESIAN_POINT ( 'NONE',  ( -2.293366432827344421E-15, -12.48450537969573659, -73.71875000204836681 ) ) ;
#5217 = CARTESIAN_POINT ( 'NONE',  ( -5.405949406250003975, -9.363379034771801557, -55.84375000204835970 ) ) ;
#5218 = CARTESIAN_POINT ( 'NONE',  ( -9.999999999999998224, 1.224646799147353059E-15, -192.1250000040967905 ) ) ;
#5219 = CARTESIAN_POINT ( 'NONE',  ( 10.81189881249999907, 6.242252689847868297, -35.90625000204835260 ) ) ;
#5220 = CARTESIAN_POINT ( 'NONE',  ( -5.405949406249996869, 9.363379034771805109, -33.84375000204836681 ) ) ;
#5221 = CARTESIAN_POINT ( 'NONE',  ( 9.999999999999998224, 0.000000000000000000, -162.8750000040967905 ) ) ;
#5222 = CARTESIAN_POINT ( 'NONE',  ( 5.405949406249999534, 9.363379034771803333, -143.5937500020483810 ) ) ;
#5223 = CARTESIAN_POINT ( 'NONE',  ( 4.999999999999992006, -8.660254037844389075, -123.7500000000000000 ) ) ;
#5224 = CARTESIAN_POINT ( 'NONE',  ( 9.999999999999479527, 5.773502691896553074, -145.8750000000000000 ) ) ;
#5225 = CIRCLE ( 'NONE', #15554, 24.99999999999999645 ) ;
#5226 = CARTESIAN_POINT ( 'NONE',  ( 9.999999999999996447, -5.773502691896262640, -77.12499999999998579 ) ) ;
#5227 = CARTESIAN_POINT ( 'NONE',  ( -10.81189881249999907, -6.242252689847864744, -140.1562500020484094 ) ) ;
#5228 = CARTESIAN_POINT ( 'NONE',  ( 10.81189881249999729, 0.000000000000000000, -7.531250002048350822 ) ) ;
#5229 =( BOUNDED_CURVE ( )  B_SPLINE_CURVE ( 2, ( #428, #7100, #40101, #29552, #16573, #26944, #4073 ),
 .UNSPECIFIED., .F., .F. ) 
 B_SPLINE_CURVE_WITH_KNOTS ( ( 3, 2, 2, 3 ),
 ( 0.9253731343283585487, 0.9266169154228859339, 0.9278606965174133192, 0.9291044776119405935 ),
 .UNSPECIFIED. ) 
 CURVE ( )  GEOMETRIC_REPRESENTATION_ITEM ( )  RATIONAL_B_SPLINE_CURVE ( ( 0.9999999999999641398, 0.8660254037844745678, 1.000000000000000000, 0.8660254037844387076, 1.000000000000000000, 0.8660254037844028474, 1.000000000000035971 ) ) 
 REPRESENTATION_ITEM ( '' )  );
#5230 = ORIENTED_EDGE ( 'NONE', *, *, #480, .F. ) ;
#5231 = VECTOR ( 'NONE', #13385, 1000.000000000000000 ) ;
#5232 = CARTESIAN_POINT ( 'NONE',  ( 7.644554776091147741E-16, 12.48450537969573659, -101.6562500020483952 ) ) ;
#5233 = CARTESIAN_POINT ( 'NONE',  ( 5.000000000000000000, 8.660254037844385522, -116.1250000040967905 ) ) ;
#5234 = CARTESIAN_POINT ( 'NONE',  ( -9.999999999999479527, -5.773502691896549521, -140.6250000000000000 ) ) ;
#5235 = CARTESIAN_POINT ( 'NONE',  ( -10.81189881249999729, 6.242252689847871849, -77.21875000204838102 ) ) ;
#5236 = CARTESIAN_POINT ( 'NONE',  ( 4.999999999999992006, -8.660254037844389075, -29.62500000409676204 ) ) ;
#5237 = CARTESIAN_POINT ( 'NONE',  ( -9.999999999999998224, 1.224646799147353059E-15, -14.74999999999995737 ) ) ;
#5238 = CARTESIAN_POINT ( 'NONE',  ( -10.81189881249999729, 6.242252689847871849, -45.90625000204836681 ) ) ;
#5239 =( BOUNDED_CURVE ( )  B_SPLINE_CURVE ( 2, ( #38706, #36468, #38275, #9140, #8932, #30006, #20057 ),
 .UNSPECIFIED., .F., .F. ) 
 B_SPLINE_CURVE_WITH_KNOTS ( ( 3, 2, 2, 3 ),
 ( 0.4216417910447762818, 0.4228855721393036671, 0.4241293532338309413, 0.4253731343283583266 ),
 .UNSPECIFIED. ) 
 CURVE ( )  GEOMETRIC_REPRESENTATION_ITEM ( )  RATIONAL_B_SPLINE_CURVE ( ( 0.9999999999999820144, 0.8660254037844566932, 1.000000000000000000, 0.8660254037844387076, 1.000000000000000000, 0.8660254037844267172, 1.000000000000011990 ) ) 
 REPRESENTATION_ITEM ( '' )  );
#5240 = CARTESIAN_POINT ( 'NONE',  ( 4.999999999999992006, -8.660254037844389075, -137.2499999999999716 ) ) ;
#5241 = CARTESIAN_POINT ( 'NONE',  ( 5.405949406249992428, -9.363379034771808662, -144.2812500020483810 ) ) ;
#5242 = CARTESIAN_POINT ( 'NONE',  ( 5.405949406249999534, 9.363379034771803333, -125.5937500020483668 ) ) ;
#5243 = CARTESIAN_POINT ( 'NONE',  ( -9.999999999998969713, -5.773502691896847949, -65.62499999999997158 ) ) ;
#5244 = DIRECTION ( 'NONE',  ( 1.000000000000000000, 0.000000000000000000, 0.000000000000000000 ) ) ;
#5245 = ORIENTED_EDGE ( 'NONE', *, *, #40189, .T. ) ;
#5246 = VERTEX_POINT ( 'NONE', #1380 ) ;
#5247 = ORIENTED_EDGE ( 'NONE', *, *, #39940, .F. ) ;
#5248 = AXIS2_PLACEMENT_3D ( 'NONE', #22088, #14578, #27766 ) ;
#5249 = EDGE_CURVE ( 'NONE', #38512, #29237, #13223, .T. ) ;
#5250 = CARTESIAN_POINT ( 'NONE',  ( -4.999999999999996447, 8.660254037844387298, -135.3750000040967905 ) ) ;
#5251 = CARTESIAN_POINT ( 'NONE',  ( 10.81189881249999729, 0.000000000000000000, -184.3437500020483810 ) ) ;
#5252 = CARTESIAN_POINT ( 'NONE',  ( -10.81189881249999729, 1.324075727343319199E-15, -35.09375000204836681 ) ) ;
#5253 = CARTESIAN_POINT ( 'NONE',  ( -4.999999999999996447, 8.660254037844387298, -109.8750000040967763 ) ) ;
#5254 = CARTESIAN_POINT ( 'NONE',  ( -5.405949406250003975, -9.363379034771801557, -171.3437500020484094 ) ) ;
#5255 = CARTESIAN_POINT ( 'NONE',  ( -5.405949406249996869, 9.363379034771805109, -150.8437500020483810 ) ) ;
#5256 = CARTESIAN_POINT ( 'NONE',  ( 9.473483644329045106, -5.401111886679669460, 3.466673899897024536E-30 ) ) ;
#5257 = CARTESIAN_POINT ( 'NONE',  ( 10.81189881249999551, -6.242252689847874514, -136.4687500020483810 ) ) ;
#5258 = CARTESIAN_POINT ( 'NONE',  ( -10.81189881249999729, 1.324075727343319199E-15, -138.7812500020483810 ) ) ;
#5259 = CARTESIAN_POINT ( 'NONE',  ( 10.81189881249999729, 6.242252689847867408, -151.2187500020484094 ) ) ;
#5260 = DIRECTION ( 'NONE',  ( -1.000000000000000000, 0.000000000000000000, 0.000000000000000000 ) ) ;
#5261 = CARTESIAN_POINT ( 'NONE',  ( 5.000000000000000000, 8.660254037844385522, -157.7500000000000000 ) ) ;
#5262 = CARTESIAN_POINT ( 'NONE',  ( -9.999999999999998224, 1.224646799147353059E-15, -172.2500000000000000 ) ) ;
#5263 = CARTESIAN_POINT ( 'NONE',  ( -10.81189881249999729, 1.324075727343319199E-15, -81.59375000204838102 ) ) ;
#5264 = CARTESIAN_POINT ( 'NONE',  ( 9.999999999999998224, 0.000000000000000000, -81.87500000409676204 ) ) ;
#5265 = CARTESIAN_POINT ( 'NONE',  ( 10.81189881249999729, 0.000000000000000000, -61.53125000204837391 ) ) ;
#5266 = CARTESIAN_POINT ( 'NONE',  ( -10.00648583918756884, -2.605931783459911610, -100.0000000000000000 ) ) ;
#5267 = CARTESIAN_POINT ( 'NONE',  ( 5.405949406249992428, -9.363379034771808662, -171.0937500020484094 ) ) ;
#5268 = CARTESIAN_POINT ( 'NONE',  ( 10.81189881249999907, 6.242252689847868297, -116.9062500020483952 ) ) ;
#5269 = CARTESIAN_POINT ( 'NONE',  ( 10.81189881249999551, -6.242252689847874514, -145.6562500020484094 ) ) ;
#5270 = CARTESIAN_POINT ( 'NONE',  ( -9.999999999999998224, 1.224646799147353059E-15, -15.12500000409674961 ) ) ;
#5271 = CARTESIAN_POINT ( 'NONE',  ( -10.81189881249999907, -6.242252689847864744, -45.65625000204837391 ) ) ;
#5272 = CARTESIAN_POINT ( 'NONE',  ( 7.070501591499377789E-16, 11.54700538379251284, -123.5000000040967905 ) ) ;
#5273 = CARTESIAN_POINT ( 'NONE',  ( 9.999999999999998224, 0.000000000000000000, -96.49999999999998579 ) ) ;
#5274 = ORIENTED_EDGE ( 'NONE', *, *, #538, .T. ) ;
#5275 = CARTESIAN_POINT ( 'NONE',  ( 10.81189881249999729, 0.000000000000000000, -123.0312500020483952 ) ) ;
#5276 = CARTESIAN_POINT ( 'NONE',  ( 4.999999999999992006, -8.660254037844389075, -146.6250000040967905 ) ) ;
#5277 = LINE ( 'NONE', #30975, #31856 ) ;
#5278 = CARTESIAN_POINT ( 'NONE',  ( -5.405949406250003975, -9.363379034771801557, -180.5312500020483810 ) ) ;
#5279 = ORIENTED_EDGE ( 'NONE', *, *, #9308, .F. ) ;
#5280 = CARTESIAN_POINT ( 'NONE',  ( 10.81189881249999729, 0.000000000000000000, -175.3437500020483810 ) ) ;
#5281 = CARTESIAN_POINT ( 'NONE',  ( 5.000000000000000000, 8.660254037844385522, -53.12500000409675494 ) ) ;
#5282 = DIRECTION ( 'NONE',  ( 0.000000000000000000, 0.000000000000000000, 1.000000000000000000 ) ) ;
#5283 = PERSON ( 'NAUO-PER2', 'UNSPECIFIED', 'UNSPECIFIED', ('UNSPECIFIED'), ('UNSPECIFIED'), ('UNSPECIFIED') ) ;
#5284 = CARTESIAN_POINT ( 'NONE',  ( 10.81189881249999729, 0.000000000000000000, -66.03125000204838102 ) ) ;
#5285 = AXIS2_PLACEMENT_3D ( 'NONE', #30798, #38119, #21284 ) ;
#5286 = CARTESIAN_POINT ( 'NONE',  ( -2.121150477449813534E-15, -11.54700538379251284, -41.75000000409676204 ) ) ;
#5287 = CARTESIAN_POINT ( 'NONE',  ( -5.405949406249996869, 9.363379034771805109, -0.8437500020483656993 ) ) ;
#5288 = CARTESIAN_POINT ( 'NONE',  ( -2.121150477449813534E-15, -11.54700538379251284, -134.7500000040967905 ) ) ;
#5289 = CARTESIAN_POINT ( 'NONE',  ( -5.405949406250003975, -9.363379034771801557, -170.0312500020484094 ) ) ;
#5290 = CARTESIAN_POINT ( 'NONE',  ( 7.070501591499376803E-16, 11.54700538379251284, -183.5000000040967905 ) ) ;
#5291 = CARTESIAN_POINT ( 'NONE',  ( -5.000000000000003553, -8.660254037844383745, -178.0000000000000000 ) ) ;
#5292 = ORIENTED_EDGE ( 'NONE', *, *, #356, .T. ) ;
#5293 = CARTESIAN_POINT ( 'NONE',  ( -10.00000000000102496, 5.773502691895664007, -84.25000000409676204 ) ) ;
#5294 = CARTESIAN_POINT ( 'NONE',  ( -9.999999999999872102, -5.773502691896326589, -194.6250000000000000 ) ) ;
#5295 = CARTESIAN_POINT ( 'NONE',  ( -10.00000000000007994, 5.773502691896212013, -195.2500000040968189 ) ) ;
#5297 = ORIENTED_EDGE ( 'NONE', *, *, #22828, .F. ) ;
#5296 = CARTESIAN_POINT ( 'NONE',  ( -10.81189881249999729, 6.242252689847871849, -78.90625000204838102 ) ) ;
#5298 =( NAMED_UNIT ( * ) SI_UNIT ( $, .STERADIAN. ) SOLID_ANGLE_UNIT ( ) );
#5300 = ORIENTED_EDGE ( 'NONE', *, *, #5846, .F. ) ;
#5299 = CARTESIAN_POINT ( 'NONE',  ( -9.999999999999998224, 1.224646799147353059E-15, -29.74999999999997158 ) ) ;
#5301 = PRODUCT_DEFINITION_SHAPE ( 'NONE', 'NONE',  #42692 ) ;
#5302 = ORIENTED_EDGE ( 'NONE', *, *, #29746, .T. ) ;
#5303 = CARTESIAN_POINT ( 'NONE',  ( -10.81189881249999729, 6.242252689847871849, -35.21875000204835260 ) ) ;
#5304 = CARTESIAN_POINT ( 'NONE',  ( -2.121150477449813534E-15, -11.54700538379251284, -170.7500000040968189 ) ) ;
#5305 = CARTESIAN_POINT ( 'NONE',  ( 7.644554776091147741E-16, 12.48450537969573659, -5.656250002048358816 ) ) ;
#5307 = ORIENTED_EDGE ( 'NONE', *, *, #24919, .T. ) ;
#5306 = CARTESIAN_POINT ( 'NONE',  ( -10.81189881249999729, 1.324075727343319199E-15, -56.09375000204835970 ) ) ;
#5308 = CARTESIAN_POINT ( 'NONE',  ( 9.999999999999227285, 5.773502691896701400, -112.8749999999999716 ) ) ;
#5309 = EDGE_CURVE ( 'NONE', #12174, #41090, #5569, .T. ) ;
#5310 = CARTESIAN_POINT ( 'NONE',  ( 7.070501591499377789E-16, 11.54700538379251284, -40.62499999999997158 ) ) ;
#5311 = CARTESIAN_POINT ( 'NONE',  ( 10.81189881249999551, -6.242252689847874514, -196.4687500020484094 ) ) ;
#5312 = CARTESIAN_POINT ( 'NONE',  ( -10.81189881249999729, 1.324075727343319199E-15, -177.5937500020484094 ) ) ;
#5313 =( BOUNDED_CURVE ( )  B_SPLINE_CURVE ( 2, ( #6166, #16264, #9810, #39168, #12825, #29891, #13450 ),
 .UNSPECIFIED., .F., .F. ) 
 B_SPLINE_CURVE_WITH_KNOTS ( ( 3, 2, 2, 3 ),
 ( 0.1828358208955224162, 0.1840796019900497738, 0.1853233830845771313, 0.1865671641791045166 ),
 .UNSPECIFIED. ) 
 CURVE ( )  GEOMETRIC_REPRESENTATION_ITEM ( )  RATIONAL_B_SPLINE_CURVE ( ( 0.9999999999999970024, 0.8660254037844417052, 1.000000000000000000, 0.8660254037844387076, 1.000000000000000000, 0.8660254037844357100, 1.000000000000002887 ) ) 
 REPRESENTATION_ITEM ( '' )  );
#5314 = CARTESIAN_POINT ( 'NONE',  ( -5.405949406249996869, 9.363379034771805109, -153.8437500020483810 ) ) ;
#5315 = CARTESIAN_POINT ( 'NONE',  ( 10.81189881249999729, 0.000000000000000000, -175.3437500020483810 ) ) ;
#5316 = CARTESIAN_POINT ( 'NONE',  ( 9.999999999999998224, 0.000000000000000000, -101.3750000040967905 ) ) ;
#5317 = CARTESIAN_POINT ( 'NONE',  ( 7.070501591499377789E-16, 11.54700538379251284, -193.6250000000000000 ) ) ;
#5318 = CARTESIAN_POINT ( 'NONE',  ( -2.293366432827344421E-15, -12.48450537969573659, -103.7187500020483668 ) ) ;
#5319 = CARTESIAN_POINT ( 'NONE',  ( 0.000000000000000000, 0.000000000000000000, -219.9999999999999716 ) ) ;
#5320 = CARTESIAN_POINT ( 'NONE',  ( 10.81189881249999907, 6.242252689847868297, -80.90625000204839523 ) ) ;
#5321 = CARTESIAN_POINT ( 'NONE',  ( 7.644554776091147741E-16, 12.48450537969573659, -90.96875000204838102 ) ) ;
#5322 = CARTESIAN_POINT ( 'NONE',  ( -10.81189881249999907, -6.242252689847864744, -66.65625000204839523 ) ) ;
#5323 = CARTESIAN_POINT ( 'NONE',  ( -10.00000000000000000, -5.773502691896251982, -144.0000000040967905 ) ) ;
#5324 = CARTESIAN_POINT ( 'NONE',  ( -9.999999999999998224, 1.224646799147353059E-15, -127.2499999999999716 ) ) ;
#5325 = CARTESIAN_POINT ( 'NONE',  ( -5.405949406250003975, -9.363379034771801557, -150.5312500020483810 ) ) ;
#5326 = CARTESIAN_POINT ( 'NONE',  ( 7.644554776091147741E-16, 12.48450537969573659, -167.6562500020483810 ) ) ;
#5327 = CARTESIAN_POINT ( 'NONE',  ( -9.999999999999998224, 1.224646799147353059E-15, -13.62500000409674961 ) ) ;
#5328 = CARTESIAN_POINT ( 'NONE',  ( 10.00000000000012790, 5.773502691896179151, -172.8750000000000000 ) ) ;
#5329 = CARTESIAN_POINT ( 'NONE',  ( 10.81189881249999729, 0.000000000000000000, -98.84375000204838102 ) ) ;
#5330 = VERTEX_POINT ( 'NONE', #19623 ) ;
#5331 = CARTESIAN_POINT ( 'NONE',  ( 5.000000000000000000, 8.660254037844385522, -69.24999999999997158 ) ) ;
#5332 = CARTESIAN_POINT ( 'NONE',  ( -10.81189881249999729, 6.242252689847871849, -194.2187500020483810 ) ) ;
#5333 = CARTESIAN_POINT ( 'NONE',  ( 5.000000000000000000, 8.660254037844385522, -81.62500000409676204 ) ) ;
#5334 = DIRECTION ( 'NONE',  ( 0.000000000000000000, 0.000000000000000000, -1.000000000000000000 ) ) ;
#5335 = DIRECTION ( 'NONE',  ( -0.000000000000000000, -0.000000000000000000, 1.000000000000000000 ) ) ;
#5336 = CARTESIAN_POINT ( 'NONE',  ( -5.405949406250003975, -9.363379034771801557, -95.03125000204838102 ) ) ;
#5337 = CARTESIAN_POINT ( 'NONE',  ( -10.81189881249999729, 6.242252689847871849, -74.40625000204836681 ) ) ;
#5338 = CARTESIAN_POINT ( 'NONE',  ( 10.00000000000000000, 5.773502691896255534, -68.25000000409679046 ) ) ;
#5339 = LINE ( 'NONE', #21949, #22259 ) ;
#5340 = CARTESIAN_POINT ( 'NONE',  ( 10.81189881249999907, 6.242252689847868297, -25.21875000204837747 ) ) ;
#5341 = ORIENTED_EDGE ( 'NONE', *, *, #32265, .F. ) ;
#5342 = CARTESIAN_POINT ( 'NONE',  ( -10.81189881249999729, 6.242252689847871849, -192.9062500020484094 ) ) ;
#5343 = CARTESIAN_POINT ( 'NONE',  ( -5.405949406249996869, 9.363379034771805109, -17.53125000204835970 ) ) ;
#5344 = CARTESIAN_POINT ( 'NONE',  ( -5.405949406250003975, -9.363379034771801557, -7.843750002048343717 ) ) ;
#5345 = CARTESIAN_POINT ( 'NONE',  ( 9.999999999999872102, 5.773502691896329253, -160.8750000000000000 ) ) ;
#5346 = CARTESIAN_POINT ( 'NONE',  ( 10.81189881249999551, -6.242252689847874514, -146.9687500020484094 ) ) ;
#5347 = CARTESIAN_POINT ( 'NONE',  ( -9.999999999998456346, -5.773502691897145489, -50.62499999999995026 ) ) ;
#5348 = PLANE ( 'NONE',  #3164 ) ;
#5349 = CARTESIAN_POINT ( 'NONE',  ( 9.999999999999996447, -5.773502691896262640, -171.6250000000000284 ) ) ;
#5350 = CARTESIAN_POINT ( 'NONE',  ( 7.070501591499376803E-16, 11.54700538379251284, -176.0000000040967905 ) ) ;
#5352 = ORIENTED_EDGE ( 'NONE', *, *, #19995, .F. ) ;
#5351 = CARTESIAN_POINT ( 'NONE',  ( -2.293366432827344421E-15, -12.48450537969573659, -102.4062500020483952 ) ) ;
#5353 = CARTESIAN_POINT ( 'NONE',  ( 10.00000000000012257, -5.773502691896188921, -161.5000000040968189 ) ) ;
#5354 = ORIENTED_EDGE ( 'NONE', *, *, #33499, .F. ) ;
#5355 = EDGE_LOOP ( 'NONE', ( #27850, #5544, #28826, #18077 ) ) ;
#5356 =( BOUNDED_CURVE ( )  B_SPLINE_CURVE ( 2, ( #9181, #18467, #31875, #11772, #5528, #38961, #41761 ),
 .UNSPECIFIED., .F., .F. ) 
 B_SPLINE_CURVE_WITH_KNOTS ( ( 3, 2, 2, 3 ),
 ( 0.8955223880597017461, 0.8967661691542291313, 0.8980099502487565166, 0.8992537313432839019 ),
 .UNSPECIFIED. ) 
 CURVE ( )  GEOMETRIC_REPRESENTATION_ITEM ( )  RATIONAL_B_SPLINE_CURVE ( ( 0.9999999999999761302, 0.8660254037844625774, 1.000000000000000000, 0.8660254037844387076, 1.000000000000000000, 0.8660254037844028474, 1.000000000000035971 ) ) 
 REPRESENTATION_ITEM ( '' )  );
#5357 = CARTESIAN_POINT ( 'NONE',  ( 5.405949406249999534, 9.363379034771803333, -31.28125000204837036 ) ) ;
#5358 = APPROVAL_STATUS ( 'not_yet_approved' ) ;
#5359 = CARTESIAN_POINT ( 'NONE',  ( -5.405949406250003975, -9.363379034771801557, -88.84375000204838102 ) ) ;
#5360 = CARTESIAN_POINT ( 'NONE',  ( -2.121150477449813534E-15, -11.54700538379251284, -4.250000004096763817 ) ) ;
#5361 = EDGE_CURVE ( 'NONE', #24022, #258, #10543, .T. ) ;
#5362 = CARTESIAN_POINT ( 'NONE',  ( 5.000000000000000000, 8.660254037844385522, -126.2499999999999716 ) ) ;
#5363 = ADVANCED_FACE ( 'NONE', ( #42493 ), #10332, .T. ) ;
#5364 = EDGE_CURVE ( 'NONE', #19714, #4329, #35323, .T. ) ;
#5365 = ADVANCED_FACE ( 'NONE', ( #3240 ), #39481, .T. ) ;
#5366 = LINE ( 'NONE', #18519, #39817 ) ;
#5367 = CARTESIAN_POINT ( 'NONE',  ( -10.81189881249999907, -6.242252689847864744, -162.6562500020483810 ) ) ;
#5368 = CARTESIAN_POINT ( 'NONE',  ( 10.00000000000000000, 5.773502691896255534, -8.250000004096751383 ) ) ;
#5369 = CYLINDRICAL_SURFACE ( 'NONE', #9484, 9.999999999999998224 ) ;
#5370 = CARTESIAN_POINT ( 'NONE',  ( -5.405949406249996869, 9.363379034771805109, -116.3437500020483810 ) ) ;
#5371 = APPROVAL ( #39214, 'UNKNOWN' ) ;
#5372 = CARTESIAN_POINT ( 'NONE',  ( -5.405949406249996869, 9.363379034771805109, -83.34375000204836681 ) ) ;
#5373 = CARTESIAN_POINT ( 'NONE',  ( 7.644554776091147741E-16, 12.48450537969573659, -1.156250002048369474 ) ) ;
#5374 = CARTESIAN_POINT ( 'NONE',  ( 5.405949406249999534, 9.363379034771803333, -197.5937500020484094 ) ) ;
#5375 = CARTESIAN_POINT ( 'NONE',  ( -5.405949406250003975, -9.363379034771801557, -96.53125000204839523 ) ) ;
#5376 = CARTESIAN_POINT ( 'NONE',  ( -2.121150477449813534E-15, -11.54700538379251284, -181.2500000040967905 ) ) ;
#5377 = CARTESIAN_POINT ( 'NONE',  ( 10.81189881249999729, 6.242252689847867408, -172.4062500020484094 ) ) ;
#5378 = CARTESIAN_POINT ( 'NONE',  ( -10.00000000000102496, 5.773502691895664007, -68.87499999999995737 ) ) ;
#5379 = CARTESIAN_POINT ( 'NONE',  ( -10.81189881249999729, -6.242252689847864744, -173.1562500020484379 ) ) ;
#5380 = CARTESIAN_POINT ( 'NONE',  ( -5.405949406250003975, -9.363379034771801557, -188.0312500020484094 ) ) ;
#5381 = CARTESIAN_POINT ( 'NONE',  ( 5.405949406249992428, -9.363379034771808662, -46.59375000204838102 ) ) ;
#5382 = CARTESIAN_POINT ( 'NONE',  ( -9.999999999999998224, 1.224646799147353059E-15, -160.6250000040967905 ) ) ;
#5383 = CARTESIAN_POINT ( 'NONE',  ( -5.405949406249996869, 9.363379034771805109, -5.531250002048376579 ) ) ;
#5384 = CARTESIAN_POINT ( 'NONE',  ( 10.81189881249999729, 0.000000000000000000, -14.84375000204835082 ) ) ;
#5385 = CYLINDRICAL_SURFACE ( 'NONE', #35777, 9.999999999999998224 ) ;
#5386 = CARTESIAN_POINT ( 'NONE',  ( 5.405949406249999534, 9.363379034771803333, -119.5937500020483810 ) ) ;
#5387 = CARTESIAN_POINT ( 'NONE',  ( -5.000000000000003553, -8.660254037844383745, -86.49999999999998579 ) ) ;
#5388 = CARTESIAN_POINT ( 'NONE',  ( 10.81189881249999907, 6.242252689847868297, -20.90625000204837747 ) ) ;
#5389 = CARTESIAN_POINT ( 'NONE',  ( 9.999999999999996447, -5.773502691896262640, -106.0000000040967763 ) ) ;
#5390 = EDGE_CURVE ( 'NONE', #1002, #36790, #8006, .T. ) ;
#5391 = CARTESIAN_POINT ( 'NONE',  ( 9.999999999999998224, 0.000000000000000000, -135.8750000040967905 ) ) ;
#5392 = CARTESIAN_POINT ( 'NONE',  ( -9.999999999999998224, 5.773502691896259087, -50.87499999999997868 ) ) ;
#5393 = CARTESIAN_POINT ( 'NONE',  ( -10.81189881249999729, 6.242252689847871849, -119.4062500020483952 ) ) ;
#5394 = CARTESIAN_POINT ( 'NONE',  ( 10.81189881249999729, 0.000000000000000000, -102.0312500020483952 ) ) ;
#5395 = ORIENTED_EDGE ( 'NONE', *, *, #30592, .T. ) ;
#5396 = CARTESIAN_POINT ( 'NONE',  ( -2.121150477449813534E-15, -11.54700538379251284, -92.75000000409677625 ) ) ;
#5397 = DIRECTION ( 'NONE',  ( -1.000000000000000000, 0.000000000000000000, 0.000000000000000000 ) ) ;
#5398 = CARTESIAN_POINT ( 'NONE',  ( -10.81189881249999907, -6.242252689847864744, -158.1562500020484094 ) ) ;
#5399 = CARTESIAN_POINT ( 'NONE',  ( -5.405949406250003975, -9.363379034771801557, -52.84375000204835970 ) ) ;
#5401 = EDGE_CURVE ( 'NONE', #23672, #35866, #20422, .T. ) ;
#5400 = ORIENTED_EDGE ( 'NONE', *, *, #8956, .T. ) ;
#5402 = CARTESIAN_POINT ( 'NONE',  ( -10.00000000000000000, -5.773502691896251982, -19.12499999999997868 ) ) ;
#5403 = VECTOR ( 'NONE', #16964, 1000.000000000000000 ) ;
#5404 = CARTESIAN_POINT ( 'NONE',  ( 10.81189881249999729, 0.000000000000000000, -28.53125000204837036 ) ) ;
#5405 = CARTESIAN_POINT ( 'NONE',  ( -10.00000000000000000, -5.773502691896251982, -151.1250000000000284 ) ) ;
#5406 = ADVANCED_FACE ( 'NONE', ( #32808 ), #16584, .T. ) ;
#5407 = VECTOR ( 'NONE', #26904, 1000.000000000000000 ) ;
#5408 = CARTESIAN_POINT ( 'NONE',  ( -4.999999999999996447, 8.660254037844387298, -21.37500000409675494 ) ) ;
#5409 = CARTESIAN_POINT ( 'NONE',  ( -99.99999999999994316, 39.99999999999999289, -160.0000000000000000 ) ) ;
#5410 = CARTESIAN_POINT ( 'NONE',  ( 10.81189881249999907, 6.242252689847868297, -125.9062500020483810 ) ) ;
#5411 = LINE ( 'NONE', #8222, #7614 ) ;
#5412 = ADVANCED_FACE ( 'NONE', ( #20047 ), #40111, .T. ) ;
#5413 = CARTESIAN_POINT ( 'NONE',  ( -1.040834085586084257E-14, -139.9999999999999716, 42.49999999999999289 ) ) ;
#5414 = ADVANCED_FACE ( 'NONE', ( #13349, #26540 ), #39689, .F. ) ;
#5415 = VERTEX_POINT ( 'NONE', #3668 ) ;
#5416 = CARTESIAN_POINT ( 'NONE',  ( -2.293366432827344421E-15, -12.48450537969573659, -58.90625000204838813 ) ) ;
#5417 = PERSON_AND_ORGANIZATION ( #11915, #17965 ) ;
#5418 = CARTESIAN_POINT ( 'NONE',  ( 10.81189881249999551, -6.242252689847874514, -109.4687500020483810 ) ) ;
#5420 = VERTEX_POINT ( 'NONE', #22883 ) ;
#5419 = ORIENTED_EDGE ( 'NONE', *, *, #29704, .T. ) ;
#5421 = CARTESIAN_POINT ( 'NONE',  ( -5.000000000000003553, -8.660254037844383745, -85.37500000409677625 ) ) ;
#5422 = CARTESIAN_POINT ( 'NONE',  ( 10.00000000000003020, -5.773502691896243988, -197.5000000040967905 ) ) ;
#5423 = CARTESIAN_POINT ( 'NONE',  ( -10.81189881249999729, 1.324075727343319199E-15, -155.0937500020483810 ) ) ;
#5424 = CARTESIAN_POINT ( 'NONE',  ( 5.405949406249999534, 9.363379034771803333, -187.2812500020484094 ) ) ;
#5425 = CARTESIAN_POINT ( 'NONE',  ( -10.81189881249999729, 6.242252689847871849, -9.718750002048363257 ) ) ;
#5426 = CARTESIAN_POINT ( 'NONE',  ( 10.81189881249999729, 6.242252689847867408, -142.2187500020483810 ) ) ;
#5427 = AXIS2_PLACEMENT_3D ( 'NONE', #35737, #42184, #6165 ) ;
#5428 = CARTESIAN_POINT ( 'NONE',  ( -5.405949406249996869, 9.363379034771805109, -113.3437500020483810 ) ) ;
#5429 = CARTESIAN_POINT ( 'NONE',  ( 7.070501591499376803E-16, 11.54700538379251284, -191.0000000040968189 ) ) ;
#5430 = CARTESIAN_POINT ( 'NONE',  ( -5.405949406250003975, -9.363379034771801557, -119.0312500020483952 ) ) ;
#5431 = CARTESIAN_POINT ( 'NONE',  ( -10.81189881249999729, 1.324075727343319199E-15, -3.593750002048368142 ) ) ;
#5432 = CARTESIAN_POINT ( 'NONE',  ( 5.405949406249999534, 9.363379034771803333, -121.0937500020483952 ) ) ;
#5433 = CARTESIAN_POINT ( 'NONE',  ( 5.405949406249999534, 9.363379034771803333, -197.7812500020484094 ) ) ;
#5434 = CARTESIAN_POINT ( 'NONE',  ( 5.000000000000000000, 8.660254037844385522, -165.6250000040967905 ) ) ;
#5435 = CARTESIAN_POINT ( 'NONE',  ( 5.000000000000000000, 8.660254037844385522, -144.2500000000000000 ) ) ;
#5436 = CARTESIAN_POINT ( 'NONE',  ( 10.00000000000000000, 5.773502691896255534, -13.87499999999997158 ) ) ;
#5437 = EDGE_CURVE ( 'NONE', #20460, #25374, #33681, .T. ) ;
#5438 = CARTESIAN_POINT ( 'NONE',  ( -2.293366432827344421E-15, -12.48450537969573659, -70.71875000204839523 ) ) ;
#5439 = CARTESIAN_POINT ( 'NONE',  ( 10.81189881249999907, 6.242252689847868297, -56.71875000204838813 ) ) ;
#5440 = CARTESIAN_POINT ( 'NONE',  ( 7.070501591499377789E-16, 11.54700538379251284, -189.5000000040968189 ) ) ;
#5441 = CARTESIAN_POINT ( 'NONE',  ( -5.405949406249996869, 9.363379034771805109, -26.53125000204836681 ) ) ;
#5442 = CARTESIAN_POINT ( 'NONE',  ( -2.293366432827344421E-15, -12.48450537969573659, -39.21875000204835970 ) ) ;
#5443 = CARTESIAN_POINT ( 'NONE',  ( 9.999999999999479527, 5.773502691896553074, -95.25000000409674783 ) ) ;
#5444 = CARTESIAN_POINT ( 'NONE',  ( 10.81189881249999551, -6.242252689847874514, -145.4687500020483810 ) ) ;
#5445 = CARTESIAN_POINT ( 'NONE',  ( -9.999999999999998224, 5.773502691896259087, -110.8749999999999858 ) ) ;
#5446 = CARTESIAN_POINT ( 'NONE',  ( 9.999999999999998224, 0.000000000000000000, -170.0000000000000000 ) ) ;
#5447 = CARTESIAN_POINT ( 'NONE',  ( -10.00000000000000000, -5.773502691896251982, -77.62499999999998579 ) ) ;
#5448 = CARTESIAN_POINT ( 'NONE',  ( 5.405949406249999534, 9.363379034771803333, -143.7812500020483810 ) ) ;
#5449 = CARTESIAN_POINT ( 'NONE',  ( 10.81189881249999551, -6.242252689847874514, -13.65625000204836503 ) ) ;
#5450 = ORIENTED_EDGE ( 'NONE', *, *, #35980, .F. ) ;
#5451 = PLANE ( 'NONE',  #28654 ) ;
#5452 = CARTESIAN_POINT ( 'NONE',  ( -9.999999999999998224, 1.224646799147353059E-15, -117.1250000040967905 ) ) ;
#5453 = LINE ( 'NONE', #3697, #41533 ) ;
#5454 = CARTESIAN_POINT ( 'NONE',  ( 5.405949406249999534, 9.363379034771803333, -73.09375000204838102 ) ) ;
#5455 = CARTESIAN_POINT ( 'NONE',  ( -5.000000000000003553, -8.660254037844383745, -48.99999999999998579 ) ) ;
#5456 = CARTESIAN_POINT ( 'NONE',  ( 5.000000000000000000, 8.660254037844385522, -27.62500000409676204 ) ) ;
#5457 = CARTESIAN_POINT ( 'NONE',  ( 4.999999999999992006, -8.660254037844389075, -2.625000004096766926 ) ) ;
#5458 = CARTESIAN_POINT ( 'NONE',  ( -2.293366432827344421E-15, -12.48450537969573659, -40.90625000204836681 ) ) ;
#5459 = CARTESIAN_POINT ( 'NONE',  ( 4.999999999999992006, -8.660254037844389075, -99.74999999999998579 ) ) ;
#5460 = CARTESIAN_POINT ( 'NONE',  ( -5.405949406249996869, 9.363379034771805109, -148.0312500020483810 ) ) ;
#5461 = CARTESIAN_POINT ( 'NONE',  ( 10.81189881249999729, 0.000000000000000000, -153.0312500020484094 ) ) ;
#5462 = DIRECTION ( 'NONE',  ( 0.000000000000000000, 1.000000000000000000, 0.000000000000000000 ) ) ;
#5463 = DIRECTION ( 'NONE',  ( -0.000000000000000000, -0.000000000000000000, 1.000000000000000000 ) ) ;
#5464 = ORIENTED_EDGE ( 'NONE', *, *, #18255, .F. ) ;
#5465 = ORIENTED_EDGE ( 'NONE', *, *, #12760, .F. ) ;
#5466 = ORIENTED_EDGE ( 'NONE', *, *, #1000, .T. ) ;
#5467 = DIRECTION ( 'NONE',  ( 1.000000000000000000, 0.000000000000000000, 0.000000000000000000 ) ) ;
#5468 = CARTESIAN_POINT ( 'NONE',  ( 5.405949406249999534, 9.363379034771803333, -179.5937500020484094 ) ) ;
#5469 = AXIS2_PLACEMENT_3D ( 'NONE', #1605, #7863, #21011 ) ;
#5470 = CARTESIAN_POINT ( 'NONE',  ( 10.81189881249999729, 0.000000000000000000, -28.34375000204836326 ) ) ;
#5471 = CARTESIAN_POINT ( 'NONE',  ( -10.81189881249999729, 6.242252689847871849, -167.2187500020484379 ) ) ;
#5472 = CARTESIAN_POINT ( 'NONE',  ( 10.81189881249999907, 6.242252689847868297, -149.7187500020483810 ) ) ;
#5473 = DIRECTION ( 'NONE',  ( 1.000000000000000000, 0.000000000000000000, 0.000000000000000000 ) ) ;
#5474 = CARTESIAN_POINT ( 'NONE',  ( -5.405949406250003975, -9.363379034771801557, -135.3437500020484094 ) ) ;
#5475 = CARTESIAN_POINT ( 'NONE',  ( -5.405949406250003975, -9.363379034771801557, -140.0312500020484094 ) ) ;
#5476 =( BOUNDED_CURVE ( )  B_SPLINE_CURVE ( 2, ( #9646, #27110, #29935, #26685, #13073, #23030, #20409 ),
 .UNSPECIFIED., .F., .F. ) 
 B_SPLINE_CURVE_WITH_KNOTS ( ( 3, 2, 2, 3 ),
 ( 0.2276119402985075368, 0.2288557213930349221, 0.2300995024875622796, 0.2313432835820896372 ),
 .UNSPECIFIED. ) 
 CURVE ( )  GEOMETRIC_REPRESENTATION_ITEM ( )  RATIONAL_B_SPLINE_CURVE ( ( 0.9999999999999910072, 0.8660254037844477004, 1.000000000000000000, 0.8660254037844387076, 1.000000000000000000, 0.8660254037844297148, 1.000000000000008882 ) ) 
 REPRESENTATION_ITEM ( '' )  );
#5477 = CARTESIAN_POINT ( 'NONE',  ( -2.293366432827344421E-15, -12.48450537969573659, -142.7187500020483810 ) ) ;
#5478 = CARTESIAN_POINT ( 'NONE',  ( -10.00000000000076916, 5.773502691895813221, -134.8750000000000000 ) ) ;
#5479 = CARTESIAN_POINT ( 'NONE',  ( 7.070501591499377789E-16, 11.54700538379251284, -172.6249999999999716 ) ) ;
#5480 = EDGE_CURVE ( 'NONE', #11999, #38843, #6478, .T. ) ;
#5481 = CARTESIAN_POINT ( 'NONE',  ( 10.81189881249999551, -6.242252689847874514, -77.96875000204838102 ) ) ;
#5482 = CARTESIAN_POINT ( 'NONE',  ( 7.070501591499376803E-16, 11.54700538379251284, -185.0000000040967620 ) ) ;
#5483 = CARTESIAN_POINT ( 'NONE',  ( -10.81189881249999729, 6.242252689847871849, -48.90625000204836681 ) ) ;
#5484 = CARTESIAN_POINT ( 'NONE',  ( -7.290834969540838983, 7.951501520053491312, -99.99999999999995737 ) ) ;
#5485 = CARTESIAN_POINT ( 'NONE',  ( 7.644554776091147741E-16, 12.48450537969573659, -173.4687500020483810 ) ) ;
#5486 = CARTESIAN_POINT ( 'NONE',  ( -10.81189881249999729, 1.324075727343319199E-15, -111.7812500020483810 ) ) ;
#5487 = CARTESIAN_POINT ( 'NONE',  ( -10.81189881249999729, 6.242252689847871849, -149.4062500020484094 ) ) ;
#5488 = CARTESIAN_POINT ( 'NONE',  ( -4.999999999999996447, 8.660254037844387298, -142.8750000040967905 ) ) ;
#5489 = CARTESIAN_POINT ( 'NONE',  ( -10.81189881249999907, -6.242252689847864744, -42.65625000204836681 ) ) ;
#5490 = CARTESIAN_POINT ( 'NONE',  ( 9.999999999999996447, -5.773502691896262640, -121.0000000040967905 ) ) ;
#5491 = CARTESIAN_POINT ( 'NONE',  ( -9.999999999999998224, 1.224646799147353059E-15, -98.74999999999998579 ) ) ;
#5492 = ORIENTED_EDGE ( 'NONE', *, *, #7995, .T. ) ;
#5493 = CARTESIAN_POINT ( 'NONE',  ( -10.81189881249999729, -6.242252689847864744, -126.6562500020483810 ) ) ;
#5494 = CARTESIAN_POINT ( 'NONE',  ( -2.121150477449813534E-15, -11.54700538379251284, -143.7500000040968189 ) ) ;
#5495 = CARTESIAN_POINT ( 'NONE',  ( 5.000000000000000000, 8.660254037844385522, -184.7500000000000000 ) ) ;
#5496 = CARTESIAN_POINT ( 'NONE',  ( -10.81189881249999729, 6.242252689847871849, -182.4062500020483810 ) ) ;
#5497 = ORIENTED_EDGE ( 'NONE', *, *, #20467, .F. ) ;
#5498 = CARTESIAN_POINT ( 'NONE',  ( -2.121150477449813534E-15, -11.54700538379251284, -52.25000000409676915 ) ) ;
#5499 = DIRECTION ( 'NONE',  ( 1.000000000000000000, 0.000000000000000000, 0.000000000000000000 ) ) ;
#5500 = CARTESIAN_POINT ( 'NONE',  ( 10.81189881249999551, -6.242252689847874514, -69.15625000204839523 ) ) ;
#5501 = EDGE_CURVE ( 'NONE', #36434, #19099, #24382, .T. ) ;
#5502 = CARTESIAN_POINT ( 'NONE',  ( 0.000000000000000000, 0.000000000000000000, -99.99999999999998579 ) ) ;
#5503 = CARTESIAN_POINT ( 'NONE',  ( 10.81189881249999551, -6.242252689847874514, -171.1562500020484094 ) ) ;
#5504 = CARTESIAN_POINT ( 'NONE',  ( 5.000000000000000000, 8.660254037844385522, -7.749999999999978684 ) ) ;
#5505 = CARTESIAN_POINT ( 'NONE',  ( -5.000000000000003553, -8.660254037844383745, -56.49999999999996447 ) ) ;
#5506 = ORIENTED_EDGE ( 'NONE', *, *, #14973, .F. ) ;
#5507 = DIRECTION ( 'NONE',  ( 1.000000000000000000, 0.000000000000000000, 0.000000000000000000 ) ) ;
#5508 = DIRECTION ( 'NONE',  ( 1.000000000000000000, 0.000000000000000000, 0.000000000000000000 ) ) ;
#5509 = CARTESIAN_POINT ( 'NONE',  ( -10.00000000000076916, 5.773502691895813221, -136.7500000040967620 ) ) ;
#5511 = ORIENTED_EDGE ( 'NONE', *, *, #19077, .T. ) ;
#5510 = CARTESIAN_POINT ( 'NONE',  ( -10.81189881249999907, -6.242252689847864744, -80.15625000204839523 ) ) ;
#5513 = VERTEX_POINT ( 'NONE', #14631 ) ;
#5512 = CARTESIAN_POINT ( 'NONE',  ( 4.999999999999992006, -8.660254037844389075, -178.1250000040968189 ) ) ;
#5514 = ORIENTED_EDGE ( 'NONE', *, *, #29945, .F. ) ;
#5515 = CARTESIAN_POINT ( 'NONE',  ( -10.81189881249999729, 6.242252689847871849, -30.71875000204834905 ) ) ;
#5516 = CARTESIAN_POINT ( 'NONE',  ( 9.999999999999998224, 0.000000000000000000, -74.37500000409677625 ) ) ;
#5517 = CARTESIAN_POINT ( 'NONE',  ( 10.81189881249999729, 0.000000000000000000, -9.031250002048352599 ) ) ;
#5518 = CONICAL_SURFACE ( 'NONE', #26890, 60.00000000000000711, 0.7853981633974447263 ) ;
#5520 = VERTEX_POINT ( 'NONE', #20899 ) ;
#5519 = CARTESIAN_POINT ( 'NONE',  ( -5.405949406249996869, 9.363379034771805109, -56.34375000204835970 ) ) ;
#5521 = CYLINDRICAL_SURFACE ( 'NONE', #27505, 9.999999999999998224 ) ;
#5522 = CARTESIAN_POINT ( 'NONE',  ( -2.121150477449813534E-15, -11.54700538379251284, -33.87499999999995737 ) ) ;
#5523 = CARTESIAN_POINT ( 'NONE',  ( 10.81189881249999729, 0.000000000000000000, -184.3437500020483810 ) ) ;
#5524 = CARTESIAN_POINT ( 'NONE',  ( -10.81189881249999729, 1.324075727343319199E-15, -176.0937500020484094 ) ) ;
#5525 = CARTESIAN_POINT ( 'NONE',  ( 10.81189881249999907, 6.242252689847868297, -161.7187500020483810 ) ) ;
#5527 = ADVANCED_FACE ( 'NONE', ( #23729 ), #15687, .T. ) ;
#5526 = CARTESIAN_POINT ( 'NONE',  ( 5.405949406249999534, 9.363379034771803333, -172.0937500020484094 ) ) ;
#5528 = CARTESIAN_POINT ( 'NONE',  ( -4.999999999999996447, 8.660254037844387298, -18.37500000409675494 ) ) ;
#5529 = CARTESIAN_POINT ( 'NONE',  ( -2.121150477449813534E-15, -11.54700538379251284, -191.7500000040967905 ) ) ;
#5530 = CARTESIAN_POINT ( 'NONE',  ( 5.000000000000000000, 8.660254037844385522, -198.2500000000000000 ) ) ;
#5531 = CARTESIAN_POINT ( 'NONE',  ( 10.81189881249999907, 6.242252689847868297, -101.7187500020483810 ) ) ;
#5532 = DIRECTION ( 'NONE',  ( 1.000000000000000000, 0.000000000000000000, 0.000000000000000000 ) ) ;
#5533 = CARTESIAN_POINT ( 'NONE',  ( -10.81189881249999729, 6.242252689847871849, -86.40625000204836681 ) ) ;
#5534 = CARTESIAN_POINT ( 'NONE',  ( 7.644554776091147741E-16, 12.48450537969573659, -95.46875000204838102 ) ) ;
#5535 = CARTESIAN_POINT ( 'NONE',  ( -5.405949406249996869, 9.363379034771805109, -70.03125000204838102 ) ) ;
#5536 = CARTESIAN_POINT ( 'NONE',  ( 4.999999999999992006, -8.660254037844389075, -142.1250000040967905 ) ) ;
#5537 = CARTESIAN_POINT ( 'NONE',  ( 4.999999999999992006, -8.660254037844389075, -122.2500000000000000 ) ) ;
#5538 = EDGE_LOOP ( 'NONE', ( #37836, #18432, #17220, #37888 ) ) ;
#5539 = CARTESIAN_POINT ( 'NONE',  ( 10.81189881249999729, 0.000000000000000000, -148.5312500020483810 ) ) ;
#5540 = CARTESIAN_POINT ( 'NONE',  ( -10.81189881249999729, 1.324075727343319199E-15, -161.2812500020484094 ) ) ;
#5541 = LINE ( 'NONE', #42409, #29579 ) ;
#5542 = CYLINDRICAL_SURFACE ( 'NONE', #2716, 9.999999999999998224 ) ;
#5543 = CARTESIAN_POINT ( 'NONE',  ( -10.81189881249999907, -6.242252689847864744, -94.96875000204838102 ) ) ;
#5544 = ORIENTED_EDGE ( 'NONE', *, *, #15514, .T. ) ;
#5545 = CARTESIAN_POINT ( 'NONE',  ( -9.999999999999998224, 1.224646799147353059E-15, -64.24999999999997158 ) ) ;
#5546 = CARTESIAN_POINT ( 'NONE',  ( 5.405949406249999534, 9.363379034771803333, -197.5937500020484094 ) ) ;
#5547 = CARTESIAN_POINT ( 'NONE',  ( -9.999999999999998224, 1.224646799147353059E-15, -73.62500000409677625 ) ) ;
#5548 = CARTESIAN_POINT ( 'NONE',  ( -0.03154043146628307537, -10.44038505333712052, -179.9999999999999716 ) ) ;
#5549 = CARTESIAN_POINT ( 'NONE',  ( -2.121150477449813534E-15, -11.54700538379251284, -11.75000000409676737 ) ) ;
#5550 = CARTESIAN_POINT ( 'NONE',  ( 5.405949406249992428, -9.363379034771808662, -88.78125000204838102 ) ) ;
#5551 = CARTESIAN_POINT ( 'NONE',  ( -5.405949406249996869, 9.363379034771805109, -77.53125000204838102 ) ) ;
#5552 = CARTESIAN_POINT ( 'NONE',  ( 7.070501591499377789E-16, 11.54700538379251284, -66.50000000409677625 ) ) ;
#5553 = DIRECTION ( 'NONE',  ( -1.000000000000000000, 0.000000000000000000, 0.000000000000000000 ) ) ;
#5554 = CARTESIAN_POINT ( 'NONE',  ( -5.405949406249996869, 9.363379034771805109, -27.84375000204836326 ) ) ;
#5555 = CYLINDRICAL_SURFACE ( 'NONE', #14102, 9.999999999999998224 ) ;
#5556 = CARTESIAN_POINT ( 'NONE',  ( -10.81189881249999729, 6.242252689847871849, -191.4062500020484094 ) ) ;
#5557 = VECTOR ( 'NONE', #17004, 1000.000000000000000 ) ;
#5558 = CARTESIAN_POINT ( 'NONE',  ( 10.81189881249999551, -6.242252689847874514, -16.65625000204837391 ) ) ;
#5559 = EDGE_CURVE ( 'NONE', #31328, #35190, #4941, .T. ) ;
#5560 = CARTESIAN_POINT ( 'NONE',  ( -5.405949406249996869, 9.363379034771805109, -2.343750002048366810 ) ) ;
#5561 = CARTESIAN_POINT ( 'NONE',  ( 0.000000000000000000, 0.000000000000000000, -200.0000000000000000 ) ) ;
#5562 = CARTESIAN_POINT ( 'NONE',  ( -4.999999999999996447, 8.660254037844387298, -192.0000000000000000 ) ) ;
#5563 = CARTESIAN_POINT ( 'NONE',  ( 9.999999999999998224, 0.000000000000000000, -35.37500000409676915 ) ) ;
#5564 = CARTESIAN_POINT ( 'NONE',  ( -2.121150477449813534E-15, -11.54700538379251284, -177.8750000000000284 ) ) ;
#5566 = ORIENTED_EDGE ( 'NONE', *, *, #10403, .F. ) ;
#5565 = CARTESIAN_POINT ( 'NONE',  ( 7.644554776091147741E-16, 12.48450537969573659, -103.1562500020483952 ) ) ;
#5567 = CARTESIAN_POINT ( 'NONE',  ( 10.00000000000038014, -5.773502691896040595, -179.5000000040967620 ) ) ;
#5568 = ORIENTED_EDGE ( 'NONE', *, *, #5896, .F. ) ;
#5569 =( BOUNDED_CURVE ( )  B_SPLINE_CURVE ( 2, ( #34401, #17968, #35207, #26749, #30214, #10125, #23090 ),
 .UNSPECIFIED., .F., .F. ) 
 B_SPLINE_CURVE_WITH_KNOTS ( ( 3, 2, 2, 3 ),
 ( 0.9179104477611943480, 0.9191542288557217333, 0.9203980099502490075, 0.9216417910447763928 ),
 .UNSPECIFIED. ) 
 CURVE ( )  GEOMETRIC_REPRESENTATION_ITEM ( )  RATIONAL_B_SPLINE_CURVE ( ( 0.9999999999999641398, 0.8660254037844745678, 1.000000000000000000, 0.8660254037844387076, 1.000000000000000000, 0.8660254037844148378, 1.000000000000023981 ) ) 
 REPRESENTATION_ITEM ( '' )  );
#5570 = VERTEX_POINT ( 'NONE', #27819 ) ;
#5571 = CARTESIAN_POINT ( 'NONE',  ( -10.81189881249999907, -6.242252689847864744, -30.65625000204835260 ) ) ;
#5572 = DATE_AND_TIME ( #35148, #29404 ) ;
#5573 = CARTESIAN_POINT ( 'NONE',  ( 7.644554776091147741E-16, 12.48450537969573659, -77.46875000204838102 ) ) ;
#5574 = DIRECTION ( 'NONE',  ( -0.000000000000000000, 1.000000000000000000, -0.000000000000000000 ) ) ;
#5575 = CARTESIAN_POINT ( 'NONE',  ( -10.81189881249999729, 6.242252689847871849, -198.7187500020484379 ) ) ;
#5576 = CARTESIAN_POINT ( 'NONE',  ( -2.121150477449813534E-15, -11.54700538379251284, -127.2500000040967763 ) ) ;
#5577 =( REPRESENTATION_RELATIONSHIP ('NONE','NONE', #21658, #40929 ) REPRESENTATION_RELATIONSHIP_WITH_TRANSFORMATION ( #2763 )SHAPE_REPRESENTATION_RELATIONSHIP( ) );
#5578 = CARTESIAN_POINT ( 'NONE',  ( -10.81189881249999907, -6.242252689847864744, -164.1562500020484094 ) ) ;
#5579 = CARTESIAN_POINT ( 'NONE',  ( -9.999999999999998224, 5.773502691896259087, -13.75000000409676204 ) ) ;
#5580 = CARTESIAN_POINT ( 'NONE',  ( 9.999999999999866773, -5.773502691896336358, -172.0000000040967620 ) ) ;
#5581 = CARTESIAN_POINT ( 'NONE',  ( -5.405949406249996869, 9.363379034771805109, -128.3437500020484094 ) ) ;
#5582 = AXIS2_PLACEMENT_3D ( 'NONE', #18873, #12589, #31631 ) ;
#5583 = CARTESIAN_POINT ( 'NONE',  ( 10.81189881249999729, 0.000000000000000000, -116.8437500020483810 ) ) ;
#5584 = CARTESIAN_POINT ( 'NONE',  ( 5.405949406249992428, -9.363379034771808662, -82.59375000204836681 ) ) ;
#5585 = CARTESIAN_POINT ( 'NONE',  ( 10.81189881249999907, 6.242252689847868297, -191.7187500020484094 ) ) ;
#5586 = CARTESIAN_POINT ( 'NONE',  ( 7.644554776091147741E-16, 12.48450537969573659, -95.65625000204838102 ) ) ;
#5587 = CARTESIAN_POINT ( 'NONE',  ( -9.999999999999998224, 1.224646799147353059E-15, -172.6250000040968189 ) ) ;
#5588 = CARTESIAN_POINT ( 'NONE',  ( 10.81189881249999729, 0.000000000000000000, -172.5312500020484094 ) ) ;
#5589 = CARTESIAN_POINT ( 'NONE',  ( 5.000000000000000000, 8.660254037844385522, -69.24999999999997158 ) ) ;
#5590 = CARTESIAN_POINT ( 'NONE',  ( -10.81189881249999729, -6.242252689847864744, -171.6562500020484094 ) ) ;
#5591 = CARTESIAN_POINT ( 'NONE',  ( 5.405949406249999534, 9.363379034771803333, -191.7812500020484094 ) ) ;
#5592 = CARTESIAN_POINT ( 'NONE',  ( 5.405949406249992428, -9.363379034771808662, -48.09375000204838102 ) ) ;
#5593 = CARTESIAN_POINT ( 'NONE',  ( -9.999999999999998224, 1.224646799147353059E-15, -163.6250000040967905 ) ) ;
#5594 = CARTESIAN_POINT ( 'NONE',  ( 10.81189881249999551, -6.242252689847874514, -6.156250002048360592 ) ) ;
#5595 = CARTESIAN_POINT ( 'NONE',  ( 7.644554776091147741E-16, 12.48450537969573659, -17.46875000204836681 ) ) ;
#5596 = CARTESIAN_POINT ( 'NONE',  ( 7.070501591499376803E-16, 11.54700538379251284, -6.124999999999964473 ) ) ;
#5597 = CARTESIAN_POINT ( 'NONE',  ( 5.405949406249999534, 9.363379034771803333, -122.5937500020483952 ) ) ;
#5598 = CARTESIAN_POINT ( 'NONE',  ( 9.999999999999996447, -5.773502691896262640, -86.12499999999998579 ) ) ;
#5599 = CARTESIAN_POINT ( 'NONE',  ( -5.405949406250003975, -9.363379034771801557, -23.03125000204836326 ) ) ;
#5600 = CARTESIAN_POINT ( 'NONE',  ( -2.121150477449813534E-15, -11.54700538379251284, -101.7500000040967763 ) ) ;
#5601 = CARTESIAN_POINT ( 'NONE',  ( -9.999999999999998224, 1.224646799147353059E-15, -157.6250000040967905 ) ) ;
#5602 = CARTESIAN_POINT ( 'NONE',  ( -10.81189881249999729, 6.242252689847871849, -113.4062500020483810 ) ) ;
#5603 = CARTESIAN_POINT ( 'NONE',  ( -10.81189881249999729, 6.242252689847871849, -96.90625000204839523 ) ) ;
#5604 = ORIENTED_EDGE ( 'NONE', *, *, #20666, .F. ) ;
#5605 = CARTESIAN_POINT ( 'NONE',  ( -10.00000000000000000, -5.773502691896251982, -88.50000000409679046 ) ) ;
#5606 = CARTESIAN_POINT ( 'NONE',  ( -9.999999999999998224, 1.224646799147353059E-15, -4.249999999999976019 ) ) ;
#5607 = CARTESIAN_POINT ( 'NONE',  ( -5.405949406249996869, 9.363379034771805109, -154.0312500020484094 ) ) ;
#5608 = CARTESIAN_POINT ( 'NONE',  ( -2.293366432827344421E-15, -12.48450537969573659, -51.21875000204836681 ) ) ;
#5609 = EDGE_LOOP ( 'NONE', ( #14936, #24531, #13344, #38796 ) ) ;
#5610 = CARTESIAN_POINT ( 'NONE',  ( 5.000000000000000000, 8.660254037844385522, -16.74999999999996092 ) ) ;
#5611 = EDGE_CURVE ( 'NONE', #24501, #24966, #25115, .T. ) ;
#5612 = CARTESIAN_POINT ( 'NONE',  ( 10.81189881249999729, 0.000000000000000000, -30.03125000204837036 ) ) ;
#5613 = CARTESIAN_POINT ( 'NONE',  ( 9.999999999999996447, -5.773502691896262640, -156.6250000000000000 ) ) ;
#5614 = CARTESIAN_POINT ( 'NONE',  ( 4.999999999999992006, -8.660254037844389075, -22.12500000409675494 ) ) ;
#5615 = EDGE_CURVE ( 'NONE', #24472, #10661, #15996, .T. ) ;
#5616 = AXIS2_PLACEMENT_3D ( 'NONE', #9112, #12744, #9531 ) ;
#5617 =( BOUNDED_CURVE ( )  B_SPLINE_CURVE ( 2, ( #23624, #30735, #40624, #11280, #14289, #36769, #7206 ),
 .UNSPECIFIED., .F., .F. ) 
 B_SPLINE_CURVE_WITH_KNOTS ( ( 3, 2, 2, 3 ),
 ( 0.2126865671641791633, 0.2139303482587065208, 0.2151741293532339061, 0.2164179104477612636 ),
 .UNSPECIFIED. ) 
 CURVE ( )  GEOMETRIC_REPRESENTATION_ITEM ( )  RATIONAL_B_SPLINE_CURVE ( ( 0.9999999999999940048, 0.8660254037844447028, 1.000000000000000000, 0.8660254037844387076, 1.000000000000000000, 0.8660254037844297148, 1.000000000000008882 ) ) 
 REPRESENTATION_ITEM ( '' )  );
#5618 = LOCAL_TIME ( 11, 57, 6.000000000000000000, #11598 ) ;
#5619 = CARTESIAN_POINT ( 'NONE',  ( -9.999999999999998224, 5.773502691896259087, -199.3750000000000000 ) ) ;
#5621 = ORIENTED_EDGE ( 'NONE', *, *, #35493, .T. ) ;
#5620 = CARTESIAN_POINT ( 'NONE',  ( -10.81189881249999907, -6.242252689847864744, -126.6562500020483810 ) ) ;
#5622 = CARTESIAN_POINT ( 'NONE',  ( 7.070501591499376803E-16, 11.54700538379251284, -143.0000000040967905 ) ) ;
#5623 = EDGE_LOOP ( 'NONE', ( #1704, #31810, #14532, #33862 ) ) ;
#5624 =( BOUNDED_CURVE ( )  B_SPLINE_CURVE ( 2, ( #36925, #20515, #17057, #33702, #30474, #32278, #903 ),
 .UNSPECIFIED., .F., .F. ) 
 B_SPLINE_CURVE_WITH_KNOTS ( ( 3, 2, 2, 3 ),
 ( 0.4589552238805971740, 0.4601990049751245593, 0.4614427860696518890, 0.4626865671641792743 ),
 .UNSPECIFIED. ) 
 CURVE ( )  GEOMETRIC_REPRESENTATION_ITEM ( )  RATIONAL_B_SPLINE_CURVE ( ( 0.9999999999999820144, 0.8660254037844566932, 1.000000000000000000, 0.8660254037844387076, 1.000000000000000000, 0.8660254037844207220, 1.000000000000017986 ) ) 
 REPRESENTATION_ITEM ( '' )  );
#5625 = CARTESIAN_POINT ( 'NONE',  ( 10.81189881249999729, 0.000000000000000000, -55.53125000204836681 ) ) ;
#5626 = PERSON_AND_ORGANIZATION ( #11915, #17965 ) ;
#5627 = CIRCLE ( 'NONE', #10431, 9.999999999999998224 ) ;
#5628 = CARTESIAN_POINT ( 'NONE',  ( 7.644554776091147741E-16, 12.48450537969573659, -102.9687500020483952 ) ) ;
#5630 = ORIENTED_EDGE ( 'NONE', *, *, #23769, .F. ) ;
#5629 = ORIENTED_EDGE ( 'NONE', *, *, #32636, .F. ) ;
#5631 = EDGE_CURVE ( 'NONE', #22153, #22184, #36443, .T. ) ;
#5632 = CARTESIAN_POINT ( 'NONE',  ( 9.999999999999998224, 0.000000000000000000, -176.0000000000000000 ) ) ;
#5633 = CARTESIAN_POINT ( 'NONE',  ( 9.999999999999998224, 0.000000000000000000, -197.3750000040967905 ) ) ;
#5634 = CARTESIAN_POINT ( 'NONE',  ( -5.405949406250003975, -9.363379034771801557, -160.8437500020484094 ) ) ;
#5635 = CARTESIAN_POINT ( 'NONE',  ( -10.81189881249999729, 6.242252689847871849, -189.9062500020484379 ) ) ;
#5636 = CARTESIAN_POINT ( 'NONE',  ( 10.81189881249999729, 0.000000000000000000, -7.343750002048343717 ) ) ;
#5637 = CYLINDRICAL_SURFACE ( 'NONE', #17619, 9.999999999999998224 ) ;
#5638 = EDGE_CURVE ( 'NONE', #21857, #21669, #30843, .T. ) ;
#5639 = CARTESIAN_POINT ( 'NONE',  ( -5.405949406249996869, 9.363379034771805109, -140.3437500020484094 ) ) ;
#5640 = CARTESIAN_POINT ( 'NONE',  ( -10.81189881249999729, 6.242252689847871849, -113.2187500020483952 ) ) ;
#5641 = CARTESIAN_POINT ( 'NONE',  ( 10.00000000000051159, -5.773502691895965988, -149.5000000040967905 ) ) ;
#5642 = CARTESIAN_POINT ( 'NONE',  ( -5.405949406249996869, 9.363379034771805109, -116.5312500020483952 ) ) ;
#5643 = CARTESIAN_POINT ( 'NONE',  ( -5.000000000000003553, -8.660254037844383745, -193.3750000040967905 ) ) ;
#5644 = CARTESIAN_POINT ( 'NONE',  ( -5.405949406250003975, -9.363379034771801557, -121.8437500020483952 ) ) ;
#5645 = VECTOR ( 'NONE', #18229, 1000.000000000000227 ) ;
#5646 = CARTESIAN_POINT ( 'NONE',  ( 5.405949406249992428, -9.363379034771808662, -196.7812500020484094 ) ) ;
#5647 = CARTESIAN_POINT ( 'NONE',  ( 0.000000000000000000, 20.00000000000000000, -235.0000000000000000 ) ) ;
#5648 = CARTESIAN_POINT ( 'NONE',  ( -2.121150477449813534E-15, -11.54700538379251284, -150.8750000000000284 ) ) ;
#5649 = CARTESIAN_POINT ( 'NONE',  ( -5.000000000000003553, -8.660254037844383745, -15.99999999999995914 ) ) ;
#5650 = CC_DESIGN_SECURITY_CLASSIFICATION ( #138, ( #42692 ) ) ;
#5651 = CARTESIAN_POINT ( 'NONE',  ( 10.81189881249999729, 6.242252689847867408, -68.71875000204838102 ) ) ;
#5652 = CARTESIAN_POINT ( 'NONE',  ( 5.405949406249992428, -9.363379034771808662, -58.59375000204835970 ) ) ;
#5653 = CARTESIAN_POINT ( 'NONE',  ( 9.999999999999998224, 0.000000000000000000, -188.3750000040967905 ) ) ;
#5654 = CARTESIAN_POINT ( 'NONE',  ( 10.81189881249999729, 0.000000000000000000, -24.03125000204836681 ) ) ;
#5655 = CARTESIAN_POINT ( 'NONE',  ( 5.405949406249999534, 9.363379034771803333, -37.09375000204836681 ) ) ;
#5656 = CARTESIAN_POINT ( 'NONE',  ( -10.00000000000051337, 5.773502691895962435, -94.75000000409677625 ) ) ;
#5657 = CARTESIAN_POINT ( 'NONE',  ( 10.81189881249999907, 6.242252689847868297, -145.2187500020484094 ) ) ;
#5658 = CARTESIAN_POINT ( 'NONE',  ( 10.00000000000000000, 5.773502691896255534, -114.3750000000000000 ) ) ;
#5659 = CARTESIAN_POINT ( 'NONE',  ( 9.999999999999998224, 0.000000000000000000, -101.3750000040967905 ) ) ;
#5660 = CARTESIAN_POINT ( 'NONE',  ( 5.000000000000000000, 8.660254037844385522, -75.24999999999998579 ) ) ;
#5661 = CARTESIAN_POINT ( 'NONE',  ( 10.81189881249999551, -6.242252689847874514, -142.6562500020484094 ) ) ;
#5662 = CARTESIAN_POINT ( 'NONE',  ( -10.81189881249999729, -6.242252689847864744, -14.15625000204836503 ) ) ;
#5663 = ORIENTED_EDGE ( 'NONE', *, *, #34958, .T. ) ;
#5664 = CARTESIAN_POINT ( 'NONE',  ( 4.999999999999992006, -8.660254037844389075, -176.2500000000000284 ) ) ;
#5665 = CARTESIAN_POINT ( 'NONE',  ( -9.999999999999998224, 5.773502691896259087, -112.7500000040967763 ) ) ;
#5666 = CARTESIAN_POINT ( 'NONE',  ( 7.644554776091147741E-16, 12.48450537969573659, -77.46875000204838102 ) ) ;
#5667 = CARTESIAN_POINT ( 'NONE',  ( -10.00000000000000000, -5.773502691896251982, -38.62499999999995737 ) ) ;
#5668 = AXIS2_PLACEMENT_3D ( 'NONE', #12172, #21686, #2066 ) ;
#5669 = CARTESIAN_POINT ( 'NONE',  ( 7.070501591499377789E-16, 11.54700538379251284, -29.00000000409675494 ) ) ;
#5670 = ADVANCED_FACE ( 'NONE', ( #4087 ), #30428, .T. ) ;
#5671 = CARTESIAN_POINT ( 'NONE',  ( -10.81189881249999729, 1.324075727343319199E-15, -54.78125000204836681 ) ) ;
#5672 = FACE_OUTER_BOUND ( 'NONE', #17159, .T. ) ;
#5673 = CARTESIAN_POINT ( 'NONE',  ( 5.405949406249999534, 9.363379034771803333, -34.28125000204837391 ) ) ;
#5674 = EDGE_CURVE ( 'NONE', #10661, #15576, #2554, .T. ) ;
#5675 = CARTESIAN_POINT ( 'NONE',  ( 5.000000000000000000, 8.660254037844385522, -24.24999999999996447 ) ) ;
#5676 = CARTESIAN_POINT ( 'NONE',  ( 10.81189881249999729, 0.000000000000000000, -144.0312500020483810 ) ) ;
#5677 = EDGE_CURVE ( 'NONE', #27845, #32468, #26486, .T. ) ;
#5678 = CARTESIAN_POINT ( 'NONE',  ( -2.293366432827344421E-15, -12.48450537969573659, -148.9062500020483810 ) ) ;
#5679 = CARTESIAN_POINT ( 'NONE',  ( 9.999999999998969713, 5.773502691896851502, -78.75000000409674783 ) ) ;
#5680 = APPROVAL ( #42591, 'UNSPECIFIED' ) ;
#5681 = CARTESIAN_POINT ( 'NONE',  ( -9.999999999999998224, 1.224646799147353059E-15, -31.24999999999997158 ) ) ;
#5682 = EDGE_LOOP ( 'NONE', ( #1759, #20073, #33063, #21543 ) ) ;
#5683 = VECTOR ( 'NONE', #19780, 1000.000000000000000 ) ;
#5684 = ORIENTED_EDGE ( 'NONE', *, *, #41197, .T. ) ;
#5685 = VERTEX_POINT ( 'NONE', #40743 ) ;
#5686 = EDGE_CURVE ( 'NONE', #25155, #24776, #15277, .T. ) ;
#5687 = CARTESIAN_POINT ( 'NONE',  ( -5.000000000000003553, -8.660254037844383745, -100.3750000040967905 ) ) ;
#5688 = CARTESIAN_POINT ( 'NONE',  ( -10.81189881249999907, -6.242252689847864744, -178.9687500020484094 ) ) ;
#5689 = AXIS2_PLACEMENT_3D ( 'NONE', #32372, #15079, #25677 ) ;
#5690 = CARTESIAN_POINT ( 'NONE',  ( -10.81189881249999907, -6.242252689847864744, -33.46875000204834549 ) ) ;
#5691 = DIRECTION ( 'NONE',  ( -0.000000000000000000, -0.000000000000000000, -1.000000000000000000 ) ) ;
#5692 = CARTESIAN_POINT ( 'NONE',  ( 10.81189881249999729, 0.000000000000000000, -163.3437500020484094 ) ) ;
#5693 = CARTESIAN_POINT ( 'NONE',  ( 5.405949406249992428, -9.363379034771808662, -154.5937500020483810 ) ) ;
#5694 = CARTESIAN_POINT ( 'NONE',  ( 9.999999999999998224, 0.000000000000000000, -65.37500000409676204 ) ) ;
#5695 = CARTESIAN_POINT ( 'NONE',  ( 10.81189881249999907, 6.242252689847868297, -134.7187500020484094 ) ) ;
#5696 = CARTESIAN_POINT ( 'NONE',  ( -5.405949406249996869, 9.363379034771805109, -140.5312500020484094 ) ) ;
#5697 = CARTESIAN_POINT ( 'NONE',  ( 5.000000000000000000, 8.660254037844385522, -104.1250000040967763 ) ) ;
#5698 = CARTESIAN_POINT ( 'NONE',  ( -5.405949406249996869, 9.363379034771805109, -146.3437500020483810 ) ) ;
#5699 = CARTESIAN_POINT ( 'NONE',  ( 9.999999999999479527, 5.773502691896553074, -127.8749999999999858 ) ) ;
#5700 = CARTESIAN_POINT ( 'NONE',  ( 5.000000000000000000, 8.660254037844385522, -33.62500000409676915 ) ) ;
#5701 = CARTESIAN_POINT ( 'NONE',  ( -5.000000000000003553, -8.660254037844383745, -169.0000000000000000 ) ) ;
#5702 = CARTESIAN_POINT ( 'NONE',  ( -10.81189881249999907, -6.242252689847864744, -82.96875000204836681 ) ) ;
#5703 = DIRECTION ( 'NONE',  ( 1.000000000000000000, 0.000000000000000000, 0.000000000000000000 ) ) ;
#5704 = CARTESIAN_POINT ( 'NONE',  ( -5.405949406250003975, -9.363379034771801557, -53.03125000204836681 ) ) ;
#5705 = CYLINDRICAL_SURFACE ( 'NONE', #13000, 9.999999999999998224 ) ;
#5706 = CARTESIAN_POINT ( 'NONE',  ( 5.405949406249992428, -9.363379034771808662, -172.5937500020484094 ) ) ;
#5707 = CARTESIAN_POINT ( 'NONE',  ( 10.00000000000000000, 5.773502691896255534, -139.8750000000000000 ) ) ;
#5708 = CARTESIAN_POINT ( 'NONE',  ( -10.81189881249999729, 1.324075727343319199E-15, -143.2812500020483810 ) ) ;
#5709 = CARTESIAN_POINT ( 'NONE',  ( 23.09401076758504345, 1.040834085586084257E-14, 45.00000000000009237 ) ) ;
#5710 = CARTESIAN_POINT ( 'NONE',  ( -10.81189881249999729, 6.242252689847871849, -33.90625000204835970 ) ) ;
#5711 = CARTESIAN_POINT ( 'NONE',  ( -5.000000000000003553, -8.660254037844383745, -125.8750000040967905 ) ) ;
#5712 = CARTESIAN_POINT ( 'NONE',  ( -9.999999999999998224, 5.773502691896259087, -97.37500000000000000 ) ) ;
#5713 = ORIENTED_EDGE ( 'NONE', *, *, #36231, .T. ) ;
#5714 = CARTESIAN_POINT ( 'NONE',  ( 10.81189881249999729, 6.242252689847867408, -121.4062500020483810 ) ) ;
#5715 = CARTESIAN_POINT ( 'NONE',  ( 10.00000000000000000, 5.773502691896255534, -138.7500000040967905 ) ) ;
#5716 = CARTESIAN_POINT ( 'NONE',  ( -2.121150477449813534E-15, -11.54700538379251284, -22.25000000409676915 ) ) ;
#5717 = CARTESIAN_POINT ( 'NONE',  ( 10.81189881249999551, -6.242252689847874514, -172.6562500020484379 ) ) ;
#5718 = CARTESIAN_POINT ( 'NONE',  ( 5.000000000000000000, 8.660254037844385522, -50.12500000409675494 ) ) ;
#5719 = CYLINDRICAL_SURFACE ( 'NONE', #14547, 9.999999999999998224 ) ;
#5720 = CARTESIAN_POINT ( 'NONE',  ( -10.81189881249999729, 6.242252689847871849, -56.40625000204838813 ) ) ;
#5721 = CARTESIAN_POINT ( 'NONE',  ( -9.999999999999998224, 1.224646799147353059E-15, -31.24999999999997158 ) ) ;
#5722 = CARTESIAN_POINT ( 'NONE',  ( -2.293366432827344421E-15, -12.48450537969573659, -166.9062500020483810 ) ) ;
#5723 = VECTOR ( 'NONE', #28446, 1000.000000000000000 ) ;
#5724 = CARTESIAN_POINT ( 'NONE',  ( -9.999999999998969713, -5.773502691896847949, -34.50000000409672651 ) ) ;
#5725 = VERTEX_POINT ( 'NONE', #18306 ) ;
#5726 = CARTESIAN_POINT ( 'NONE',  ( -9.999999999998969713, -5.773502691896847949, -1.124999999999947597 ) ) ;
#5727 = CARTESIAN_POINT ( 'NONE',  ( -10.00000000000154188, 5.773502691895366468, -26.87499999999993960 ) ) ;
#5728 = ADVANCED_FACE ( 'NONE', ( #12251 ), #5369, .T. ) ;
#5730 = VERTEX_POINT ( 'NONE', #18734 ) ;
#5729 = CARTESIAN_POINT ( 'NONE',  ( 7.644554776091147741E-16, 12.48450537969573659, -74.65625000204838102 ) ) ;
#5732 = ORIENTED_EDGE ( 'NONE', *, *, #9584, .F. ) ;
#5731 = CARTESIAN_POINT ( 'NONE',  ( -9.999999999999998224, 1.224646799147353059E-15, -178.6250000040968189 ) ) ;
#5733 = VERTEX_POINT ( 'NONE', #38807 ) ;
#5734 =( BOUNDED_CURVE ( )  B_SPLINE_CURVE ( 2, ( #17956, #37401, #4598, #30931, #6098, #28978, #8487 ),
 .UNSPECIFIED., .F., .F. ) 
 B_SPLINE_CURVE_WITH_KNOTS ( ( 3, 2, 2, 3 ),
 ( 0.04477611940298512061, 0.04601990049751248507, 0.04726368159203984259, 0.04850746268656720706 ),
 .UNSPECIFIED. ) 
 CURVE ( )  GEOMETRIC_REPRESENTATION_ITEM ( )  RATIONAL_B_SPLINE_CURVE ( ( 0.9999999999999947820, 0.8660254037844439257, 1.000000000000000000, 0.8660254037844387076, 1.000000000000000000, 0.8660254037844342667, 1.000000000000004441 ) ) 
 REPRESENTATION_ITEM ( '' )  );
#5735 = CARTESIAN_POINT ( 'NONE',  ( 7.644554776091147741E-16, 12.48450537969573659, -32.46875000204835970 ) ) ;
#5736 = CARTESIAN_POINT ( 'NONE',  ( 10.81189881249999907, 6.242252689847868297, -4.406250002048352599 ) ) ;
#5738 = EDGE_LOOP ( 'NONE', ( #4208, #28085, #9434, #17525 ) ) ;
#5737 = CARTESIAN_POINT ( 'NONE',  ( 5.405949406249992428, -9.363379034771808662, -57.09375000204835970 ) ) ;
#5739 = CARTESIAN_POINT ( 'NONE',  ( -2.121150477449813534E-15, -11.54700538379251284, -112.2500000040967763 ) ) ;
#5740 = CARTESIAN_POINT ( 'NONE',  ( 7.070501591499377789E-16, 11.54700538379251284, -37.62499999999996447 ) ) ;
#5741 = CARTESIAN_POINT ( 'NONE',  ( 10.81189881249999551, -6.242252689847874514, -190.4687500020484094 ) ) ;
#5742 = CARTESIAN_POINT ( 'NONE',  ( 5.405949406249999534, 9.363379034771803333, -176.5937500020484094 ) ) ;
#5743 = CARTESIAN_POINT ( 'NONE',  ( -5.405949406249996869, 9.363379034771805109, -156.8437500020483810 ) ) ;
#5744 = CARTESIAN_POINT ( 'NONE',  ( 5.405949406249999534, 9.363379034771803333, -173.5937500020484094 ) ) ;
#5745 = CARTESIAN_POINT ( 'NONE',  ( -5.000000000000003553, -8.660254037844383745, -75.99999999999998579 ) ) ;
#5746 = CARTESIAN_POINT ( 'NONE',  ( -10.00000000000102496, 5.773502691895664007, -131.8749999999999432 ) ) ;
#5747 = CARTESIAN_POINT ( 'NONE',  ( -5.000000000000003553, -8.660254037844383745, -193.0000000000000000 ) ) ;
#5748 = CARTESIAN_POINT ( 'NONE',  ( 5.405949406249999534, 9.363379034771803333, -104.5937500020483810 ) ) ;
#5749 = CYLINDRICAL_SURFACE ( 'NONE', #7963, 9.999999999999998224 ) ;
#5750 = CARTESIAN_POINT ( 'NONE',  ( 5.405949406249992428, -9.363379034771808662, -72.28125000204838102 ) ) ;
#5751 = CARTESIAN_POINT ( 'NONE',  ( 10.81189881249999551, -6.242252689847874514, -89.96875000204838102 ) ) ;
#5752 = CARTESIAN_POINT ( 'NONE',  ( 10.81189881249999551, -6.242252689847874514, -61.65625000204838813 ) ) ;
#5753 = CARTESIAN_POINT ( 'NONE',  ( -2.121150477449813534E-15, -11.54700538379251284, -145.2500000040967905 ) ) ;
#5754 = CARTESIAN_POINT ( 'NONE',  ( 7.070501591499377789E-16, 11.54700538379251284, -124.6249999999999858 ) ) ;
#5755 = ORIENTED_EDGE ( 'NONE', *, *, #38350, .F. ) ;
#5756 = CARTESIAN_POINT ( 'NONE',  ( 7.644554776091147741E-16, 12.48450537969573659, -142.1562500020484094 ) ) ;
#5757 = CARTESIAN_POINT ( 'NONE',  ( -10.81189881249999729, 6.242252689847871849, -155.4062500020483810 ) ) ;
#5758 = CARTESIAN_POINT ( 'NONE',  ( -11.54700538379250396, -20.00000000000000355, 49.99999999999998579 ) ) ;
#5759 = CARTESIAN_POINT ( 'NONE',  ( -10.00000000000076916, 5.773502691895813221, -104.8749999999999716 ) ) ;
#5760 = CARTESIAN_POINT ( 'NONE',  ( 10.81189881249999551, -6.242252689847874514, -86.96875000204838102 ) ) ;
#5761 = ORIENTED_EDGE ( 'NONE', *, *, #4288, .F. ) ;
#5762 = CARTESIAN_POINT ( 'NONE',  ( 9.999999999999998224, 0.000000000000000000, -64.99999999999997158 ) ) ;
#5763 = CARTESIAN_POINT ( 'NONE',  ( 10.81189881249999907, 6.242252689847868297, -196.2187500020484094 ) ) ;
#5764 = CARTESIAN_POINT ( 'NONE',  ( 7.070501591499377789E-16, 11.54700538379251284, -74.00000000409677625 ) ) ;
#5765 = CARTESIAN_POINT ( 'NONE',  ( -9.999999999999998224, 1.224646799147353059E-15, -47.74999999999998579 ) ) ;
#5766 = LINE ( 'NONE', #31897, #1060 ) ;
#5767 = CARTESIAN_POINT ( 'NONE',  ( 10.81189881249999729, 0.000000000000000000, -88.53125000204838102 ) ) ;
#5768 = CARTESIAN_POINT ( 'NONE',  ( 5.405949406249992428, -9.363379034771808662, -69.28125000204838102 ) ) ;
#5769 = CARTESIAN_POINT ( 'NONE',  ( -2.121150477449813534E-15, -11.54700538379251284, -65.75000000409679046 ) ) ;
#5770 = CARTESIAN_POINT ( 'NONE',  ( -9.999999999999998224, 1.224646799147353059E-15, -200.0000000000000000 ) ) ;
#5771 = CARTESIAN_POINT ( 'NONE',  ( 5.405949406249992428, -9.363379034771808662, -27.09375000204835970 ) ) ;
#5772 = CARTESIAN_POINT ( 'NONE',  ( 9.999999999998969713, 5.773502691896851502, -47.25000000409674072 ) ) ;
#5773 = CARTESIAN_POINT ( 'NONE',  ( 5.405949406249999534, 9.363379034771803333, -194.7812500020484094 ) ) ;
#5774 = CARTESIAN_POINT ( 'NONE',  ( -5.405949406249996869, 9.363379034771805109, -23.53125000204836681 ) ) ;
#5775 = CARTESIAN_POINT ( 'NONE',  ( 10.81189881249999729, 6.242252689847867408, -2.718750002048361480 ) ) ;
#5776 = CARTESIAN_POINT ( 'NONE',  ( 10.00000000000076916, -5.773502691895816774, -110.5000000040967763 ) ) ;
#5777 = CARTESIAN_POINT ( 'NONE',  ( -2.121150477449813534E-15, -11.54700538379251284, -107.7500000040967763 ) ) ;
#5778 = CARTESIAN_POINT ( 'NONE',  ( 9.999999999999998224, 0.000000000000000000, -173.0000000000000284 ) ) ;
#5779 = CARTESIAN_POINT ( 'NONE',  ( 9.999999999999996447, -5.773502691896262640, -174.6250000000000000 ) ) ;
#5780 = FACE_OUTER_BOUND ( 'NONE', #2693, .T. ) ;
#5782 = ORIENTED_EDGE ( 'NONE', *, *, #3528, .F. ) ;
#5781 = CARTESIAN_POINT ( 'NONE',  ( -10.81189881249999907, -6.242252689847864744, -105.6562500020483952 ) ) ;
#5783 = CARTESIAN_POINT ( 'NONE',  ( 0.000000000000000000, 0.000000000000000000, -200.0000000000000000 ) ) ;
#5784 = VERTEX_POINT ( 'NONE', #2565 ) ;
#5785 = ORIENTED_EDGE ( 'NONE', *, *, #16511, .F. ) ;
#5786 = CARTESIAN_POINT ( 'NONE',  ( 10.81189881249999551, -6.242252689847874514, -27.15625000204838102 ) ) ;
#5787 = PERSON_AND_ORGANIZATION ( #24326, #16633 ) ;
#5788 = CARTESIAN_POINT ( 'NONE',  ( 10.81189881249999729, 0.000000000000000000, -82.34375000204836681 ) ) ;
#5789 = LINE ( 'NONE', #22397, #7054 ) ;
#5790 = EDGE_CURVE ( 'NONE', #18722, #6299, #8813, .T. ) ;
#5791 = CARTESIAN_POINT ( 'NONE',  ( 7.644554776091147741E-16, 12.48450537969573659, -197.4687500020484094 ) ) ;
#5792 = CARTESIAN_POINT ( 'NONE',  ( 4.999999999999992006, -8.660254037844389075, -130.1250000040967620 ) ) ;
#5793 = CARTESIAN_POINT ( 'NONE',  ( -9.999999999999998224, 1.224646799147353059E-15, -16.62500000409675138 ) ) ;
#5794 = CARTESIAN_POINT ( 'NONE',  ( -5.405949406250003975, -9.363379034771801557, -156.5312500020484094 ) ) ;
#5795 = CARTESIAN_POINT ( 'NONE',  ( 10.00000000000000000, 5.773502691896255534, -12.75000000409675671 ) ) ;
#5796 = CARTESIAN_POINT ( 'NONE',  ( -1.040834085586084257E-14, 125.0000000000000000, 2.499999999999992006 ) ) ;
#5797 = CARTESIAN_POINT ( 'NONE',  ( 10.81189881249999551, -6.242252689847874514, -127.4687500020483810 ) ) ;
#5798 = CARTESIAN_POINT ( 'NONE',  ( -10.81189881249999729, -6.242252689847864744, -117.4687500020483810 ) ) ;
#5799 = CARTESIAN_POINT ( 'NONE',  ( 10.81189881249999551, -6.242252689847874514, -76.46875000204838102 ) ) ;
#5800 = CARTESIAN_POINT ( 'NONE',  ( 10.81189881249999907, 6.242252689847868297, -88.40625000204839523 ) ) ;
#5801 = CARTESIAN_POINT ( 'NONE',  ( -5.000000000000003553, -8.660254037844383745, -167.8750000040967905 ) ) ;
#5802 = LINE ( 'NONE', #19376, #19926 ) ;
#5803 = CARTESIAN_POINT ( 'NONE',  ( -2.293366432827344421E-15, -12.48450537969573659, -171.4062500020484379 ) ) ;
#5804 = CARTESIAN_POINT ( 'NONE',  ( -5.405949406250003975, -9.363379034771801557, -185.0312500020484094 ) ) ;
#5805 = CARTESIAN_POINT ( 'NONE',  ( -10.81189881249999729, -6.242252689847864744, -43.96875000204835970 ) ) ;
#5806 = CARTESIAN_POINT ( 'NONE',  ( -5.000000000000003553, -8.660254037844383745, -166.3750000040967905 ) ) ;
#5807 = CARTESIAN_POINT ( 'NONE',  ( 10.81189881249999551, -6.242252689847874514, -4.656250002048353487 ) ) ;
#5808 = CARTESIAN_POINT ( 'NONE',  ( 10.81189881249999551, -6.242252689847874514, -14.96875000204836503 ) ) ;
#5809 = CARTESIAN_POINT ( 'NONE',  ( 9.999999999999998224, 0.000000000000000000, -156.5000000000000000 ) ) ;
#5810 = CARTESIAN_POINT ( 'NONE',  ( -5.405949406249996869, 9.363379034771805109, -125.3437500020483952 ) ) ;
#5811 = CARTESIAN_POINT ( 'NONE',  ( -5.000000000000003553, -8.660254037844383745, -90.99999999999998579 ) ) ;
#5812 = CARTESIAN_POINT ( 'NONE',  ( 10.81189881249999729, 0.000000000000000000, -22.53125000204836326 ) ) ;
#5813 = CARTESIAN_POINT ( 'NONE',  ( -10.00000000000000000, -5.773502691896251982, -102.0000000040967905 ) ) ;
#5814 = CYLINDRICAL_SURFACE ( 'NONE', #9289, 9.999999999999998224 ) ;
#5815 = CARTESIAN_POINT ( 'NONE',  ( 5.405949406249992428, -9.363379034771808662, -114.2812500020483952 ) ) ;
#5816 = CARTESIAN_POINT ( 'NONE',  ( -10.81189881249999729, 6.242252689847871849, -95.40625000204838102 ) ) ;
#5817 = ORIENTED_EDGE ( 'NONE', *, *, #28585, .T. ) ;
#5818 = CARTESIAN_POINT ( 'NONE',  ( 10.00000000000000000, 5.773502691896255534, -95.25000000409679046 ) ) ;
#5819 = CARTESIAN_POINT ( 'NONE',  ( -4.999999999999996447, 8.660254037844387298, -71.99999999999998579 ) ) ;
#5820 = CARTESIAN_POINT ( 'NONE',  ( -10.81189881249999729, 1.324075727343319199E-15, -156.7812500020484094 ) ) ;
#5821 = CARTESIAN_POINT ( 'NONE',  ( 10.81189881249999729, 0.000000000000000000, -52.34375000204835260 ) ) ;
#5822 = ORIENTED_EDGE ( 'NONE', *, *, #26747, .T. ) ;
#5823 = CARTESIAN_POINT ( 'NONE',  ( -9.999999999999998224, 5.773502691896259087, -20.87499999999996803 ) ) ;
#5824 = CARTESIAN_POINT ( 'NONE',  ( 10.81189881249999551, -6.242252689847874514, -31.65625000204835260 ) ) ;
#5825 = CARTESIAN_POINT ( 'NONE',  ( 9.999999999999996447, -5.773502691896262640, -153.6250000000000284 ) ) ;
#5826 =( BOUNDED_CURVE ( )  B_SPLINE_CURVE ( 2, ( #24897, #38046, #21855, #35034, #2238, #15362, #38467 ),
 .UNSPECIFIED., .F., .F. ) 
 B_SPLINE_CURVE_WITH_KNOTS ( ( 3, 2, 2, 3 ),
 ( 0.3544776119402986980, 0.3557213930348260278, 0.3569651741293533576, 0.3582089552238806873 ),
 .UNSPECIFIED. ) 
 CURVE ( )  GEOMETRIC_REPRESENTATION_ITEM ( )  RATIONAL_B_SPLINE_CURVE ( ( 0.9999999999999820144, 0.8660254037844566932, 1.000000000000000000, 0.8660254037844387076, 1.000000000000000000, 0.8660254037844267172, 1.000000000000011990 ) ) 
 REPRESENTATION_ITEM ( '' )  );
#5827 = CARTESIAN_POINT ( 'NONE',  ( -9.999999999999998224, 1.224646799147353059E-15, -21.12500000409675494 ) ) ;
#5828 = CARTESIAN_POINT ( 'NONE',  ( -10.00000000000000000, -5.773502691896251982, -197.6250000000000284 ) ) ;
#5830 = VERTEX_POINT ( 'NONE', #24812 ) ;
#5829 = CARTESIAN_POINT ( 'NONE',  ( 5.405949406249999534, 9.363379034771803333, -125.7812500020483668 ) ) ;
#5831 = CARTESIAN_POINT ( 'NONE',  ( 9.999999999998969713, 5.773502691896851502, -65.25000000409676204 ) ) ;
#5832 = ORIENTED_EDGE ( 'NONE', *, *, #9357, .F. ) ;
#5833 = CARTESIAN_POINT ( 'NONE',  ( 10.81189881249999729, 0.000000000000000000, -51.03125000204835970 ) ) ;
#5834 = CALENDAR_DATE ( 2026, 28, 9 ) ;
#5835 = CARTESIAN_POINT ( 'NONE',  ( -5.405949406249996869, 9.363379034771805109, -105.8437500020483810 ) ) ;
#5837 = ORIENTED_EDGE ( 'NONE', *, *, #36120, .F. ) ;
#5836 = VERTEX_POINT ( 'NONE', #29103 ) ;
#5838 = CARTESIAN_POINT ( 'NONE',  ( 0.000000000000000000, 0.000000000000000000, -200.0000000000000000 ) ) ;
#5839 = CARTESIAN_POINT ( 'NONE',  ( -9.999999999999998224, 1.224646799147353059E-15, -166.6250000040967905 ) ) ;
#5840 = CARTESIAN_POINT ( 'NONE',  ( -2.293366432827344421E-15, -12.48450537969573659, -156.2187500020483810 ) ) ;
#5841 = CARTESIAN_POINT ( 'NONE',  ( -10.81189881249999729, 1.324075727343319199E-15, -179.2812500020484094 ) ) ;
#5842 = CARTESIAN_POINT ( 'NONE',  ( 10.81189881249999729, 0.000000000000000000, -8.843750002048345493 ) ) ;
#5843 = CARTESIAN_POINT ( 'NONE',  ( 9.999999999999998224, 0.000000000000000000, -131.0000000000000000 ) ) ;
#5844 = EDGE_CURVE ( 'NONE', #38940, #33541, #19043, .T. ) ;
#5845 = CARTESIAN_POINT ( 'NONE',  ( -10.81189881249999729, 1.324075727343319199E-15, -143.0937500020483810 ) ) ;
#5846 = EDGE_CURVE ( 'NONE', #39187, #5967, #12909, .T. ) ;
#5847 = CARTESIAN_POINT ( 'NONE',  ( 10.81189881249999551, -6.242252689847874514, -106.4687500020483810 ) ) ;
#5848 = CARTESIAN_POINT ( 'NONE',  ( 9.999999999999998224, 0.000000000000000000, -200.0000000000000000 ) ) ;
#5849 = CARTESIAN_POINT ( 'NONE',  ( -5.405949406249996869, 9.363379034771805109, -113.5312500020483952 ) ) ;
#5850 = CARTESIAN_POINT ( 'NONE',  ( 4.999999999999992006, -8.660254037844389075, -196.1250000040967905 ) ) ;
#5851 = CARTESIAN_POINT ( 'NONE',  ( 10.81189881249999551, -6.242252689847874514, -119.9687500020483952 ) ) ;
#5852 = CARTESIAN_POINT ( 'NONE',  ( 10.81189881249999729, 0.000000000000000000, -192.0312500020484094 ) ) ;
#5853 = VECTOR ( 'NONE', #27951, 1000.000000000000000 ) ;
#5854 = CARTESIAN_POINT ( 'NONE',  ( -9.999999999999998224, 1.224646799147353059E-15, -157.2500000000000000 ) ) ;
#5855 = CARTESIAN_POINT ( 'NONE',  ( 10.00000000000000000, 5.773502691896255534, -136.8750000000000000 ) ) ;
#5856 = CARTESIAN_POINT ( 'NONE',  ( -5.000000000000003553, -8.660254037844383745, -14.49999999999995737 ) ) ;
#5857 = CARTESIAN_POINT ( 'NONE',  ( 10.81189881249999551, -6.242252689847874514, -67.46875000204838102 ) ) ;
#5858 = CARTESIAN_POINT ( 'NONE',  ( 5.405949406249999534, 9.363379034771803333, -55.09375000204835970 ) ) ;
#5859 = CARTESIAN_POINT ( 'NONE',  ( -5.000000000000003553, -8.660254037844383745, -185.8750000040967905 ) ) ;
#5860 = CARTESIAN_POINT ( 'NONE',  ( -2.293366432827344421E-15, -12.48450537969573659, -30.40625000204834905 ) ) ;
#5861 = CARTESIAN_POINT ( 'NONE',  ( -10.81189881249999729, 6.242252689847871849, -41.21875000204835970 ) ) ;
#5862 = CARTESIAN_POINT ( 'NONE',  ( -9.999999999999998224, 1.224646799147353059E-15, -21.12500000409675494 ) ) ;
#5863 = CARTESIAN_POINT ( 'NONE',  ( 5.405949406249999534, 9.363379034771803333, -149.5937500020483810 ) ) ;
#5864 = CARTESIAN_POINT ( 'NONE',  ( 10.00000000000000000, 5.773502691896255534, -109.8750000000000000 ) ) ;
#5865 = CARTESIAN_POINT ( 'NONE',  ( 7.070501591499376803E-16, 11.54700538379251284, -136.6250000000000000 ) ) ;
#5866 = CARTESIAN_POINT ( 'NONE',  ( 10.00000000000000000, 5.773502691896255534, -64.87499999999998579 ) ) ;
#5867 = CARTESIAN_POINT ( 'NONE',  ( -10.81189881249999729, 6.242252689847871849, -143.4062500020484094 ) ) ;
#5868 = CARTESIAN_POINT ( 'NONE',  ( -10.81189881249999729, -6.242252689847864744, -114.6562500020483952 ) ) ;
#5869 = ORIENTED_EDGE ( 'NONE', *, *, #26514, .T. ) ;
#5870 =( BOUNDED_CURVE ( )  B_SPLINE_CURVE ( 2, ( #41313, #24737, #37884, #1856, #34870, #5293, #2069 ),
 .UNSPECIFIED., .F., .F. ) 
 B_SPLINE_CURVE_WITH_KNOTS ( ( 3, 2, 2, 3 ),
 ( 0.5671641791044778058, 0.5684079601990051911, 0.5696517412935325764, 0.5708955223880599616 ),
 .UNSPECIFIED. ) 
 CURVE ( )  GEOMETRIC_REPRESENTATION_ITEM ( )  RATIONAL_B_SPLINE_CURVE ( ( 0.9999999999999761302, 0.8660254037844625774, 1.000000000000000000, 0.8660254037844387076, 1.000000000000000000, 0.8660254037844148378, 1.000000000000023981 ) ) 
 REPRESENTATION_ITEM ( '' )  );
#5871 = CARTESIAN_POINT ( 'NONE',  ( -10.00000000000005329, 5.773502691896226224, -196.7500000040968757 ) ) ;
#5872 = CARTESIAN_POINT ( 'NONE',  ( 9.999999999999998224, 0.000000000000000000, -119.3750000040967905 ) ) ;
#5873 = CARTESIAN_POINT ( 'NONE',  ( -4.999999999999996447, 8.660254037844387298, -169.5000000000000000 ) ) ;
#5874 = CARTESIAN_POINT ( 'NONE',  ( 10.81189881249999551, -6.242252689847874514, -76.46875000204838102 ) ) ;
#5875 = CARTESIAN_POINT ( 'NONE',  ( -9.999999999999998224, 1.224646799147353059E-15, -43.24999999999998579 ) ) ;
#5876 = CARTESIAN_POINT ( 'NONE',  ( -9.999999999999998224, 1.224646799147353059E-15, -27.12500000409676204 ) ) ;
#5877 = CARTESIAN_POINT ( 'NONE',  ( 7.644554776091147741E-16, 12.48450537969573659, -52.15625000204838102 ) ) ;
#5878 = DIRECTION ( 'NONE',  ( 0.000000000000000000, 0.000000000000000000, -1.000000000000000000 ) ) ;
#5879 = CARTESIAN_POINT ( 'NONE',  ( -10.81189881249999729, 6.242252689847871849, -35.40625000204835970 ) ) ;
#5880 =( BOUNDED_CURVE ( )  B_SPLINE_CURVE ( 2, ( #6266, #21812, #5421, #26326, #33015, #20471, #10120 ),
 .UNSPECIFIED., .F., .F. ) 
 B_SPLINE_CURVE_WITH_KNOTS ( ( 3, 2, 2, 3 ),
 ( 0.5634328358208957610, 0.5646766169154231463, 0.5659203980099504205, 0.5671641791044778058 ),
 .UNSPECIFIED. ) 
 CURVE ( )  GEOMETRIC_REPRESENTATION_ITEM ( )  RATIONAL_B_SPLINE_CURVE ( ( 0.9999999999999761302, 0.8660254037844625774, 1.000000000000000000, 0.8660254037844387076, 1.000000000000000000, 0.8660254037844148378, 1.000000000000023981 ) ) 
 REPRESENTATION_ITEM ( '' )  );
#5881 = CARTESIAN_POINT ( 'NONE',  ( -5.000000000000003553, -8.660254037844383745, -105.9999999999999858 ) ) ;
#5882 = CARTESIAN_POINT ( 'NONE',  ( -5.405949406249996869, 9.363379034771805109, -145.0312500020483810 ) ) ;
#5883 = CARTESIAN_POINT ( 'NONE',  ( -5.405949406249996869, 9.363379034771805109, -149.5312500020483810 ) ) ;
#5884 = CARTESIAN_POINT ( 'NONE',  ( 9.999999999999998224, 0.000000000000000000, -164.3750000040967905 ) ) ;
#5885 = CARTESIAN_POINT ( 'NONE',  ( -9.999999999999998224, 1.224646799147353059E-15, -200.0000000000000000 ) ) ;
#5886 = ORIENTED_EDGE ( 'NONE', *, *, #8126, .T. ) ;
#5887 = ORIENTED_EDGE ( 'NONE', *, *, #16876, .F. ) ;
#5888 = ORIENTED_EDGE ( 'NONE', *, *, #40899, .F. ) ;
#5889 = CARTESIAN_POINT ( 'NONE',  ( 10.00000000000051159, -5.773502691895965988, -100.0000000040968047 ) ) ;
#5890 = CARTESIAN_POINT ( 'NONE',  ( 5.405949406249999534, 9.363379034771803333, -185.5937500020483810 ) ) ;
#5891 = CARTESIAN_POINT ( 'NONE',  ( 10.81189881249999907, 6.242252689847868297, -31.21875000204835260 ) ) ;
#5892 = CARTESIAN_POINT ( 'NONE',  ( -4.999999999999996447, 8.660254037844387298, -118.5000000000000000 ) ) ;
#5893 = EDGE_CURVE ( 'NONE', #30027, #3790, #15744, .T. ) ;
#5894 = CARTESIAN_POINT ( 'NONE',  ( -5.405949406249996869, 9.363379034771805109, -161.3437500020484094 ) ) ;
#5895 = CARTESIAN_POINT ( 'NONE',  ( 10.81189881249999907, 6.242252689847868297, -151.2187500020483810 ) ) ;
#5896 = EDGE_CURVE ( 'NONE', #23620, #3659, #24860, .T. ) ;
#5897 = CARTESIAN_POINT ( 'NONE',  ( 10.10436387341741948, -4.101143746035988968, 1.152242674263551285E-14 ) ) ;
#5898 = CARTESIAN_POINT ( 'NONE',  ( 5.405949406249999534, 9.363379034771803333, -134.5937500020483810 ) ) ;
#5899 = VECTOR ( 'NONE', #17979, 1000.000000000000000 ) ;
#5900 = CARTESIAN_POINT ( 'NONE',  ( 5.405949406249999534, 9.363379034771803333, -137.7812500020483810 ) ) ;
#5901 = CARTESIAN_POINT ( 'NONE',  ( -10.81189881249999729, 1.324075727343319199E-15, -17.09375000204835260 ) ) ;
#5903 = ADVANCED_FACE ( 'NONE', ( #15897 ), #6009, .F. ) ;
#5902 = CARTESIAN_POINT ( 'NONE',  ( -10.81189881249999729, -6.242252689847864744, -148.9687500020484094 ) ) ;
#5904 = CYLINDRICAL_SURFACE ( 'NONE', #32299, 9.999999999999998224 ) ;
#5905 = CARTESIAN_POINT ( 'NONE',  ( 9.999999999999998224, 0.000000000000000000, -70.99999999999998579 ) ) ;
#5906 = CARTESIAN_POINT ( 'NONE',  ( -9.999999999999998224, 1.224646799147353059E-15, -164.7500000000000000 ) ) ;
#5907 = CARTESIAN_POINT ( 'NONE',  ( -10.81189881249999729, 6.242252689847871849, -81.71875000204838102 ) ) ;
#5908 = DIRECTION ( 'NONE',  ( -0.000000000000000000, -0.000000000000000000, -1.000000000000000000 ) ) ;
#5909 = CARTESIAN_POINT ( 'NONE',  ( -10.81189881249999729, 1.324075727343319199E-15, -50.28125000204835970 ) ) ;
#5910 = CARTESIAN_POINT ( 'NONE',  ( -2.293366432827344421E-15, -12.48450537969573659, -58.71875000204837391 ) ) ;
#5911 = CARTESIAN_POINT ( 'NONE',  ( 9.999999999999998224, 1.224646799147353059E-15, -99.99999999999998579 ) ) ;
#5912 = CARTESIAN_POINT ( 'NONE',  ( 7.644554776091147741E-16, 12.48450537969573659, -168.9687500020483810 ) ) ;
#5913 = CARTESIAN_POINT ( 'NONE',  ( -2.121150477449813534E-15, -11.54700538379251284, -135.8750000000000000 ) ) ;
#5914 = AXIS2_PLACEMENT_3D ( 'NONE', #41951, #22121, #28399 ) ;
#5915 = CARTESIAN_POINT ( 'NONE',  ( 10.81189881249999729, 6.242252689847867408, -148.4062500020484094 ) ) ;
#5916 = APPROVAL ( #10634, 'UNSPECIFIED' ) ;
#5917 = CARTESIAN_POINT ( 'NONE',  ( 9.999999999999479527, 5.773502691896553074, -143.2500000040967905 ) ) ;
#5918 = CARTESIAN_POINT ( 'NONE',  ( 7.070501591499377789E-16, 11.54700538379251284, -120.5000000040967905 ) ) ;
#5919 = CARTESIAN_POINT ( 'NONE',  ( 5.000000000000000000, 8.660254037844385522, -96.24999999999998579 ) ) ;
#5920 = EDGE_LOOP ( 'NONE', ( #19867, #7524, #23507, #21156 ) ) ;
#5921 = CARTESIAN_POINT ( 'NONE',  ( -10.81189881249999729, -6.242252689847864744, -122.1562500020483810 ) ) ;
#5922 = CARTESIAN_POINT ( 'NONE',  ( 4.999999999999992006, -8.660254037844389075, -142.1250000040967905 ) ) ;
#5923 = CARTESIAN_POINT ( 'NONE',  ( 9.999999999999998224, 0.000000000000000000, -84.87500000409677625 ) ) ;
#5924 = CARTESIAN_POINT ( 'NONE',  ( 10.81189881249999729, 0.000000000000000000, -175.5312500020483810 ) ) ;
#5925 = CARTESIAN_POINT ( 'NONE',  ( 5.000000000000000000, 8.660254037844385522, -51.62500000409675494 ) ) ;
#5926 = CARTESIAN_POINT ( 'NONE',  ( -9.999999999999998224, 1.224646799147353059E-15, -98.74999999999998579 ) ) ;
#5927 = CARTESIAN_POINT ( 'NONE',  ( 5.405949406249992428, -9.363379034771808662, -63.28125000204837391 ) ) ;
#5928 = CARTESIAN_POINT ( 'NONE',  ( 9.999999999999998224, 0.000000000000000000, -9.875000004096746054 ) ) ;
#5929 = CARTESIAN_POINT ( 'NONE',  ( 10.81189881249999907, 6.242252689847868297, -169.4062500020484094 ) ) ;
#5930 = EDGE_CURVE ( 'NONE', #34292, #1053, #14353, .T. ) ;
#5931 = CARTESIAN_POINT ( 'NONE',  ( 5.000000000000000000, 8.660254037844385522, -183.6250000040967905 ) ) ;
#5932 = FACE_OUTER_BOUND ( 'NONE', #16627, .T. ) ;
#5933 = ORIENTED_EDGE ( 'NONE', *, *, #3546, .T. ) ;
#5934 = CARTESIAN_POINT ( 'NONE',  ( -9.999999999999998224, 1.224646799147353059E-15, -123.1250000040967905 ) ) ;
#5935 = AXIS2_PLACEMENT_3D ( 'NONE', #14018, #2703, #6942 ) ;
#5936 = VECTOR ( 'NONE', #25218, 1000.000000000000000 ) ;
#5937 = CARTESIAN_POINT ( 'NONE',  ( 9.999999999999998224, 0.000000000000000000, -137.3750000040967905 ) ) ;
#5939 = VERTEX_POINT ( 'NONE', #41606 ) ;
#5938 = CARTESIAN_POINT ( 'NONE',  ( 10.81189881249999907, 6.242252689847868297, -79.40625000204839523 ) ) ;
#5940 =( NAMED_UNIT ( * ) PLANE_ANGLE_UNIT ( ) SI_UNIT ( $, .RADIAN. ) );
#5942 = ORIENTED_EDGE ( 'NONE', *, *, #20424, .F. ) ;
#5941 = DIRECTION ( 'NONE',  ( -0.000000000000000000, -0.000000000000000000, 1.000000000000000000 ) ) ;
#5943 = VECTOR ( 'NONE', #21330, 999.9999999999998863 ) ;
#5944 =( BOUNDED_CURVE ( )  B_SPLINE_CURVE ( 2, ( #14937, #41269, #34189, #17322, #11707, #21213, #37621 ),
 .UNSPECIFIED., .F., .F. ) 
 B_SPLINE_CURVE_WITH_KNOTS ( ( 3, 2, 2, 3 ),
 ( 0.2649253731343284568, 0.2661691542288558421, 0.2674129353233831718, 0.2686567164179105571 ),
 .UNSPECIFIED. ) 
 CURVE ( )  GEOMETRIC_REPRESENTATION_ITEM ( )  RATIONAL_B_SPLINE_CURVE ( ( 0.9999999999999880096, 0.8660254037844506980, 1.000000000000000000, 0.8660254037844387076, 1.000000000000000000, 0.8660254037844267172, 1.000000000000011990 ) ) 
 REPRESENTATION_ITEM ( '' )  );
#5945 = ORIENTED_EDGE ( 'NONE', *, *, #2764, .F. ) ;
#5946 = CARTESIAN_POINT ( 'NONE',  ( 10.81189881249999551, -6.242252689847874514, -26.96875000204837747 ) ) ;
#5947 = CARTESIAN_POINT ( 'NONE',  ( 9.999999999999998224, 0.000000000000000000, -159.5000000000000000 ) ) ;
#5948 = CARTESIAN_POINT ( 'NONE',  ( -5.405949406249996869, 9.363379034771805109, -5.531250002048376579 ) ) ;
#5950 = EDGE_LOOP ( 'NONE', ( #25169, #34075, #32926, #26843 ) ) ;
#5949 = CARTESIAN_POINT ( 'NONE',  ( 5.405949406249992428, -9.363379034771808662, -52.59375000204835260 ) ) ;
#5951 = CARTESIAN_POINT ( 'NONE',  ( 4.999999999999992006, -8.660254037844389075, -3.749999999999975575 ) ) ;
#5952 = CARTESIAN_POINT ( 'NONE',  ( 7.070501591499377789E-16, 11.54700538379251284, -27.12499999999998224 ) ) ;
#5953 = CARTESIAN_POINT ( 'NONE',  ( 5.405949406249992428, -9.363379034771808662, -190.5937500020484094 ) ) ;
#5954 = CARTESIAN_POINT ( 'NONE',  ( 5.405949406249992428, -9.363379034771808662, -177.0937500020484094 ) ) ;
#5955 = CARTESIAN_POINT ( 'NONE',  ( -10.81189881249999729, 6.242252689847871849, -161.2187500020483526 ) ) ;
#5956 = CARTESIAN_POINT ( 'NONE',  ( 5.405949406249992428, -9.363379034771808662, -169.5937500020484094 ) ) ;
#5957 = CARTESIAN_POINT ( 'NONE',  ( 9.999999999999998224, 0.000000000000000000, -125.0000000000000000 ) ) ;
#5958 = CARTESIAN_POINT ( 'NONE',  ( 10.00000000000051159, -5.773502691895965988, -101.5000000040967763 ) ) ;
#5959 = CARTESIAN_POINT ( 'NONE',  ( 9.999999999999998224, 0.000000000000000000, -191.0000000000000000 ) ) ;
#5960 = CARTESIAN_POINT ( 'NONE',  ( 5.405949406249992428, -9.363379034771808662, -108.0937500020483810 ) ) ;
#5961 = CARTESIAN_POINT ( 'NONE',  ( 7.644554776091147741E-16, 12.48450537969573659, -77.65625000204838102 ) ) ;
#5962 = CARTESIAN_POINT ( 'NONE',  ( 10.81189881249999551, -6.242252689847874514, -85.46875000204836681 ) ) ;
#5963 = CIRCLE ( 'NONE', #5248, 22.00000000000000711 ) ;
#5964 = CARTESIAN_POINT ( 'NONE',  ( 7.644554776091147741E-16, 12.48450537969573659, -58.15625000204838102 ) ) ;
#5965 = CARTESIAN_POINT ( 'NONE',  ( -9.999999999999998224, 1.224646799147353059E-15, -147.1250000040967905 ) ) ;
#5966 = CARTESIAN_POINT ( 'NONE',  ( 4.999999999999992006, -8.660254037844389075, -123.7500000000000000 ) ) ;
#5967 = VERTEX_POINT ( 'NONE', #5796 ) ;
#5968 = CARTESIAN_POINT ( 'NONE',  ( -2.293366432827344421E-15, -12.48450537969573659, -145.9062500020484094 ) ) ;
#5969 = CARTESIAN_POINT ( 'NONE',  ( -2.293366432827344421E-15, -12.48450537969573659, -159.4062500020483810 ) ) ;
#5970 = EDGE_CURVE ( 'NONE', #2425, #39731, #6941, .T. ) ;
#5971 = CARTESIAN_POINT ( 'NONE',  ( 10.81189881249999907, 6.242252689847868297, -199.4062500020484094 ) ) ;
#5972 = CARTESIAN_POINT ( 'NONE',  ( -5.000000000000003553, -8.660254037844383745, -51.99999999999996447 ) ) ;
#5973 = CARTESIAN_POINT ( 'NONE',  ( 7.644554776091147741E-16, 12.48450537969573659, -90.96875000204838102 ) ) ;
#5974 = VERTEX_POINT ( 'NONE', #39636 ) ;
#5975 = CARTESIAN_POINT ( 'NONE',  ( 5.000000000000000000, 8.660254037844385522, -64.74999999999997158 ) ) ;
#5976 = CARTESIAN_POINT ( 'NONE',  ( 5.405949406249999534, 9.363379034771803333, -188.5937500020483810 ) ) ;
#5977 = CARTESIAN_POINT ( 'NONE',  ( -5.000000000000003553, -8.660254037844383745, -76.37500000409677625 ) ) ;
#5978 = CARTESIAN_POINT ( 'NONE',  ( 0.000000000000000000, 0.000000000000000000, -200.0000000000000000 ) ) ;
#5979 = LINE ( 'NONE', #41996, #30034 ) ;
#5980 = CARTESIAN_POINT ( 'NONE',  ( 10.81189881249999729, 0.000000000000000000, -85.53125000204838102 ) ) ;
#5981 = CARTESIAN_POINT ( 'NONE',  ( 7.644554776091147741E-16, 12.48450537969573659, -68.65625000204840944 ) ) ;
#5982 = CARTESIAN_POINT ( 'NONE',  ( -10.00000000000000000, -5.773502691896251982, -60.00000000409677625 ) ) ;
#5983 = CARTESIAN_POINT ( 'NONE',  ( 10.81189881249999551, -6.242252689847874514, -14.96875000204836503 ) ) ;
#5984 = VERTEX_POINT ( 'NONE', #20000 ) ;
#5985 = CARTESIAN_POINT ( 'NONE',  ( 5.405949406249992428, -9.363379034771808662, -189.2812500020484094 ) ) ;
#5986 = CARTESIAN_POINT ( 'NONE',  ( 5.405949406249999534, 9.363379034771803333, -8.781250002048352599 ) ) ;
#5987 = CARTESIAN_POINT ( 'NONE',  ( -2.293366432827344421E-15, -12.48450537969573659, -3.218750002048363257 ) ) ;
#5988 = CARTESIAN_POINT ( 'NONE',  ( -4.999999999999996447, 8.660254037844387298, -136.8750000040967905 ) ) ;
#5989 = CARTESIAN_POINT ( 'NONE',  ( -9.999999999999998224, 1.224646799147353059E-15, -181.2500000000000284 ) ) ;
#5990 = CARTESIAN_POINT ( 'NONE',  ( 9.999999999999998224, 0.000000000000000000, -155.3750000040967905 ) ) ;
#5991 =( BOUNDED_CURVE ( )  B_SPLINE_CURVE ( 2, ( #22073, #5243, #18612, #15991, #21854, #19245, #2437 ),
 .UNSPECIFIED., .F., .F. ) 
 B_SPLINE_CURVE_WITH_KNOTS ( ( 3, 2, 2, 3 ),
 ( 0.6679104477611942370, 0.6691542288557216223, 0.6703980099502490075, 0.6716417910447763928 ),
 .UNSPECIFIED. ) 
 CURVE ( )  GEOMETRIC_REPRESENTATION_ITEM ( )  RATIONAL_B_SPLINE_CURVE ( ( 0.9999999999999761302, 0.8660254037844625774, 1.000000000000000000, 0.8660254037844387076, 1.000000000000000000, 0.8660254037844148378, 1.000000000000023981 ) ) 
 REPRESENTATION_ITEM ( '' )  );
#5992 = CARTESIAN_POINT ( 'NONE',  ( 10.00000000000000000, 5.773502691896255534, -174.3750000000000000 ) ) ;
#5993 = CARTESIAN_POINT ( 'NONE',  ( 9.999999999999998224, 0.000000000000000000, -116.3750000040967905 ) ) ;
#5995 = ORIENTED_EDGE ( 'NONE', *, *, #33288, .T. ) ;
#5994 = CARTESIAN_POINT ( 'NONE',  ( 5.405949406249999534, 9.363379034771803333, -104.7812500020483810 ) ) ;
#5996 = DIRECTION ( 'NONE',  ( 1.000000000000000000, 0.000000000000000000, 0.000000000000000000 ) ) ;
#5997 = ORIENTED_EDGE ( 'NONE', *, *, #6781, .F. ) ;
#5998 = VERTEX_POINT ( 'NONE', #22617 ) ;
#5999 = CARTESIAN_POINT ( 'NONE',  ( -5.405949406250003975, -9.363379034771801557, -26.03125000204836681 ) ) ;
#6000 = LOCAL_TIME ( 11, 57, 6.000000000000000000, #3613 ) ;
#6001 = COORDINATED_UNIVERSAL_TIME_OFFSET ( 6, 0, .AHEAD. ) ;
#6002 = CARTESIAN_POINT ( 'NONE',  ( 10.81189881249999551, -6.242252689847874514, -79.46875000204838102 ) ) ;
#6003 = FACE_OUTER_BOUND ( 'NONE', #37784, .T. ) ;
#6004 = CARTESIAN_POINT ( 'NONE',  ( 0.000000000000000000, 0.000000000000000000, -200.0000000000000000 ) ) ;
#6005 = CARTESIAN_POINT ( 'NONE',  ( -9.999999999999227285, -5.773502691896698735, -127.5000000040967763 ) ) ;
#6006 = CARTESIAN_POINT ( 'NONE',  ( 7.070501591499376803E-16, 11.54700538379251284, -129.1250000000000000 ) ) ;
#6007 = CARTESIAN_POINT ( 'NONE',  ( 10.81189881249999907, 6.242252689847868297, -157.4062500020483810 ) ) ;
#6008 = CARTESIAN_POINT ( 'NONE',  ( 9.999999999999998224, 0.000000000000000000, -12.87500000409674783 ) ) ;
#6009 = CYLINDRICAL_SURFACE ( 'NONE', #18442, 9.999999999999998224 ) ;
#6010 = CARTESIAN_POINT ( 'NONE',  ( 10.81189881249999907, 6.242252689847868297, -130.2187500020483810 ) ) ;
#6011 = CARTESIAN_POINT ( 'NONE',  ( 5.405949406249992428, -9.363379034771808662, -100.7812500020483952 ) ) ;
#6012 = CARTESIAN_POINT ( 'NONE',  ( 7.644554776091147741E-16, 12.48450537969573659, -116.4687500020483668 ) ) ;
#6013 = CARTESIAN_POINT ( 'NONE',  ( 10.81189881249999907, 6.242252689847868297, -76.21875000204836681 ) ) ;
#6014 = CARTESIAN_POINT ( 'NONE',  ( 10.81189881249999551, -6.242252689847874514, -87.15625000204838102 ) ) ;
#6015 = CARTESIAN_POINT ( 'NONE',  ( -9.999999999999998224, 1.224646799147353059E-15, -168.1250000040967905 ) ) ;
#6016 = CARTESIAN_POINT ( 'NONE',  ( -9.999999999999227285, -5.773502691896698735, -133.5000000040967620 ) ) ;
#6017 = CARTESIAN_POINT ( 'NONE',  ( 5.405949406249992428, -9.363379034771808662, -168.2812500020484094 ) ) ;
#6018 = CARTESIAN_POINT ( 'NONE',  ( 10.81189881249999551, -6.242252689847874514, -178.6562500020484094 ) ) ;
#6019 = CARTESIAN_POINT ( 'NONE',  ( 10.81189881249999729, 6.242252689847867408, -47.71875000204837391 ) ) ;
#6020 = CARTESIAN_POINT ( 'NONE',  ( -9.999999999999998224, 1.224646799147353059E-15, -154.6250000040967905 ) ) ;
#6021 = CARTESIAN_POINT ( 'NONE',  ( -2.293366432827344421E-15, -12.48450537969573659, -0.4062500020483658103 ) ) ;
#6022 = CARTESIAN_POINT ( 'NONE',  ( -10.81189881249999729, 6.242252689847871849, -6.718750002048357040 ) ) ;
#6023 = CARTESIAN_POINT ( 'NONE',  ( 9.999999999999998224, 0.000000000000000000, -87.49999999999998579 ) ) ;
#6024 = CARTESIAN_POINT ( 'NONE',  ( 10.81189881249999907, 6.242252689847868297, -110.7187500020483810 ) ) ;
#6025 = CARTESIAN_POINT ( 'NONE',  ( -10.00000000000000000, -5.773502691896251982, -91.12499999999998579 ) ) ;
#6026 = CARTESIAN_POINT ( 'NONE',  ( 5.405949406249992428, -9.363379034771808662, -10.78125000204835438 ) ) ;
#6027 = CARTESIAN_POINT ( 'NONE',  ( 4.999999999999992006, -8.660254037844389075, -94.12500000409677625 ) ) ;
#6028 = CARTESIAN_POINT ( 'NONE',  ( 9.999999999999479527, 5.773502691896553074, -150.7500000040967336 ) ) ;
#6029 = CARTESIAN_POINT ( 'NONE',  ( 10.81189881249999551, -6.242252689847874514, -108.1562500020483810 ) ) ;
#6030 = CARTESIAN_POINT ( 'NONE',  ( 10.81189881249999729, 0.000000000000000000, -94.53125000204838102 ) ) ;
#6031 = ORIENTED_EDGE ( 'NONE', *, *, #39381, .F. ) ;
#6032 = CARTESIAN_POINT ( 'NONE',  ( -9.999999999999998224, 5.773502691896259087, -93.25000000409677625 ) ) ;
#6033 = DIRECTION ( 'NONE',  ( -1.000000000000000000, 0.000000000000000000, 0.000000000000000000 ) ) ;
#6034 = CARTESIAN_POINT ( 'NONE',  ( 7.644554776091147741E-16, 12.48450537969573659, -42.96875000204835970 ) ) ;
#6035 = ORIENTED_EDGE ( 'NONE', *, *, #34843, .T. ) ;
#6036 = CARTESIAN_POINT ( 'NONE',  ( 9.999999999999996447, -5.773502691896262640, -18.62499999999997868 ) ) ;
#6037 = CARTESIAN_POINT ( 'NONE',  ( 10.81189881249999551, -6.242252689847874514, -22.65625000204837391 ) ) ;
#6038 = CARTESIAN_POINT ( 'NONE',  ( -9.999999999999998224, 5.773502691896259087, -157.3749999999999716 ) ) ;
#6039 = CARTESIAN_POINT ( 'NONE',  ( -10.00000000000000000, -5.773502691896251982, -19.50000000409676915 ) ) ;
#6040 = ADVANCED_FACE ( 'NONE', ( #3831 ), #42239, .T. ) ;
#6041 = CARTESIAN_POINT ( 'NONE',  ( 7.070501591499377789E-16, 11.54700538379251284, -195.1250000000000284 ) ) ;
#6043 = VERTEX_POINT ( 'NONE', #35791 ) ;
#6042 = CARTESIAN_POINT ( 'NONE',  ( 5.405949406249999534, 9.363379034771803333, -122.7812500020483952 ) ) ;
#6044 = CARTESIAN_POINT ( 'NONE',  ( -2.121150477449813534E-15, -11.54700538379251284, -12.87499999999996447 ) ) ;
#6045 = ORIENTED_EDGE ( 'NONE', *, *, #27910, .F. ) ;
#6046 = CARTESIAN_POINT ( 'NONE',  ( 10.81189881249999729, 0.000000000000000000, -54.03125000204836681 ) ) ;
#6047 = CALENDAR_DATE ( 2026, 28, 9 ) ;
#6048 = CARTESIAN_POINT ( 'NONE',  ( -5.405949406250003975, -9.363379034771801557, -100.8437500020483810 ) ) ;
#6050 = ORIENTED_EDGE ( 'NONE', *, *, #33285, .T. ) ;
#6049 = ORIENTED_EDGE ( 'NONE', *, *, #30937, .T. ) ;
#6051 = DIRECTION ( 'NONE',  ( -0.000000000000000000, -0.000000000000000000, 1.000000000000000000 ) ) ;
#6052 = CARTESIAN_POINT ( 'NONE',  ( -4.999999999999996447, 8.660254037844387298, -144.3750000040967905 ) ) ;
#6053 = CARTESIAN_POINT ( 'NONE',  ( -10.81189881249999729, 1.324075727343319199E-15, -150.5937500020483810 ) ) ;
#6054 = CARTESIAN_POINT ( 'NONE',  ( -2.293366432827344421E-15, -12.48450537969573659, -183.4062500020483810 ) ) ;
#6055 = CARTESIAN_POINT ( 'NONE',  ( 10.81189881249999729, 0.000000000000000000, 0.1562499979516351889 ) ) ;
#6056 = CARTESIAN_POINT ( 'NONE',  ( -9.999999999999998224, 1.224646799147353059E-15, -161.7500000000000000 ) ) ;
#6057 = ADVANCED_FACE ( 'NONE', ( #29304 ), #12664, .T. ) ;
#6058 = CARTESIAN_POINT ( 'NONE',  ( 7.644554776091147741E-16, 12.48450537969573659, -137.4687500020483810 ) ) ;
#6059 = CARTESIAN_POINT ( 'NONE',  ( 5.405949406249999534, 9.363379034771803333, -104.5937500020483810 ) ) ;
#6060 = CARTESIAN_POINT ( 'NONE',  ( 4.999999999999992006, -8.660254037844389075, -147.7500000000000000 ) ) ;
#6061 = CARTESIAN_POINT ( 'NONE',  ( 10.81189881249999907, 6.242252689847868297, -109.4062500020483952 ) ) ;
#6062 = CARTESIAN_POINT ( 'NONE',  ( -9.999999999999998224, 5.773502691896259087, -192.2500000040968189 ) ) ;
#6063 = CARTESIAN_POINT ( 'NONE',  ( -2.293366432827344421E-15, -12.48450537969573659, -121.7187500020483952 ) ) ;
#6064 = CARTESIAN_POINT ( 'NONE',  ( 7.644554776091147741E-16, 12.48450537969573659, -190.1562500020483810 ) ) ;
#6065 = EDGE_CURVE ( 'NONE', #32933, #16776, #12966, .T. ) ;
#6066 = CARTESIAN_POINT ( 'NONE',  ( 9.999999999999479527, 5.773502691896553074, -149.2500000040967905 ) ) ;
#6067 = CARTESIAN_POINT ( 'NONE',  ( 9.999999999999998224, 0.000000000000000000, -135.5000000000000000 ) ) ;
#6068 = CARTESIAN_POINT ( 'NONE',  ( -5.000000000000003553, -8.660254037844383745, -8.499999999999952038 ) ) ;
#6069 = CARTESIAN_POINT ( 'NONE',  ( -10.81189881249999729, -6.242252689847864744, -70.96875000204839523 ) ) ;
#6070 = CARTESIAN_POINT ( 'NONE',  ( -5.405949406249996869, 9.363379034771805109, -47.34375000204838102 ) ) ;
#6071 =( REPRESENTATION_RELATIONSHIP ('NONE','NONE', #21658, #31964 ) REPRESENTATION_RELATIONSHIP_WITH_TRANSFORMATION ( #42231 )SHAPE_REPRESENTATION_RELATIONSHIP( ) );
#6072 = CARTESIAN_POINT ( 'NONE',  ( 4.999999999999992006, -8.660254037844389075, -178.1250000040968189 ) ) ;
#6073 = CARTESIAN_POINT ( 'NONE',  ( -5.405949406249996869, 9.363379034771805109, -28.03125000204837036 ) ) ;
#6074 = VECTOR ( 'NONE', #10804, 1000.000000000000000 ) ;
#6075 = CARTESIAN_POINT ( 'NONE',  ( -5.405949406250003975, -9.363379034771801557, -25.84375000204835970 ) ) ;
#6076 = CARTESIAN_POINT ( 'NONE',  ( 9.999999999999998224, 0.000000000000000000, -117.5000000000000000 ) ) ;
#6077 = CARTESIAN_POINT ( 'NONE',  ( -10.81189881249999907, -6.242252689847864744, -139.9687500020483810 ) ) ;
#6078 = CARTESIAN_POINT ( 'NONE',  ( -10.00000000000000000, -5.773502691896251982, -116.6249999999999858 ) ) ;
#6079 = AXIS2_PLACEMENT_3D ( 'NONE', #38693, #11926, #8495 ) ;
#6080 =( BOUNDED_CURVE ( )  B_SPLINE_CURVE ( 2, ( #9793, #19925, #33539, #39353, #16674, #12804, #6559 ),
 .UNSPECIFIED., .F., .F. ) 
 B_SPLINE_CURVE_WITH_KNOTS ( ( 3, 2, 2, 3 ),
 ( 0.04477611940298512061, 0.04601990049751248507, 0.04726368159203984259, 0.04850746268656720706 ),
 .UNSPECIFIED. ) 
 CURVE ( )  GEOMETRIC_REPRESENTATION_ITEM ( )  RATIONAL_B_SPLINE_CURVE ( ( 0.9999999999999947820, 0.8660254037844439257, 1.000000000000000000, 0.8660254037844387076, 1.000000000000000000, 0.8660254037844342667, 1.000000000000004441 ) ) 
 REPRESENTATION_ITEM ( '' )  );
#6081 = CARTESIAN_POINT ( 'NONE',  ( -4.999999999999996447, 8.660254037844387298, -67.49999999999997158 ) ) ;
#6082 = CARTESIAN_POINT ( 'NONE',  ( -10.81189881249999907, -6.242252689847864744, -143.1562500020484094 ) ) ;
#6083 = CARTESIAN_POINT ( 'NONE',  ( 5.405949406249999534, 9.363379034771803333, -116.7812500020483952 ) ) ;
#6084 = ORIENTED_EDGE ( 'NONE', *, *, #24740, .F. ) ;
#6085 = CARTESIAN_POINT ( 'NONE',  ( 7.070501591499376803E-16, 11.54700538379251284, -197.0000000040968189 ) ) ;
#6086 = CARTESIAN_POINT ( 'NONE',  ( 10.00000000000000000, 5.773502691896255534, -119.2500000040967905 ) ) ;
#6087 = CARTESIAN_POINT ( 'NONE',  ( -2.121150477449813534E-15, -11.54700538379251284, -38.75000000409676204 ) ) ;
#6088 = CARTESIAN_POINT ( 'NONE',  ( 7.644554776091147741E-16, 12.48450537969573659, -72.96875000204835260 ) ) ;
#6089 = CARTESIAN_POINT ( 'NONE',  ( 9.999999999999998224, 0.000000000000000000, -43.99999999999998579 ) ) ;
#6090 = CARTESIAN_POINT ( 'NONE',  ( -9.999999999999998224, 1.224646799147353059E-15, -25.62500000409675849 ) ) ;
#6091 = CARTESIAN_POINT ( 'NONE',  ( 5.405949406249992428, -9.363379034771808662, -42.28125000204838102 ) ) ;
#6092 = CYLINDRICAL_SURFACE ( 'NONE', #5616, 10.00000000000000178 ) ;
#6093 = CARTESIAN_POINT ( 'NONE',  ( -9.999999999999998224, 5.773502691896259087, -46.75000000409676915 ) ) ;
#6094 = CARTESIAN_POINT ( 'NONE',  ( 10.81189881249999729, 0.000000000000000000, -33.03125000204837391 ) ) ;
#6095 = DIRECTION ( 'NONE',  ( -0.000000000000000000, -0.000000000000000000, -1.000000000000000000 ) ) ;
#6096 = CARTESIAN_POINT ( 'NONE',  ( -10.81189881249999907, -6.242252689847864744, -140.1562500020484094 ) ) ;
#6097 = CARTESIAN_POINT ( 'NONE',  ( -5.405949406250003975, -9.363379034771801557, -149.0312500020483810 ) ) ;
#6099 = EDGE_CURVE ( 'NONE', #6043, #15363, #29258, .T. ) ;
#6098 = CARTESIAN_POINT ( 'NONE',  ( -4.999999999999996447, 8.660254037844387298, -190.5000000000000000 ) ) ;
#6100 = DIRECTION ( 'NONE',  ( 0.000000000000000000, 0.000000000000000000, 1.000000000000000000 ) ) ;
#6101 = ORIENTED_EDGE ( 'NONE', *, *, #26161, .F. ) ;
#6102 = VERTEX_POINT ( 'NONE', #3194 ) ;
#6103 = ORIENTED_EDGE ( 'NONE', *, *, #1721, .F. ) ;
#6104 = LINE ( 'NONE', #2654, #20785 ) ;
#6105 = CARTESIAN_POINT ( 'NONE',  ( -10.81189881249999907, -6.242252689847864744, -172.9687500020484094 ) ) ;
#6106 = CARTESIAN_POINT ( 'NONE',  ( 7.644554776091147741E-16, 12.48450537969573659, -30.96875000204835260 ) ) ;
#6107 = CARTESIAN_POINT ( 'NONE',  ( -2.293366432827344421E-15, -12.48450537969573659, -163.7187500020483810 ) ) ;
#6108 = CARTESIAN_POINT ( 'NONE',  ( 10.81189881249999729, 0.000000000000000000, -146.8437500020483810 ) ) ;
#6109 = FACE_OUTER_BOUND ( 'NONE', #7357, .T. ) ;
#6110 = CARTESIAN_POINT ( 'NONE',  ( -10.81189881249999729, 1.324075727343319199E-15, -128.0937500020483810 ) ) ;
#6111 = CARTESIAN_POINT ( 'NONE',  ( -10.81189881249999907, -6.242252689847864744, -131.1562500020483810 ) ) ;
#6112 = CARTESIAN_POINT ( 'NONE',  ( -2.293366432827344421E-15, -12.48450537969573659, -18.21875000204837036 ) ) ;
#6113 = CARTESIAN_POINT ( 'NONE',  ( -5.405949406249996869, 9.363379034771805109, -147.8437500020483810 ) ) ;
#6114 = LINE ( 'NONE', #39961, #12282 ) ;
#6115 =( BOUNDED_CURVE ( )  B_SPLINE_CURVE ( 2, ( #34015, #10898, #40666, #21043, #21261, #40882, #3805 ),
 .UNSPECIFIED., .F., .F. ) 
 B_SPLINE_CURVE_WITH_KNOTS ( ( 3, 2, 2, 3 ),
 ( 0.4104477611940299253, 0.4116915422885572551, 0.4129353233830846959, 0.4141791044776120256 ),
 .UNSPECIFIED. ) 
 CURVE ( )  GEOMETRIC_REPRESENTATION_ITEM ( )  RATIONAL_B_SPLINE_CURVE ( ( 0.9999999999999940048, 0.8660254037844447028, 1.000000000000000000, 0.8660254037844387076, 1.000000000000000000, 0.8660254037844267172, 1.000000000000011990 ) ) 
 REPRESENTATION_ITEM ( '' )  );
#6116 = CARTESIAN_POINT ( 'NONE',  ( -9.999999999999998224, 1.224646799147353059E-15, -119.7500000000000000 ) ) ;
#6117 = CARTESIAN_POINT ( 'NONE',  ( -5.000000000000003553, -8.660254037844383745, -166.0000000000000000 ) ) ;
#6118 = CARTESIAN_POINT ( 'NONE',  ( 5.405949406249992428, -9.363379034771808662, -73.59375000204838102 ) ) ;
#6119 = CARTESIAN_POINT ( 'NONE',  ( 10.81189881249999907, 6.242252689847868297, -47.90625000204836681 ) ) ;
#6120 = CARTESIAN_POINT ( 'NONE',  ( 7.644554776091147741E-16, 12.48450537969573659, -63.96875000204837391 ) ) ;
#6121 = CARTESIAN_POINT ( 'NONE',  ( -2.121150477449813534E-15, -11.54700538379251284, -174.8750000000000000 ) ) ;
#6122 = CARTESIAN_POINT ( 'NONE',  ( 7.644554776091147741E-16, 12.48450537969573659, -171.9687500020483810 ) ) ;
#6123 = CARTESIAN_POINT ( 'NONE',  ( 9.999999999999998224, 0.000000000000000000, -141.5000000000000000 ) ) ;
#6124 = CARTESIAN_POINT ( 'NONE',  ( 10.81189881249999729, 6.242252689847867408, -149.9062500020484094 ) ) ;
#6125 = DIRECTION ( 'NONE',  ( -0.000000000000000000, -0.000000000000000000, -1.000000000000000000 ) ) ;
#6126 = CARTESIAN_POINT ( 'NONE',  ( -4.999999999999996447, 8.660254037844387298, -123.3750000040967905 ) ) ;
#6127 = CARTESIAN_POINT ( 'NONE',  ( 5.000000000000000000, 8.660254037844385522, -94.74999999999998579 ) ) ;
#6128 = EDGE_LOOP ( 'NONE', ( #7801, #4234, #34167, #15316 ) ) ;
#6129 =( BOUNDED_CURVE ( )  B_SPLINE_CURVE ( 2, ( #39477, #17221, #16362 ),
 .UNSPECIFIED., .F., .T. ) 
 B_SPLINE_CURVE_WITH_KNOTS ( ( 3, 3 ),
 ( 0.9894244345683576025, 0.9894279716579621464 ),
 .UNSPECIFIED. ) 
 CURVE ( )  GEOMETRIC_REPRESENTATION_ITEM ( )  RATIONAL_B_SPLINE_CURVE ( ( 0.9330147350531647898, 0.9330126360445730738, 0.9330127040248163972 ) ) 
 REPRESENTATION_ITEM ( '' )  );
#6130 = CARTESIAN_POINT ( 'NONE',  ( -2.293366432827344421E-15, -12.48450537969573659, -120.4062500020483952 ) ) ;
#6131 = CARTESIAN_POINT ( 'NONE',  ( 7.070501591499377789E-16, 11.54700538379251284, -143.0000000040967905 ) ) ;
#6132 = CARTESIAN_POINT ( 'NONE',  ( 9.999999999999998224, 0.000000000000000000, -152.0000000000000000 ) ) ;
#6133 = CARTESIAN_POINT ( 'NONE',  ( -10.81189881249999729, 1.324075727343319199E-15, -168.7812500020484094 ) ) ;
#6134 = CARTESIAN_POINT ( 'NONE',  ( -9.999999999999998224, 1.224646799147353059E-15, -48.12500000409677625 ) ) ;
#6135 = VECTOR ( 'NONE', #26712, 1000.000000000000000 ) ;
#6136 = DIRECTION ( 'NONE',  ( -1.000000000000000000, 0.000000000000000000, 0.000000000000000000 ) ) ;
#6137 = CARTESIAN_POINT ( 'NONE',  ( 10.81189881249999551, -6.242252689847874514, -58.65625000204838813 ) ) ;
#6138 = CARTESIAN_POINT ( 'NONE',  ( 11.54700538379250396, 20.00000000000000711, 49.99999999999998579 ) ) ;
#6139 = CARTESIAN_POINT ( 'NONE',  ( 10.81189881249999729, 0.000000000000000000, -163.5312500020484094 ) ) ;
#6140 = CIRCLE ( 'NONE', #13709, 9.999999999999998224 ) ;
#6141 = CARTESIAN_POINT ( 'NONE',  ( 5.405949406249992428, -9.363379034771808662, -144.0937500020483810 ) ) ;
#6142 = DIRECTION ( 'NONE',  ( -0.000000000000000000, -0.000000000000000000, 1.000000000000000000 ) ) ;
#6144 = EDGE_CURVE ( 'NONE', #19099, #1402, #6223, .T. ) ;
#6143 = CARTESIAN_POINT ( 'NONE',  ( 9.999999999999998224, 0.000000000000000000, -64.99999999999997158 ) ) ;
#6145 = ORIENTED_EDGE ( 'NONE', *, *, #40683, .F. ) ;
#6146 = EDGE_CURVE ( 'NONE', #5178, #13534, #41079, .T. ) ;
#6147 = CARTESIAN_POINT ( 'NONE',  ( -5.000000000000003553, -8.660254037844383745, -52.37500000409675494 ) ) ;
#6148 = VECTOR ( 'NONE', #2459, 1000.000000000000000 ) ;
#6150 = ORIENTED_EDGE ( 'NONE', *, *, #598, .T. ) ;
#6149 = CARTESIAN_POINT ( 'NONE',  ( 7.644554776091147741E-16, 12.48450537969573659, -71.65625000204836681 ) ) ;
#6152 = ORIENTED_EDGE ( 'NONE', *, *, #32185, .T. ) ;
#6151 = CARTESIAN_POINT ( 'NONE',  ( -9.999999999999479527, -5.773502691896549521, -143.6250000000000000 ) ) ;
#6153 = ORIENTED_EDGE ( 'NONE', *, *, #21972, .F. ) ;
#6154 = CARTESIAN_POINT ( 'NONE',  ( 10.81189881249999729, 0.000000000000000000, -28.34375000204836326 ) ) ;
#6155 = CARTESIAN_POINT ( 'NONE',  ( -10.00000000000076916, 5.773502691895813221, -107.8749999999999574 ) ) ;
#6156 = CARTESIAN_POINT ( 'NONE',  ( 7.644554776091147741E-16, 12.48450537969573659, -8.656250002048372139 ) ) ;
#6157 = CARTESIAN_POINT ( 'NONE',  ( 5.405949406249992428, -9.363379034771808662, -54.09375000204835970 ) ) ;
#6158 = CARTESIAN_POINT ( 'NONE',  ( 9.999999999999998224, 0.000000000000000000, -71.37500000409677625 ) ) ;
#6159 = CARTESIAN_POINT ( 'NONE',  ( 4.999999999999992006, -8.660254037844389075, -30.74999999999997158 ) ) ;
#6160 = EDGE_CURVE ( 'NONE', #40301, #35906, #17383, .T. ) ;
#6161 = CARTESIAN_POINT ( 'NONE',  ( 10.81189881249999729, 6.242252689847867408, -188.7187500020484094 ) ) ;
#6162 = CARTESIAN_POINT ( 'NONE',  ( 10.81189881249999907, 6.242252689847868297, -169.2187500020483810 ) ) ;
#6163 = CARTESIAN_POINT ( 'NONE',  ( 10.81189881249999729, 0.000000000000000000, -155.8437500020483810 ) ) ;
#6164 = CARTESIAN_POINT ( 'NONE',  ( 10.81189881249999729, 6.242252689847867408, -172.2187500020483810 ) ) ;
#6165 = DIRECTION ( 'NONE',  ( -1.000000000000000000, 0.000000000000000000, 0.000000000000000000 ) ) ;
#6166 = CARTESIAN_POINT ( 'NONE',  ( -9.999999999999998224, 1.224646799147353059E-15, -162.1250000040967905 ) ) ;
#6167 = CARTESIAN_POINT ( 'NONE',  ( 9.999999999999998224, 0.000000000000000000, -189.5000000000000000 ) ) ;
#6168 = CARTESIAN_POINT ( 'NONE',  ( -5.405949406249996869, 9.363379034771805109, -108.8437500020483810 ) ) ;
#6169 = CARTESIAN_POINT ( 'NONE',  ( -5.000000000000003553, -8.660254037844383745, -72.99999999999998579 ) ) ;
#6170 = CARTESIAN_POINT ( 'NONE',  ( -10.81189881249999907, -6.242252689847864744, -72.65625000204836681 ) ) ;
#6171 = CARTESIAN_POINT ( 'NONE',  ( 7.070501591499376803E-16, 11.54700538379251284, -96.50000000409677625 ) ) ;
#6172 = CARTESIAN_POINT ( 'NONE',  ( -5.405949406250003975, -9.363379034771801557, -87.34375000204836681 ) ) ;
#6173 = EDGE_CURVE ( 'NONE', #9851, #8327, #35073, .T. ) ;
#6174 = CARTESIAN_POINT ( 'NONE',  ( -10.81189881249999729, 1.324075727343319199E-15, -63.78125000204837391 ) ) ;
#6175 = CARTESIAN_POINT ( 'NONE',  ( -9.999999999999998224, 5.773502691896259087, -144.2500000040967905 ) ) ;
#6176 = CARTESIAN_POINT ( 'NONE',  ( -9.999999999999998224, 5.773502691896259087, -116.8750000000000000 ) ) ;
#6177 = ORIENTED_EDGE ( 'NONE', *, *, #14835, .T. ) ;
#6178 = VECTOR ( 'NONE', #4830, 1000.000000000000000 ) ;
#6179 = CARTESIAN_POINT ( 'NONE',  ( 5.405949406249999534, 9.363379034771803333, -145.2812500020483810 ) ) ;
#6180 = CARTESIAN_POINT ( 'NONE',  ( -10.81189881249999729, 6.242252689847871849, -156.9062500020483810 ) ) ;
#6181 = CARTESIAN_POINT ( 'NONE',  ( 5.405949406249999534, 9.363379034771803333, -193.2812500020484094 ) ) ;
#6182 = DIRECTION ( 'NONE',  ( 1.000000000000000000, 0.000000000000000000, 0.000000000000000000 ) ) ;
#6183 = CARTESIAN_POINT ( 'NONE',  ( 7.644554776091147741E-16, 12.48450537969573659, -87.96875000204838102 ) ) ;
#6184 = ORIENTED_EDGE ( 'NONE', *, *, #40441, .T. ) ;
#6185 = CARTESIAN_POINT ( 'NONE',  ( -5.000000000000003553, -8.660254037844383745, -60.99999999999997158 ) ) ;
#6186 = CARTESIAN_POINT ( 'NONE',  ( 5.405949406249999534, 9.363379034771803333, -191.5937500020484094 ) ) ;
#6187 = CARTESIAN_POINT ( 'NONE',  ( -4.999999999999996447, 8.660254037844387298, -75.37500000409677625 ) ) ;
#6188 = CARTESIAN_POINT ( 'NONE',  ( 5.000000000000000000, 8.660254037844385522, -66.24999999999997158 ) ) ;
#6189 = CARTESIAN_POINT ( 'NONE',  ( 5.000000000000000000, 8.660254037844385522, -140.1250000040967905 ) ) ;
#6190 = CARTESIAN_POINT ( 'NONE',  ( -2.293366432827344421E-15, -12.48450537969573659, -84.40625000204838102 ) ) ;
#6191 = CARTESIAN_POINT ( 'NONE',  ( 10.81189881249999729, 0.000000000000000000, -67.53125000204838102 ) ) ;
#6192 = CARTESIAN_POINT ( 'NONE',  ( 7.070501591499377789E-16, 11.54700538379251284, -62.00000000409678336 ) ) ;
#6193 = CARTESIAN_POINT ( 'NONE',  ( 10.81189881249999729, 0.000000000000000000, -19.34375000204835260 ) ) ;
#6194 = ORIENTED_EDGE ( 'NONE', *, *, #33703, .F. ) ;
#6195 = CARTESIAN_POINT ( 'NONE',  ( -5.405949406250003975, -9.363379034771801557, -192.5312500020484094 ) ) ;
#6196 = CARTESIAN_POINT ( 'NONE',  ( 7.644554776091147741E-16, 12.48450537969573659, -14.65625000204837214 ) ) ;
#6197 = CARTESIAN_POINT ( 'NONE',  ( -10.81189881249999729, -6.242252689847864744, -6.468750002048346381 ) ) ;
#6198 = CARTESIAN_POINT ( 'NONE',  ( -9.999999999999998224, 1.224646799147353059E-15, -160.2500000000000000 ) ) ;
#6199 =( BOUNDED_CURVE ( )  B_SPLINE_CURVE ( 2, ( #4052, #24133, #16984, #27142, #23491, #4477, #37274 ),
 .UNSPECIFIED., .F., .F. ) 
 B_SPLINE_CURVE_WITH_KNOTS ( ( 3, 2, 2, 3 ),
 ( 0.5111940298507463565, 0.5124378109452737418, 0.5136815920398011270, 0.5149253731343285123 ),
 .UNSPECIFIED. ) 
 CURVE ( )  GEOMETRIC_REPRESENTATION_ITEM ( )  RATIONAL_B_SPLINE_CURVE ( ( 0.9999999999999880096, 0.8660254037844506980, 1.000000000000000000, 0.8660254037844387076, 1.000000000000000000, 0.8660254037844267172, 1.000000000000011990 ) ) 
 REPRESENTATION_ITEM ( '' )  );
#6200 = FACE_OUTER_BOUND ( 'NONE', #36762, .T. ) ;
#6201 = FACE_OUTER_BOUND ( 'NONE', #25952, .T. ) ;
#6202 = ADVANCED_FACE ( 'NONE', ( #9868 ), #29735, .T. ) ;
#6203 = CARTESIAN_POINT ( 'NONE',  ( -4.999999999999996447, 8.660254037844387298, -171.0000000000000000 ) ) ;
#6204 = CARTESIAN_POINT ( 'NONE',  ( 9.999999999998969713, 5.773502691896851502, -1.874999999999918954 ) ) ;
#6205 = VECTOR ( 'NONE', #32948, 1000.000000000000000 ) ;
#6206 = ADVANCED_FACE ( 'NONE', ( #21065 ), #14358, .T. ) ;
#6208 = ORIENTED_EDGE ( 'NONE', *, *, #9328, .F. ) ;
#6207 = CARTESIAN_POINT ( 'NONE',  ( 10.81189881249999729, 0.000000000000000000, -97.53125000204839523 ) ) ;
#6209 = CARTESIAN_POINT ( 'NONE',  ( -9.999999999999998224, 1.224646799147353059E-15, -169.6250000040967905 ) ) ;
#6210 = VERTEX_POINT ( 'NONE', #4669 ) ;
#6211 = EDGE_LOOP ( 'NONE', ( #7741, #33440, #25469, #31095 ) ) ;
#6212 = CARTESIAN_POINT ( 'NONE',  ( -10.81189881249999729, 1.324075727343319199E-15, -32.09375000204836681 ) ) ;
#6213 = CARTESIAN_POINT ( 'NONE',  ( -10.81189881249999729, 6.242252689847871849, -33.90625000204836681 ) ) ;
#6214 = CALENDAR_DATE ( 2026, 28, 9 ) ;
#6215 = CARTESIAN_POINT ( 'NONE',  ( 10.81189881249999729, 0.000000000000000000, -79.34375000204838102 ) ) ;
#6216 = DIRECTION ( 'NONE',  ( 1.000000000000000000, 0.000000000000000000, 0.000000000000000000 ) ) ;
#6217 = CARTESIAN_POINT ( 'NONE',  ( 10.25440575037869273, 0.6849317685095945851, -100.0000000000000142 ) ) ;
#6218 = EDGE_CURVE ( 'NONE', #29288, #19092, #40690, .T. ) ;
#6219 = CYLINDRICAL_SURFACE ( 'NONE', #15688, 9.999999999999998224 ) ;
#6220 = CARTESIAN_POINT ( 'NONE',  ( -11.54700538379250396, -20.00000000000000355, 45.00000000000009237 ) ) ;
#6221 = CARTESIAN_POINT ( 'NONE',  ( -10.81189881249999907, -6.242252689847864744, -155.1562500020484094 ) ) ;
#6222 = CARTESIAN_POINT ( 'NONE',  ( 9.999999999999998224, 0.000000000000000000, -8.375000004096744277 ) ) ;
#6223 = LINE ( 'NONE', #13510, #21210 ) ;
#6224 = CARTESIAN_POINT ( 'NONE',  ( 5.405949406249992428, -9.363379034771808662, -127.5937500020483668 ) ) ;
#6225 = CARTESIAN_POINT ( 'NONE',  ( -2.293366432827344421E-15, -12.48450537969573659, -99.40625000204839523 ) ) ;
#6226 = CARTESIAN_POINT ( 'NONE',  ( 10.81189881249999729, 0.000000000000000000, -110.8437500020483810 ) ) ;
#6227 = CARTESIAN_POINT ( 'NONE',  ( -5.405949406249996869, 9.363379034771805109, -80.34375000204838102 ) ) ;
#6228 = CARTESIAN_POINT ( 'NONE',  ( -10.81189881249999729, 6.242252689847871849, -87.90625000204838102 ) ) ;
#6229 = CARTESIAN_POINT ( 'NONE',  ( 9.999999999999998224, 0.000000000000000000, -171.8750000040968189 ) ) ;
#6230 = CARTESIAN_POINT ( 'NONE',  ( -5.000000000000003553, -8.660254037844383745, -133.3750000040967905 ) ) ;
#6231 = CARTESIAN_POINT ( 'NONE',  ( -10.81189881249999729, -6.242252689847864744, -165.6562500020483810 ) ) ;
#6232 = CARTESIAN_POINT ( 'NONE',  ( -10.81189881249999907, -6.242252689847864744, -179.1562500020484094 ) ) ;
#6233 = AXIS2_PLACEMENT_3D ( 'NONE', #14338, #8110, #11325 ) ;
#6234 = CARTESIAN_POINT ( 'NONE',  ( 5.000000000000000000, 8.660254037844385522, -156.6250000040967905 ) ) ;
#6235 = DIRECTION ( 'NONE',  ( -0.000000000000000000, -0.000000000000000000, 1.000000000000000000 ) ) ;
#6236 = CARTESIAN_POINT ( 'NONE',  ( 10.81189881249999551, -6.242252689847874514, -8.968750002048359704 ) ) ;
#6237 = CARTESIAN_POINT ( 'NONE',  ( -10.00000000000102496, 5.773502691895664007, -5.874999999999936939 ) ) ;
#6238 = CARTESIAN_POINT ( 'NONE',  ( 5.405949406249999534, 9.363379034771803333, -112.0937500020483810 ) ) ;
#6239 = CARTESIAN_POINT ( 'NONE',  ( 5.000000000000000000, 8.660254037844385522, -93.24999999999998579 ) ) ;
#6240 = CARTESIAN_POINT ( 'NONE',  ( -10.81189881249999729, 1.324075727343319199E-15, -14.28125000204835615 ) ) ;
#6241 = CARTESIAN_POINT ( 'NONE',  ( 4.999999999999992006, -8.660254037844389075, -97.12500000409677625 ) ) ;
#6242 = DIRECTION ( 'NONE',  ( -0.000000000000000000, -0.000000000000000000, 1.000000000000000000 ) ) ;
#6243 = CARTESIAN_POINT ( 'NONE',  ( -10.81189881249999907, -6.242252689847864744, -108.6562500020483952 ) ) ;
#6244 = CARTESIAN_POINT ( 'NONE',  ( -10.81189881249999729, 1.324075727343319199E-15, -92.28125000204838102 ) ) ;
#6245 = ORIENTED_EDGE ( 'NONE', *, *, #24624, .T. ) ;
#6246 =( BOUNDED_CURVE ( )  B_SPLINE_CURVE ( 2, ( #18104, #41405, #28268, #24399, #41620, #14426, #12054 ),
 .UNSPECIFIED., .F., .F. ) 
 B_SPLINE_CURVE_WITH_KNOTS ( ( 3, 2, 2, 3 ),
 ( 0.1977611940298507898, 0.1990049751243781750, 0.2002487562189055326, 0.2014925373134328901 ),
 .UNSPECIFIED. ) 
 CURVE ( )  GEOMETRIC_REPRESENTATION_ITEM ( )  RATIONAL_B_SPLINE_CURVE ( ( 0.9999999999999940048, 0.8660254037844447028, 1.000000000000000000, 0.8660254037844387076, 1.000000000000000000, 0.8660254037844327124, 1.000000000000005995 ) ) 
 REPRESENTATION_ITEM ( '' )  );
#6247 = CARTESIAN_POINT ( 'NONE',  ( 4.999999999999992006, -8.660254037844389075, -82.12500000409676204 ) ) ;
#6248 = CARTESIAN_POINT ( 'NONE',  ( 9.999999999999998224, 0.000000000000000000, -72.49999999999998579 ) ) ;
#6249 = CARTESIAN_POINT ( 'NONE',  ( 7.644554776091147741E-16, 12.48450537969573659, -41.46875000204835970 ) ) ;
#6250 = ORIENTED_EDGE ( 'NONE', *, *, #36218, .T. ) ;
#6251 = CARTESIAN_POINT ( 'NONE',  ( -4.999999999999996447, 8.660254037844387298, -20.99999999999996447 ) ) ;
#6252 = CARTESIAN_POINT ( 'NONE',  ( -2.121150477449813534E-15, -11.54700538379251284, -153.8750000000000000 ) ) ;
#6253 = CARTESIAN_POINT ( 'NONE',  ( 7.070501591499377789E-16, 11.54700538379251284, -11.00000000409676026 ) ) ;
#6255 = ORIENTED_EDGE ( 'NONE', *, *, #37201, .F. ) ;
#6254 = CARTESIAN_POINT ( 'NONE',  ( 7.644554776091147741E-16, 12.48450537969573659, -128.6562500020483810 ) ) ;
#6256 = CARTESIAN_POINT ( 'NONE',  ( 9.999999999999998224, 0.000000000000000000, -92.37500000409677625 ) ) ;
#6257 = ORIENTED_EDGE ( 'NONE', *, *, #23342, .T. ) ;
#6258 = CARTESIAN_POINT ( 'NONE',  ( -2.293366432827344421E-15, -12.48450537969573659, -54.40625000204838102 ) ) ;
#6259 = PERSON_AND_ORGANIZATION ( #11915, #17965 ) ;
#6260 = AXIS2_PLACEMENT_3D ( 'NONE', #21154, #18561, #24423 ) ;
#6261 = EDGE_CURVE ( 'NONE', #7227, #17891, #11130, .T. ) ;
#6262 = CARTESIAN_POINT ( 'NONE',  ( 5.405949406249999534, 9.363379034771803333, -103.0937500020483810 ) ) ;
#6264 = ORIENTED_EDGE ( 'NONE', *, *, #22573, .F. ) ;
#6263 = VERTEX_POINT ( 'NONE', #20428 ) ;
#6265 = AXIS2_PLACEMENT_3D ( 'NONE', #6138, #6981, #16238 ) ;
#6266 = CARTESIAN_POINT ( 'NONE',  ( -9.999999999999998224, 1.224646799147353059E-15, -85.62500000409677625 ) ) ;
#6267 = CARTESIAN_POINT ( 'NONE',  ( 0.000000000000000000, 0.000000000000000000, -200.0000000000000000 ) ) ;
#6268 = CARTESIAN_POINT ( 'NONE',  ( -2.293366432827344421E-15, -12.48450537969573659, -177.4062500020483810 ) ) ;
#6269 = CYLINDRICAL_SURFACE ( 'NONE', #35105, 9.999999999999998224 ) ;
#6270 = CARTESIAN_POINT ( 'NONE',  ( 5.405949406249999534, 9.363379034771803333, -128.5937500020483810 ) ) ;
#6271 = CARTESIAN_POINT ( 'NONE',  ( -10.81189881249999729, 6.242252689847871849, -101.2187500020483810 ) ) ;
#6272 = DIRECTION ( 'NONE',  ( 0.000000000000000000, 0.000000000000000000, 1.000000000000000000 ) ) ;
#6273 = CARTESIAN_POINT ( 'NONE',  ( 10.81189881249999729, 0.000000000000000000, -106.5312500020483810 ) ) ;
#6274 = CARTESIAN_POINT ( 'NONE',  ( 9.999999999999998224, 0.000000000000000000, -195.8750000040967905 ) ) ;
#6276 = EDGE_CURVE ( 'NONE', #2082, #29986, #24540, .T. ) ;
#6275 = CARTESIAN_POINT ( 'NONE',  ( 7.644554776091147741E-16, 12.48450537969573659, -116.4687500020483668 ) ) ;
#6277 = CARTESIAN_POINT ( 'NONE',  ( -10.81189881249999729, 1.324075727343319199E-15, -183.7812500020484094 ) ) ;
#6278 = PLANE ( 'NONE',  #39219 ) ;
#6279 = CARTESIAN_POINT ( 'NONE',  ( -5.000000000000003553, -8.660254037844383745, -136.0000000000000000 ) ) ;
#6280 = CARTESIAN_POINT ( 'NONE',  ( -9.999999999999998224, 1.224646799147353059E-15, -4.249999999999976019 ) ) ;
#6281 = CARTESIAN_POINT ( 'NONE',  ( 7.644554776091147741E-16, 12.48450537969573659, -65.46875000204836681 ) ) ;
#6282 = CARTESIAN_POINT ( 'NONE',  ( 5.405949406249999534, 9.363379034771803333, -52.09375000204835260 ) ) ;
#6283 = DESIGN_CONTEXT ( 'detailed design', #1658, 'design' ) ;
#6284 = CARTESIAN_POINT ( 'NONE',  ( -4.999999999999996447, 8.660254037844387298, -177.3750000040967905 ) ) ;
#6285 = CARTESIAN_POINT ( 'NONE',  ( -2.293366432827344421E-15, -12.48450537969573659, -22.90625000204837747 ) ) ;
#6286 = CARTESIAN_POINT ( 'NONE',  ( -2.293366432827344421E-15, -12.48450537969573659, -30.21875000204835260 ) ) ;
#6287 = CARTESIAN_POINT ( 'NONE',  ( 4.999999999999992006, -8.660254037844389075, -107.6250000040967763 ) ) ;
#6288 = CARTESIAN_POINT ( 'NONE',  ( -2.293366432827344421E-15, -12.48450537969573659, -135.2187500020483810 ) ) ;
#6289 = CARTESIAN_POINT ( 'NONE',  ( -4.999999999999996447, 8.660254037844387298, -117.0000000000000000 ) ) ;
#6290 = CARTESIAN_POINT ( 'NONE',  ( 4.999999999999992006, -8.660254037844389075, -147.7500000000000000 ) ) ;
#6291 = CARTESIAN_POINT ( 'NONE',  ( -9.999999999999998224, 1.224646799147353059E-15, -70.24999999999998579 ) ) ;
#6292 = CARTESIAN_POINT ( 'NONE',  ( 10.81189881249999551, -6.242252689847874514, -133.6562500020483810 ) ) ;
#6293 = CARTESIAN_POINT ( 'NONE',  ( 7.644554776091147741E-16, 12.48450537969573659, -118.1562500020483952 ) ) ;
#6294 = ORIENTED_EDGE ( 'NONE', *, *, #6971, .F. ) ;
#6295 = AXIS2_PLACEMENT_3D ( 'NONE', #39092, #35241, #5878 ) ;
#6296 = CARTESIAN_POINT ( 'NONE',  ( -9.999999999999998224, 1.224646799147353059E-15, -167.7500000000000000 ) ) ;
#6297 = CARTESIAN_POINT ( 'NONE',  ( 9.999999999999998224, 0.000000000000000000, -104.3750000040967763 ) ) ;
#6298 = CARTESIAN_POINT ( 'NONE',  ( -10.81189881249999729, 1.324075727343319199E-15, -65.09375000204836681 ) ) ;
#6299 = VERTEX_POINT ( 'NONE', #30587 ) ;
#6300 = CARTESIAN_POINT ( 'NONE',  ( -2.121150477449813534E-15, -11.54700538379251284, -39.87499999999996447 ) ) ;
#6301 = CARTESIAN_POINT ( 'NONE',  ( -10.00000000000000000, -5.773502691896251982, -21.00000000409677980 ) ) ;
#6302 = CARTESIAN_POINT ( 'NONE',  ( 10.81189881249999729, 0.000000000000000000, -40.53125000204838102 ) ) ;
#6303 = CARTESIAN_POINT ( 'NONE',  ( -5.000000000000003553, -8.660254037844383745, -43.37500000409677625 ) ) ;
#6304 = CARTESIAN_POINT ( 'NONE',  ( 10.81189881249999551, -6.242252689847874514, -34.65625000204835970 ) ) ;
#6305 = CARTESIAN_POINT ( 'NONE',  ( 7.070501591499376803E-16, 11.54700538379251284, -166.6250000000000000 ) ) ;
#6306 = CARTESIAN_POINT ( 'NONE',  ( 7.644554776091147741E-16, 12.48450537969573659, -137.6562500020483810 ) ) ;
#6307 = CARTESIAN_POINT ( 'NONE',  ( 5.405949406249992428, -9.363379034771808662, -150.2812500020483810 ) ) ;
#6308 = CARTESIAN_POINT ( 'NONE',  ( -9.999999999999998224, 1.224646799147353059E-15, -110.7499999999999858 ) ) ;
#6309 = ORIENTED_EDGE ( 'NONE', *, *, #20273, .T. ) ;
#6310 = ADVANCED_FACE ( 'NONE', ( #40473 ), #31015, .T. ) ;
#6311 = ORIENTED_EDGE ( 'NONE', *, *, #39923, .T. ) ;
#6312 = EDGE_LOOP ( 'NONE', ( #7412, #31573, #14175, #27061, #25280, #34976, #37676 ) ) ;
#6313 = VECTOR ( 'NONE', #20614, 1000.000000000000000 ) ;
#6314 = CARTESIAN_POINT ( 'NONE',  ( 4.999999999999992006, -8.660254037844389075, -104.2499999999999858 ) ) ;
#6315 = CARTESIAN_POINT ( 'NONE',  ( -10.81189881249999907, -6.242252689847864744, -177.4687500020484094 ) ) ;
#6316 = CC_DESIGN_SECURITY_CLASSIFICATION ( #9061, ( #22864 ) ) ;
#6317 = CARTESIAN_POINT ( 'NONE',  ( -10.81189881249999729, 1.324075727343319199E-15, -26.09375000204835970 ) ) ;
#6318 = CARTESIAN_POINT ( 'NONE',  ( -9.999999999999998224, 1.224646799147353059E-15, -200.0000000000000000 ) ) ;
#6319 = CARTESIAN_POINT ( 'NONE',  ( -10.81189881249999729, -6.242252689847864744, -160.9687500020484094 ) ) ;
#6320 = CARTESIAN_POINT ( 'NONE',  ( 10.81189881249999729, 0.000000000000000000, -145.3437500020483810 ) ) ;
#6321 = EDGE_CURVE ( 'NONE', #24042, #30761, #808, .T. ) ;
#6322 =( BOUNDED_CURVE ( )  B_SPLINE_CURVE ( 2, ( #12858, #29081, #12437, #39203, #12646, #31692, #32116 ),
 .UNSPECIFIED., .F., .F. ) 
 B_SPLINE_CURVE_WITH_KNOTS ( ( 3, 2, 2, 3 ),
 ( 0.3097014925373136052, 0.3109452736318408794, 0.3121890547263682092, 0.3134328358208955390 ),
 .UNSPECIFIED. ) 
 CURVE ( )  GEOMETRIC_REPRESENTATION_ITEM ( )  RATIONAL_B_SPLINE_CURVE ( ( 0.9999999999999820144, 0.8660254037844566932, 1.000000000000000000, 0.8660254037844387076, 1.000000000000000000, 0.8660254037844387076, 1.000000000000000000 ) ) 
 REPRESENTATION_ITEM ( '' )  );
#6323 = CARTESIAN_POINT ( 'NONE',  ( 4.999999999999992006, -8.660254037844389075, -88.12500000409677625 ) ) ;
#6324 = CARTESIAN_POINT ( 'NONE',  ( 10.81189881249999907, 6.242252689847868297, -127.2187500020483668 ) ) ;
#6325 = CARTESIAN_POINT ( 'NONE',  ( 10.81189881249999729, 0.000000000000000000, -130.5312500020484094 ) ) ;
#6326 = CARTESIAN_POINT ( 'NONE',  ( 10.81189881249999551, -6.242252689847874514, -14.96875000204837036 ) ) ;
#6327 = CARTESIAN_POINT ( 'NONE',  ( 7.644554776091147741E-16, 12.48450537969573659, -144.9687500020484094 ) ) ;
#6328 = CARTESIAN_POINT ( 'NONE',  ( 10.70731569305653252, 1.500182182591227154, -180.0000000000000284 ) ) ;
#6329 = DIRECTION ( 'NONE',  ( 1.000000000000000000, 0.000000000000000000, 0.000000000000000000 ) ) ;
#6330 = CARTESIAN_POINT ( 'NONE',  ( 5.000000000000000000, 8.660254037844385522, -160.7500000000000000 ) ) ;
#6331 = CARTESIAN_POINT ( 'NONE',  ( -5.405949406249996869, 9.363379034771805109, 0.4687499979516285276 ) ) ;
#6332 = VECTOR ( 'NONE', #39526, 1000.000000000000000 ) ;
#6333 = CARTESIAN_POINT ( 'NONE',  ( -10.81189881249999729, 1.324075727343319199E-15, -72.59375000204838102 ) ) ;
#6334 = CARTESIAN_POINT ( 'NONE',  ( 10.81189881249999729, 0.000000000000000000, -51.03125000204835970 ) ) ;
#6335 = CARTESIAN_POINT ( 'NONE',  ( 5.405949406249992428, -9.363379034771808662, -51.09375000204835260 ) ) ;
#6336 = CARTESIAN_POINT ( 'NONE',  ( 10.00000000000154010, -5.773502691895370020, -16.00000000409673362 ) ) ;
#6337 = CARTESIAN_POINT ( 'NONE',  ( -2.293366432827344421E-15, -12.48450537969573659, -160.7187500020483810 ) ) ;
#6338 = CARTESIAN_POINT ( 'NONE',  ( -9.999999999999998224, 5.773502691896259087, -137.8750000000000000 ) ) ;
#6339 = CARTESIAN_POINT ( 'NONE',  ( 5.405949406249992428, -9.363379034771808662, -136.7812500020483810 ) ) ;
#6340 = DIRECTION ( 'NONE',  ( 1.000000000000000000, 0.000000000000000000, 0.000000000000000000 ) ) ;
#6341 = CARTESIAN_POINT ( 'NONE',  ( 9.999999999999998224, 0.000000000000000000, -113.3750000040967763 ) ) ;
#6342 = CARTESIAN_POINT ( 'NONE',  ( 4.999999999999992006, -8.660254037844389075, -95.24999999999998579 ) ) ;
#6343 = ORIENTED_EDGE ( 'NONE', *, *, #42516, .F. ) ;
#6344 = CARTESIAN_POINT ( 'NONE',  ( -10.81189881249999729, 6.242252689847871849, -114.9062500020483952 ) ) ;
#6345 = CARTESIAN_POINT ( 'NONE',  ( -9.999999999999998224, 1.224646799147353059E-15, -136.6250000040967620 ) ) ;
#6346 = CARTESIAN_POINT ( 'NONE',  ( -9.999999999999998224, 1.224646799147353059E-15, -141.1250000040967905 ) ) ;
#6347 = CARTESIAN_POINT ( 'NONE',  ( -5.405949406249996869, 9.363379034771805109, -176.5312500020483810 ) ) ;
#6348 = CARTESIAN_POINT ( 'NONE',  ( 4.999999999999992006, -8.660254037844389075, -38.62500000409676915 ) ) ;
#6349 = CARTESIAN_POINT ( 'NONE',  ( -2.121150477449813534E-15, -11.54700538379251284, -159.8750000000000000 ) ) ;
#6350 = CARTESIAN_POINT ( 'NONE',  ( 10.81189881249999907, 6.242252689847868297, -62.90625000204838813 ) ) ;
#6351 = AXIS2_PLACEMENT_3D ( 'NONE', #15746, #26543, #19837 ) ;
#6352 = CARTESIAN_POINT ( 'NONE',  ( 5.405949406249999534, 9.363379034771803333, -158.7812500020484094 ) ) ;
#6353 = CARTESIAN_POINT ( 'NONE',  ( 10.81189881249999551, -6.242252689847874514, -143.9687500020483810 ) ) ;
#6354 = CARTESIAN_POINT ( 'NONE',  ( 10.00000000000102318, -5.773502691895667560, -50.50000000409673362 ) ) ;
#6355 = CARTESIAN_POINT ( 'NONE',  ( 4.999999999999992006, -8.660254037844389075, -195.7500000000000000 ) ) ;
#6356 = ORIENTED_EDGE ( 'NONE', *, *, #17169, .F. ) ;
#6357 = FACE_OUTER_BOUND ( 'NONE', #17056, .T. ) ;
#6358 = AXIS2_PLACEMENT_3D ( 'NONE', #35803, #6235, #193 ) ;
#6360 = EDGE_LOOP ( 'NONE', ( #10845, #42056, #11228, #23275, #19389 ) ) ;
#6359 = CARTESIAN_POINT ( 'NONE',  ( 5.405949406249999534, 9.363379034771803333, -73.28125000204838102 ) ) ;
#6361 = APPROVAL_ROLE ( '' ) ;
#6363 = ORIENTED_EDGE ( 'NONE', *, *, #4762, .T. ) ;
#6362 = CARTESIAN_POINT ( 'NONE',  ( -10.81189881249999907, -6.242252689847864744, -121.9687500020483952 ) ) ;
#6364 = ORIENTED_EDGE ( 'NONE', *, *, #14285, .F. ) ;
#6365 = CARTESIAN_POINT ( 'NONE',  ( -10.81189881249999729, 6.242252689847871849, -26.21875000204837391 ) ) ;
#6366 =( BOUNDED_CURVE ( )  B_SPLINE_CURVE ( 2, ( #19737, #32917, #3350, #16483, #34415, #18416, #20797 ),
 .UNSPECIFIED., .F., .F. ) 
 B_SPLINE_CURVE_WITH_KNOTS ( ( 3, 2, 2, 3 ),
 ( 0.000000000000000000, 0.001243781094527364461, 0.002487562189054728923, 0.003731343283582092950 ),
 .UNSPECIFIED. ) 
 CURVE ( )  GEOMETRIC_REPRESENTATION_ITEM ( )  RATIONAL_B_SPLINE_CURVE ( ( 1.000000000000000000, 0.8660254037844387076, 1.000000000000000000, 0.8660254037844387076, 1.000000000000000000, 0.8660254037844383745, 1.000000000000000444 ) ) 
 REPRESENTATION_ITEM ( '' )  );
#6367 = CARTESIAN_POINT ( 'NONE',  ( 10.81189881249999551, -6.242252689847874514, -1.656250002048371694 ) ) ;
#6368 = CARTESIAN_POINT ( 'NONE',  ( 10.81189881249999907, 6.242252689847868297, -44.71875000204837391 ) ) ;
#6369 = DIRECTION ( 'NONE',  ( -0.000000000000000000, -0.000000000000000000, 1.000000000000000000 ) ) ;
#6370 = CARTESIAN_POINT ( 'NONE',  ( -4.999999999999996447, 8.660254037844387298, -31.49999999999997158 ) ) ;
#6371 = CARTESIAN_POINT ( 'NONE',  ( -2.293366432827344421E-15, -12.48450537969573659, -187.7187500020484094 ) ) ;
#6372 = CARTESIAN_POINT ( 'NONE',  ( -2.293366432827344421E-15, -12.48450537969573659, -172.7187500020484094 ) ) ;
#6373 = CARTESIAN_POINT ( 'NONE',  ( 5.405949406249992428, -9.363379034771808662, -150.0937500020483810 ) ) ;
#6374 = CARTESIAN_POINT ( 'NONE',  ( 5.405949406249992428, -9.363379034771808662, -168.0937500020484094 ) ) ;
#6375 = CARTESIAN_POINT ( 'NONE',  ( -8.571370657139810611E-15, -145.0000000000000000, 7.499999999999982236 ) ) ;
#6376 =( BOUNDED_CURVE ( )  B_SPLINE_CURVE ( 2, ( #12120, #42104, #19440, #38457, #15979, #12539, #29381 ),
 .UNSPECIFIED., .F., .F. ) 
 B_SPLINE_CURVE_WITH_KNOTS ( ( 3, 2, 2, 3 ),
 ( 0.3544776119402986980, 0.3557213930348260278, 0.3569651741293533576, 0.3582089552238806873 ),
 .UNSPECIFIED. ) 
 CURVE ( )  GEOMETRIC_REPRESENTATION_ITEM ( )  RATIONAL_B_SPLINE_CURVE ( ( 0.9999999999999820144, 0.8660254037844566932, 1.000000000000000000, 0.8660254037844387076, 1.000000000000000000, 0.8660254037844267172, 1.000000000000011990 ) ) 
 REPRESENTATION_ITEM ( '' )  );
#6377 = CARTESIAN_POINT ( 'NONE',  ( -10.00000000000154188, 5.773502691895366468, -19.75000000409673362 ) ) ;
#6378 = CARTESIAN_POINT ( 'NONE',  ( -9.999999999999998224, 5.773502691896259087, -185.8750000000000000 ) ) ;
#6379 = CARTESIAN_POINT ( 'NONE',  ( -10.81189881249999729, 6.242252689847871849, -99.71875000204839523 ) ) ;
#6380 = CARTESIAN_POINT ( 'NONE',  ( -10.00000000000051337, 5.773502691895962435, -108.2500000040967763 ) ) ;
#6381 = CARTESIAN_POINT ( 'NONE',  ( 10.81189881249999729, 0.000000000000000000, -78.03125000204838102 ) ) ;
#6382 = CARTESIAN_POINT ( 'NONE',  ( -9.999999999999998224, 1.224646799147353059E-15, -96.12500000409677625 ) ) ;
#6383 = ADVANCED_FACE ( 'NONE', ( #14138 ), #40905, .T. ) ;
#6384 = CARTESIAN_POINT ( 'NONE',  ( -10.81189881249999907, -6.242252689847864744, -183.4687500020484379 ) ) ;
#6385 = CARTESIAN_POINT ( 'NONE',  ( -5.405949406249996869, 9.363379034771805109, -170.5312500020484094 ) ) ;
#6386 = EDGE_CURVE ( 'NONE', #2082, #19929, #1156, .T. ) ;
#6387 = CARTESIAN_POINT ( 'NONE',  ( -10.81189881249999729, 6.242252689847871849, -62.40625000204838813 ) ) ;
#6388 = CARTESIAN_POINT ( 'NONE',  ( -2.121150477449813534E-15, -11.54700538379251284, -134.7500000040967905 ) ) ;
#6389 = CARTESIAN_POINT ( 'NONE',  ( 7.070501591499377789E-16, 11.54700538379251284, -112.6249999999999858 ) ) ;
#6390 = ORIENTED_EDGE ( 'NONE', *, *, #35439, .F. ) ;
#6391 = CARTESIAN_POINT ( 'NONE',  ( -5.405949406250003975, -9.363379034771801557, -141.5312500020483810 ) ) ;
#6392 = CARTESIAN_POINT ( 'NONE',  ( 10.81189881249999729, 0.000000000000000000, -157.5312500020484094 ) ) ;
#6393 = CARTESIAN_POINT ( 'NONE',  ( 10.81189881249999729, 0.000000000000000000, -195.0312500020484094 ) ) ;
#6394 = CARTESIAN_POINT ( 'NONE',  ( 9.999999999999998224, 0.000000000000000000, -200.0000000000000000 ) ) ;
#6395 = CARTESIAN_POINT ( 'NONE',  ( -10.81189881249999907, -6.242252689847864744, -93.46875000204836681 ) ) ;
#6396 = VERTEX_POINT ( 'NONE', #14579 ) ;
#6397 = CARTESIAN_POINT ( 'NONE',  ( -10.00000000000000000, -5.773502691896251982, -55.12499999999997158 ) ) ;
#6398 = CARTESIAN_POINT ( 'NONE',  ( 5.405949406249999534, 9.363379034771803333, -190.0937500020483810 ) ) ;
#6399 = CARTESIAN_POINT ( 'NONE',  ( 9.999999999999998224, 0.000000000000000000, -75.87500000409677625 ) ) ;
#6400 = CARTESIAN_POINT ( 'NONE',  ( 10.00000000000025402, -5.773502691896113426, -116.5000000040967763 ) ) ;
#6401 = CARTESIAN_POINT ( 'NONE',  ( -9.999999999999998224, 1.224646799147353059E-15, -160.6250000040967905 ) ) ;
#6402 = CARTESIAN_POINT ( 'NONE',  ( 7.644554776091147741E-16, 12.48450537969573659, -82.15625000204838102 ) ) ;
#6403 = CARTESIAN_POINT ( 'NONE',  ( -2.293366432827344421E-15, -12.48450537969573659, -70.90625000204839523 ) ) ;
#6404 = CARTESIAN_POINT ( 'NONE',  ( 9.999999999999996447, -5.773502691896262640, -61.00000000409677625 ) ) ;
#6405 = CARTESIAN_POINT ( 'NONE',  ( 10.81189881249999551, -6.242252689847874514, -17.96875000204836681 ) ) ;
#6406 = CYLINDRICAL_SURFACE ( 'NONE', #24204, 9.999999999999998224 ) ;
#6407 = CARTESIAN_POINT ( 'NONE',  ( 5.405949406249999534, 9.363379034771803333, -182.7812500020484094 ) ) ;
#6408 = CARTESIAN_POINT ( 'NONE',  ( -10.81189881249999729, 1.324075727343319199E-15, -11.28125000204835438 ) ) ;
#6409 = DIRECTION ( 'NONE',  ( -1.000000000000000000, 0.000000000000000000, 0.000000000000000000 ) ) ;
#6410 = DIRECTION ( 'NONE',  ( 1.000000000000000000, 0.000000000000000000, 0.000000000000000000 ) ) ;
#6411 = CARTESIAN_POINT ( 'NONE',  ( 100.0000000000000284, -40.00000000000001421, -160.0000000000000000 ) ) ;
#6412 = DIRECTION ( 'NONE',  ( -0.000000000000000000, -0.000000000000000000, -1.000000000000000000 ) ) ;
#6413 = CARTESIAN_POINT ( 'NONE',  ( -5.000000000000003553, -8.660254037844383745, -169.0000000000000000 ) ) ;
#6414 = FACE_OUTER_BOUND ( 'NONE', #18182, .T. ) ;
#6416 = ORIENTED_EDGE ( 'NONE', *, *, #37047, .T. ) ;
#6415 = CARTESIAN_POINT ( 'NONE',  ( 5.405949406249992428, -9.363379034771808662, -96.28125000204838102 ) ) ;
#6417 = CARTESIAN_POINT ( 'NONE',  ( -5.000000000000003553, -8.660254037844383745, -181.3750000040967905 ) ) ;
#6419 = VERTEX_POINT ( 'NONE', #17179 ) ;
#6418 = DIRECTION ( 'NONE',  ( -0.000000000000000000, -0.000000000000000000, 1.000000000000000000 ) ) ;
#6420 = VERTEX_POINT ( 'NONE', #27767 ) ;
#6421 = CARTESIAN_POINT ( 'NONE',  ( -10.81189881249999729, 1.324075727343319199E-15, -38.09375000204837391 ) ) ;
#6422 = CARTESIAN_POINT ( 'NONE',  ( 10.81189881249999729, 0.000000000000000000, -21.03125000204836326 ) ) ;
#6423 = CALENDAR_DATE ( 2026, 28, 9 ) ;
#6424 = CARTESIAN_POINT ( 'NONE',  ( 10.81189881249999729, 0.000000000000000000, -80.84375000204838102 ) ) ;
#6425 = CARTESIAN_POINT ( 'NONE',  ( 5.405949406249999534, 9.363379034771803333, -194.5937500020484094 ) ) ;
#6426 = CARTESIAN_POINT ( 'NONE',  ( -11.54700538379251817, 20.00000000000000355, 49.99999999999998579 ) ) ;
#6427 = CARTESIAN_POINT ( 'NONE',  ( 9.999999999999998224, 0.000000000000000000, -200.0000000000000000 ) ) ;
#6428 = CARTESIAN_POINT ( 'NONE',  ( -10.81189881249999729, 1.324075727343319199E-15, -153.7812500020484094 ) ) ;
#6429 = CARTESIAN_POINT ( 'NONE',  ( 5.000000000000000000, 8.660254037844385522, -6.625000004096770923 ) ) ;
#6430 = DIRECTION ( 'NONE',  ( -0.000000000000000000, -0.000000000000000000, 1.000000000000000000 ) ) ;
#6431 = CARTESIAN_POINT ( 'NONE',  ( 5.405949406249992428, -9.363379034771808662, -118.5937500020483810 ) ) ;
#6432 = CARTESIAN_POINT ( 'NONE',  ( -2.293366432827344421E-15, -12.48450537969573659, -97.90625000204839523 ) ) ;
#6433 = EDGE_CURVE ( 'NONE', #16098, #30518, #9955, .T. ) ;
#6434 = CARTESIAN_POINT ( 'NONE',  ( 5.405949406249999534, 9.363379034771803333, -104.5937500020483810 ) ) ;
#6435 = CARTESIAN_POINT ( 'NONE',  ( -10.81189881249999729, 6.242252689847871849, -75.71875000204836681 ) ) ;
#6436 = CARTESIAN_POINT ( 'NONE',  ( -5.405949406249996869, 9.363379034771805109, -82.03125000204839523 ) ) ;
#6437 = CARTESIAN_POINT ( 'NONE',  ( 9.999999999999996447, -5.773502691896262640, -169.0000000040967905 ) ) ;
#6438 = EDGE_CURVE ( 'NONE', #3489, #3790, #603, .T. ) ;
#6439 = CARTESIAN_POINT ( 'NONE',  ( -9.999999999999998224, 1.224646799147353059E-15, -145.6250000040967905 ) ) ;
#6440 = CARTESIAN_POINT ( 'NONE',  ( -10.81189881249999729, 6.242252689847871849, -168.9062500020484094 ) ) ;
#6441 = CARTESIAN_POINT ( 'NONE',  ( 10.81189881249999907, 6.242252689847868297, -176.9062500020484094 ) ) ;
#6442 = EDGE_CURVE ( 'NONE', #40023, #23935, #40064, .T. ) ;
#6443 = CARTESIAN_POINT ( 'NONE',  ( 5.000000000000000000, 8.660254037844385522, -153.6250000040967905 ) ) ;
#6444 = CARTESIAN_POINT ( 'NONE',  ( 0.000000000000000000, 0.000000000000000000, -219.9999999999999716 ) ) ;
#6445 = CARTESIAN_POINT ( 'NONE',  ( -10.81189881249999729, 1.324075727343319199E-15, -5.093750002048369474 ) ) ;
#6446 = CARTESIAN_POINT ( 'NONE',  ( -5.000000000000003553, -8.660254037844383745, -127.0000000000000000 ) ) ;
#6447 = CARTESIAN_POINT ( 'NONE',  ( -10.81189881249999729, 1.324075727343319199E-15, -116.0937500020483810 ) ) ;
#6448 = CARTESIAN_POINT ( 'NONE',  ( -4.999999999999996447, 8.660254037844387298, -85.49999999999998579 ) ) ;
#6449 = CARTESIAN_POINT ( 'NONE',  ( 10.81189881249999729, 0.000000000000000000, -12.03125000204835438 ) ) ;
#6450 = CARTESIAN_POINT ( 'NONE',  ( 4.999999999999992006, -8.660254037844389075, -100.1250000040967905 ) ) ;
#6451 =( BOUNDED_CURVE ( )  B_SPLINE_CURVE ( 2, ( #19306, #3771, #16905, #13244, #19734, #13032, #39582 ),
 .UNSPECIFIED., .F., .F. ) 
 B_SPLINE_CURVE_WITH_KNOTS ( ( 3, 2, 2, 3 ),
 ( 0.02985074626865674360, 0.03109452736318411153, 0.03233830845771147600, 0.03358208955223884046 ),
 .UNSPECIFIED. ) 
 CURVE ( )  GEOMETRIC_REPRESENTATION_ITEM ( )  RATIONAL_B_SPLINE_CURVE ( ( 0.9999999999999970024, 0.8660254037844417052, 1.000000000000000000, 0.8660254037844387076, 1.000000000000000000, 0.8660254037844349329, 1.000000000000003775 ) ) 
 REPRESENTATION_ITEM ( '' )  );
#6452 = CARTESIAN_POINT ( 'NONE',  ( 9.999999999999998224, 0.000000000000000000, -200.0000000000000000 ) ) ;
#6453 = CC_DESIGN_PERSON_AND_ORGANIZATION_ASSIGNMENT ( #3966, #17106, ( #1498 ) ) ;
#6454 = CARTESIAN_POINT ( 'NONE',  ( -10.81189881249999729, 1.324075727343319199E-15, -107.2812500020483810 ) ) ;
#6455 = CARTESIAN_POINT ( 'NONE',  ( 10.81189881249999551, -6.242252689847874514, -88.65625000204838102 ) ) ;
#6456 = ORIENTED_EDGE ( 'NONE', *, *, #8166, .F. ) ;
#6457 = CARTESIAN_POINT ( 'NONE',  ( -9.999999999999998224, 1.224646799147353059E-15, -81.12500000409677625 ) ) ;
#6458 = CARTESIAN_POINT ( 'NONE',  ( 0.000000000000000000, 0.000000000000000000, -200.0000000000000000 ) ) ;
#6459 = CARTESIAN_POINT ( 'NONE',  ( 5.405949406249992428, -9.363379034771808662, -39.09375000204837391 ) ) ;
#6460 = EDGE_LOOP ( 'NONE', ( #2524, #40983, #42374, #38132 ) ) ;
#6461 = CARTESIAN_POINT ( 'NONE',  ( 9.999999999999996447, -5.773502691896262640, -6.624999999999968026 ) ) ;
#6462 = CARTESIAN_POINT ( 'NONE',  ( -4.999999999999996447, 8.660254037844387298, -144.0000000000000000 ) ) ;
#6463 = CARTESIAN_POINT ( 'NONE',  ( -5.000000000000003553, -8.660254037844383745, -11.87500000409674783 ) ) ;
#6464 = ADVANCED_FACE ( 'NONE', ( #17390 ), #11341, .T. ) ;
#6465 = CARTESIAN_POINT ( 'NONE',  ( 5.000000000000000000, 8.660254037844385522, -196.7500000000000000 ) ) ;
#6467 = ORIENTED_EDGE ( 'NONE', *, *, #23858, .T. ) ;
#6466 = CARTESIAN_POINT ( 'NONE',  ( -5.405949406249996869, 9.363379034771805109, -116.5312500020483952 ) ) ;
#6468 = CARTESIAN_POINT ( 'NONE',  ( 4.999999999999992006, -8.660254037844389075, -12.74999999999995559 ) ) ;
#6469 = VERTEX_POINT ( 'NONE', #32871 ) ;
#6470 = CARTESIAN_POINT ( 'NONE',  ( -10.81189881249999729, 6.242252689847871849, -51.90625000204838813 ) ) ;
#6471 = COORDINATED_UNIVERSAL_TIME_OFFSET ( 6, 0, .AHEAD. ) ;
#6472 = CARTESIAN_POINT ( 'NONE',  ( -2.293366432827344421E-15, -12.48450537969573659, -103.7187500020483668 ) ) ;
#6473 = CARTESIAN_POINT ( 'NONE',  ( 10.81189881249999551, -6.242252689847874514, -127.6562500020483810 ) ) ;
#6474 = ORIENTED_EDGE ( 'NONE', *, *, #41638, .F. ) ;
#6475 = CARTESIAN_POINT ( 'NONE',  ( -4.999999999999996447, 8.660254037844387298, -127.8750000040967905 ) ) ;
#6476 = CARTESIAN_POINT ( 'NONE',  ( -5.405949406249996869, 9.363379034771805109, -178.0312500020483810 ) ) ;
#6477 = CARTESIAN_POINT ( 'NONE',  ( 5.405949406249999534, 9.363379034771803333, -1.093750002048365921 ) ) ;
#6478 = LINE ( 'NONE', #37523, #24560 ) ;
#6479 = CARTESIAN_POINT ( 'NONE',  ( -10.81189881249999729, 1.324075727343319199E-15, -135.5937500020483810 ) ) ;
#6480 = CARTESIAN_POINT ( 'NONE',  ( 10.81189881249999907, 6.242252689847868297, -104.7187500020483810 ) ) ;
#6481 = DIRECTION ( 'NONE',  ( -0.000000000000000000, -0.000000000000000000, 1.000000000000000000 ) ) ;
#6482 = CARTESIAN_POINT ( 'NONE',  ( -10.81189881249999729, 1.324075727343319199E-15, -108.7812500020483810 ) ) ;
#6483 = CARTESIAN_POINT ( 'NONE',  ( -5.000000000000003553, -8.660254037844383745, -194.8750000040967905 ) ) ;
#6484 = CARTESIAN_POINT ( 'NONE',  ( 7.644554776091147741E-16, 12.48450537969573659, -117.9687500020483668 ) ) ;
#6485 = CARTESIAN_POINT ( 'NONE',  ( -5.405949406249996869, 9.363379034771805109, -187.0312500020484094 ) ) ;
#6486 =( BOUNDED_CURVE ( )  B_SPLINE_CURVE ( 2, ( #29062, #39185, #32516, #42200, #2318, #22575, #35754 ),
 .UNSPECIFIED., .F., .F. ) 
 B_SPLINE_CURVE_WITH_KNOTS ( ( 3, 2, 2, 3 ),
 ( 0.1007462686567163757, 0.1019900497512437887, 0.1032338308457712017, 0.1044776119402986148 ),
 .UNSPECIFIED. ) 
 CURVE ( )  GEOMETRIC_REPRESENTATION_ITEM ( )  RATIONAL_B_SPLINE_CURVE ( ( 1.000000000000004441, 0.8660254037844342667, 1.000000000000000000, 0.8660254037844387076, 1.000000000000000000, 0.8660254037844267172, 1.000000000000011990 ) ) 
 REPRESENTATION_ITEM ( '' )  );
#6487 = CARTESIAN_POINT ( 'NONE',  ( -2.121150477449813534E-15, -11.54700538379251284, -143.3750000000000000 ) ) ;
#6488 = CARTESIAN_POINT ( 'NONE',  ( 9.999999999999996447, -5.773502691896262640, -5.124999999999963585 ) ) ;
#6489 = CARTESIAN_POINT ( 'NONE',  ( -2.293366432827344421E-15, -12.48450537969573659, -61.71875000204839523 ) ) ;
#6490 = CARTESIAN_POINT ( 'NONE',  ( 10.81189881249999907, 6.242252689847868297, -52.21875000204837391 ) ) ;
#6491 = CARTESIAN_POINT ( 'NONE',  ( 7.070501591499377789E-16, 11.54700538379251284, -183.5000000040968189 ) ) ;
#6492 = CARTESIAN_POINT ( 'NONE',  ( -5.405949406250003975, -9.363379034771801557, -21.53125000204836326 ) ) ;
#6493 = CARTESIAN_POINT ( 'NONE',  ( 10.81189881249999551, -6.242252689847874514, -26.96875000204837391 ) ) ;
#6494 = CARTESIAN_POINT ( 'NONE',  ( -5.405949406249996869, 9.363379034771805109, -134.3437500020484094 ) ) ;
#6495 = CARTESIAN_POINT ( 'NONE',  ( -9.999999999999998224, 1.224646799147353059E-15, -101.7500000000000000 ) ) ;
#6496 = CARTESIAN_POINT ( 'NONE',  ( 10.81189881249999907, 6.242252689847868297, -38.90625000204836681 ) ) ;
#6497 = CARTESIAN_POINT ( 'NONE',  ( -5.000000000000003553, -8.660254037844383745, -114.9999999999999858 ) ) ;
#6498 = CARTESIAN_POINT ( 'NONE',  ( -5.000000000000003553, -8.660254037844383745, -68.49999999999997158 ) ) ;
#6499 = CARTESIAN_POINT ( 'NONE',  ( -10.81189881249999907, -6.242252689847864744, -132.6562500020484094 ) ) ;
#6500 = CARTESIAN_POINT ( 'NONE',  ( -2.293366432827344421E-15, -12.48450537969573659, -117.4062500020483952 ) ) ;
#6501 = ORIENTED_EDGE ( 'NONE', *, *, #11941, .T. ) ;
#6502 = CARTESIAN_POINT ( 'NONE',  ( -9.999999999999998224, 1.224646799147353059E-15, -200.0000000000000000 ) ) ;
#6503 = CARTESIAN_POINT ( 'NONE',  ( -2.121150477449813534E-15, -11.54700538379251284, -107.7500000040967763 ) ) ;
#6504 = CARTESIAN_POINT ( 'NONE',  ( -5.000000000000003553, -8.660254037844383745, -136.3750000040967905 ) ) ;
#6505 = CARTESIAN_POINT ( 'NONE',  ( 5.405949406249999534, 9.363379034771803333, -64.09375000204836681 ) ) ;
#6506 = ORIENTED_EDGE ( 'NONE', *, *, #3873, .F. ) ;
#6507 = CARTESIAN_POINT ( 'NONE',  ( 9.999999999999998224, 0.000000000000000000, -40.99999999999997868 ) ) ;
#6508 = EDGE_CURVE ( 'NONE', #5998, #8957, #30898, .T. ) ;
#6509 = CARTESIAN_POINT ( 'NONE',  ( 5.000000000000000000, 8.660254037844385522, -15.62500000409675138 ) ) ;
#6510 = CARTESIAN_POINT ( 'NONE',  ( -5.405949406249996869, 9.363379034771805109, -41.53125000204838102 ) ) ;
#6511 = CARTESIAN_POINT ( 'NONE',  ( 9.999999999999998224, 0.000000000000000000, -119.3750000040967905 ) ) ;
#6512 = CARTESIAN_POINT ( 'NONE',  ( -5.000000000000003553, -8.660254037844383745, -32.87500000409676915 ) ) ;
#6513 = LINE ( 'NONE', #3068, #37623 ) ;
#6514 = CARTESIAN_POINT ( 'NONE',  ( -10.81189881249999907, -6.242252689847864744, -138.6562500020484094 ) ) ;
#6515 = CARTESIAN_POINT ( 'NONE',  ( 10.81189881249999551, -6.242252689847874514, -138.1562500020484094 ) ) ;
#6516 = CARTESIAN_POINT ( 'NONE',  ( 10.00000000000051159, -5.773502691895965988, -123.6250000000000142 ) ) ;
#6517 = EDGE_LOOP ( 'NONE', ( #1159, #8804, #2499, #4989 ) ) ;
#6518 = VERTEX_POINT ( 'NONE', #36520 ) ;
#6519 = ORIENTED_EDGE ( 'NONE', *, *, #12748, .T. ) ;
#6520 = LINE ( 'NONE', #16201, #18710 ) ;
#6521 = CARTESIAN_POINT ( 'NONE',  ( -10.81189881249999729, 1.324075727343319199E-15, -173.0937500020484094 ) ) ;
#6522 = CARTESIAN_POINT ( 'NONE',  ( 7.644554776091147741E-16, 12.48450537969573659, -26.46875000204837747 ) ) ;
#6523 = CARTESIAN_POINT ( 'NONE',  ( -9.999999999999998224, 1.224646799147353059E-15, -111.1250000040967763 ) ) ;
#6524 = CARTESIAN_POINT ( 'NONE',  ( 5.405949406249999534, 9.363379034771803333, -155.5937500020483810 ) ) ;
#6525 = CARTESIAN_POINT ( 'NONE',  ( -2.293366432827344421E-15, -12.48450537969573659, -141.2187500020483810 ) ) ;
#6526 = CARTESIAN_POINT ( 'NONE',  ( -9.999999999999998224, 1.224646799147353059E-15, -200.0000000000000000 ) ) ;
#6527 = CARTESIAN_POINT ( 'NONE',  ( 10.81189881249999907, 6.242252689847868297, -128.7187500020483810 ) ) ;
#6528 = CARTESIAN_POINT ( 'NONE',  ( 7.644554776091147741E-16, 12.48450537969573659, -136.1562500020483810 ) ) ;
#6529 = CARTESIAN_POINT ( 'NONE',  ( 7.644554776091147741E-16, 12.48450537969573659, -21.96875000204837391 ) ) ;
#6530 = CARTESIAN_POINT ( 'NONE',  ( -10.81189881249999729, 6.242252689847871849, -140.2187500020483810 ) ) ;
#6531 = DIRECTION ( 'NONE',  ( -0.000000000000000000, -0.000000000000000000, 1.000000000000000000 ) ) ;
#6532 = CARTESIAN_POINT ( 'NONE',  ( -4.999999999999996447, 8.660254037844387298, -25.49999999999996803 ) ) ;
#6533 = CARTESIAN_POINT ( 'NONE',  ( 9.999999999999998224, 0.000000000000000000, -167.0000000000000000 ) ) ;
#6534 = CARTESIAN_POINT ( 'NONE',  ( 10.81189881249999729, 0.000000000000000000, -0.03125000204837191653 ) ) ;
#6535 = CARTESIAN_POINT ( 'NONE',  ( 7.644554776091147741E-16, 12.48450537969573659, -71.46875000204838102 ) ) ;
#6536 = CARTESIAN_POINT ( 'NONE',  ( 10.81189881249999907, 6.242252689847868297, -41.90625000204836681 ) ) ;
#6537 = CARTESIAN_POINT ( 'NONE',  ( -10.81189881249999907, -6.242252689847864744, -55.96875000204836681 ) ) ;
#6538 = CARTESIAN_POINT ( 'NONE',  ( 0.000000000000000000, 0.000000000000000000, -99.99999999999998579 ) ) ;
#6539 = CARTESIAN_POINT ( 'NONE',  ( -10.81189881249999907, -6.242252689847864744, -165.4687500020484094 ) ) ;
#6540 = CARTESIAN_POINT ( 'NONE',  ( -9.999999999999998224, 1.224646799147353059E-15, -136.2499999999999716 ) ) ;
#6541 = CARTESIAN_POINT ( 'NONE',  ( 10.81189881249999729, 6.242252689847867408, -134.9062500020483810 ) ) ;
#6542 = CARTESIAN_POINT ( 'NONE',  ( 10.00000000000051159, -5.773502691895965988, -98.50000000409677625 ) ) ;
#6543 = CARTESIAN_POINT ( 'NONE',  ( 5.000000000000000000, 8.660254037844385522, -117.6250000040967905 ) ) ;
#6544 = CARTESIAN_POINT ( 'NONE',  ( 4.999999999999992006, -8.660254037844389075, -87.74999999999998579 ) ) ;
#6545 = VERTEX_POINT ( 'NONE', #36100 ) ;
#6546 = CARTESIAN_POINT ( 'NONE',  ( 5.405949406249999534, 9.363379034771803333, -119.7812500020483952 ) ) ;
#6547 = CARTESIAN_POINT ( 'NONE',  ( 10.00000000000000000, 5.773502691896255534, -135.7500000040967905 ) ) ;
#6548 = CARTESIAN_POINT ( 'NONE',  ( -5.000000000000003553, -8.660254037844383745, -48.99999999999998579 ) ) ;
#6549 = CARTESIAN_POINT ( 'NONE',  ( -2.293366432827344421E-15, -12.48450537969573659, -172.9062500020484379 ) ) ;
#6550 = CARTESIAN_POINT ( 'NONE',  ( 9.999999999999996447, -5.773502691896262640, -38.50000000409676915 ) ) ;
#6551 = CARTESIAN_POINT ( 'NONE',  ( -2.121150477449813534E-15, -11.54700538379251284, -91.25000000409677625 ) ) ;
#6552 = CARTESIAN_POINT ( 'NONE',  ( 5.405949406249992428, -9.363379034771808662, -57.28125000204836681 ) ) ;
#6553 = CARTESIAN_POINT ( 'NONE',  ( 9.999999999999998224, 0.000000000000000000, -45.49999999999998579 ) ) ;
#6554 = CARTESIAN_POINT ( 'NONE',  ( -2.293366432827344421E-15, -12.48450537969573659, -159.4062500020483810 ) ) ;
#6555 = CARTESIAN_POINT ( 'NONE',  ( 10.81189881249999551, -6.242252689847874514, -145.4687500020483810 ) ) ;
#6556 = DIRECTION ( 'NONE',  ( 0.000000000000000000, 0.000000000000000000, 1.000000000000000000 ) ) ;
#6557 = LINE ( 'NONE', #32894, #17166 ) ;
#6558 = ORIENTED_EDGE ( 'NONE', *, *, #18255, .T. ) ;
#6559 = CARTESIAN_POINT ( 'NONE',  ( -9.999999999999998224, 1.224646799147353059E-15, -189.1250000040967905 ) ) ;
#6560 = EDGE_CURVE ( 'NONE', #7227, #28673, #29016, .T. ) ;
#6562 = ORIENTED_EDGE ( 'NONE', *, *, #32262, .T. ) ;
#6561 = CARTESIAN_POINT ( 'NONE',  ( 5.405949406249992428, -9.363379034771808662, -73.78125000204838102 ) ) ;
#6564 = VERTEX_POINT ( 'NONE', #16646 ) ;
#6563 = CARTESIAN_POINT ( 'NONE',  ( 10.81189881249999729, 0.000000000000000000, -118.3437500020483810 ) ) ;
#6565 = VERTEX_POINT ( 'NONE', #33304 ) ;
#6566 = AXIS2_PLACEMENT_3D ( 'NONE', #10357, #39929, #7353 ) ;
#6567 = CARTESIAN_POINT ( 'NONE',  ( 10.81189881249999729, 6.242252689847867408, -20.71875000204836681 ) ) ;
#6568 = CARTESIAN_POINT ( 'NONE',  ( -2.293366432827344421E-15, -12.48450537969573659, -1.906250002048373027 ) ) ;
#6569 = CARTESIAN_POINT ( 'NONE',  ( 10.81189881249999551, -6.242252689847874514, -46.46875000204837391 ) ) ;
#6570 = CYLINDRICAL_SURFACE ( 'NONE', #41200, 9.999999999999998224 ) ;
#6571 = CARTESIAN_POINT ( 'NONE',  ( 10.00000000000000000, 5.773502691896255534, -30.37499999999995737 ) ) ;
#6572 = CARTESIAN_POINT ( 'NONE',  ( 10.81189881249999729, 6.242252689847867408, -176.7187500020484094 ) ) ;
#6573 = CARTESIAN_POINT ( 'NONE',  ( 10.81189881249999907, 6.242252689847868297, -167.7187500020483810 ) ) ;
#6574 = CARTESIAN_POINT ( 'NONE',  ( -10.81189881249999729, 6.242252689847871849, -150.7187500020483810 ) ) ;
#6575 = CARTESIAN_POINT ( 'NONE',  ( -5.405949406250003975, -9.363379034771801557, -160.8437500020484094 ) ) ;
#6576 = CARTESIAN_POINT ( 'NONE',  ( 10.00000000000051159, -5.773502691895965988, -104.5000000040967620 ) ) ;
#6577 = CYLINDRICAL_SURFACE ( 'NONE', #9513, 9.999999999999998224 ) ;
#6578 = CARTESIAN_POINT ( 'NONE',  ( -2.121150477449813534E-15, -11.54700538379251284, -191.3750000000000284 ) ) ;
#6579 = CARTESIAN_POINT ( 'NONE',  ( 10.81189881249999729, 0.000000000000000000, -94.34375000204838102 ) ) ;
#6580 = EDGE_CURVE ( 'NONE', #29342, #14673, #39964, .T. ) ;
#6581 = CARTESIAN_POINT ( 'NONE',  ( 9.999999999999998224, 0.000000000000000000, -123.8750000040967905 ) ) ;
#6582 = CARTESIAN_POINT ( 'NONE',  ( 7.644554776091147741E-16, 12.48450537969573659, -70.15625000204839523 ) ) ;
#6583 = CARTESIAN_POINT ( 'NONE',  ( -2.121150477449813534E-15, -11.54700538379251284, -5.374999999999961808 ) ) ;
#6584 = CARTESIAN_POINT ( 'NONE',  ( 5.405949406249999534, 9.363379034771803333, -188.5937500020483810 ) ) ;
#6585 = CARTESIAN_POINT ( 'NONE',  ( -2.293366432827344421E-15, -12.48450537969573659, -165.4062500020483526 ) ) ;
#6586 = CARTESIAN_POINT ( 'NONE',  ( -10.81189881249999907, -6.242252689847864744, -62.15625000204838102 ) ) ;
#6587 = CARTESIAN_POINT ( 'NONE',  ( -10.00000000000000000, -5.773502691896251982, -141.0000000040967905 ) ) ;
#6588 = CARTESIAN_POINT ( 'NONE',  ( -4.999999999999996447, 8.660254037844387298, -118.5000000000000000 ) ) ;
#6589 = ORIENTED_EDGE ( 'NONE', *, *, #5190, .F. ) ;
#6590 = CARTESIAN_POINT ( 'NONE',  ( -2.293366432827344421E-15, -12.48450537969573659, -144.4062500020484094 ) ) ;
#6591 = CARTESIAN_POINT ( 'NONE',  ( 5.405949406249999534, 9.363379034771803333, -152.7812500020484094 ) ) ;
#6592 = CARTESIAN_POINT ( 'NONE',  ( -10.81189881249999729, 1.324075727343319199E-15, -198.7812500020484094 ) ) ;
#6593 = CYLINDRICAL_SURFACE ( 'NONE', #8913, 9.999999999999998224 ) ;
#6594 = CARTESIAN_POINT ( 'NONE',  ( 10.81189881249999729, 0.000000000000000000, -89.84375000204838102 ) ) ;
#6595 = VERTEX_POINT ( 'NONE', #22946 ) ;
#6596 = CARTESIAN_POINT ( 'NONE',  ( 9.999999999999998224, 0.000000000000000000, -58.99999999999997158 ) ) ;
#6597 = CARTESIAN_POINT ( 'NONE',  ( 10.81189881249999907, 6.242252689847868297, -190.2187500020484094 ) ) ;
#6598 = CARTESIAN_POINT ( 'NONE',  ( 5.000000000000000000, 8.660254037844385522, -66.62500000409676204 ) ) ;
#6599 = DIRECTION ( 'NONE',  ( 1.000000000000000000, 0.000000000000000000, 0.000000000000000000 ) ) ;
#6600 = CARTESIAN_POINT ( 'NONE',  ( -2.121150477449813534E-15, -11.54700538379251284, -160.2500000040967620 ) ) ;
#6601 = CARTESIAN_POINT ( 'NONE',  ( 10.81189881249999907, 6.242252689847868297, -83.90625000204836681 ) ) ;
#6602 = CARTESIAN_POINT ( 'NONE',  ( 5.405949406249999534, 9.363379034771803333, -59.78125000204836681 ) ) ;
#6603 =( BOUNDED_CURVE ( )  B_SPLINE_CURVE ( 2, ( #19403, #35191, #2808, #28929, #32593, #35825, #38841 ),
 .UNSPECIFIED., .F., .F. ) 
 B_SPLINE_CURVE_WITH_KNOTS ( ( 3, 2, 2, 3 ),
 ( 0.5447761194029852039, 0.5460199004975125892, 0.5472636815920398634, 0.5485074626865672487 ),
 .UNSPECIFIED. ) 
 CURVE ( )  GEOMETRIC_REPRESENTATION_ITEM ( )  RATIONAL_B_SPLINE_CURVE ( ( 0.9999999999999880096, 0.8660254037844506980, 1.000000000000000000, 0.8660254037844387076, 1.000000000000000000, 0.8660254037844267172, 1.000000000000011990 ) ) 
 REPRESENTATION_ITEM ( '' )  );
#6604 = AXIS2_PLACEMENT_3D ( 'NONE', #29393, #9947, #36497 ) ;
#6605 = CARTESIAN_POINT ( 'NONE',  ( -9.999999999999998224, 5.773502691896259087, -60.25000000409677625 ) ) ;
#6606 = CARTESIAN_POINT ( 'NONE',  ( -5.405949406249996869, 9.363379034771805109, -18.84375000204835260 ) ) ;
#6607 = CARTESIAN_POINT ( 'NONE',  ( 9.999999999999998224, 0.000000000000000000, -38.37500000409676915 ) ) ;
#6608 = CARTESIAN_POINT ( 'NONE',  ( -5.405949406249996869, 9.363379034771805109, -184.0312500020484094 ) ) ;
#6609 = CARTESIAN_POINT ( 'NONE',  ( -5.405949406249996869, 9.363379034771805109, -14.53125000204835615 ) ) ;
#6610 = CARTESIAN_POINT ( 'NONE',  ( 9.999999999999998224, 0.000000000000000000, -85.99999999999998579 ) ) ;
#6611 = CARTESIAN_POINT ( 'NONE',  ( -9.999999999999742428, -5.773502691896402084, -161.6250000000000284 ) ) ;
#6612 = CIRCLE ( 'NONE', #30738, 10.00000000000000178 ) ;
#6613 = CARTESIAN_POINT ( 'NONE',  ( 7.070501591499376803E-16, 11.54700538379251284, -114.5000000040967905 ) ) ;
#6614 = CARTESIAN_POINT ( 'NONE',  ( -9.999999999999804601, 5.773502691896371886, -177.2500000040967905 ) ) ;
#6615 =( BOUNDED_CURVE ( )  B_SPLINE_CURVE ( 2, ( #20275, #17658, #36891, #4307, #4095, #21124, #37534 ),
 .UNSPECIFIED., .F., .F. ) 
 B_SPLINE_CURVE_WITH_KNOTS ( ( 3, 2, 2, 3 ),
 ( 0.3805970149253732338, 0.3818407960199006190, 0.3830845771144278933, 0.3843283582089552786 ),
 .UNSPECIFIED. ) 
 CURVE ( )  GEOMETRIC_REPRESENTATION_ITEM ( )  RATIONAL_B_SPLINE_CURVE ( ( 0.9999999999999880096, 0.8660254037844506980, 1.000000000000000000, 0.8660254037844387076, 1.000000000000000000, 0.8660254037844327124, 1.000000000000005995 ) ) 
 REPRESENTATION_ITEM ( '' )  );
#6616 = CARTESIAN_POINT ( 'NONE',  ( -5.000000000000003553, -8.660254037844383745, -170.5000000000000000 ) ) ;
#6618 = EDGE_LOOP ( 'NONE', ( #21421, #7789, #41950, #5568 ) ) ;
#6617 = CARTESIAN_POINT ( 'NONE',  ( 10.81189881249999907, 6.242252689847868297, -97.40625000204839523 ) ) ;
#6619 = CARTESIAN_POINT ( 'NONE',  ( 9.999999999998969713, 5.773502691896851502, -83.25000000409676204 ) ) ;
#6620 = EDGE_CURVE ( 'NONE', #27209, #10842, #20676, .T. ) ;
#6622 = ORIENTED_EDGE ( 'NONE', *, *, #37625, .F. ) ;
#6621 = CARTESIAN_POINT ( 'NONE',  ( 9.999999999999998224, 0.000000000000000000, -24.49999999999996447 ) ) ;
#6623 = ORIENTED_EDGE ( 'NONE', *, *, #18083, .T. ) ;
#6624 = CARTESIAN_POINT ( 'NONE',  ( -5.405949406250003975, -9.363379034771801557, -33.34375000204836681 ) ) ;
#6625 = CARTESIAN_POINT ( 'NONE',  ( 5.405949406249992428, -9.363379034771808662, -25.78125000204836681 ) ) ;
#6626 =( BOUNDED_CURVE ( )  B_SPLINE_CURVE ( 2, ( #15770, #39086, #25312, #2846, #5873, #32632, #12737 ),
 .UNSPECIFIED., .F., .F. ) 
 B_SPLINE_CURVE_WITH_KNOTS ( ( 3, 2, 2, 3 ),
 ( 0.1492537313432835966, 0.1504975124378109819, 0.1517412935323383116, 0.1529850746268656692 ),
 .UNSPECIFIED. ) 
 CURVE ( )  GEOMETRIC_REPRESENTATION_ITEM ( )  RATIONAL_B_SPLINE_CURVE ( ( 0.9999999999999970024, 0.8660254037844417052, 1.000000000000000000, 0.8660254037844387076, 1.000000000000000000, 0.8660254037844387076, 1.000000000000000000 ) ) 
 REPRESENTATION_ITEM ( '' )  );
#6627 = APPROVAL_DATE_TIME ( #16528, #32804 ) ;
#6628 = CARTESIAN_POINT ( 'NONE',  ( 10.81189881249999551, -6.242252689847874514, -74.96875000204838102 ) ) ;
#6629 = DIRECTION ( 'NONE',  ( 0.000000000000000000, 0.000000000000000000, -1.000000000000000000 ) ) ;
#6630 = CARTESIAN_POINT ( 'NONE',  ( 5.405949406249999534, 9.363379034771803333, -190.0937500020483810 ) ) ;
#6631 = AXIS2_PLACEMENT_3D ( 'NONE', #37693, #15007, #5532 ) ;
#6632 = CARTESIAN_POINT ( 'NONE',  ( 9.999999999999998224, 0.000000000000000000, -78.87500000409677625 ) ) ;
#6633 = DIRECTION ( 'NONE',  ( 1.000000000000000000, -0.000000000000000000, -0.000000000000000000 ) ) ;
#6634 = CARTESIAN_POINT ( 'NONE',  ( 10.81189881249999551, -6.242252689847874514, -153.1562500020484379 ) ) ;
#6635 = CARTESIAN_POINT ( 'NONE',  ( -4.999999999999996447, 8.660254037844387298, -3.375000004096767370 ) ) ;
#6636 = CARTESIAN_POINT ( 'NONE',  ( 9.999999999999998224, 0.000000000000000000, -179.0000000000000000 ) ) ;
#6637 = CARTESIAN_POINT ( 'NONE',  ( -5.405949406249996869, 9.363379034771805109, -117.8437500020483810 ) ) ;
#6638 = CARTESIAN_POINT ( 'NONE',  ( -5.405949406249996869, 9.363379034771805109, -100.0312500020483952 ) ) ;
#6639 = CARTESIAN_POINT ( 'NONE',  ( -5.405949406250003975, -9.363379034771801557, -108.3437500020483810 ) ) ;
#6640 = CARTESIAN_POINT ( 'NONE',  ( -10.81189881249999729, 6.242252689847871849, -78.71875000204838102 ) ) ;
#6641 = CARTESIAN_POINT ( 'NONE',  ( 10.81189881249999907, 6.242252689847868297, -80.90625000204839523 ) ) ;
#6642 = CARTESIAN_POINT ( 'NONE',  ( 5.000000000000000000, 8.660254037844385522, -164.1250000040967905 ) ) ;
#6643 = FACE_OUTER_BOUND ( 'NONE', #1005, .T. ) ;
#6644 = CARTESIAN_POINT ( 'NONE',  ( 5.405949406249992428, -9.363379034771808662, -163.7812500020484094 ) ) ;
#6645 = CARTESIAN_POINT ( 'NONE',  ( -10.81189881249999907, -6.242252689847864744, -183.6562500020483810 ) ) ;
#6646 = CARTESIAN_POINT ( 'NONE',  ( 7.070501591499377789E-16, 11.54700538379251284, -155.0000000040968189 ) ) ;
#6647 = DIRECTION ( 'NONE',  ( -0.000000000000000000, -0.000000000000000000, -1.000000000000000000 ) ) ;
#6648 = CARTESIAN_POINT ( 'NONE',  ( 10.81189881249999551, -6.242252689847874514, -2.968750002048353931 ) ) ;
#6649 = CARTESIAN_POINT ( 'NONE',  ( -9.999999999999998224, 1.224646799147353059E-15, -54.12500000409675494 ) ) ;
#6650 = CARTESIAN_POINT ( 'NONE',  ( -10.81189881249999729, 6.242252689847871849, -111.7187500020483810 ) ) ;
#6651 = CARTESIAN_POINT ( 'NONE',  ( -9.999999999999998224, 5.773502691896259087, -77.87499999999998579 ) ) ;
#6652 = CARTESIAN_POINT ( 'NONE',  ( 7.644554776091147741E-16, 12.48450537969573659, -10.15625000204836681 ) ) ;
#6653 = CARTESIAN_POINT ( 'NONE',  ( 9.999999999999996447, -5.773502691896262640, -94.00000000409677625 ) ) ;
#6654 = CARTESIAN_POINT ( 'NONE',  ( 0.000000000000000000, 0.000000000000000000, -200.0000000000000000 ) ) ;
#6655 = CARTESIAN_POINT ( 'NONE',  ( -2.293366432827344421E-15, -12.48450537969573659, -106.9062500020483952 ) ) ;
#6656 = CARTESIAN_POINT ( 'NONE',  ( -5.405949406250003975, -9.363379034771801557, -93.53125000204838102 ) ) ;
#6657 = EDGE_LOOP ( 'NONE', ( #21542, #13231, #19181, #40618 ) ) ;
#6658 = CARTESIAN_POINT ( 'NONE',  ( 10.00000000000000000, 5.773502691896255534, -80.25000000409679046 ) ) ;
#6659 = CARTESIAN_POINT ( 'NONE',  ( -4.999999999999996447, 8.660254037844387298, -47.99999999999998579 ) ) ;
#6660 = CARTESIAN_POINT ( 'NONE',  ( -10.81189881249999729, 6.242252689847871849, -44.21875000204836681 ) ) ;
#6661 = VERTEX_POINT ( 'NONE', #9555 ) ;
#6662 = CARTESIAN_POINT ( 'NONE',  ( 10.00000000000000000, 5.773502691896255534, -12.37499999999996270 ) ) ;
#6663 = CARTESIAN_POINT ( 'NONE',  ( -9.999999999999998224, 5.773502691896259087, -142.3750000000000000 ) ) ;
#6664 = CARTESIAN_POINT ( 'NONE',  ( -2.121150477449813534E-15, -11.54700538379251284, -32.37499999999995737 ) ) ;
#6665 = CARTESIAN_POINT ( 'NONE',  ( 10.00000000000000000, 5.773502691896255534, -12.75000000409676204 ) ) ;
#6666 = CARTESIAN_POINT ( 'NONE',  ( -5.000000000000003553, -8.660254037844383745, -190.0000000000000000 ) ) ;
#6668 = ORIENTED_EDGE ( 'NONE', *, *, #13828, .F. ) ;
#6667 = CARTESIAN_POINT ( 'NONE',  ( 5.405949406249992428, -9.363379034771808662, -117.2812500020483952 ) ) ;
#6669 = CARTESIAN_POINT ( 'NONE',  ( 0.000000000000000000, 0.000000000000000000, -200.0000000000000000 ) ) ;
#6670 = ADVANCED_FACE ( 'NONE', ( #32455 ), #32661, .F. ) ;
#6671 = EDGE_CURVE ( 'NONE', #3950, #37390, #29514, .T. ) ;
#6672 = ORIENTED_EDGE ( 'NONE', *, *, #24644, .T. ) ;
#6673 = EDGE_CURVE ( 'NONE', #9647, #31274, #39709, .T. ) ;
#6674 = CARTESIAN_POINT ( 'NONE',  ( 10.81189881249999551, -6.242252689847874514, -45.15625000204836681 ) ) ;
#6675 = SECURITY_CLASSIFICATION_LEVEL ( 'unclassified' ) ;
#6676 = CARTESIAN_POINT ( 'NONE',  ( 10.81189881249999551, -6.242252689847874514, -91.46875000204838102 ) ) ;
#6677 = CARTESIAN_POINT ( 'NONE',  ( 10.81189881249999551, -6.242252689847874514, -123.1562500020483952 ) ) ;
#6678 = ORIENTED_EDGE ( 'NONE', *, *, #8111, .F. ) ;
#6679 = CARTESIAN_POINT ( 'NONE',  ( -8.265208957352971163E-15, -145.0000000000000000, 7.499999999999980460 ) ) ;
#6680 = CARTESIAN_POINT ( 'NONE',  ( -10.81189881249999907, -6.242252689847864744, -180.6562500020484094 ) ) ;
#6681 = CARTESIAN_POINT ( 'NONE',  ( -9.999999999999998224, 1.224646799147353059E-15, -0.1250000040967647053 ) ) ;
#6682 = ADVANCED_FACE ( 'NONE', ( #4559 ), #23777, .T. ) ;
#6683 = CARTESIAN_POINT ( 'NONE',  ( -5.405949406249996869, 9.363379034771805109, -131.3437500020484094 ) ) ;
#6684 =( BOUNDED_CURVE ( )  B_SPLINE_CURVE ( 2, ( #33302, #38914, #42556, #284, #19896, #29416, #6116 ),
 .UNSPECIFIED., .F., .F. ) 
 B_SPLINE_CURVE_WITH_KNOTS ( ( 3, 2, 2, 3 ),
 ( 0.3955223880597015795, 0.3967661691542289648, 0.3980099502487563501, 0.3992537313432836799 ),
 .UNSPECIFIED. ) 
 CURVE ( )  GEOMETRIC_REPRESENTATION_ITEM ( )  RATIONAL_B_SPLINE_CURVE ( ( 0.9999999999999880096, 0.8660254037844506980, 1.000000000000000000, 0.8660254037844387076, 1.000000000000000000, 0.8660254037844267172, 1.000000000000011990 ) ) 
 REPRESENTATION_ITEM ( '' )  );
#6685 = CARTESIAN_POINT ( 'NONE',  ( 10.81189881249999551, -6.242252689847874514, -98.96875000204838102 ) ) ;
#6686 = LINE ( 'NONE', #36256, #2200 ) ;
#6687 = CARTESIAN_POINT ( 'NONE',  ( 5.405949406249999534, 9.363379034771803333, -110.7812500020483810 ) ) ;
#6688 = CARTESIAN_POINT ( 'NONE',  ( 9.999999999999998224, 0.000000000000000000, -182.3750000040967905 ) ) ;
#6689 = CARTESIAN_POINT ( 'NONE',  ( -10.81189881249999729, 6.242252689847871849, -114.7187500020483810 ) ) ;
#6690 = CARTESIAN_POINT ( 'NONE',  ( 10.81189881249999729, 0.000000000000000000, -183.0312500020484094 ) ) ;
#6691 = LINE ( 'NONE', #23312, #24083 ) ;
#6692 = CARTESIAN_POINT ( 'NONE',  ( 5.000000000000000000, 8.660254037844385522, -185.1250000040967905 ) ) ;
#6693 = CARTESIAN_POINT ( 'NONE',  ( 5.000000000000000000, 8.660254037844385522, -132.2499999999999716 ) ) ;
#6694 = CARTESIAN_POINT ( 'NONE',  ( -5.000000000000003553, -8.660254037844383745, -3.999999999999976019 ) ) ;
#6695 = ADVANCED_FACE ( 'NONE', ( #23358 ), #7585, .T. ) ;
#6696 = CARTESIAN_POINT ( 'NONE',  ( 10.81189881249999729, 0.000000000000000000, -56.84375000204835970 ) ) ;
#6697 = CARTESIAN_POINT ( 'NONE',  ( 10.81189881249999729, 0.000000000000000000, -46.34375000204838102 ) ) ;
#6698 = CARTESIAN_POINT ( 'NONE',  ( -2.121150477449813534E-15, -11.54700538379251284, -178.2500000040967620 ) ) ;
#6699 = CARTESIAN_POINT ( 'NONE',  ( -5.405949406249996869, 9.363379034771805109, -17.53125000204835970 ) ) ;
#6700 = CARTESIAN_POINT ( 'NONE',  ( 10.81189881249999907, 6.242252689847868297, -28.21875000204838102 ) ) ;
#6701 = CARTESIAN_POINT ( 'NONE',  ( -10.00000000000154188, 5.773502691895366468, -27.25000000409673007 ) ) ;
#6702 = CARTESIAN_POINT ( 'NONE',  ( -5.405949406249996869, 9.363379034771805109, -140.3437500020484094 ) ) ;
#6703 = CARTESIAN_POINT ( 'NONE',  ( -10.00000000000000000, -5.773502691896251982, -103.1249999999999858 ) ) ;
#6704 = CARTESIAN_POINT ( 'NONE',  ( 10.81189881249999551, -6.242252689847874514, -33.15625000204835970 ) ) ;
#6705 = EDGE_CURVE ( 'NONE', #39621, #31210, #33928, .T. ) ;
#6706 = DIRECTION ( 'NONE',  ( -0.000000000000000000, -0.000000000000000000, -1.000000000000000000 ) ) ;
#6707 = CARTESIAN_POINT ( 'NONE',  ( 5.000000000000000000, 8.660254037844385522, -66.24999999999997158 ) ) ;
#6708 = CARTESIAN_POINT ( 'NONE',  ( -10.81189881249999907, -6.242252689847864744, -129.6562500020483810 ) ) ;
#6709 = CARTESIAN_POINT ( 'NONE',  ( -10.81189881249999729, 1.324075727343319199E-15, -119.2812500020483952 ) ) ;
#6710 = ORIENTED_EDGE ( 'NONE', *, *, #33868, .F. ) ;
#6711 = CARTESIAN_POINT ( 'NONE',  ( 7.070501591499376803E-16, 11.54700538379251284, -160.6250000000000284 ) ) ;
#6712 = CARTESIAN_POINT ( 'NONE',  ( -9.999999999999998224, 1.224646799147353059E-15, -111.1250000040967763 ) ) ;
#6713 = CARTESIAN_POINT ( 'NONE',  ( 4.999999999999992006, -8.660254037844389075, -194.6250000040967905 ) ) ;
#6714 = CARTESIAN_POINT ( 'NONE',  ( -2.293366432827344421E-15, -12.48450537969573659, -63.21875000204838102 ) ) ;
#6715 = VERTEX_POINT ( 'NONE', #16848 ) ;
#6716 = CARTESIAN_POINT ( 'NONE',  ( -5.000000000000003553, -8.660254037844383745, -33.99999999999997158 ) ) ;
#6717 = CARTESIAN_POINT ( 'NONE',  ( -4.999999999999996447, 8.660254037844387298, -19.87500000409675494 ) ) ;
#6718 = CARTESIAN_POINT ( 'NONE',  ( 7.644554776091147741E-16, 12.48450537969573659, -47.65625000204836681 ) ) ;
#6719 = ADVANCED_FACE ( 'NONE', ( #33708 ), #36717, .T. ) ;
#6720 = FACE_OUTER_BOUND ( 'NONE', #27467, .T. ) ;
#6721 = CARTESIAN_POINT ( 'NONE',  ( 7.070501591499377789E-16, 11.54700538379251284, -39.50000000409675494 ) ) ;
#6722 = CARTESIAN_POINT ( 'NONE',  ( -9.999999999999998224, 1.224646799147353059E-15, -166.2500000000000000 ) ) ;
#6723 = CARTESIAN_POINT ( 'NONE',  ( -2.293366432827344421E-15, -12.48450537969573659, -144.4062500020484094 ) ) ;
#6724 = CARTESIAN_POINT ( 'NONE',  ( -9.999999999999998224, 1.224646799147353059E-15, -42.12500000409677625 ) ) ;
#6725 = ORIENTED_EDGE ( 'NONE', *, *, #29092, .T. ) ;
#6726 = ORIENTED_EDGE ( 'NONE', *, *, #11274, .T. ) ;
#6727 = VERTEX_POINT ( 'NONE', #27440 ) ;
#6728 = CARTESIAN_POINT ( 'NONE',  ( -5.000000000000003553, -8.660254037844383745, -130.0000000000000000 ) ) ;
#6729 =( BOUNDED_CURVE ( )  B_SPLINE_CURVE ( 2, ( #33980, #41057, #36989, #4402, #7862, #30743, #40849 ),
 .UNSPECIFIED., .F., .F. ) 
 B_SPLINE_CURVE_WITH_KNOTS ( ( 3, 2, 2, 3 ),
 ( 0.7798507462686569136, 0.7810945273631842989, 0.7823383084577115731, 0.7835820895522389584 ),
 .UNSPECIFIED. ) 
 CURVE ( )  GEOMETRIC_REPRESENTATION_ITEM ( )  RATIONAL_B_SPLINE_CURVE ( ( 0.9999999999999761302, 0.8660254037844625774, 1.000000000000000000, 0.8660254037844387076, 1.000000000000000000, 0.8660254037844267172, 1.000000000000011990 ) ) 
 REPRESENTATION_ITEM ( '' )  );
#6730 = CARTESIAN_POINT ( 'NONE',  ( -10.81189881249999729, 1.324075727343319199E-15, -177.5937500020484094 ) ) ;
#6731 = CARTESIAN_POINT ( 'NONE',  ( 5.405949406249999534, 9.363379034771803333, -25.09375000204835970 ) ) ;
#6732 = AXIS2_PLACEMENT_3D ( 'NONE', #27869, #14682, #34567 ) ;
#6733 = CARTESIAN_POINT ( 'NONE',  ( 10.81189881249999729, 0.000000000000000000, -152.8437500020483810 ) ) ;
#6734 = VECTOR ( 'NONE', #38055, 1000.000000000000000 ) ;
#6735 = CARTESIAN_POINT ( 'NONE',  ( -5.405949406249996869, 9.363379034771805109, -144.8437500020483810 ) ) ;
#6736 = LINE ( 'NONE', #6526, #32129 ) ;
#6737 = CARTESIAN_POINT ( 'NONE',  ( -10.81189881249999729, 1.324075727343319199E-15, -125.0937500020483668 ) ) ;
#6738 = CARTESIAN_POINT ( 'NONE',  ( -5.405949406249996869, 9.363379034771805109, -130.0312500020484094 ) ) ;
#6739 = CARTESIAN_POINT ( 'NONE',  ( -10.81189881249999729, 1.324075727343319199E-15, -18.59375000204835260 ) ) ;
#6741 = ADVANCED_FACE ( 'NONE', ( #7374 ), #34140, .T. ) ;
#6740 = CARTESIAN_POINT ( 'NONE',  ( 10.81189881249999551, -6.242252689847874514, -140.9687500020483810 ) ) ;
#6742 = DIRECTION ( 'NONE',  ( -1.000000000000000000, 0.000000000000000000, 0.000000000000000000 ) ) ;
#6743 = LINE ( 'NONE', #29846, #22016 ) ;
#6744 = CARTESIAN_POINT ( 'NONE',  ( 7.070501591499377789E-16, 11.54700538379251284, -160.6250000000000284 ) ) ;
#6745 = CARTESIAN_POINT ( 'NONE',  ( -10.00000000000102496, 5.773502691895664007, -55.75000000409674072 ) ) ;
#6746 = CARTESIAN_POINT ( 'NONE',  ( -5.405949406249996869, 9.363379034771805109, -75.84375000204838102 ) ) ;
#6747 = CARTESIAN_POINT ( 'NONE',  ( -10.81189881249999729, 1.324075727343319199E-15, -44.28125000204838102 ) ) ;
#6748 = CARTESIAN_POINT ( 'NONE',  ( 5.405949406249992428, -9.363379034771808662, -57.09375000204835970 ) ) ;
#6749 = CARTESIAN_POINT ( 'NONE',  ( -10.81189881249999729, 6.242252689847871849, -164.2187500020483810 ) ) ;
#6750 = CARTESIAN_POINT ( 'NONE',  ( -9.999999999999998224, 5.773502691896259087, -131.8749999999999716 ) ) ;
#6751 = CARTESIAN_POINT ( 'NONE',  ( 10.81189881249999551, -6.242252689847874514, -135.1562500020483810 ) ) ;
#6752 = CARTESIAN_POINT ( 'NONE',  ( -1.040834085586084257E-14, 125.0000000000000000, 12.74999999999998934 ) ) ;
#6753 = CARTESIAN_POINT ( 'NONE',  ( 9.999999999999996447, -5.773502691896262640, -113.5000000040967763 ) ) ;
#6754 = CARTESIAN_POINT ( 'NONE',  ( -9.999999999999998224, 1.224646799147353059E-15, -92.74999999999998579 ) ) ;
#6755 = EDGE_LOOP ( 'NONE', ( #7989, #39422, #27911, #36759 ) ) ;
#6756 = CARTESIAN_POINT ( 'NONE',  ( 10.81189881249999729, 6.242252689847867408, -112.4062500020483952 ) ) ;
#6757 = CARTESIAN_POINT ( 'NONE',  ( 4.999999999999992006, -8.660254037844389075, -133.1250000040967620 ) ) ;
#6758 = CARTESIAN_POINT ( 'NONE',  ( 9.999999999999998224, 0.000000000000000000, -111.4999999999999858 ) ) ;
#6759 = CARTESIAN_POINT ( 'NONE',  ( 5.405949406249992428, -9.363379034771808662, -163.7812500020484094 ) ) ;
#6760 = CARTESIAN_POINT ( 'NONE',  ( 4.999999999999992006, -8.660254037844389075, -40.12500000409676915 ) ) ;
#6761 = CARTESIAN_POINT ( 'NONE',  ( 9.999999999999998224, 0.000000000000000000, -26.37500000409676204 ) ) ;
#6762 = CARTESIAN_POINT ( 'NONE',  ( 5.405949406249992428, -9.363379034771808662, -52.78125000204836681 ) ) ;
#6763 = DIRECTION ( 'NONE',  ( 1.000000000000000000, 0.000000000000000000, 0.000000000000000000 ) ) ;
#6764 = CARTESIAN_POINT ( 'NONE',  ( 10.81189881249999729, 0.000000000000000000, -162.0312500020484094 ) ) ;
#6765 = CARTESIAN_POINT ( 'NONE',  ( 7.644554776091147741E-16, 12.48450537969573659, -131.4687500020483810 ) ) ;
#6766 = CARTESIAN_POINT ( 'NONE',  ( -9.999999999999998224, 1.224646799147353059E-15, -200.0000000000000000 ) ) ;
#6767 = CARTESIAN_POINT ( 'NONE',  ( 9.999999999999998224, 0.000000000000000000, -174.5000000000000284 ) ) ;
#6768 = VECTOR ( 'NONE', #16694, 1000.000000000000000 ) ;
#6769 = EDGE_LOOP ( 'NONE', ( #11755, #31426, #30833, #8115 ) ) ;
#6770 = CARTESIAN_POINT ( 'NONE',  ( 4.999999999999992006, -8.660254037844389075, -30.74999999999997158 ) ) ;
#6772 = ORIENTED_EDGE ( 'NONE', *, *, #9853, .F. ) ;
#6771 = CARTESIAN_POINT ( 'NONE',  ( -10.81189881249999729, 1.324075727343319199E-15, -71.28125000204838102 ) ) ;
#6773 = DIRECTION ( 'NONE',  ( 1.000000000000000000, 0.000000000000000000, 0.000000000000000000 ) ) ;
#6775 = ORIENTED_EDGE ( 'NONE', *, *, #56, .T. ) ;
#6774 = CARTESIAN_POINT ( 'NONE',  ( 10.81189881249999907, 6.242252689847868297, -119.7187500020483810 ) ) ;
#6776 = VERTEX_POINT ( 'NONE', #14023 ) ;
#6777 = CARTESIAN_POINT ( 'NONE',  ( -10.81189881249999729, -6.242252689847864744, -21.46875000204837036 ) ) ;
#6778 = CARTESIAN_POINT ( 'NONE',  ( -10.81189881249999729, 1.324075727343319199E-15, -197.0937500020484094 ) ) ;
#6779 = SHAPE_REPRESENTATION ( 'reaction body', ( #39998 ), #29026 ) ;
#6781 = EDGE_CURVE ( 'NONE', #26104, #20093, #20309, .T. ) ;
#6780 = CARTESIAN_POINT ( 'NONE',  ( -10.81189881249999729, 1.324075727343319199E-15, -48.59375000204838102 ) ) ;
#6782 = FACE_OUTER_BOUND ( 'NONE', #28411, .T. ) ;
#6783 = CARTESIAN_POINT ( 'NONE',  ( 7.070501591499377789E-16, 11.54700538379251284, -30.12499999999995737 ) ) ;
#6784 = CARTESIAN_POINT ( 'NONE',  ( -10.81189881249999729, 1.324075727343319199E-15, -183.5937500020483810 ) ) ;
#6785 = CARTESIAN_POINT ( 'NONE',  ( 5.405949406249992428, -9.363379034771808662, -169.5937500020484094 ) ) ;
#6786 = CARTESIAN_POINT ( 'NONE',  ( 10.81189881249999551, -6.242252689847874514, -146.9687500020484094 ) ) ;
#6787 = CARTESIAN_POINT ( 'NONE',  ( -10.81189881249999729, -6.242252689847864744, -160.9687500020484094 ) ) ;
#6788 = CARTESIAN_POINT ( 'NONE',  ( 9.999999999999998224, 0.000000000000000000, -117.8750000040967905 ) ) ;
#6789 = DIRECTION ( 'NONE',  ( -0.000000000000000000, -0.000000000000000000, 1.000000000000000000 ) ) ;
#6790 = CARTESIAN_POINT ( 'NONE',  ( 9.999999999999996447, -5.773502691896262640, -186.6250000000000284 ) ) ;
#6791 = CARTESIAN_POINT ( 'NONE',  ( 10.81189881249999907, 6.242252689847868297, -98.71875000204838102 ) ) ;
#6792 = CARTESIAN_POINT ( 'NONE',  ( -9.999999999999998224, 1.224646799147353059E-15, -101.7500000000000000 ) ) ;
#6793 = CARTESIAN_POINT ( 'NONE',  ( 10.81189881249999729, 0.000000000000000000, -64.53125000204836681 ) ) ;
#6794 = CARTESIAN_POINT ( 'NONE',  ( 9.999999999999998224, 0.000000000000000000, -96.87500000409677625 ) ) ;
#6795 = CARTESIAN_POINT ( 'NONE',  ( -10.81189881249999729, 1.324075727343319199E-15, -186.5937500020483810 ) ) ;
#6796 = CARTESIAN_POINT ( 'NONE',  ( 10.81189881249999729, 0.000000000000000000, -123.0312500020483952 ) ) ;
#6797 = VECTOR ( 'NONE', #10559, 1000.000000000000000 ) ;
#6798 = CARTESIAN_POINT ( 'NONE',  ( -5.405949406250003975, -9.363379034771801557, -165.5312500020484094 ) ) ;
#6799 = PERSON ( 'NAUO-PER5', 'UNSPECIFIED', 'UNSPECIFIED', ('UNSPECIFIED'), ('UNSPECIFIED'), ('UNSPECIFIED') ) ;
#6800 = CARTESIAN_POINT ( 'NONE',  ( 7.644554776091147741E-16, 12.48450537969573659, -55.15625000204838102 ) ) ;
#6801 = CARTESIAN_POINT ( 'NONE',  ( 7.070501591499377789E-16, 11.54700538379251284, -140.0000000040968189 ) ) ;
#6802 = CARTESIAN_POINT ( 'NONE',  ( 7.070501591499377789E-16, 11.54700538379251284, -115.6249999999999858 ) ) ;
#6803 = ADVANCED_FACE ( 'NONE', ( #40578 ), #33925, .T. ) ;
#6804 = ORIENTED_EDGE ( 'NONE', *, *, #15885, .T. ) ;
#6805 = CARTESIAN_POINT ( 'NONE',  ( -10.81189881249999729, 1.324075727343319199E-15, -134.2812500020483810 ) ) ;
#6806 = CARTESIAN_POINT ( 'NONE',  ( 7.644554776091147741E-16, 12.48450537969573659, -149.6562500020484094 ) ) ;
#6807 = CARTESIAN_POINT ( 'NONE',  ( 10.81189881249999551, -6.242252689847874514, -186.1562500020484379 ) ) ;
#6808 = CARTESIAN_POINT ( 'NONE',  ( 9.999999999999998224, 0.000000000000000000, -200.0000000000000000 ) ) ;
#6809 = CARTESIAN_POINT ( 'NONE',  ( -5.405949406250003975, -9.363379034771801557, -82.84375000204836681 ) ) ;
#6810 = VERTEX_POINT ( 'NONE', #7157 ) ;
#6811 = CARTESIAN_POINT ( 'NONE',  ( -9.999999999999998224, 5.773502691896259087, -59.87499999999999289 ) ) ;
#6812 = CARTESIAN_POINT ( 'NONE',  ( -2.293366432827344421E-15, -12.48450537969573659, -187.7187500020484094 ) ) ;
#6813 = CARTESIAN_POINT ( 'NONE',  ( -9.999999999999998224, 1.224646799147353059E-15, -64.62500000409676204 ) ) ;
#6814 = CARTESIAN_POINT ( 'NONE',  ( 9.999999999998456346, 5.773502691897149042, -21.75000000409673007 ) ) ;
#6815 = CARTESIAN_POINT ( 'NONE',  ( 0.000000000000000000, 0.000000000000000000, -200.0000000000000000 ) ) ;
#6816 = CARTESIAN_POINT ( 'NONE',  ( 5.405949406249992428, -9.363379034771808662, -84.28125000204838102 ) ) ;
#6817 = CARTESIAN_POINT ( 'NONE',  ( 10.81189881249999551, -6.242252689847874514, -58.65625000204837391 ) ) ;
#6818 = CARTESIAN_POINT ( 'NONE',  ( -5.000000000000003553, -8.660254037844383745, -62.87500000409676204 ) ) ;
#6819 = CARTESIAN_POINT ( 'NONE',  ( 10.81189881249999907, 6.242252689847868297, -19.21875000204836681 ) ) ;
#6820 = CARTESIAN_POINT ( 'NONE',  ( 0.000000000000000000, 0.000000000000000000, -200.0000000000000000 ) ) ;
#6821 = CARTESIAN_POINT ( 'NONE',  ( 10.81189881249999729, 0.000000000000000000, -189.0312500020484094 ) ) ;
#6822 = CARTESIAN_POINT ( 'NONE',  ( -10.81189881249999729, 1.324075727343319199E-15, -15.78125000204835793 ) ) ;
#6823 = DIRECTION ( 'NONE',  ( -0.000000000000000000, -0.000000000000000000, 1.000000000000000000 ) ) ;
#6824 = CARTESIAN_POINT ( 'NONE',  ( -9.433396038363706992, 3.431119748995231422, -0.000000000000000000 ) ) ;
#6825 = CARTESIAN_POINT ( 'NONE',  ( 5.000000000000000000, 8.660254037844385522, -169.7500000000000000 ) ) ;
#6826 = CARTESIAN_POINT ( 'NONE',  ( 9.999999999999994671, -5.773502691896262640, -137.5000000040967905 ) ) ;
#6828 = ORIENTED_EDGE ( 'NONE', *, *, #3873, .T. ) ;
#6827 = CARTESIAN_POINT ( 'NONE',  ( 7.644554776091147741E-16, 12.48450537969573659, -91.15625000204838102 ) ) ;
#6829 = CARTESIAN_POINT ( 'NONE',  ( 9.999999999999998224, 0.000000000000000000, -107.3750000040967763 ) ) ;
#6831 = VERTEX_POINT ( 'NONE', #40159 ) ;
#6830 = CARTESIAN_POINT ( 'NONE',  ( -9.999999999999998224, 1.224646799147353059E-15, -161.7500000000000000 ) ) ;
#6832 = EDGE_LOOP ( 'NONE', ( #14825, #22223, #19986, #23822 ) ) ;
#6833 = EDGE_CURVE ( 'NONE', #1591, #19597, #32, .T. ) ;
#6834 = CARTESIAN_POINT ( 'NONE',  ( -5.405949406249996869, 9.363379034771805109, -32.34375000204836681 ) ) ;
#6835 = CARTESIAN_POINT ( 'NONE',  ( 10.81189881249999551, -6.242252689847874514, -24.15625000204838102 ) ) ;
#6836 = ITEM_DEFINED_TRANSFORMATION ( 'NONE', 'NONE', #26949,  #39998 ) ;
#6837 = VECTOR ( 'NONE', #13942, 1000.000000000000000 ) ;
#6838 = CARTESIAN_POINT ( 'NONE',  ( -2.293366432827344421E-15, -12.48450537969573659, -69.21875000204839523 ) ) ;
#6839 = FACE_OUTER_BOUND ( 'NONE', #22128, .T. ) ;
#6840 = CARTESIAN_POINT ( 'NONE',  ( -10.81189881249999907, -6.242252689847864744, -189.4687500020484094 ) ) ;
#6841 = CARTESIAN_POINT ( 'NONE',  ( 7.644554776091147741E-16, 12.48450537969573659, -149.4687500020484094 ) ) ;
#6842 = DIRECTION ( 'NONE',  ( -0.000000000000000000, -0.000000000000000000, -1.000000000000000000 ) ) ;
#6843 = CIRCLE ( 'NONE', #42657, 5.000000000000002665 ) ;
#6844 = CARTESIAN_POINT ( 'NONE',  ( -4.999999999999996447, 8.660254037844387298, -112.4999999999999858 ) ) ;
#6845 = CARTESIAN_POINT ( 'NONE',  ( -5.405949406249996869, 9.363379034771805109, -148.0312500020483810 ) ) ;
#6846 = CARTESIAN_POINT ( 'NONE',  ( 9.999999999999998224, 0.000000000000000000, -5.375000004096769146 ) ) ;
#6847 = CARTESIAN_POINT ( 'NONE',  ( 9.999999999999998224, 0.000000000000000000, -125.0000000000000000 ) ) ;
#6848 = CARTESIAN_POINT ( 'NONE',  ( -5.405949406250003975, -9.363379034771801557, -117.3437500020483810 ) ) ;
#6849 = CARTESIAN_POINT ( 'NONE',  ( 9.999999999999479527, 5.773502691896553074, -109.8749999999999716 ) ) ;
#6850 = CARTESIAN_POINT ( 'NONE',  ( 10.81189881249999907, 6.242252689847868297, -89.90625000204839523 ) ) ;
#6851 = CARTESIAN_POINT ( 'NONE',  ( -5.405949406250003975, -9.363379034771801557, -106.8437500020483810 ) ) ;
#6852 = CARTESIAN_POINT ( 'NONE',  ( -2.293366432827344421E-15, -12.48450537969573659, -67.71875000204838102 ) ) ;
#6853 = CARTESIAN_POINT ( 'NONE',  ( 10.81189881249999551, -6.242252689847874514, -78.15625000204838102 ) ) ;
#6854 = CARTESIAN_POINT ( 'NONE',  ( -9.999999999999998224, 5.773502691896259087, -165.2500000040967905 ) ) ;
#6855 =( BOUNDED_CURVE ( )  B_SPLINE_CURVE ( 2, ( #3606, #6619, #36603, #19985, #29720, #23455, #23669 ),
 .UNSPECIFIED., .F., .F. ) 
 B_SPLINE_CURVE_WITH_KNOTS ( ( 3, 2, 2, 3 ),
 ( 0.5746268656716420065, 0.5758706467661693917, 0.5771144278606968880, 0.5783582089552241623 ),
 .UNSPECIFIED. ) 
 CURVE ( )  GEOMETRIC_REPRESENTATION_ITEM ( )  RATIONAL_B_SPLINE_CURVE ( ( 0.9999999999999761302, 0.8660254037844625774, 1.000000000000000000, 0.8660254037844387076, 1.000000000000000000, 0.8660254037844028474, 1.000000000000035971 ) ) 
 REPRESENTATION_ITEM ( '' )  );
#6856 = DIRECTION ( 'NONE',  ( -1.000000000000000000, 0.000000000000000000, -0.000000000000000000 ) ) ;
#6857 = CARTESIAN_POINT ( 'NONE',  ( -10.81189881249999729, 1.324075727343319199E-15, -168.7812500020484094 ) ) ;
#6858 = CARTESIAN_POINT ( 'NONE',  ( -5.405949406250003975, -9.363379034771801557, -182.0312500020483810 ) ) ;
#6859 = CARTESIAN_POINT ( 'NONE',  ( 0.000000000000000000, 0.000000000000000000, -99.99999999999998579 ) ) ;
#6860 = CARTESIAN_POINT ( 'NONE',  ( 10.81189881249999729, 0.000000000000000000, -2.843750002048367698 ) ) ;
#6861 = CARTESIAN_POINT ( 'NONE',  ( 10.00000000000051159, -5.773502691895965988, -149.1249999999999716 ) ) ;
#6862 = CARTESIAN_POINT ( 'NONE',  ( -10.81189881249999729, 1.324075727343319199E-15, -114.5937500020483810 ) ) ;
#6863 = EDGE_CURVE ( 'NONE', #25211, #17989, #19820, .T. ) ;
#6864 = CARTESIAN_POINT ( 'NONE',  ( -9.999999999999998224, 5.773502691896259087, -79.37500000000000000 ) ) ;
#6865 = CARTESIAN_POINT ( 'NONE',  ( -10.81189881249999907, -6.242252689847864744, -9.656250002048366810 ) ) ;
#6866 = CARTESIAN_POINT ( 'NONE',  ( 9.999999999999998224, 0.000000000000000000, -90.87500000409677625 ) ) ;
#6867 = CARTESIAN_POINT ( 'NONE',  ( -9.999999999999998224, 1.224646799147353059E-15, -150.1250000040967905 ) ) ;
#6868 = CARTESIAN_POINT ( 'NONE',  ( -2.293366432827344421E-15, -12.48450537969573659, -105.4062500020483810 ) ) ;
#6869 = CARTESIAN_POINT ( 'NONE',  ( 7.644554776091147741E-16, 12.48450537969573659, -85.15625000204838102 ) ) ;
#6870 = ORIENTED_EDGE ( 'NONE', *, *, #23177, .T. ) ;
#6871 = CARTESIAN_POINT ( 'NONE',  ( 4.999999999999992006, -8.660254037844389075, -83.62500000409677625 ) ) ;
#6872 = CARTESIAN_POINT ( 'NONE',  ( -9.999999999999998224, 1.224646799147353059E-15, -154.2500000000000000 ) ) ;
#6873 = CARTESIAN_POINT ( 'NONE',  ( 5.405949406249999534, 9.363379034771803333, -46.09375000204838102 ) ) ;
#6874 = VERTEX_POINT ( 'NONE', #27652 ) ;
#6875 = CARTESIAN_POINT ( 'NONE',  ( -4.999999999999996447, 8.660254037844387298, -11.99999999999995559 ) ) ;
#6876 = CIRCLE ( 'NONE', #24103, 5.500000000000003553 ) ;
#6877 = CARTESIAN_POINT ( 'NONE',  ( 4.999999999999992006, -8.660254037844389075, -144.7500000000000000 ) ) ;
#6878 = FACE_OUTER_BOUND ( 'NONE', #22429, .T. ) ;
#6879 = CARTESIAN_POINT ( 'NONE',  ( -5.000000000000003553, -8.660254037844383745, -13.37500000409674783 ) ) ;
#6880 = CARTESIAN_POINT ( 'NONE',  ( 10.00000000000000000, 5.773502691896255534, -187.8750000000000568 ) ) ;
#6881 = LINE ( 'NONE', #39673, #10980 ) ;
#6883 = ORIENTED_EDGE ( 'NONE', *, *, #4462, .F. ) ;
#6882 = CARTESIAN_POINT ( 'NONE',  ( 10.81189881249999729, 0.000000000000000000, -121.5312500020483952 ) ) ;
#6884 = DIRECTION ( 'NONE',  ( -0.000000000000000000, -0.000000000000000000, 1.000000000000000000 ) ) ;
#6885 = VERTEX_POINT ( 'NONE', #40793 ) ;
#6886 = CARTESIAN_POINT ( 'NONE',  ( -10.81189881249999907, -6.242252689847864744, -48.65625000204836681 ) ) ;
#6887 = COORDINATED_UNIVERSAL_TIME_OFFSET ( 6, 0, .AHEAD. ) ;
#6888 = CARTESIAN_POINT ( 'NONE',  ( 5.405949406249992428, -9.363379034771808662, -97.59375000204838102 ) ) ;
#6889 = CARTESIAN_POINT ( 'NONE',  ( 5.405949406249992428, -9.363379034771808662, -123.2812500020483952 ) ) ;
#6890 = ORIENTED_EDGE ( 'NONE', *, *, #8772, .T. ) ;
#6891 = CARTESIAN_POINT ( 'NONE',  ( 4.999999999999992006, -8.660254037844389075, -111.7499999999999858 ) ) ;
#6892 = DIRECTION ( 'NONE',  ( -0.000000000000000000, -0.000000000000000000, 1.000000000000000000 ) ) ;
#6893 = CARTESIAN_POINT ( 'NONE',  ( -10.81189881249999729, 6.242252689847871849, -176.4062500020484094 ) ) ;
#6894 = DIRECTION ( 'NONE',  ( 1.000000000000000000, 0.000000000000000000, 0.000000000000000000 ) ) ;
#6895 = VECTOR ( 'NONE', #24520, 1000.000000000000000 ) ;
#6896 = CARTESIAN_POINT ( 'NONE',  ( 10.81189881249999729, 0.000000000000000000, -134.8437500020484094 ) ) ;
#6897 = CARTESIAN_POINT ( 'NONE',  ( -10.81189881249999729, 1.324075727343319199E-15, -104.0937500020483810 ) ) ;
#6898 = DIRECTION ( 'NONE',  ( 1.000000000000000000, 0.000000000000000000, 0.000000000000000000 ) ) ;
#6899 = CARTESIAN_POINT ( 'NONE',  ( 10.81189881249999907, 6.242252689847868297, -104.9062500020483952 ) ) ;
#6900 = CARTESIAN_POINT ( 'NONE',  ( -4.999999999999996447, 8.660254037844387298, -186.3750000040967905 ) ) ;
#6901 = CARTESIAN_POINT ( 'NONE',  ( 10.81189881249999551, -6.242252689847874514, -116.9687500020483810 ) ) ;
#6902 = CARTESIAN_POINT ( 'NONE',  ( -10.81189881249999729, 1.324075727343319199E-15, -188.2812500020484094 ) ) ;
#6903 = CARTESIAN_POINT ( 'NONE',  ( 0.000000000000000000, 0.000000000000000000, -236.9999999999999716 ) ) ;
#6904 = CARTESIAN_POINT ( 'NONE',  ( 5.000000000000000000, 8.660254037844385522, -130.7499999999999716 ) ) ;
#6905 = CARTESIAN_POINT ( 'NONE',  ( -9.999999999999998224, 1.224646799147353059E-15, -1.249999999999973355 ) ) ;
#6906 = CARTESIAN_POINT ( 'NONE',  ( 5.405949406249999534, 9.363379034771803333, -62.59375000204836681 ) ) ;
#6907 = CARTESIAN_POINT ( 'NONE',  ( -10.81189881249999729, 6.242252689847871849, -47.21875000204836681 ) ) ;
#6908 = CARTESIAN_POINT ( 'NONE',  ( 9.999999999999996447, -5.773502691896262640, -184.0000000040968189 ) ) ;
#6909 = CARTESIAN_POINT ( 'NONE',  ( -5.405949406249996869, 9.363379034771805109, -20.53125000204836326 ) ) ;
#6910 = CARTESIAN_POINT ( 'NONE',  ( -5.405949406250003975, -9.363379034771801557, -27.34375000204835970 ) ) ;
#6911 = DIRECTION ( 'NONE',  ( -0.000000000000000000, -0.000000000000000000, -1.000000000000000000 ) ) ;
#6912 = CARTESIAN_POINT ( 'NONE',  ( -5.405949406249996869, 9.363379034771805109, -135.8437500020484094 ) ) ;
#6913 = EDGE_CURVE ( 'NONE', #25998, #5147, #23979, .T. ) ;
#6914 = CARTESIAN_POINT ( 'NONE',  ( -10.00000000000000000, -5.773502691896251982, -104.6249999999999858 ) ) ;
#6915 = CARTESIAN_POINT ( 'NONE',  ( 7.644554776091147741E-16, 12.48450537969573659, -38.65625000204836681 ) ) ;
#6916 = CARTESIAN_POINT ( 'NONE',  ( 9.999999999999998224, 0.000000000000000000, -111.4999999999999858 ) ) ;
#6917 = ADVANCED_FACE ( 'NONE', ( #22192 ), #37790, .T. ) ;
#6918 = CARTESIAN_POINT ( 'NONE',  ( 4.999999999999992006, -8.660254037844389075, -59.24999999999997158 ) ) ;
#6919 = CARTESIAN_POINT ( 'NONE',  ( -5.405949406250003975, -9.363379034771801557, -135.5312500020484094 ) ) ;
#6920 = CARTESIAN_POINT ( 'NONE',  ( -2.293366432827344421E-15, -12.48450537969573659, -103.9062500020483810 ) ) ;
#6921 = ORIENTED_EDGE ( 'NONE', *, *, #32093, .F. ) ;
#6922 = CARTESIAN_POINT ( 'NONE',  ( -9.999999999998969713, -5.773502691896847949, -131.6250000000000000 ) ) ;
#6923 = CARTESIAN_POINT ( 'NONE',  ( 5.000000000000000000, 8.660254037844385522, -107.1250000040967763 ) ) ;
#6924 = CARTESIAN_POINT ( 'NONE',  ( 4.999999999999992006, -8.660254037844389075, -136.1250000040967620 ) ) ;
#6925 = CARTESIAN_POINT ( 'NONE',  ( 5.405949406249992428, -9.363379034771808662, -64.59375000204836681 ) ) ;
#6926 = ORIENTED_EDGE ( 'NONE', *, *, #32437, .T. ) ;
#6927 = CARTESIAN_POINT ( 'NONE',  ( 9.999999999999996447, -5.773502691896262640, -32.12499999999995737 ) ) ;
#6928 = CARTESIAN_POINT ( 'NONE',  ( 5.000000000000000000, 8.660254037844385522, -17.12500000409675138 ) ) ;
#6929 = CARTESIAN_POINT ( 'NONE',  ( 10.81189881249999729, 0.000000000000000000, -46.53125000204838813 ) ) ;
#6930 = CARTESIAN_POINT ( 'NONE',  ( 9.999999999999742428, 5.773502691896404748, -125.2500000040967478 ) ) ;
#6931 = CARTESIAN_POINT ( 'NONE',  ( -4.999999999999996447, 8.660254037844387298, -33.37500000409676915 ) ) ;
#6932 = CARTESIAN_POINT ( 'NONE',  ( 9.999999999999998224, 1.224646799147353059E-15, -99.99999999999998579 ) ) ;
#6933 = VECTOR ( 'NONE', #37079, 1000.000000000000000 ) ;
#6934 = CARTESIAN_POINT ( 'NONE',  ( -5.405949406249996869, 9.363379034771805109, -143.5312500020483810 ) ) ;
#6935 = AXIS2_PLACEMENT_3D ( 'NONE', #7672, #20824, #1418 ) ;
#6936 = CYLINDRICAL_SURFACE ( 'NONE', #24525, 9.999999999999998224 ) ;
#6937 = VERTEX_POINT ( 'NONE', #12454 ) ;
#6938 = ORIENTED_EDGE ( 'NONE', *, *, #36139, .F. ) ;
#6939 = ORIENTED_EDGE ( 'NONE', *, *, #17487, .F. ) ;
#6940 = EDGE_CURVE ( 'NONE', #31885, #31861, #4426, .T. ) ;
#6941 =( BOUNDED_CURVE ( )  B_SPLINE_CURVE ( 2, ( #22403, #19157, #32348, #2772, #16967, #16108, #6847 ),
 .UNSPECIFIED., .F., .F. ) 
 B_SPLINE_CURVE_WITH_KNOTS ( ( 3, 2, 2, 3 ),
 ( 0.3694029850746270438, 0.3706467661691543181, 0.3718905472636817033, 0.3731343283582090331 ),
 .UNSPECIFIED. ) 
 CURVE ( )  GEOMETRIC_REPRESENTATION_ITEM ( )  RATIONAL_B_SPLINE_CURVE ( ( 0.9999999999999820144, 0.8660254037844566932, 1.000000000000000000, 0.8660254037844387076, 1.000000000000000000, 0.8660254037844327124, 1.000000000000005995 ) ) 
 REPRESENTATION_ITEM ( '' )  );
#6942 = DIRECTION ( 'NONE',  ( -1.000000000000000000, 0.000000000000000000, 0.000000000000000000 ) ) ;
#6943 = CYLINDRICAL_SURFACE ( 'NONE', #26998, 9.999999999999998224 ) ;
#6944 = CARTESIAN_POINT ( 'NONE',  ( -10.81189881249999907, -6.242252689847864744, -171.4687500020484094 ) ) ;
#6945 = CARTESIAN_POINT ( 'NONE',  ( 5.405949406249992428, -9.363379034771808662, -24.09375000204835970 ) ) ;
#6946 = CARTESIAN_POINT ( 'NONE',  ( -9.999999999999998224, 1.224646799147353059E-15, -111.1250000040967763 ) ) ;
#6947 = CARTESIAN_POINT ( 'NONE',  ( -2.275517850991317657E-15, -20.00000000000000000, -235.0000000000000000 ) ) ;
#6948 = CARTESIAN_POINT ( 'NONE',  ( 5.405949406249992428, -9.363379034771808662, -153.0937500020483810 ) ) ;
#6949 = CARTESIAN_POINT ( 'NONE',  ( -10.81189881249999729, 1.324075727343319199E-15, -147.5937500020483810 ) ) ;
#6950 = CARTESIAN_POINT ( 'NONE',  ( -10.00000000000154188, 5.773502691895366468, -67.37499999999995737 ) ) ;
#6951 = CARTESIAN_POINT ( 'NONE',  ( -10.81189881249999729, 1.324075727343319199E-15, -122.0937500020483952 ) ) ;
#6952 = CARTESIAN_POINT ( 'NONE',  ( -10.81189881249999907, -6.242252689847864744, -132.6562500020484094 ) ) ;
#6953 = CARTESIAN_POINT ( 'NONE',  ( -10.81189881249999729, 6.242252689847871849, -14.21875000204836681 ) ) ;
#6954 = CARTESIAN_POINT ( 'NONE',  ( -2.293366432827344421E-15, -12.48450537969573659, -136.7187500020483810 ) ) ;
#6955 = FACE_OUTER_BOUND ( 'NONE', #37730, .T. ) ;
#6956 = CARTESIAN_POINT ( 'NONE',  ( -10.00000000000051337, 5.773502691895962435, -141.2500000040967905 ) ) ;
#6957 = CARTESIAN_POINT ( 'NONE',  ( -5.000000000000003553, -8.660254037844383745, -155.5000000000000000 ) ) ;
#6958 = DIRECTION ( 'NONE',  ( -1.000000000000000000, 0.000000000000000000, 0.000000000000000000 ) ) ;
#6959 = APPROVAL_PERSON_ORGANIZATION ( #38422, #42283, #11868 ) ;
#6960 = CARTESIAN_POINT ( 'NONE',  ( 10.81189881249999729, 0.000000000000000000, -85.34375000204836681 ) ) ;
#6961 = CARTESIAN_POINT ( 'NONE',  ( 5.405949406249992428, -9.363379034771808662, -70.59375000204836681 ) ) ;
#6962 = CARTESIAN_POINT ( 'NONE',  ( 10.81189881249999729, 0.000000000000000000, -45.03125000204838102 ) ) ;
#6963 = CARTESIAN_POINT ( 'NONE',  ( -10.81189881249999907, -6.242252689847864744, -52.96875000204837391 ) ) ;
#6964 = CARTESIAN_POINT ( 'NONE',  ( 5.000000000000000000, 8.660254037844385522, -186.2500000000000000 ) ) ;
#6965 = CARTESIAN_POINT ( 'NONE',  ( 10.81189881249999907, 6.242252689847868297, -164.7187500020483810 ) ) ;
#6966 = EDGE_CURVE ( 'NONE', #9954, #11855, #15894, .T. ) ;
#6967 = CARTESIAN_POINT ( 'NONE',  ( -9.999999999999998224, 1.224646799147353059E-15, -125.7499999999999716 ) ) ;
#6968 = CARTESIAN_POINT ( 'NONE',  ( -10.81189881249999729, 1.324075727343319199E-15, -140.2812500020483810 ) ) ;
#6969 = DIRECTION ( 'NONE',  ( -0.000000000000000000, -0.000000000000000000, 1.000000000000000000 ) ) ;
#6970 = CARTESIAN_POINT ( 'NONE',  ( 10.00000000000000000, 5.773502691896255534, -94.87499999999998579 ) ) ;
#6971 = EDGE_CURVE ( 'NONE', #42590, #21106, #2802, .T. ) ;
#6972 = EDGE_LOOP ( 'NONE', ( #41467, #38685, #6101, #19751 ) ) ;
#6973 = CARTESIAN_POINT ( 'NONE',  ( 5.405949406249999534, 9.363379034771803333, -107.7812500020483810 ) ) ;
#6974 = CARTESIAN_POINT ( 'NONE',  ( -10.00000000000000000, -5.773502691896251982, -132.0000000040967905 ) ) ;
#6975 = CARTESIAN_POINT ( 'NONE',  ( -2.121150477449813534E-15, -11.54700538379251284, -177.8750000000000000 ) ) ;
#6976 = EDGE_CURVE ( 'NONE', #21643, #18815, #29301, .T. ) ;
#6977 = CARTESIAN_POINT ( 'NONE',  ( 5.405949406249992428, -9.363379034771808662, -165.2812500020484094 ) ) ;
#6978 = CARTESIAN_POINT ( 'NONE',  ( -4.999999999999996447, 8.660254037844387298, -42.37500000409677625 ) ) ;
#6979 = DIRECTION ( 'NONE',  ( -0.000000000000000000, -0.000000000000000000, 1.000000000000000000 ) ) ;
#6980 = CARTESIAN_POINT ( 'NONE',  ( -5.405949406250003975, -9.363379034771801557, -56.03125000204836681 ) ) ;
#6981 = DIRECTION ( 'NONE',  ( 1.502314598737160017E-16, -1.000000000000000000, 0.000000000000000000 ) ) ;
#6982 = CARTESIAN_POINT ( 'NONE',  ( 10.81189881249999729, 0.000000000000000000, -159.0312500020484094 ) ) ;
#6983 = CARTESIAN_POINT ( 'NONE',  ( 7.644554776091147741E-16, 12.48450537969573659, -135.9687500020483810 ) ) ;
#6984 = LINE ( 'NONE', #526, #42165 ) ;
#6985 = CARTESIAN_POINT ( 'NONE',  ( -2.121150477449813534E-15, -11.54700538379251284, -115.2500000040967905 ) ) ;
#6986 = VERTEX_POINT ( 'NONE', #18139 ) ;
#6987 = CARTESIAN_POINT ( 'NONE',  ( -9.999999999999998224, 1.224646799147353059E-15, -114.1250000040967763 ) ) ;
#6988 = ADVANCED_FACE ( 'NONE', ( #41220 ), #17919, .T. ) ;
#6989 = VECTOR ( 'NONE', #16029, 1000.000000000000000 ) ;
#6990 =( BOUNDED_CURVE ( )  B_SPLINE_CURVE ( 2, ( #1436, #14349, #18029, #28412, #35522, #18892, #38319 ),
 .UNSPECIFIED., .F., .F. ) 
 B_SPLINE_CURVE_WITH_KNOTS ( ( 3, 2, 2, 3 ),
 ( 0.8507462686567166532, 0.8519900497512440385, 0.8532338308457714238, 0.8544776119402988090 ),
 .UNSPECIFIED. ) 
 CURVE ( )  GEOMETRIC_REPRESENTATION_ITEM ( )  RATIONAL_B_SPLINE_CURVE ( ( 0.9999999999999761302, 0.8660254037844625774, 1.000000000000000000, 0.8660254037844387076, 1.000000000000000000, 0.8660254037844028474, 1.000000000000035971 ) ) 
 REPRESENTATION_ITEM ( '' )  );
#6991 = APPROVAL_PERSON_ORGANIZATION ( #31326, #40192, #28083 ) ;
#6993 = EDGE_LOOP ( 'NONE', ( #4815, #24746, #1485, #8227 ) ) ;
#6992 = CARTESIAN_POINT ( 'NONE',  ( -10.81189881249999907, -6.242252689847864744, -66.65625000204839523 ) ) ;
#6994 = APPLICATION_PROTOCOL_DEFINITION ( 'international standard', 'config_control_design', 1994, #1658 ) ;
#6996 = VERTEX_POINT ( 'NONE', #31335 ) ;
#6995 = CARTESIAN_POINT ( 'NONE',  ( 5.405949406249992428, -9.363379034771808662, -118.5937500020483810 ) ) ;
#6997 = CARTESIAN_POINT ( 'NONE',  ( -5.405949406250003975, -9.363379034771801557, -22.84375000204835615 ) ) ;
#6998 = UNCERTAINTY_MEASURE_WITH_UNIT (LENGTH_MEASURE( 1.000000000000000082E-05 ), #1003, 'distance_accuracy_value', 'NONE');
#6999 = CARTESIAN_POINT ( 'NONE',  ( -5.405949406249996869, 9.363379034771805109, 0.4687499979516285276 ) ) ;
#7000 = AXIS2_PLACEMENT_3D ( 'NONE', #27316, #785, #27529 ) ;
#7001 = CARTESIAN_POINT ( 'NONE',  ( 10.81189881249999729, 0.000000000000000000, -43.34375000204837391 ) ) ;
#7002 = DIRECTION ( 'NONE',  ( -0.000000000000000000, -0.000000000000000000, 1.000000000000000000 ) ) ;
#7003 = CYLINDRICAL_SURFACE ( 'NONE', #35584, 9.999999999999998224 ) ;
#7004 = CARTESIAN_POINT ( 'NONE',  ( -2.293366432827344421E-15, -12.48450537969573659, -178.7187500020484094 ) ) ;
#7005 = CARTESIAN_POINT ( 'NONE',  ( -5.405949406249996869, 9.363379034771805109, -165.8437500020484094 ) ) ;
#7006 = CARTESIAN_POINT ( 'NONE',  ( 7.644554776091147741E-16, 12.48450537969573659, -147.9687500020484094 ) ) ;
#7007 = CARTESIAN_POINT ( 'NONE',  ( 10.81189881249999729, 0.000000000000000000, -160.3437500020484094 ) ) ;
#7008 = DIRECTION ( 'NONE',  ( -0.000000000000000000, -0.000000000000000000, -1.000000000000000000 ) ) ;
#7009 = CARTESIAN_POINT ( 'NONE',  ( -4.999999999999996447, 8.660254037844387298, -19.87500000409675494 ) ) ;
#7010 = CARTESIAN_POINT ( 'NONE',  ( 5.000000000000000000, 8.660254037844385522, -178.7500000000000284 ) ) ;
#7011 = CARTESIAN_POINT ( 'NONE',  ( 10.81189881249999729, 0.000000000000000000, -98.84375000204838102 ) ) ;
#7012 = DIRECTION ( 'NONE',  ( -1.000000000000000000, 0.000000000000000000, -0.000000000000000000 ) ) ;
#7013 = CARTESIAN_POINT ( 'NONE',  ( -5.405949406250003975, -9.363379034771801557, -65.03125000204838102 ) ) ;
#7014 = CARTESIAN_POINT ( 'NONE',  ( 10.00000000000102318, -5.773502691895667560, -5.124999999999934275 ) ) ;
#7015 = CARTESIAN_POINT ( 'NONE',  ( -10.81189881249999907, -6.242252689847864744, -184.9687500020484094 ) ) ;
#7016 = CARTESIAN_POINT ( 'NONE',  ( 10.81189881249999729, 0.000000000000000000, -124.5312500020483952 ) ) ;
#7017 = CARTESIAN_POINT ( 'NONE',  ( 7.644554776091147741E-16, 12.48450537969573659, -160.1562500020484094 ) ) ;
#7018 = CARTESIAN_POINT ( 'NONE',  ( 10.81189881249999729, 0.000000000000000000, -52.53125000204835970 ) ) ;
#7019 = CARTESIAN_POINT ( 'NONE',  ( 4.999999999999992006, -8.660254037844389075, -134.6250000040967620 ) ) ;
#7020 = CARTESIAN_POINT ( 'NONE',  ( 9.999999999999996447, -5.773502691896262640, -117.6250000000000000 ) ) ;
#7021 = AXIS2_PLACEMENT_3D ( 'NONE', #23524, #20691, #36673 ) ;
#7022 = ORIENTED_EDGE ( 'NONE', *, *, #2979, .F. ) ;
#7023 = CARTESIAN_POINT ( 'NONE',  ( 10.81189881249999729, 6.242252689847867408, -137.9062500020484094 ) ) ;
#7024 = CARTESIAN_POINT ( 'NONE',  ( -10.81189881249999729, 6.242252689847871849, -149.4062500020484094 ) ) ;
#7025 = CARTESIAN_POINT ( 'NONE',  ( 10.81189881249999907, 6.242252689847868297, -185.9062500020484094 ) ) ;
#7026 = LINE ( 'NONE', #6808, #24763 ) ;
#7027 = CARTESIAN_POINT ( 'NONE',  ( 5.405949406249999534, 9.363379034771803333, -82.09375000204836681 ) ) ;
#7028 = VERTEX_POINT ( 'NONE', #5793 ) ;
#7029 = CARTESIAN_POINT ( 'NONE',  ( -5.000000000000003553, -8.660254037844383745, -56.49999999999996447 ) ) ;
#7030 = CARTESIAN_POINT ( 'NONE',  ( -10.81189881249999729, 6.242252689847871849, -179.2187500020483810 ) ) ;
#7031 = CARTESIAN_POINT ( 'NONE',  ( 10.00000000000000000, 5.773502691896255534, -66.75000000409677625 ) ) ;
#7032 = CARTESIAN_POINT ( 'NONE',  ( 9.999999999999612754, 5.773502691896477579, -153.3749999999999716 ) ) ;
#7033 = CARTESIAN_POINT ( 'NONE',  ( -9.999999999999804601, 5.773502691896371886, -178.7500000040967905 ) ) ;
#7034 = CARTESIAN_POINT ( 'NONE',  ( -2.293366432827344421E-15, -12.48450537969573659, -75.40625000204838102 ) ) ;
#7035 = CARTESIAN_POINT ( 'NONE',  ( -10.81189881249999729, 1.324075727343319199E-15, -57.78125000204836681 ) ) ;
#7036 = CARTESIAN_POINT ( 'NONE',  ( 9.999999999999996447, -5.773502691896262640, -49.00000000409676915 ) ) ;
#7037 = CARTESIAN_POINT ( 'NONE',  ( -10.81189881249999729, 6.242252689847871849, -11.21875000204835970 ) ) ;
#7038 = CARTESIAN_POINT ( 'NONE',  ( 4.999999999999992006, -8.660254037844389075, -137.6250000040967620 ) ) ;
#7039 = CARTESIAN_POINT ( 'NONE',  ( -2.293366432827344421E-15, -12.48450537969573659, -186.4062500020484094 ) ) ;
#7040 = VECTOR ( 'NONE', #402, 1000.000000000000000 ) ;
#7041 = EDGE_CURVE ( 'NONE', #40773, #2132, #28093, .T. ) ;
#7042 = CARTESIAN_POINT ( 'NONE',  ( 10.81189881249999551, -6.242252689847874514, -1.656250002048359482 ) ) ;
#7043 = CARTESIAN_POINT ( 'NONE',  ( 10.81189881249999729, 0.000000000000000000, -1.343750002048366143 ) ) ;
#7044 = CARTESIAN_POINT ( 'NONE',  ( 9.999999999999872102, 5.773502691896329253, -165.3750000000000000 ) ) ;
#7045 = CARTESIAN_POINT ( 'NONE',  ( -4.999999999999996447, 8.660254037844387298, -114.3750000040967763 ) ) ;
#7046 = CARTESIAN_POINT ( 'NONE',  ( 9.999999999999998224, 0.000000000000000000, -200.0000000000000000 ) ) ;
#7047 = FACE_OUTER_BOUND ( 'NONE', #8333, .T. ) ;
#7049 = ORIENTED_EDGE ( 'NONE', *, *, #1245, .F. ) ;
#7048 = CARTESIAN_POINT ( 'NONE',  ( -5.405949406250003975, -9.363379034771801557, -90.53125000204838102 ) ) ;
#7050 = CARTESIAN_POINT ( 'NONE',  ( 9.999999999998456346, 5.773502691897149042, -24.75000000409673007 ) ) ;
#7052 = ORIENTED_EDGE ( 'NONE', *, *, #22537, .T. ) ;
#7051 = CARTESIAN_POINT ( 'NONE',  ( -5.000000000000003553, -8.660254037844383745, -69.99999999999998579 ) ) ;
#7053 = EDGE_LOOP ( 'NONE', ( #15204, #33064 ) ) ;
#7054 = VECTOR ( 'NONE', #35785, 1000.000000000000000 ) ;
#7055 = CARTESIAN_POINT ( 'NONE',  ( 10.81189881249999729, 0.000000000000000000, -32.84375000204836681 ) ) ;
#7056 = CARTESIAN_POINT ( 'NONE',  ( -5.405949406249996869, 9.363379034771805109, -20.53125000204836326 ) ) ;
#7057 = CARTESIAN_POINT ( 'NONE',  ( -2.293366432827344421E-15, -12.48450537969573659, -72.21875000204835260 ) ) ;
#7058 = CARTESIAN_POINT ( 'NONE',  ( 9.999999999999998224, 0.000000000000000000, -83.37500000409677625 ) ) ;
#7059 = CARTESIAN_POINT ( 'NONE',  ( 4.999999999999992006, -8.660254037844389075, -41.24999999999997868 ) ) ;
#7060 = CARTESIAN_POINT ( 'NONE',  ( 5.405949406249992428, -9.363379034771808662, -196.5937500020484094 ) ) ;
#7061 = CARTESIAN_POINT ( 'NONE',  ( 10.81189881249999907, 6.242252689847868297, -149.7187500020483810 ) ) ;
#7062 = LINE ( 'NONE', #39431, #29485 ) ;
#7063 = LINE ( 'NONE', #16317, #16352 ) ;
#7064 = CARTESIAN_POINT ( 'NONE',  ( -10.81189881249999729, 6.242252689847871849, -152.4062500020483810 ) ) ;
#7065 = CARTESIAN_POINT ( 'NONE',  ( -10.00000000000000000, -5.773502691896251982, -1.500000004096750938 ) ) ;
#7066 = CIRCLE ( 'NONE', #22933, 9.750000000000001776 ) ;
#7067 = CARTESIAN_POINT ( 'NONE',  ( -5.000000000000003553, -8.660254037844383745, -80.49999999999998579 ) ) ;
#7068 = CARTESIAN_POINT ( 'NONE',  ( 10.81189881249999551, -6.242252689847874514, -119.9687500020483952 ) ) ;
#7069 = CARTESIAN_POINT ( 'NONE',  ( -9.999999999999998224, 1.224646799147353059E-15, -14.74999999999995737 ) ) ;
#7070 = CARTESIAN_POINT ( 'NONE',  ( -2.293366432827344421E-15, -12.48450537969573659, -90.40625000204838102 ) ) ;
#7071 = CARTESIAN_POINT ( 'NONE',  ( -5.405949406249996869, 9.363379034771805109, -107.3437500020483810 ) ) ;
#7072 = CARTESIAN_POINT ( 'NONE',  ( 10.81189881249999729, 0.000000000000000000, -71.84375000204836681 ) ) ;
#7073 = CARTESIAN_POINT ( 'NONE',  ( 7.644554776091147741E-16, 12.48450537969573659, -73.15625000204836681 ) ) ;
#7074 = CARTESIAN_POINT ( 'NONE',  ( 9.999999999999996447, -5.773502691896262640, -158.5000000040968189 ) ) ;
#7075 = CARTESIAN_POINT ( 'NONE',  ( 5.405949406249999534, 9.363379034771803333, -161.7812500020484094 ) ) ;
#7076 = CARTESIAN_POINT ( 'NONE',  ( -10.81189881249999729, 1.324075727343319199E-15, -176.2812500020484094 ) ) ;
#7077 = DIRECTION ( 'NONE',  ( -0.000000000000000000, -0.000000000000000000, 1.000000000000000000 ) ) ;
#7078 = CARTESIAN_POINT ( 'NONE',  ( 0.000000000000000000, 0.000000000000000000, -200.0000000000000000 ) ) ;
#7079 = CARTESIAN_POINT ( 'NONE',  ( -9.999999999998969713, -5.773502691896847949, -54.00000000409674072 ) ) ;
#7080 = CARTESIAN_POINT ( 'NONE',  ( -5.405949406249996869, 9.363379034771805109, -104.3437500020483810 ) ) ;
#7081 = CARTESIAN_POINT ( 'NONE',  ( -10.00000000000000000, -5.773502691896251982, -83.62499999999998579 ) ) ;
#7082 = CARTESIAN_POINT ( 'NONE',  ( 5.405949406249992428, -9.363379034771808662, -4.781250002048375691 ) ) ;
#7083 = CARTESIAN_POINT ( 'NONE',  ( 5.000000000000000000, 8.660254037844385522, -86.12500000409677625 ) ) ;
#7084 = FACE_OUTER_BOUND ( 'NONE', #17858, .T. ) ;
#7085 = CARTESIAN_POINT ( 'NONE',  ( 10.81189881249999729, 0.000000000000000000, -103.5312500020483810 ) ) ;
#7086 = CARTESIAN_POINT ( 'NONE',  ( -5.405949406250003975, -9.363379034771801557, -87.53125000204838102 ) ) ;
#7087 = VERTEX_POINT ( 'NONE', #14895 ) ;
#7088 = CARTESIAN_POINT ( 'NONE',  ( 10.00000000000000000, 5.773502691896255534, -84.75000000409677625 ) ) ;
#7089 = CARTESIAN_POINT ( 'NONE',  ( 9.999999999999998224, 0.000000000000000000, -188.0000000000000000 ) ) ;
#7090 = CARTESIAN_POINT ( 'NONE',  ( 10.81189881249999551, -6.242252689847874514, -32.96875000204835260 ) ) ;
#7091 = ORIENTED_EDGE ( 'NONE', *, *, #28102, .T. ) ;
#7092 = CARTESIAN_POINT ( 'NONE',  ( -9.999999999999998224, 5.773502691896259087, -13.37499999999996803 ) ) ;
#7093 = CARTESIAN_POINT ( 'NONE',  ( 10.81189881249999907, 6.242252689847868297, -35.90625000204835970 ) ) ;
#7094 = CARTESIAN_POINT ( 'NONE',  ( -5.000000000000003553, -8.660254037844383745, -146.5000000000000000 ) ) ;
#7095 = CARTESIAN_POINT ( 'NONE',  ( -4.999999999999996447, 8.660254037844387298, -12.37500000409674783 ) ) ;
#7096 = CARTESIAN_POINT ( 'NONE',  ( 4.999999999999992006, -8.660254037844389075, -188.2500000000000000 ) ) ;
#7097 = CARTESIAN_POINT ( 'NONE',  ( 10.00000000000038369, -5.773502691896038819, -155.5000000040967905 ) ) ;
#7099 = EDGE_LOOP ( 'NONE', ( #31859, #8534, #41414, #34019 ) ) ;
#7098 = CARTESIAN_POINT ( 'NONE',  ( 10.81189881249999907, 6.242252689847868297, -121.4062500020483810 ) ) ;
#7100 = CARTESIAN_POINT ( 'NONE',  ( 9.999999999998456346, 5.773502691897149042, -13.87499999999993072 ) ) ;
#7101 = ORIENTED_EDGE ( 'NONE', *, *, #2237, .F. ) ;
#7102 = CARTESIAN_POINT ( 'NONE',  ( 10.81189881249999551, -6.242252689847874514, -43.65625000204838102 ) ) ;
#7103 = APPROVAL_DATE_TIME ( #29779, #30720 ) ;
#7104 = CARTESIAN_POINT ( 'NONE',  ( -2.293366432827344421E-15, -12.48450537969573659, -96.21875000204839523 ) ) ;
#7105 = CARTESIAN_POINT ( 'NONE',  ( -5.405949406250003975, -9.363379034771801557, -120.5312500020483952 ) ) ;
#7106 = ORIENTED_EDGE ( 'NONE', *, *, #38786, .F. ) ;
#7107 = CARTESIAN_POINT ( 'NONE',  ( -9.999999999999998224, 1.224646799147353059E-15, -153.1250000040967905 ) ) ;
#7108 = CARTESIAN_POINT ( 'NONE',  ( 9.999999999998969713, 5.773502691896851502, -33.37499999999994316 ) ) ;
#7109 =( BOUNDED_CURVE ( )  B_SPLINE_CURVE ( 2, ( #10932, #20228, #21079, #33417, #34267, #40077, #37057 ),
 .UNSPECIFIED., .F., .F. ) 
 B_SPLINE_CURVE_WITH_KNOTS ( ( 3, 2, 2, 3 ),
 ( 0.2649253731343284568, 0.2661691542288558421, 0.2674129353233831718, 0.2686567164179105571 ),
 .UNSPECIFIED. ) 
 CURVE ( )  GEOMETRIC_REPRESENTATION_ITEM ( )  RATIONAL_B_SPLINE_CURVE ( ( 0.9999999999999880096, 0.8660254037844506980, 1.000000000000000000, 0.8660254037844387076, 1.000000000000000000, 0.8660254037844267172, 1.000000000000011990 ) ) 
 REPRESENTATION_ITEM ( '' )  );
#7110 = CARTESIAN_POINT ( 'NONE',  ( 10.81189881249999551, -6.242252689847874514, -169.6562500020484094 ) ) ;
#7111 = CARTESIAN_POINT ( 'NONE',  ( -9.999999999999998224, 1.224646799147353059E-15, -147.1250000040967905 ) ) ;
#7112 = CARTESIAN_POINT ( 'NONE',  ( 10.81189881249999729, 6.242252689847867408, -134.7187500020483810 ) ) ;
#7113 = CARTESIAN_POINT ( 'NONE',  ( -2.293366432827344421E-15, -12.48450537969573659, -90.21875000204838102 ) ) ;
#7114 = CARTESIAN_POINT ( 'NONE',  ( 0.000000000000000000, 0.000000000000000000, -200.0000000000000000 ) ) ;
#7115 = CARTESIAN_POINT ( 'NONE',  ( -10.81189881249999729, 6.242252689847871849, -102.9062500020483810 ) ) ;
#7116 = CARTESIAN_POINT ( 'NONE',  ( 9.999999999999998224, 0.000000000000000000, -185.3750000040967905 ) ) ;
#7117 = CARTESIAN_POINT ( 'NONE',  ( 5.405949406249992428, -9.363379034771808662, -114.0937500020483810 ) ) ;
#7118 = CARTESIAN_POINT ( 'NONE',  ( 5.405949406249992428, -9.363379034771808662, -178.7812500020484094 ) ) ;
#7119 = DIRECTION ( 'NONE',  ( -0.000000000000000000, -0.000000000000000000, -1.000000000000000000 ) ) ;
#7120 = DIRECTION ( 'NONE',  ( -0.000000000000000000, -0.000000000000000000, 1.000000000000000000 ) ) ;
#7121 = CARTESIAN_POINT ( 'NONE',  ( 7.644554776091147741E-16, 12.48450537969573659, -197.6562500020484379 ) ) ;
#7122 = CARTESIAN_POINT ( 'NONE',  ( 7.644554776091147741E-16, 12.48450537969573659, -60.96875000204838102 ) ) ;
#7123 = CARTESIAN_POINT ( 'NONE',  ( -2.293366432827344421E-15, -12.48450537969573659, -42.21875000204835970 ) ) ;
#7124 = CARTESIAN_POINT ( 'NONE',  ( 10.00000000000000000, 5.773502691896255534, -171.7500000040967905 ) ) ;
#7125 = CARTESIAN_POINT ( 'NONE',  ( 5.405949406249999534, 9.363379034771803333, -20.78125000204836326 ) ) ;
#7126 = CARTESIAN_POINT ( 'NONE',  ( -10.81189881249999729, 6.242252689847871849, -18.71875000204837036 ) ) ;
#7127 = DIRECTION ( 'NONE',  ( -0.000000000000000000, -1.000000000000000000, -0.000000000000000000 ) ) ;
#7128 = CARTESIAN_POINT ( 'NONE',  ( -10.81189881249999729, 1.324075727343319199E-15, -134.0937500020483810 ) ) ;
#7129 = CARTESIAN_POINT ( 'NONE',  ( 10.00000000000000000, 5.773502691896255534, -108.3749999999999858 ) ) ;
#7130 = CARTESIAN_POINT ( 'NONE',  ( -5.405949406250003975, -9.363379034771801557, -27.53125000204836681 ) ) ;
#7131 = CARTESIAN_POINT ( 'NONE',  ( -9.999999999999998224, 1.224646799147353059E-15, -49.62500000409675494 ) ) ;
#7132 = CARTESIAN_POINT ( 'NONE',  ( 5.000000000000000000, 8.660254037844385522, -58.74999999999997158 ) ) ;
#7133 = CARTESIAN_POINT ( 'NONE',  ( -10.81189881249999729, 1.324075727343319199E-15, -132.7812500020483810 ) ) ;
#7134 = CARTESIAN_POINT ( 'NONE',  ( -2.293366432827344421E-15, -12.48450537969573659, -109.9062500020483810 ) ) ;
#7135 = ORIENTED_EDGE ( 'NONE', *, *, #30471, .T. ) ;
#7136 = FACE_BOUND ( 'NONE', #35464, .T. ) ;
#7137 = CARTESIAN_POINT ( 'NONE',  ( -9.999999999999998224, 5.773502691896259087, -108.2500000040967763 ) ) ;
#7138 = CARTESIAN_POINT ( 'NONE',  ( 9.999999999999998224, 0.000000000000000000, -101.3750000040967905 ) ) ;
#7139 = CARTESIAN_POINT ( 'NONE',  ( 10.81189881249999907, 6.242252689847868297, -67.21875000204838102 ) ) ;
#7140 = ORIENTED_EDGE ( 'NONE', *, *, #9357, .T. ) ;
#7141 = CARTESIAN_POINT ( 'NONE',  ( 9.999999999999998224, 0.000000000000000000, -31.99999999999997158 ) ) ;
#7142 = CARTESIAN_POINT ( 'NONE',  ( -2.293366432827344421E-15, -12.48450537969573659, -33.40625000204835970 ) ) ;
#7143 = CARTESIAN_POINT ( 'NONE',  ( 9.999999999999227285, 5.773502691896701400, -111.7500000040967478 ) ) ;
#7144 = CARTESIAN_POINT ( 'NONE',  ( 4.999999999999992006, -8.660254037844389075, -34.12500000409676915 ) ) ;
#7145 = CARTESIAN_POINT ( 'NONE',  ( -4.999999999999996447, 8.660254037844387298, -133.5000000000000000 ) ) ;
#7146 = CARTESIAN_POINT ( 'NONE',  ( 10.81189881249999551, -6.242252689847874514, -142.6562500020484094 ) ) ;
#7147 = CARTESIAN_POINT ( 'NONE',  ( 9.999999999999998224, 0.000000000000000000, -200.0000000000000000 ) ) ;
#7148 = ORIENTED_EDGE ( 'NONE', *, *, #20142, .T. ) ;
#7149 = EDGE_CURVE ( 'NONE', #21158, #20251, #7194, .T. ) ;
#7150 = ORIENTED_EDGE ( 'NONE', *, *, #10841, .T. ) ;
#7151 = CARTESIAN_POINT ( 'NONE',  ( 0.000000000000000000, 0.000000000000000000, -200.0000000000000000 ) ) ;
#7152 = ADVANCED_FACE ( 'NONE', ( #31116, #35788 ), #39011, .T. ) ;
#7153 = CARTESIAN_POINT ( 'NONE',  ( -9.999999999999227285, -5.773502691896698735, -104.6249999999999574 ) ) ;
#7154 = CARTESIAN_POINT ( 'NONE',  ( -10.81189881249999729, 6.242252689847871849, -162.7187500020483810 ) ) ;
#7155 = CARTESIAN_POINT ( 'NONE',  ( 10.81189881249999907, 6.242252689847868297, -199.4062500020484094 ) ) ;
#7156 = CARTESIAN_POINT ( 'NONE',  ( 10.81189881249999551, -6.242252689847874514, -19.46875000204837391 ) ) ;
#7157 = CARTESIAN_POINT ( 'NONE',  ( -9.999999999999998224, 1.224646799147353059E-15, -110.7499999999999858 ) ) ;
#7158 = CARTESIAN_POINT ( 'NONE',  ( 5.405949406249992428, -9.363379034771808662, -159.0937500020484094 ) ) ;
#7159 = CARTESIAN_POINT ( 'NONE',  ( -5.405949406250003975, -9.363379034771801557, -139.8437500020484094 ) ) ;
#7160 = CARTESIAN_POINT ( 'NONE',  ( -9.999999999999998224, 1.224646799147353059E-15, -119.7500000000000000 ) ) ;
#7161 = CARTESIAN_POINT ( 'NONE',  ( -2.293366432827344421E-15, -12.48450537969573659, -120.2187500020483952 ) ) ;
#7162 = CARTESIAN_POINT ( 'NONE',  ( -2.121150477449813534E-15, -11.54700538379251284, -193.2500000040968473 ) ) ;
#7163 = CARTESIAN_POINT ( 'NONE',  ( -10.81189881249999729, 6.242252689847871849, -126.9062500020483810 ) ) ;
#7164 = CARTESIAN_POINT ( 'NONE',  ( -10.81189881249999729, 6.242252689847871849, -12.71875000204837747 ) ) ;
#7165 = CARTESIAN_POINT ( 'NONE',  ( 5.405949406249999534, 9.363379034771803333, -140.5937500020483810 ) ) ;
#7166 = CARTESIAN_POINT ( 'NONE',  ( 9.999999999998969713, 5.773502691896851502, -63.75000000409677625 ) ) ;
#7167 = CARTESIAN_POINT ( 'NONE',  ( 7.070501591499376803E-16, 11.54700538379251284, -125.0000000040967763 ) ) ;
#7168 = CARTESIAN_POINT ( 'NONE',  ( 9.999999999999996447, -5.773502691896262640, -152.1250000000000284 ) ) ;
#7169 = CARTESIAN_POINT ( 'NONE',  ( 7.644554776091147741E-16, 12.48450537969573659, 0.3437499979516422943 ) ) ;
#7170 = CARTESIAN_POINT ( 'NONE',  ( -10.81189881249999729, -6.242252689847864744, -82.96875000204836681 ) ) ;
#7171 = CARTESIAN_POINT ( 'NONE',  ( -10.81189881249999729, 6.242252689847871849, -62.21875000204838813 ) ) ;
#7172 = CARTESIAN_POINT ( 'NONE',  ( 10.81189881249999551, -6.242252689847874514, -40.65625000204835970 ) ) ;
#7173 = CARTESIAN_POINT ( 'NONE',  ( -10.81189881249999907, -6.242252689847864744, -54.46875000204836681 ) ) ;
#7174 = CARTESIAN_POINT ( 'NONE',  ( 7.070501591499376803E-16, 11.54700538379251284, -186.1250000000000000 ) ) ;
#7175 = CARTESIAN_POINT ( 'NONE',  ( -10.81189881249999907, -6.242252689847864744, -154.9687500020484094 ) ) ;
#7176 = CARTESIAN_POINT ( 'NONE',  ( 7.070501591499377789E-16, 11.54700538379251284, -126.1249999999999858 ) ) ;
#7177 = CARTESIAN_POINT ( 'NONE',  ( 7.644554776091147741E-16, 12.48450537969573659, -139.1562500020484094 ) ) ;
#7178 = CARTESIAN_POINT ( 'NONE',  ( 4.999999999999992006, -8.660254037844389075, -150.7500000000000000 ) ) ;
#7179 = CARTESIAN_POINT ( 'NONE',  ( 9.999999999999998224, 0.000000000000000000, -85.99999999999998579 ) ) ;
#7180 = CARTESIAN_POINT ( 'NONE',  ( 5.405949406249992428, -9.363379034771808662, -21.28125000204836326 ) ) ;
#7181 = ORIENTED_EDGE ( 'NONE', *, *, #14541, .T. ) ;
#7182 = CARTESIAN_POINT ( 'NONE',  ( 10.81189881249999729, 0.000000000000000000, -109.5312500020483810 ) ) ;
#7183 = CARTESIAN_POINT ( 'NONE',  ( -9.999999999999998224, 5.773502691896259087, -130.7500000040967905 ) ) ;
#7184 = CARTESIAN_POINT ( 'NONE',  ( 5.000000000000000000, 8.660254037844385522, -39.24999999999997868 ) ) ;
#7185 = CARTESIAN_POINT ( 'NONE',  ( -4.999999999999996447, 8.660254037844387298, -45.37500000409677625 ) ) ;
#7186 = LINE ( 'NONE', #20770, #12491 ) ;
#7187 = CARTESIAN_POINT ( 'NONE',  ( -5.405949406250003975, -9.363379034771801557, -51.53125000204835970 ) ) ;
#7188 = CARTESIAN_POINT ( 'NONE',  ( -9.999999999999998224, 1.224646799147353059E-15, -146.7500000000000000 ) ) ;
#7189 = CARTESIAN_POINT ( 'NONE',  ( -10.81189881249999729, 6.242252689847871849, -150.9062500020484094 ) ) ;
#7190 = CARTESIAN_POINT ( 'NONE',  ( -2.293366432827344421E-15, -12.48450537969573659, -136.7187500020483810 ) ) ;
#7191 = FACE_OUTER_BOUND ( 'NONE', #8752, .T. ) ;
#7192 = CARTESIAN_POINT ( 'NONE',  ( -4.999999999999996447, 8.660254037844387298, -151.5000000000000000 ) ) ;
#7193 = ORIENTED_EDGE ( 'NONE', *, *, #32563, .T. ) ;
#7194 =( BOUNDED_CURVE ( )  B_SPLINE_CURVE ( 2, ( #2562, #9448, #15692, #22614, #12661, #34352, #9231 ),
 .UNSPECIFIED., .F., .F. ) 
 B_SPLINE_CURVE_WITH_KNOTS ( ( 3, 2, 2, 3 ),
 ( 0.7462686567164180662, 0.7475124378109453405, 0.7487562189054727257, 0.7500000000000001110 ),
 .UNSPECIFIED. ) 
 CURVE ( )  GEOMETRIC_REPRESENTATION_ITEM ( )  RATIONAL_B_SPLINE_CURVE ( ( 0.9999999999999880096, 0.8660254037844506980, 1.000000000000000000, 0.8660254037844387076, 1.000000000000000000, 0.8660254037844267172, 1.000000000000011990 ) ) 
 REPRESENTATION_ITEM ( '' )  );
#7196 = VERTEX_POINT ( 'NONE', #6220 ) ;
#7195 = CARTESIAN_POINT ( 'NONE',  ( 7.644554776091147741E-16, 12.48450537969573659, -61.15625000204838102 ) ) ;
#7197 = CALENDAR_DATE ( 2026, 28, 9 ) ;
#7198 = EDGE_CURVE ( 'NONE', #21756, #36343, #42024, .T. ) ;
#7199 = EDGE_CURVE ( 'NONE', #39779, #27592, #38804, .T. ) ;
#7201 = VERTEX_POINT ( 'NONE', #19154 ) ;
#7200 = CARTESIAN_POINT ( 'NONE',  ( 7.644554776091147741E-16, 12.48450537969573659, -122.4687500020483952 ) ) ;
#7202 = EDGE_CURVE ( 'NONE', #14562, #22008, #32345, .T. ) ;
#7203 = CARTESIAN_POINT ( 'NONE',  ( 10.81189881249999729, 0.000000000000000000, -20.84375000204835615 ) ) ;
#7204 = CARTESIAN_POINT ( 'NONE',  ( 10.81189881249999729, 0.000000000000000000, -199.3437500020484094 ) ) ;
#7205 = CARTESIAN_POINT ( 'NONE',  ( 10.81189881249999907, 6.242252689847868297, -49.21875000204835260 ) ) ;
#7206 = CARTESIAN_POINT ( 'NONE',  ( 9.999999999999998224, 0.000000000000000000, -155.3750000040967905 ) ) ;
#7207 = CARTESIAN_POINT ( 'NONE',  ( 9.999999999999998224, 0.000000000000000000, -9.875000004096746054 ) ) ;
#7208 = CARTESIAN_POINT ( 'NONE',  ( 5.405949406249992428, -9.363379034771808662, -183.0937500020483810 ) ) ;
#7209 = CARTESIAN_POINT ( 'NONE',  ( 10.81189881249999729, 0.000000000000000000, -164.8437500020484094 ) ) ;
#7210 = APPROVAL ( #7315, 'UNSPECIFIED' ) ;
#7211 = CARTESIAN_POINT ( 'NONE',  ( 10.81189881249999551, -6.242252689847874514, -149.9687500020483810 ) ) ;
#7212 = CARTESIAN_POINT ( 'NONE',  ( -5.405949406250003975, -9.363379034771801557, -159.3437500020484094 ) ) ;
#7213 = CARTESIAN_POINT ( 'NONE',  ( 9.999999999999742428, 5.773502691896404748, -123.7500000040967763 ) ) ;
#7214 = CARTESIAN_POINT ( 'NONE',  ( 9.999999999999479527, 5.773502691896553074, -36.37499999999995026 ) ) ;
#7215 = CARTESIAN_POINT ( 'NONE',  ( -10.00000000000000000, -5.773502691896251982, -176.6250000000000284 ) ) ;
#7216 = CARTESIAN_POINT ( 'NONE',  ( -10.81189881249999729, 1.324075727343319199E-15, -101.0937500020483810 ) ) ;
#7217 = CARTESIAN_POINT ( 'NONE',  ( 7.070501591499376803E-16, 11.54700538379251284, -34.62499999999995737 ) ) ;
#7218 = CARTESIAN_POINT ( 'NONE',  ( -5.405949406249996869, 9.363379034771805109, -68.53125000204838102 ) ) ;
#7219 = CARTESIAN_POINT ( 'NONE',  ( -10.00000000000051337, 5.773502691895962435, -145.7500000040967905 ) ) ;
#7220 = CARTESIAN_POINT ( 'NONE',  ( 10.81189881249999907, 6.242252689847868297, -185.7187500020483810 ) ) ;
#7221 = EDGE_CURVE ( 'NONE', #36222, #31836, #33177, .T. ) ;
#7222 = CARTESIAN_POINT ( 'NONE',  ( 10.81189881249999907, 6.242252689847868297, -124.4062500020483810 ) ) ;
#7223 = CARTESIAN_POINT ( 'NONE',  ( -10.81189881249999729, 1.324075727343319199E-15, -164.2812500020484094 ) ) ;
#7224 = CARTESIAN_POINT ( 'NONE',  ( -10.81189881249999907, -6.242252689847864744, -50.15625000204837391 ) ) ;
#7225 = CARTESIAN_POINT ( 'NONE',  ( -10.00000000000000000, -5.773502691896251982, -138.0000000040967905 ) ) ;
#7226 = CARTESIAN_POINT ( 'NONE',  ( 9.999999999999996447, -5.773502691896262640, -110.1250000000000000 ) ) ;
#7227 = VERTEX_POINT ( 'NONE', #19997 ) ;
#7228 = CARTESIAN_POINT ( 'NONE',  ( -5.405949406250003975, -9.363379034771801557, -131.0312500020484094 ) ) ;
#7229 = CARTESIAN_POINT ( 'NONE',  ( 10.81189881249999729, 0.000000000000000000, -147.0312500020483810 ) ) ;
#7230 = ADVANCED_FACE ( 'NONE', ( #39848 ), #16746, .F. ) ;
#7231 = CARTESIAN_POINT ( 'NONE',  ( -10.81189881249999729, 1.324075727343319199E-15, -186.7812500020484094 ) ) ;
#7232 = CARTESIAN_POINT ( 'NONE',  ( -5.405949406249996869, 9.363379034771805109, -84.84375000204836681 ) ) ;
#7233 = ORIENTED_EDGE ( 'NONE', *, *, #23947, .T. ) ;
#7234 = CARTESIAN_POINT ( 'NONE',  ( 4.999999999999992006, -8.660254037844389075, -45.74999999999998579 ) ) ;
#7235 = CARTESIAN_POINT ( 'NONE',  ( 7.644554776091147741E-16, 12.48450537969573659, -180.9687500020484094 ) ) ;
#7236 = CARTESIAN_POINT ( 'NONE',  ( -10.00000000000000000, -5.773502691896251982, -64.50000000409677625 ) ) ;
#7237 = CARTESIAN_POINT ( 'NONE',  ( -2.121150477449813534E-15, -11.54700538379251284, -109.2500000040967763 ) ) ;
#7238 = CARTESIAN_POINT ( 'NONE',  ( 10.00000000000051159, -5.773502691895965988, -175.0000000040968189 ) ) ;
#7239 = CARTESIAN_POINT ( 'NONE',  ( -5.405949406250003975, -9.363379034771801557, -78.53125000204838102 ) ) ;
#7240 = CARTESIAN_POINT ( 'NONE',  ( -5.405949406249996869, 9.363379034771805109, -59.53125000204836681 ) ) ;
#7241 =( BOUNDED_CURVE ( )  B_SPLINE_CURVE ( 2, ( #22886, #39692, #36045, #3243, #16587, #28945, #13137 ),
 .UNSPECIFIED., .F., .F. ) 
 B_SPLINE_CURVE_WITH_KNOTS ( ( 3, 2, 2, 3 ),
 ( 0.2052238805970149627, 0.2064676616915423202, 0.2077114427860697055, 0.2089552238805970630 ),
 .UNSPECIFIED. ) 
 CURVE ( )  GEOMETRIC_REPRESENTATION_ITEM ( )  RATIONAL_B_SPLINE_CURVE ( ( 0.9999999999999970024, 0.8660254037844417052, 1.000000000000000000, 0.8660254037844387076, 1.000000000000000000, 0.8660254037844327124, 1.000000000000005995 ) ) 
 REPRESENTATION_ITEM ( '' )  );
#7242 = CARTESIAN_POINT ( 'NONE',  ( -5.000000000000003553, -8.660254037844383745, -49.37500000409678336 ) ) ;
#7243 = CARTESIAN_POINT ( 'NONE',  ( -5.405949406250003975, -9.363379034771801557, -6.343750002048370362 ) ) ;
#7244 = DIRECTION ( 'NONE',  ( -0.000000000000000000, -0.000000000000000000, 1.000000000000000000 ) ) ;
#7245 = CARTESIAN_POINT ( 'NONE',  ( -10.81189881249999729, 6.242252689847871849, -182.4062500020483810 ) ) ;
#7246 = CARTESIAN_POINT ( 'NONE',  ( -10.81189881249999907, -6.242252689847864744, -3.656250002048361036 ) ) ;
#7247 = CARTESIAN_POINT ( 'NONE',  ( -10.00000000000051337, 5.773502691895962435, -79.37499999999998579 ) ) ;
#7248 = CARTESIAN_POINT ( 'NONE',  ( 5.000000000000000000, 8.660254037844385522, -165.2500000000000000 ) ) ;
#7249 = EDGE_CURVE ( 'NONE', #19560, #27517, #7063, .T. ) ;
#7250 = DIRECTION ( 'NONE',  ( -0.000000000000000000, -0.000000000000000000, -1.000000000000000000 ) ) ;
#7251 = CARTESIAN_POINT ( 'NONE',  ( -8.223921726897051698, 5.755749732088058401, -0.000000000000000000 ) ) ;
#7252 = AXIS2_PLACEMENT_3D ( 'NONE', #40013, #10865, #33558 ) ;
#7253 =( BOUNDED_CURVE ( )  B_SPLINE_CURVE ( 2, ( #24411, #37340, #4969, #27418, #34329, #40554, #41191 ),
 .UNSPECIFIED., .F., .F. ) 
 B_SPLINE_CURVE_WITH_KNOTS ( ( 3, 2, 2, 3 ),
 ( 0.2835820895522389029, 0.2848258706467662882, 0.2860696517412936180, 0.2873134328358210032 ),
 .UNSPECIFIED. ) 
 CURVE ( )  GEOMETRIC_REPRESENTATION_ITEM ( )  RATIONAL_B_SPLINE_CURVE ( ( 0.9999999999999880096, 0.8660254037844506980, 1.000000000000000000, 0.8660254037844387076, 1.000000000000000000, 0.8660254037844267172, 1.000000000000011990 ) ) 
 REPRESENTATION_ITEM ( '' )  );
#7254 = FACE_OUTER_BOUND ( 'NONE', #12116, .T. ) ;
#7256 = ORIENTED_EDGE ( 'NONE', *, *, #35980, .T. ) ;
#7255 = CARTESIAN_POINT ( 'NONE',  ( -10.81189881249999729, 6.242252689847871849, -84.90625000204838102 ) ) ;
#7257 = DIRECTION ( 'NONE',  ( -0.000000000000000000, -0.000000000000000000, 1.000000000000000000 ) ) ;
#7259 = ORIENTED_EDGE ( 'NONE', *, *, #11980, .F. ) ;
#7258 = CARTESIAN_POINT ( 'NONE',  ( 7.644554776091147741E-16, 12.48450537969573659, -101.4687500020483668 ) ) ;
#7260 = ORIENTED_EDGE ( 'NONE', *, *, #38889, .F. ) ;
#7261 = CARTESIAN_POINT ( 'NONE',  ( -10.81189881249999907, -6.242252689847864744, -28.96875000204835615 ) ) ;
#7262 = CARTESIAN_POINT ( 'NONE',  ( -5.405949406250003975, -9.363379034771801557, -23.03125000204836326 ) ) ;
#7263 = CONTEXT_DEPENDENT_SHAPE_REPRESENTATION ( #25113, #19309 ) ;
#7264 = CARTESIAN_POINT ( 'NONE',  ( 5.405949406249992428, -9.363379034771808662, -72.09375000204836681 ) ) ;
#7265 = CARTESIAN_POINT ( 'NONE',  ( -2.121150477449813534E-15, -11.54700538379251284, -83.75000000409677625 ) ) ;
#7266 = CARTESIAN_POINT ( 'NONE',  ( 10.00000000000000000, 5.773502691896255534, -43.87499999999996447 ) ) ;
#7267 = CARTESIAN_POINT ( 'NONE',  ( -10.81189881249999729, 6.242252689847871849, -186.7187500020483810 ) ) ;
#7268 = CARTESIAN_POINT ( 'NONE',  ( 7.644554776091147741E-16, 12.48450537969573659, -152.4687500020483810 ) ) ;
#7269 = LINE ( 'NONE', #32394, #26832 ) ;
#7270 = FACE_OUTER_BOUND ( 'NONE', #18079, .T. ) ;
#7271 = CARTESIAN_POINT ( 'NONE',  ( 9.999999999999998224, 0.000000000000000000, -174.5000000000000284 ) ) ;
#7272 = CARTESIAN_POINT ( 'NONE',  ( 10.00000000000000000, 5.773502691896255534, -3.750000004096762041 ) ) ;
#7273 = CARTESIAN_POINT ( 'NONE',  ( 0.000000000000000000, 0.000000000000000000, -200.0000000000000000 ) ) ;
#7274 = ADVANCED_FACE ( 'NONE', ( #26280 ), #18473, .T. ) ;
#7275 = CARTESIAN_POINT ( 'NONE',  ( 10.81189881249999729, 0.000000000000000000, -124.3437500020483952 ) ) ;
#7276 = CARTESIAN_POINT ( 'NONE',  ( -9.999999999999998224, 1.224646799147353059E-15, -200.0000000000000000 ) ) ;
#7277 = CARTESIAN_POINT ( 'NONE',  ( 5.405949406249992428, -9.363379034771808662, -91.78125000204838102 ) ) ;
#7278 = CARTESIAN_POINT ( 'NONE',  ( 10.81189881249999729, 6.242252689847867408, -98.71875000204838102 ) ) ;
#7279 = CARTESIAN_POINT ( 'NONE',  ( -10.81189881249999907, -6.242252689847864744, -67.96875000204838102 ) ) ;
#7280 = VECTOR ( 'NONE', #22507, 1000.000000000000000 ) ;
#7281 = CARTESIAN_POINT ( 'NONE',  ( -5.405949406250003975, -9.363379034771801557, -78.53125000204838102 ) ) ;
#7282 = CARTESIAN_POINT ( 'NONE',  ( -5.000000000000003553, -8.660254037844383745, -160.3750000040967905 ) ) ;
#7283 = CARTESIAN_POINT ( 'NONE',  ( 10.81189881249999729, 0.000000000000000000, -159.0312500020484094 ) ) ;
#7284 = CARTESIAN_POINT ( 'NONE',  ( 10.81189881249999907, 6.242252689847868297, -173.9062500020484094 ) ) ;
#7285 = DIRECTION ( 'NONE',  ( -0.000000000000000000, -0.000000000000000000, 1.000000000000000000 ) ) ;
#7286 = CARTESIAN_POINT ( 'NONE',  ( -24.99999999999999645, 0.000000000000000000, -99.99999999999998579 ) ) ;
#7287 = DIRECTION ( 'NONE',  ( -0.000000000000000000, -0.000000000000000000, 1.000000000000000000 ) ) ;
#7288 = CARTESIAN_POINT ( 'NONE',  ( -2.293366432827344421E-15, -12.48450537969573659, -103.7187500020483668 ) ) ;
#7289 = CARTESIAN_POINT ( 'NONE',  ( 9.999999999998456346, 5.773502691897149042, -63.37499999999994316 ) ) ;
#7290 = CARTESIAN_POINT ( 'NONE',  ( -4.999999999999996447, 8.660254037844387298, -77.99999999999998579 ) ) ;
#7291 = CARTESIAN_POINT ( 'NONE',  ( -2.293366432827344421E-15, -12.48450537969573659, -7.906250002048365921 ) ) ;
#7292 = CARTESIAN_POINT ( 'NONE',  ( 5.000000000000000000, 8.660254037844385522, -93.62500000409677625 ) ) ;
#7293 = AXIS2_PLACEMENT_3D ( 'NONE', #32013, #2018, #5244 ) ;
#7294 = CARTESIAN_POINT ( 'NONE',  ( 7.071067811865477282, -7.071067811865471064, -200.0000000000000000 ) ) ;
#7295 = CARTESIAN_POINT ( 'NONE',  ( 5.405949406249999534, 9.363379034771803333, -100.2812500020483952 ) ) ;
#7296 = CARTESIAN_POINT ( 'NONE',  ( -5.405949406250003975, -9.363379034771801557, -80.03125000204838102 ) ) ;
#7297 = CARTESIAN_POINT ( 'NONE',  ( -4.999999999999996447, 8.660254037844387298, -73.87500000409677625 ) ) ;
#7298 = DIRECTION ( 'NONE',  ( 0.000000000000000000, 0.000000000000000000, 1.000000000000000000 ) ) ;
#7299 = CARTESIAN_POINT ( 'NONE',  ( 5.405949406249999534, 9.363379034771803333, -31.09375000204836326 ) ) ;
#7300 = ORIENTED_EDGE ( 'NONE', *, *, #109, .F. ) ;
#7301 = CARTESIAN_POINT ( 'NONE',  ( -5.000000000000003553, -8.660254037844383745, -8.499999999999952038 ) ) ;
#7302 = CARTESIAN_POINT ( 'NONE',  ( 5.405949406249999534, 9.363379034771803333, -26.78125000204836681 ) ) ;
#7303 = CARTESIAN_POINT ( 'NONE',  ( 4.999999999999992006, -8.660254037844389075, -146.2500000000000000 ) ) ;
#7304 = CARTESIAN_POINT ( 'NONE',  ( -4.999999999999996447, 8.660254037844387298, -45.37500000409677625 ) ) ;
#7305 = CARTESIAN_POINT ( 'NONE',  ( -10.00000000000000000, -5.773502691896251982, -7.500000004096757600 ) ) ;
#7306 = CARTESIAN_POINT ( 'NONE',  ( 5.405949406249999534, 9.363379034771803333, -139.2812500020483810 ) ) ;
#7307 = CARTESIAN_POINT ( 'NONE',  ( 7.070501591499377789E-16, 11.54700538379251284, -192.1250000000000000 ) ) ;
#7309 = VERTEX_POINT ( 'NONE', #29516 ) ;
#7308 = CARTESIAN_POINT ( 'NONE',  ( 10.81189881249999907, 6.242252689847868297, -118.4062500020484094 ) ) ;
#7310 = CARTESIAN_POINT ( 'NONE',  ( 7.070501591499376803E-16, 11.54700538379251284, -23.00000000409677270 ) ) ;
#7311 = VERTEX_POINT ( 'NONE', #7271 ) ;
#7312 = AXIS2_PLACEMENT_3D ( 'NONE', #35263, #14357, #27554 ) ;
#7313 = ORIENTED_EDGE ( 'NONE', *, *, #1727, .F. ) ;
#7314 = CARTESIAN_POINT ( 'NONE',  ( -10.81189881249999907, -6.242252689847864744, -42.65625000204837391 ) ) ;
#7315 = APPROVAL_STATUS ( 'not_yet_approved' ) ;
#7316 = CARTESIAN_POINT ( 'NONE',  ( 5.405949406249999534, 9.363379034771803333, -92.59375000204838102 ) ) ;
#7317 = CARTESIAN_POINT ( 'NONE',  ( -10.81189881249999729, 1.324075727343319199E-15, -126.7812500020483668 ) ) ;
#7318 = ORIENTED_EDGE ( 'NONE', *, *, #18835, .T. ) ;
#7319 = AXIS2_PLACEMENT_3D ( 'NONE', #33453, #10, #3881 ) ;
#7320 =( BOUNDED_CURVE ( )  B_SPLINE_CURVE ( 2, ( #35060, #5917, #31612, #35276, #5488, #18638, #2268 ),
 .UNSPECIFIED., .F., .F. ) 
 B_SPLINE_CURVE_WITH_KNOTS ( ( 3, 2, 2, 3 ),
 ( 0.2761194029850747578, 0.2773631840796020875, 0.2786069651741294728, 0.2798507462686568026 ),
 .UNSPECIFIED. ) 
 CURVE ( )  GEOMETRIC_REPRESENTATION_ITEM ( )  RATIONAL_B_SPLINE_CURVE ( ( 0.9999999999999880096, 0.8660254037844506980, 1.000000000000000000, 0.8660254037844387076, 1.000000000000000000, 0.8660254037844267172, 1.000000000000011990 ) ) 
 REPRESENTATION_ITEM ( '' )  );
#7321 = DIRECTION ( 'NONE',  ( -1.000000000000000000, 0.000000000000000000, 0.000000000000000000 ) ) ;
#7322 = CARTESIAN_POINT ( 'NONE',  ( -10.81189881249999729, -6.242252689847864744, -195.4687500020484094 ) ) ;
#7323 = CARTESIAN_POINT ( 'NONE',  ( -10.81189881249999907, -6.242252689847864744, -171.6562500020484094 ) ) ;
#7324 = CARTESIAN_POINT ( 'NONE',  ( -9.999999999999998224, 1.224646799147353059E-15, -200.0000000000000000 ) ) ;
#7325 = EDGE_CURVE ( 'NONE', #27752, #38572, #177, .T. ) ;
#7326 = CARTESIAN_POINT ( 'NONE',  ( -5.405949406250003975, -9.363379034771801557, -120.3437500020483952 ) ) ;
#7327 = PRODUCT_DEFINITION_SHAPE ( 'NONE', 'NONE',  #14057 ) ;
#7328 = CARTESIAN_POINT ( 'NONE',  ( -5.405949406249996869, 9.363379034771805109, -96.84375000204838102 ) ) ;
#7329 = CARTESIAN_POINT ( 'NONE',  ( -5.405949406250003975, -9.363379034771801557, -198.3437500020484094 ) ) ;
#7330 = CARTESIAN_POINT ( 'NONE',  ( -5.405949406250003975, -9.363379034771801557, -99.53125000204839523 ) ) ;
#7331 = CARTESIAN_POINT ( 'NONE',  ( 5.000000000000000000, 8.660254037844385522, -186.6250000040967905 ) ) ;
#7332 = CARTESIAN_POINT ( 'NONE',  ( -5.405949406250003975, -9.363379034771801557, -109.8437500020483810 ) ) ;
#7333 = CARTESIAN_POINT ( 'NONE',  ( 10.81189881249999551, -6.242252689847874514, -180.1562500020484094 ) ) ;
#7334 = CARTESIAN_POINT ( 'NONE',  ( -9.999999999999998224, 1.224646799147353059E-15, -107.7499999999999858 ) ) ;
#7335 = CARTESIAN_POINT ( 'NONE',  ( 5.000000000000000000, 8.660254037844385522, -181.7500000000000000 ) ) ;
#7336 = CARTESIAN_POINT ( 'NONE',  ( -5.405949406249996869, 9.363379034771805109, -193.0312500020484094 ) ) ;
#7337 = CARTESIAN_POINT ( 'NONE',  ( -10.81189881249999729, 1.324075727343319199E-15, -57.59375000204835970 ) ) ;
#7338 = CARTESIAN_POINT ( 'NONE',  ( -5.405949406250003975, -9.363379034771801557, -39.34375000204837391 ) ) ;
#7339 = CARTESIAN_POINT ( 'NONE',  ( 5.000000000000000000, 8.660254037844385522, -168.6250000040967905 ) ) ;
#7340 = CARTESIAN_POINT ( 'NONE',  ( -10.81189881249999729, 1.324075727343319199E-15, -9.781250002048352599 ) ) ;
#7341 = CARTESIAN_POINT ( 'NONE',  ( -2.293366432827344421E-15, -12.48450537969573659, -18.21875000204836681 ) ) ;
#7342 = CARTESIAN_POINT ( 'NONE',  ( 10.00000000000051159, -5.773502691895965988, -92.50000000409676204 ) ) ;
#7343 = CARTESIAN_POINT ( 'NONE',  ( 10.81189881249999729, 0.000000000000000000, -130.3437500020484094 ) ) ;
#7344 = CARTESIAN_POINT ( 'NONE',  ( -2.121150477449813534E-15, -11.54700538379251284, -104.3749999999999716 ) ) ;
#7345 = CARTESIAN_POINT ( 'NONE',  ( 10.81189881249999551, -6.242252689847874514, -25.65625000204838102 ) ) ;
#7346 = DIRECTION ( 'NONE',  ( 0.08682659386424779191, 0.08682659386424779191, 0.9924325091389669673 ) ) ;
#7347 = VECTOR ( 'NONE', #40907, 1000.000000000000000 ) ;
#7348 = CARTESIAN_POINT ( 'NONE',  ( -9.999999999999998224, 1.224646799147353059E-15, -58.24999999999997158 ) ) ;
#7349 = CARTESIAN_POINT ( 'NONE',  ( 7.644554776091147741E-16, 12.48450537969573659, -122.6562500020483952 ) ) ;
#7350 = CARTESIAN_POINT ( 'NONE',  ( 10.81189881249999551, -6.242252689847874514, -106.6562500020484094 ) ) ;
#7351 = EDGE_CURVE ( 'NONE', #7904, #11384, #30159, .T. ) ;
#7352 = EDGE_LOOP ( 'NONE', ( #40205, #9413, #39807, #9855 ) ) ;
#7353 = DIRECTION ( 'NONE',  ( -1.000000000000000000, 0.000000000000000000, -0.000000000000000000 ) ) ;
#7354 = CARTESIAN_POINT ( 'NONE',  ( 5.000000000000000000, 8.660254037844385522, -104.1250000040967763 ) ) ;
#7355 = CYLINDRICAL_SURFACE ( 'NONE', #36702, 9.999999999999998224 ) ;
#7356 = CARTESIAN_POINT ( 'NONE',  ( -5.405949406249996869, 9.363379034771805109, -54.84375000204835970 ) ) ;
#7357 = EDGE_LOOP ( 'NONE', ( #40500, #8968, #18834, #24615 ) ) ;
#7358 = CARTESIAN_POINT ( 'NONE',  ( -5.000000000000003553, -8.660254037844383745, -35.49999999999997868 ) ) ;
#7359 = CARTESIAN_POINT ( 'NONE',  ( 10.81189881249999729, 6.242252689847867408, -37.40625000204836681 ) ) ;
#7360 = CARTESIAN_POINT ( 'NONE',  ( -9.999999999999998224, 0.000000000000000000, -99.99999999999998579 ) ) ;
#7361 = CARTESIAN_POINT ( 'NONE',  ( 9.999999999999996447, -5.773502691896262640, -40.00000000409676204 ) ) ;
#7362 = CARTESIAN_POINT ( 'NONE',  ( 10.81189881249999729, 0.000000000000000000, -142.5312500020483810 ) ) ;
#7363 = CARTESIAN_POINT ( 'NONE',  ( -9.999999999999998224, 1.224646799147353059E-15, -162.1250000040967905 ) ) ;
#7364 = EDGE_LOOP ( 'NONE', ( #25566, #16658, #11441, #32016 ) ) ;
#7365 =( BOUNDED_CURVE ( )  B_SPLINE_CURVE ( 2, ( #3536, #736, #3751, #29656, #42585, #30088, #16672 ),
 .UNSPECIFIED., .F., .F. ) 
 B_SPLINE_CURVE_WITH_KNOTS ( ( 3, 2, 2, 3 ),
 ( 0.2462686567164180107, 0.2475124378109453960, 0.2487562189054727535, 0.2500000000000001110 ),
 .UNSPECIFIED. ) 
 CURVE ( )  GEOMETRIC_REPRESENTATION_ITEM ( )  RATIONAL_B_SPLINE_CURVE ( ( 0.9999999999999880096, 0.8660254037844506980, 1.000000000000000000, 0.8660254037844387076, 1.000000000000000000, 0.8660254037844267172, 1.000000000000011990 ) ) 
 REPRESENTATION_ITEM ( '' )  );
#7366 = ADVANCED_FACE ( 'NONE', ( #600 ), #19571, .T. ) ;
#7367 = ORIENTED_EDGE ( 'NONE', *, *, #39117, .F. ) ;
#7368 = LINE ( 'NONE', #26794, #12770 ) ;
#7369 = DIRECTION ( 'NONE',  ( -0.000000000000000000, -0.000000000000000000, 1.000000000000000000 ) ) ;
#7371 = EDGE_CURVE ( 'NONE', #848, #6885, #17177, .T. ) ;
#7370 = CARTESIAN_POINT ( 'NONE',  ( 5.405949406249999534, 9.363379034771803333, -166.0937500020484094 ) ) ;
#7372 = CARTESIAN_POINT ( 'NONE',  ( 10.81189881249999907, 6.242252689847868297, -196.4062500020484379 ) ) ;
#7373 = CARTESIAN_POINT ( 'NONE',  ( 10.81189881249999907, 6.242252689847868297, -14.71875000204837036 ) ) ;
#7374 = FACE_OUTER_BOUND ( 'NONE', #28827, .T. ) ;
#7375 = CARTESIAN_POINT ( 'NONE',  ( 10.81189881249999551, -6.242252689847874514, -154.4687500020484094 ) ) ;
#7376 = CARTESIAN_POINT ( 'NONE',  ( -10.81189881249999729, 1.324075727343319199E-15, -135.5937500020483810 ) ) ;
#7377 = CARTESIAN_POINT ( 'NONE',  ( -5.405949406249996869, 9.363379034771805109, -103.0312500020483952 ) ) ;
#7378 = CARTESIAN_POINT ( 'NONE',  ( -10.81189881249999907, -6.242252689847864744, -115.9687500020483810 ) ) ;
#7379 = CARTESIAN_POINT ( 'NONE',  ( 9.999999999999998224, 0.000000000000000000, -195.8750000040967905 ) ) ;
#7380 = CARTESIAN_POINT ( 'NONE',  ( -2.293366432827344421E-15, -12.48450537969573659, -121.9062500020483952 ) ) ;
#7381 = CARTESIAN_POINT ( 'NONE',  ( -10.81189881249999907, -6.242252689847864744, -10.96875000204836859 ) ) ;
#7382 = CARTESIAN_POINT ( 'NONE',  ( -5.405949406250003975, -9.363379034771801557, -133.8437500020484094 ) ) ;
#7383 = DIRECTION ( 'NONE',  ( -0.000000000000000000, -0.000000000000000000, 1.000000000000000000 ) ) ;
#7384 = CARTESIAN_POINT ( 'NONE',  ( 7.070501591499376803E-16, 11.54700538379251284, -110.0000000040968047 ) ) ;
#7385 = CARTESIAN_POINT ( 'NONE',  ( 4.999999999999992006, -8.660254037844389075, -155.2500000000000000 ) ) ;
#7386 = CARTESIAN_POINT ( 'NONE',  ( 9.999999999999996447, -5.773502691896262640, -18.62499999999997868 ) ) ;
#7387 = CARTESIAN_POINT ( 'NONE',  ( 5.405949406249999534, 9.363379034771803333, -82.09375000204836681 ) ) ;
#7388 = CARTESIAN_POINT ( 'NONE',  ( -10.81189881249999729, 1.324075727343319199E-15, -66.59375000204836681 ) ) ;
#7389 = DIRECTION ( 'NONE',  ( -0.000000000000000000, -0.000000000000000000, 1.000000000000000000 ) ) ;
#7390 = CARTESIAN_POINT ( 'NONE',  ( -10.81189881249999907, -6.242252689847864744, -45.65625000204837391 ) ) ;
#7391 = CARTESIAN_POINT ( 'NONE',  ( -10.81189881249999729, 6.242252689847871849, -48.71875000204836681 ) ) ;
#7392 = CARTESIAN_POINT ( 'NONE',  ( -5.000000000000003553, -8.660254037844383745, -142.0000000000000000 ) ) ;
#7393 = CARTESIAN_POINT ( 'NONE',  ( -5.405949406250003975, -9.363379034771801557, -150.3437500020483810 ) ) ;
#7394 = CARTESIAN_POINT ( 'NONE',  ( -9.999999999999998224, 5.773502691896259087, -130.3750000000000000 ) ) ;
#7395 = CARTESIAN_POINT ( 'NONE',  ( 10.81189881249999729, 6.242252689847867408, -133.4062500020483810 ) ) ;
#7396 = CARTESIAN_POINT ( 'NONE',  ( -9.999999999999998224, 1.224646799147353059E-15, -94.24999999999998579 ) ) ;
#7397 = CARTESIAN_POINT ( 'NONE',  ( 9.999999999999996447, -5.773502691896262640, -83.12499999999998579 ) ) ;
#7398 = CARTESIAN_POINT ( 'NONE',  ( 5.405949406249999534, 9.363379034771803333, -20.78125000204836326 ) ) ;
#7399 = ORIENTED_EDGE ( 'NONE', *, *, #35671, .F. ) ;
#7400 = CARTESIAN_POINT ( 'NONE',  ( -10.81189881249999729, -6.242252689847864744, -110.1562500020483952 ) ) ;
#7401 = CARTESIAN_POINT ( 'NONE',  ( 10.00000000000000000, 5.773502691896255534, -122.2500000040968047 ) ) ;
#7402 = DIRECTION ( 'NONE',  ( -0.000000000000000000, -0.000000000000000000, 1.000000000000000000 ) ) ;
#7403 = CARTESIAN_POINT ( 'NONE',  ( 7.070501591499377789E-16, 11.54700538379251284, -33.50000000409675494 ) ) ;
#7404 = EDGE_CURVE ( 'NONE', #10629, #33014, #37570, .T. ) ;
#7405 = LINE ( 'NONE', #30719, #2865 ) ;
#7406 = CARTESIAN_POINT ( 'NONE',  ( -5.405949406249996869, 9.363379034771805109, -50.53125000204835970 ) ) ;
#7407 = CARTESIAN_POINT ( 'NONE',  ( 7.070501591499376803E-16, 11.54700538379251284, -76.62500000000000000 ) ) ;
#7408 = CARTESIAN_POINT ( 'NONE',  ( -10.81189881249999907, -6.242252689847864744, -155.1562500020484094 ) ) ;
#7409 = CARTESIAN_POINT ( 'NONE',  ( 5.405949406249999534, 9.363379034771803333, -136.0937500020483810 ) ) ;
#7410 = ORIENTED_EDGE ( 'NONE', *, *, #14435, .T. ) ;
#7411 = ORIENTED_EDGE ( 'NONE', *, *, #15911, .T. ) ;
#7412 = ORIENTED_EDGE ( 'NONE', *, *, #29392, .F. ) ;
#7413 = PERSON_AND_ORGANIZATION ( #11915, #17965 ) ;
#7415 = VERTEX_POINT ( 'NONE', #10493 ) ;
#7414 = CARTESIAN_POINT ( 'NONE',  ( 10.81189881249999907, 6.242252689847868297, -113.7187500020483810 ) ) ;
#7416 = CARTESIAN_POINT ( 'NONE',  ( -9.999999999999998224, 1.224646799147353059E-15, -129.1250000040967620 ) ) ;
#7417 = CARTESIAN_POINT ( 'NONE',  ( 10.81189881249999551, -6.242252689847874514, -188.9687500020484094 ) ) ;
#7418 = CARTESIAN_POINT ( 'NONE',  ( 5.405949406249992428, -9.363379034771808662, -36.09375000204836681 ) ) ;
#7419 = CARTESIAN_POINT ( 'NONE',  ( 4.947751128964601897, -9.422943186768698354, 6.544024882825221806E-15 ) ) ;
#7420 = CARTESIAN_POINT ( 'NONE',  ( -5.000020801129981152, 8.660290040615111096, 0.000000000000000000 ) ) ;
#7421 = CARTESIAN_POINT ( 'NONE',  ( 10.81189881249999729, 0.000000000000000000, -178.3437500020483810 ) ) ;
#7422 = CARTESIAN_POINT ( 'NONE',  ( -5.405949406249996869, 9.363379034771805109, -159.8437500020484094 ) ) ;
#7423 = CARTESIAN_POINT ( 'NONE',  ( -10.81189881249999907, -6.242252689847864744, -138.4687500020484094 ) ) ;
#7424 = CARTESIAN_POINT ( 'NONE',  ( 10.81189881249999729, 0.000000000000000000, -166.3437500020484094 ) ) ;
#7425 = CARTESIAN_POINT ( 'NONE',  ( 9.999999999999479527, 5.773502691896553074, -126.7500000040967478 ) ) ;
#7426 = CARTESIAN_POINT ( 'NONE',  ( -9.999999999999998224, 1.224646799147353059E-15, -41.74999999999997868 ) ) ;
#7427 = CARTESIAN_POINT ( 'NONE',  ( 9.999999999999998224, 0.000000000000000000, -176.0000000000000000 ) ) ;
#7428 = CARTESIAN_POINT ( 'NONE',  ( 10.81189881249999907, 6.242252689847868297, -92.71875000204836681 ) ) ;
#7429 = CARTESIAN_POINT ( 'NONE',  ( 9.999999999999998224, 0.000000000000000000, -34.99999999999997868 ) ) ;
#7430 = CARTESIAN_POINT ( 'NONE',  ( 5.405949406249999534, 9.363379034771803333, -64.28125000204836681 ) ) ;
#7431 = CARTESIAN_POINT ( 'NONE',  ( -2.121150477449813534E-15, -11.54700538379251284, -124.2500000040967763 ) ) ;
#7432 = CARTESIAN_POINT ( 'NONE',  ( -5.405949406249996869, 9.363379034771805109, -174.8437500020484094 ) ) ;
#7433 = CARTESIAN_POINT ( 'NONE',  ( -2.293366432827344421E-15, -12.48450537969573659, -121.9062500020483952 ) ) ;
#7434 = CARTESIAN_POINT ( 'NONE',  ( -2.293366432827344421E-15, -12.48450537969573659, -153.4062500020483810 ) ) ;
#7435 = CARTESIAN_POINT ( 'NONE',  ( -10.81189881249999729, 1.324075727343319199E-15, -51.78125000204835970 ) ) ;
#7436 = CARTESIAN_POINT ( 'NONE',  ( -2.121150477449813534E-15, -11.54700538379251284, -127.2500000040967905 ) ) ;
#7437 = CARTESIAN_POINT ( 'NONE',  ( 9.999999999999998224, 0.000000000000000000, -109.9999999999999858 ) ) ;
#7438 = VERTEX_POINT ( 'NONE', #3619 ) ;
#7439 = CARTESIAN_POINT ( 'NONE',  ( 10.81189881249999729, 0.000000000000000000, -135.0312500020484094 ) ) ;
#7440 = CARTESIAN_POINT ( 'NONE',  ( -9.999999999999998224, 5.773502691896259087, -154.7500000040967620 ) ) ;
#7441 = CARTESIAN_POINT ( 'NONE',  ( 10.81189881249999551, -6.242252689847874514, -151.6562500020484094 ) ) ;
#7442 = CARTESIAN_POINT ( 'NONE',  ( 10.81189881249999907, 6.242252689847868297, -190.4062500020484094 ) ) ;
#7443 = CARTESIAN_POINT ( 'NONE',  ( -5.405949406250003975, -9.363379034771801557, -81.34375000204838102 ) ) ;
#7444 = VECTOR ( 'NONE', #7916, 1000.000000000000000 ) ;
#7445 = ORIENTED_EDGE ( 'NONE', *, *, #1691, .T. ) ;
#7446 = CARTESIAN_POINT ( 'NONE',  ( -2.121150477449813534E-15, -11.54700538379251284, -50.37499999999997868 ) ) ;
#7447 = CARTESIAN_POINT ( 'NONE',  ( 10.81189881249999907, 6.242252689847868297, -181.2187500020484094 ) ) ;
#7448 = CARTESIAN_POINT ( 'NONE',  ( -9.999999999999998224, 1.224646799147353059E-15, -69.12500000409677625 ) ) ;
#7449 = EDGE_CURVE ( 'NONE', #9909, #11999, #36184, .T. ) ;
#7450 = AXIS2_PLACEMENT_3D ( 'NONE', #42023, #38585, #15478 ) ;
#7451 = CARTESIAN_POINT ( 'NONE',  ( -5.000000000000003553, -8.660254037844383745, -109.3750000040967763 ) ) ;
#7452 =( BOUNDED_CURVE ( )  B_SPLINE_CURVE ( 2, ( #17740, #40614, #4171, #4600, #24253, #30934, #27908 ),
 .UNSPECIFIED., .F., .F. ) 
 B_SPLINE_CURVE_WITH_KNOTS ( ( 3, 2, 2, 3 ),
 ( 0.8805970149253734558, 0.8818407960199008411, 0.8830845771144281153, 0.8843283582089555006 ),
 .UNSPECIFIED. ) 
 CURVE ( )  GEOMETRIC_REPRESENTATION_ITEM ( )  RATIONAL_B_SPLINE_CURVE ( ( 0.9999999999999641398, 0.8660254037844745678, 1.000000000000000000, 0.8660254037844387076, 1.000000000000000000, 0.8660254037844148378, 1.000000000000023981 ) ) 
 REPRESENTATION_ITEM ( '' )  );
#7453 = DIRECTION ( 'NONE',  ( -0.000000000000000000, -0.000000000000000000, -1.000000000000000000 ) ) ;
#7454 = EDGE_CURVE ( 'NONE', #27111, #16738, #32754, .T. ) ;
#7455 = CARTESIAN_POINT ( 'NONE',  ( -10.81189881249999729, 6.242252689847871849, -72.90625000204838102 ) ) ;
#7456 = CARTESIAN_POINT ( 'NONE',  ( -10.81189881249999729, 1.324075727343319199E-15, -56.28125000204836681 ) ) ;
#7457 = CARTESIAN_POINT ( 'NONE',  ( -10.00000000000000000, -5.773502691896251982, -52.50000000409676915 ) ) ;
#7458 = CARTESIAN_POINT ( 'NONE',  ( -10.81189881249999729, 1.324075727343319199E-15, -6.593750002048370362 ) ) ;
#7459 = CARTESIAN_POINT ( 'NONE',  ( 9.999999999999742428, 5.773502691896404748, -158.2500000040967905 ) ) ;
#7460 = CARTESIAN_POINT ( 'NONE',  ( 10.81189881249999907, 6.242252689847868297, -173.9062500020484094 ) ) ;
#7461 = CARTESIAN_POINT ( 'NONE',  ( -10.81189881249999729, 6.242252689847871849, -5.406250002048363257 ) ) ;
#7462 = CARTESIAN_POINT ( 'NONE',  ( 5.000000000000000000, 8.660254037844385522, -147.6250000040967905 ) ) ;
#7463 = CARTESIAN_POINT ( 'NONE',  ( 10.00000000000012257, -5.773502691896187144, -161.1250000000000568 ) ) ;
#7464 = CARTESIAN_POINT ( 'NONE',  ( -9.999999999999998224, 1.224646799147353059E-15, -89.74999999999998579 ) ) ;
#7465 = CARTESIAN_POINT ( 'NONE',  ( 0.000000000000000000, 0.000000000000000000, -200.0000000000000000 ) ) ;
#7466 = CARTESIAN_POINT ( 'NONE',  ( -9.999999999999998224, 1.224646799147353059E-15, -139.2499999999999716 ) ) ;
#7468 = ORIENTED_EDGE ( 'NONE', *, *, #37933, .T. ) ;
#7467 = CARTESIAN_POINT ( 'NONE',  ( 10.81189881249999907, 6.242252689847868297, -82.40625000204836681 ) ) ;
#7469 = ADVANCED_FACE ( 'NONE', ( #32970, #3399 ), #16534, .F. ) ;
#7470 = VERTEX_POINT ( 'NONE', #41112 ) ;
#7471 = ORIENTED_EDGE ( 'NONE', *, *, #8724, .F. ) ;
#7472 = CARTESIAN_POINT ( 'NONE',  ( 5.405949406249999534, 9.363379034771803333, -23.59375000204835970 ) ) ;
#7473 = CARTESIAN_POINT ( 'NONE',  ( 10.81189881249999907, 6.242252689847868297, -16.40625000204838102 ) ) ;
#7474 = CARTESIAN_POINT ( 'NONE',  ( 10.81189881249999729, 0.000000000000000000, -68.84375000204836681 ) ) ;
#7475 = CARTESIAN_POINT ( 'NONE',  ( 7.070501591499376803E-16, 11.54700538379251284, -93.12500000000000000 ) ) ;
#7476 = CARTESIAN_POINT ( 'NONE',  ( 7.070501591499377789E-16, 11.54700538379251284, -46.62499999999997158 ) ) ;
#7477 = EDGE_CURVE ( 'NONE', #30730, #6810, #8130, .T. ) ;
#7478 = VECTOR ( 'NONE', #14412, 1000.000000000000000 ) ;
#7479 = CARTESIAN_POINT ( 'NONE',  ( 7.644554776091147741E-16, 12.48450537969573659, -185.4687500020483810 ) ) ;
#7480 = CARTESIAN_POINT ( 'NONE',  ( -5.405949406249996869, 9.363379034771805109, -167.3437500020484094 ) ) ;
#7481 = CARTESIAN_POINT ( 'NONE',  ( 10.81189881249999551, -6.242252689847874514, 0.03124999795165228286 ) ) ;
#7482 = CARTESIAN_POINT ( 'NONE',  ( 5.000000000000000000, 8.660254037844385522, -59.12500000409676204 ) ) ;
#7483 = CARTESIAN_POINT ( 'NONE',  ( 9.999999999999998224, 0.000000000000000000, -141.5000000000000000 ) ) ;
#7484 = DIRECTION ( 'NONE',  ( 1.000000000000000000, 0.000000000000000000, 0.000000000000000000 ) ) ;
#7485 = CARTESIAN_POINT ( 'NONE',  ( -5.405949406249996869, 9.363379034771805109, -113.3437500020483810 ) ) ;
#7486 = CARTESIAN_POINT ( 'NONE',  ( 9.999999999999998224, 0.000000000000000000, -54.87500000409675494 ) ) ;
#7487 = CARTESIAN_POINT ( 'NONE',  ( -5.405949406249996869, 9.363379034771805109, -91.03125000204838102 ) ) ;
#7488 = CARTESIAN_POINT ( 'NONE',  ( -10.81189881249999729, -6.242252689847864744, -102.4687500020483810 ) ) ;
#7489 = CARTESIAN_POINT ( 'NONE',  ( 10.81189881249999729, 0.000000000000000000, -65.84375000204836681 ) ) ;
#7490 = CARTESIAN_POINT ( 'NONE',  ( 5.405949406249999534, 9.363379034771803333, -73.28125000204838102 ) ) ;
#7491 = CARTESIAN_POINT ( 'NONE',  ( 5.000000000000000000, 8.660254037844385522, -165.6250000040967905 ) ) ;
#7492 =( BOUNDED_CURVE ( )  B_SPLINE_CURVE ( 2, ( #30670, #37991, #4976, #18122, #31317, #1532, #5188 ),
 .UNSPECIFIED., .F., .F. ) 
 B_SPLINE_CURVE_WITH_KNOTS ( ( 3, 2, 2, 3 ),
 ( 0.4813432835820896649, 0.4825870646766170502, 0.4838308457711443800, 0.4850746268656717652 ),
 .UNSPECIFIED. ) 
 CURVE ( )  GEOMETRIC_REPRESENTATION_ITEM ( )  RATIONAL_B_SPLINE_CURVE ( ( 0.9999999999999880096, 0.8660254037844506980, 1.000000000000000000, 0.8660254037844387076, 1.000000000000000000, 0.8660254037844267172, 1.000000000000011990 ) ) 
 REPRESENTATION_ITEM ( '' )  );
#7493 = CARTESIAN_POINT ( 'NONE',  ( 7.644554776091147741E-16, 12.48450537969573659, -160.1562500020484094 ) ) ;
#7494 = CARTESIAN_POINT ( 'NONE',  ( -10.81189881249999729, 1.324075727343319199E-15, -168.7812500020484094 ) ) ;
#7495 = CARTESIAN_POINT ( 'NONE',  ( 7.644554776091147741E-16, 12.48450537969573659, 0.5312499979516493998 ) ) ;
#7496 = CARTESIAN_POINT ( 'NONE',  ( -9.999999999999479527, -5.773502691896549521, -109.1249999999999716 ) ) ;
#7497 = CARTESIAN_POINT ( 'NONE',  ( -10.81189881249999907, -6.242252689847864744, -109.9687500020483668 ) ) ;
#7498 = CARTESIAN_POINT ( 'NONE',  ( -4.999999999999996447, 8.660254037844387298, -62.99999999999997158 ) ) ;
#7499 = CARTESIAN_POINT ( 'NONE',  ( -2.121150477449813534E-15, -11.54700538379251284, -72.87499999999995737 ) ) ;
#7500 = CARTESIAN_POINT ( 'NONE',  ( -10.81189881249999729, 6.242252689847871849, -2.406250002048360592 ) ) ;
#7501 = CARTESIAN_POINT ( 'NONE',  ( 5.000000000000000000, 8.660254037844385522, -89.12500000409677625 ) ) ;
#7502 = EDGE_CURVE ( 'NONE', #7578, #22008, #25989, .T. ) ;
#7503 = CARTESIAN_POINT ( 'NONE',  ( -2.121150477449813534E-15, -11.54700538379251284, -168.8750000000000000 ) ) ;
#7504 = CARTESIAN_POINT ( 'NONE',  ( -10.81189881249999729, 6.242252689847871849, -99.90625000204838102 ) ) ;
#7505 = CARTESIAN_POINT ( 'NONE',  ( -10.81189881249999729, -6.242252689847864744, -86.15625000204836681 ) ) ;
#7506 = EDGE_CURVE ( 'NONE', #41312, #7415, #24538, .T. ) ;
#7507 =( BOUNDED_CURVE ( )  B_SPLINE_CURVE ( 2, ( #4271, #14163, #33635, #10943, #37714, #37279, #4482 ),
 .UNSPECIFIED., .F., .F. ) 
 B_SPLINE_CURVE_WITH_KNOTS ( ( 3, 2, 2, 3 ),
 ( 0.1567164179104477695, 0.1579601990049751270, 0.1592039800995025123, 0.1604477611940298698 ),
 .UNSPECIFIED. ) 
 CURVE ( )  GEOMETRIC_REPRESENTATION_ITEM ( )  RATIONAL_B_SPLINE_CURVE ( ( 1.000000000000000000, 0.8660254037844387076, 1.000000000000000000, 0.8660254037844387076, 1.000000000000000000, 0.8660254037844357100, 1.000000000000003109 ) ) 
 REPRESENTATION_ITEM ( '' )  );
#7508 = CARTESIAN_POINT ( 'NONE',  ( 9.999999999999996447, -5.773502691896262640, -73.00000000409676204 ) ) ;
#7509 = CARTESIAN_POINT ( 'NONE',  ( 7.070501591499376803E-16, 11.54700538379251284, -19.62499999999997868 ) ) ;
#7510 = CARTESIAN_POINT ( 'NONE',  ( 5.405949406249999534, 9.363379034771803333, -32.59375000204836681 ) ) ;
#7511 = ORIENTED_EDGE ( 'NONE', *, *, #38584, .F. ) ;
#7512 = CARTESIAN_POINT ( 'NONE',  ( -5.405949406249996869, 9.363379034771805109, -197.5312500020484094 ) ) ;
#7513 = EDGE_CURVE ( 'NONE', #36795, #36659, #30795, .T. ) ;
#7514 = CARTESIAN_POINT ( 'NONE',  ( -5.405949406250003975, -9.363379034771801557, -29.03125000204837036 ) ) ;
#7515 = CARTESIAN_POINT ( 'NONE',  ( -2.293366432827344421E-15, -12.48450537969573659, -16.71875000204836326 ) ) ;
#7516 = FACE_OUTER_BOUND ( 'NONE', #8391, .T. ) ;
#7517 = CARTESIAN_POINT ( 'NONE',  ( -2.121150477449813534E-15, -11.54700538379251284, -2.750000004096753159 ) ) ;
#7518 = CARTESIAN_POINT ( 'NONE',  ( 10.81189881249999907, 6.242252689847868297, -137.9062500020483810 ) ) ;
#7519 = CARTESIAN_POINT ( 'NONE',  ( -9.999999999999998224, 1.224646799147353059E-15, -190.2500000000000000 ) ) ;
#7520 = CARTESIAN_POINT ( 'NONE',  ( -4.999999999999996447, 8.660254037844387298, -123.0000000000000000 ) ) ;
#7522 = ORIENTED_EDGE ( 'NONE', *, *, #26988, .F. ) ;
#7521 = CARTESIAN_POINT ( 'NONE',  ( 7.644554776091147741E-16, 12.48450537969573659, -110.6562500020483952 ) ) ;
#7523 = CARTESIAN_POINT ( 'NONE',  ( -9.999999999999998224, 0.000000000000000000, -99.99999999999998579 ) ) ;
#7524 = ORIENTED_EDGE ( 'NONE', *, *, #38472, .T. ) ;
#7525 = ORIENTED_EDGE ( 'NONE', *, *, #7371, .T. ) ;
#7526 = EDGE_CURVE ( 'NONE', #30761, #22978, #18542, .T. ) ;
#7527 = CARTESIAN_POINT ( 'NONE',  ( 10.81189881249999907, 6.242252689847868297, -41.90625000204836681 ) ) ;
#7528 = DATE_AND_TIME ( #23082, #22156 ) ;
#7529 = CARTESIAN_POINT ( 'NONE',  ( 5.405949406249999534, 9.363379034771803333, -95.59375000204838102 ) ) ;
#7530 = CARTESIAN_POINT ( 'NONE',  ( -9.999999999999998224, 0.000000000000000000, -99.99999999999998579 ) ) ;
#7531 = DIRECTION ( 'NONE',  ( -0.000000000000000000, -0.000000000000000000, 1.000000000000000000 ) ) ;
#7532 = CARTESIAN_POINT ( 'NONE',  ( 5.405949406249992428, -9.363379034771808662, -195.0937500020484094 ) ) ;
#7533 = CARTESIAN_POINT ( 'NONE',  ( -5.405949406249996869, 9.363379034771805109, -170.5312500020484094 ) ) ;
#7534 = CARTESIAN_POINT ( 'NONE',  ( 7.070501591499376803E-16, 11.54700538379251284, -138.1250000000000000 ) ) ;
#7535 = CARTESIAN_POINT ( 'NONE',  ( -10.81189881249999729, -6.242252689847864744, -123.4687500020483952 ) ) ;
#7536 = CARTESIAN_POINT ( 'NONE',  ( 5.405949406249992428, -9.363379034771808662, -97.59375000204838102 ) ) ;
#7537 = CARTESIAN_POINT ( 'NONE',  ( -9.999999999999998224, 1.224646799147353059E-15, -200.0000000000000000 ) ) ;
#7538 = CARTESIAN_POINT ( 'NONE',  ( -5.405949406249996869, 9.363379034771805109, -103.0312500020483952 ) ) ;
#7539 = CARTESIAN_POINT ( 'NONE',  ( 5.000000000000000000, 8.660254037844385522, -188.1250000040967905 ) ) ;
#7540 = CARTESIAN_POINT ( 'NONE',  ( -5.405949406249996869, 9.363379034771805109, -107.3437500020483810 ) ) ;
#7541 = CARTESIAN_POINT ( 'NONE',  ( 10.81189881249999729, 0.000000000000000000, -177.0312500020483810 ) ) ;
#7542 = CARTESIAN_POINT ( 'NONE',  ( -4.999999999999996447, 8.660254037844387298, -180.0000000000000000 ) ) ;
#7543 = FACE_OUTER_BOUND ( 'NONE', #32058, .T. ) ;
#7544 = CARTESIAN_POINT ( 'NONE',  ( 10.81189881249999729, 0.000000000000000000, -196.5312500020484094 ) ) ;
#7545 = CARTESIAN_POINT ( 'NONE',  ( 7.644554776091147741E-16, 12.48450537969573659, -50.46875000204835970 ) ) ;
#7546 = AXIS2_PLACEMENT_3D ( 'NONE', #35033, #5462, #15361 ) ;
#7547 = CARTESIAN_POINT ( 'NONE',  ( 10.81189881249999551, -6.242252689847874514, -38.96875000204835970 ) ) ;
#7548 = CARTESIAN_POINT ( 'NONE',  ( -10.00000000000000000, -5.773502691896251982, -171.0000000040967905 ) ) ;
#7549 = CARTESIAN_POINT ( 'NONE',  ( 10.81189881249999907, 6.242252689847868297, -10.40625000204838102 ) ) ;
#7550 = CARTESIAN_POINT ( 'NONE',  ( 5.405949406249999534, 9.363379034771803333, -22.09375000204835615 ) ) ;
#7551 = DIRECTION ( 'NONE',  ( -1.000000000000000000, 0.000000000000000000, 0.000000000000000000 ) ) ;
#7552 = CARTESIAN_POINT ( 'NONE',  ( 10.81189881249999907, 6.242252689847868297, -128.7187500020483810 ) ) ;
#7553 = CARTESIAN_POINT ( 'NONE',  ( -5.000000000000003553, -8.660254037844383745, -93.99999999999998579 ) ) ;
#7554 = CARTESIAN_POINT ( 'NONE',  ( 5.405949406249992428, -9.363379034771808662, -28.78125000204837036 ) ) ;
#7555 = CARTESIAN_POINT ( 'NONE',  ( 9.999999999999996447, -5.773502691896262640, -115.0000000040967763 ) ) ;
#7556 = CARTESIAN_POINT ( 'NONE',  ( -2.275517850991317657E-15, -20.00000000000000000, -235.0000000000000000 ) ) ;
#7557 = CARTESIAN_POINT ( 'NONE',  ( -9.999999999999998224, 1.224646799147353059E-15, -59.74999999999997158 ) ) ;
#7558 = CARTESIAN_POINT ( 'NONE',  ( -10.81189881249999729, 6.242252689847871849, -122.4062500020483952 ) ) ;
#7559 = CARTESIAN_POINT ( 'NONE',  ( -10.81189881249999729, 1.324075727343319199E-15, -104.2812500020483810 ) ) ;
#7560 = EDGE_LOOP ( 'NONE', ( #29972, #2396, #18984, #18332 ) ) ;
#7561 = DIRECTION ( 'NONE',  ( 1.000000000000000000, 0.000000000000000000, 0.000000000000000000 ) ) ;
#7562 = CARTESIAN_POINT ( 'NONE',  ( -5.000000000000003553, -8.660254037844383745, -100.3750000040967905 ) ) ;
#7563 = DIRECTION ( 'NONE',  ( -1.000000000000000000, 0.000000000000000000, 0.000000000000000000 ) ) ;
#7564 = CARTESIAN_POINT ( 'NONE',  ( -2.293366432827344421E-15, -12.48450537969573659, -55.71875000204837391 ) ) ;
#7565 = ORIENTED_EDGE ( 'NONE', *, *, #28598, .F. ) ;
#7566 = CARTESIAN_POINT ( 'NONE',  ( 9.999999999999996447, -5.773502691896262640, -36.62499999999996447 ) ) ;
#7567 = CARTESIAN_POINT ( 'NONE',  ( -2.293366432827344421E-15, -12.48450537969573659, -34.90625000204836681 ) ) ;
#7568 = CARTESIAN_POINT ( 'NONE',  ( 7.070501591499377789E-16, 11.54700538379251284, -165.1249999999999716 ) ) ;
#7569 = CARTESIAN_POINT ( 'NONE',  ( -9.999999999999998224, 1.224646799147353059E-15, -16.24999999999995737 ) ) ;
#7570 = CARTESIAN_POINT ( 'NONE',  ( -9.999999999999998224, 1.224646799147353059E-15, -25.62500000409675849 ) ) ;
#7571 = ADVANCED_FACE ( 'NONE', ( #17598 ), #23899, .F. ) ;
#7572 = CARTESIAN_POINT ( 'NONE',  ( 5.405949406249999534, 9.363379034771803333, -137.7812500020483810 ) ) ;
#7573 =( BOUNDED_CURVE ( )  B_SPLINE_CURVE ( 2, ( #38902, #22294, #2023, #25540, #2445, #25748, #15786 ),
 .UNSPECIFIED., .F., .F. ) 
 B_SPLINE_CURVE_WITH_KNOTS ( ( 3, 2, 2, 3 ),
 ( 0.1082089552238805485, 0.1094527363184079616, 0.1106965174129353746, 0.1119402985074627876 ),
 .UNSPECIFIED. ) 
 CURVE ( )  GEOMETRIC_REPRESENTATION_ITEM ( )  RATIONAL_B_SPLINE_CURVE ( ( 1.000000000000004441, 0.8660254037844343777, 1.000000000000000000, 0.8660254037844387076, 1.000000000000000000, 0.8660254037844282715, 1.000000000000010436 ) ) 
 REPRESENTATION_ITEM ( '' )  );
#7574 = CARTESIAN_POINT ( 'NONE',  ( -9.999999999999998224, 1.224646799147353059E-15, -120.1250000040967905 ) ) ;
#7575 = ORIENTED_EDGE ( 'NONE', *, *, #17475, .T. ) ;
#7576 = CIRCLE ( 'NONE', #11, 5.000000000000002665 ) ;
#7578 = VERTEX_POINT ( 'NONE', #7483 ) ;
#7577 = EDGE_LOOP ( 'NONE', ( #9073, #29878, #38732, #42687 ) ) ;
#7579 = DIRECTION ( 'NONE',  ( -1.000000000000000000, 0.000000000000000000, 0.000000000000000000 ) ) ;
#7580 = EDGE_CURVE ( 'NONE', #24932, #8912, #38958, .T. ) ;
#7581 = CARTESIAN_POINT ( 'NONE',  ( -9.999999999999998224, 1.224646799147353059E-15, -55.62500000409676204 ) ) ;
#7582 = CARTESIAN_POINT ( 'NONE',  ( -5.405949406249996869, 9.363379034771805109, -168.8437500020484094 ) ) ;
#7583 = CARTESIAN_POINT ( 'NONE',  ( -10.81189881249999729, 1.324075727343319199E-15, -194.2812500020484094 ) ) ;
#7584 = CARTESIAN_POINT ( 'NONE',  ( 5.405949406249992428, -9.363379034771808662, -12.09375000204834727 ) ) ;
#7585 = CYLINDRICAL_SURFACE ( 'NONE', #37771, 9.999999999999998224 ) ;
#7586 = CARTESIAN_POINT ( 'NONE',  ( 10.81189881249999729, 0.000000000000000000, -151.3437500020483810 ) ) ;
#7587 = CARTESIAN_POINT ( 'NONE',  ( -10.81189881249999907, -6.242252689847864744, -135.4687500020483810 ) ) ;
#7588 = CARTESIAN_POINT ( 'NONE',  ( 10.81189881249999907, 6.242252689847868297, -107.9062500020483668 ) ) ;
#7589 = CARTESIAN_POINT ( 'NONE',  ( -5.405949406249996869, 9.363379034771805109, -120.8437500020483952 ) ) ;
#7590 = CARTESIAN_POINT ( 'NONE',  ( 7.070501591499377789E-16, 11.54700538379251284, -198.5000000040968189 ) ) ;
#7591 = CARTESIAN_POINT ( 'NONE',  ( -10.81189881249999729, 1.324075727343319199E-15, -126.7812500020483668 ) ) ;
#7592 = CARTESIAN_POINT ( 'NONE',  ( -2.293366432827344421E-15, -12.48450537969573659, -12.21875000204837391 ) ) ;
#7593 = CARTESIAN_POINT ( 'NONE',  ( 5.405949406249999534, 9.363379034771803333, -130.0937500020483810 ) ) ;
#7594 = CARTESIAN_POINT ( 'NONE',  ( -9.999999999999998224, 1.224646799147353059E-15, -63.12500000409676204 ) ) ;
#7595 = DIRECTION ( 'NONE',  ( 0.9961946980917455452, 0.000000000000000000, -0.08715574274765837404 ) ) ;
#7596 = CARTESIAN_POINT ( 'NONE',  ( -4.999999999999996447, 8.660254037844387298, -154.5000000000000000 ) ) ;
#7597 = CARTESIAN_POINT ( 'NONE',  ( 7.070501591499377789E-16, 11.54700538379251284, -24.12499999999997868 ) ) ;
#7598 = CARTESIAN_POINT ( 'NONE',  ( -5.405949406249996869, 9.363379034771805109, -72.84375000204838102 ) ) ;
#7599 = CARTESIAN_POINT ( 'NONE',  ( 5.405949406249999534, 9.363379034771803333, -65.59375000204836681 ) ) ;
#7600 = CARTESIAN_POINT ( 'NONE',  ( -2.121150477449813534E-15, -11.54700538379251284, -116.7500000040967905 ) ) ;
#7601 = CARTESIAN_POINT ( 'NONE',  ( -10.81189881249999729, 6.242252689847871849, -38.40625000204835260 ) ) ;
#7602 = CARTESIAN_POINT ( 'NONE',  ( -5.405949406250003975, -9.363379034771801557, -42.34375000204837391 ) ) ;
#7603 = DIRECTION ( 'NONE',  ( -0.000000000000000000, -0.000000000000000000, 1.000000000000000000 ) ) ;
#7604 = CARTESIAN_POINT ( 'NONE',  ( 5.405949406249999534, 9.363379034771803333, -154.0937500020483810 ) ) ;
#7605 = CARTESIAN_POINT ( 'NONE',  ( 9.999999999999996447, -5.773502691896262640, -132.6249999999999716 ) ) ;
#7606 = CARTESIAN_POINT ( 'NONE',  ( -5.405949406249996869, 9.363379034771805109, -130.0312500020484094 ) ) ;
#7607 = CARTESIAN_POINT ( 'NONE',  ( 10.63231620283895396, 1.921144686730597462, -180.0000000000000000 ) ) ;
#7608 = CARTESIAN_POINT ( 'NONE',  ( 5.000000000000000000, 8.660254037844385522, -85.74999999999998579 ) ) ;
#7609 = CARTESIAN_POINT ( 'NONE',  ( -5.405949406249996869, 9.363379034771805109, -16.03125000204835970 ) ) ;
#7610 = ORIENTED_EDGE ( 'NONE', *, *, #33066, .T. ) ;
#7611 = CARTESIAN_POINT ( 'NONE',  ( 10.81189881249999729, 6.242252689847867408, -109.4062500020483952 ) ) ;
#7612 = CARTESIAN_POINT ( 'NONE',  ( -4.999999999999996447, 8.660254037844387298, -127.8750000040967905 ) ) ;
#7613 = CARTESIAN_POINT ( 'NONE',  ( 4.999999999999992006, -8.660254037844389075, -185.2500000000000000 ) ) ;
#7614 = VECTOR ( 'NONE', #37563, 1000.000000000000000 ) ;
#7615 = CARTESIAN_POINT ( 'NONE',  ( 9.999999999999996447, -5.773502691896262640, -31.00000000409674783 ) ) ;
#7616 = CARTESIAN_POINT ( 'NONE',  ( -9.999999999999998224, 1.224646799147353059E-15, -11.74999999999995559 ) ) ;
#7617 = CARTESIAN_POINT ( 'NONE',  ( 10.81189881249999551, -6.242252689847874514, -55.65625000204837391 ) ) ;
#7618 =( BOUNDED_CURVE ( )  B_SPLINE_CURVE ( 2, ( #30692, #27022, #24223, #40168, #23786, #1125, #14248, #11029, #37373, #24868, #38437, #38652, #34792, #15334, #5433, #5006, #5212, #41869, #41663, #28531, #18584, #12306, #5646, #21612, #19007, #35215, #32192, #12099, #18148, #28949, #25293, #31343, #1989, #42086, #18368, #11885, #25503, #9087, #1773, #31556, #8880, #2619, #22255, #41450, #28103, #31772, #35004, #15751, #22043, #18794, #31983, #14903, #41230, #2409, #15540, #24656, #28742, #2201, #35425, #28310, #5852, #37799, #8244, #21392, #34576, #25081, #11667, #38017, #8461, #15115, #38226, #8671, #21824, #19841, #23097, #6064, #36466, #9288, #23311, #42295, #39696, #234, #35637, #19423, #13141, #32404, #20055, #36049, #3038, #9504, #6902, #12928, #15960, #16165, #39488, #12518, #26123, #29156, #3455, #26336, #6485, #32816, #16591, #29361, #22460, #18, #25711, #9711, #2826, #39277, #3247, #19214, #13356, #39066, #33250, #22892, #42500, #16373, #12717, #32613, #26547, #25914, #30003, #22673, #35844, #19632, #6277, #38861, #10132, #29573, #9921, #36260, #6690, #33026, #29794, #3676, #16804, #23954, #17444, #20908, #10340, #10975, #14196, #30640, #26757, #17656, #11193, #36887, #13778, #36678, #7973, #27179, #40532, #40119, #866, #7333, #30851, #23736, #10551, #20482, #1072, #23528, #17022, #4726, #39909, #660, #7118, #33669, #24171, #40322, #34090, #4093, #20272, #17235, #27395, #37318, #4513, #33460, #10763, #13982, #7541, #30436, #33883, #37098, #1288, #20695, #3887, #30221, #26962, #4305, #7764, #14417, #27611, #17875, #40751, #24391, #37532, #21122, #34311, #449, #13566, #18528, #15487, #38386, #31504, #21560, #24597, #28692, #31291, #2148, #2360, #41172, #21774, #11831, #11403, #11611, #5588, #5377, #34952, #25031, #34740, #12046, #28045, #25450, #41612, #38596, #31717, #37746, #35375, #15283, #8190, #8409, #6385, #24819, #18314, #31933, #18741, #21337, #37964, #28481, #34526, #41819, #5162, #4949, #38174, #41396, #9036, #25242, #8827, #21984, #18096, #1720, #35162, #12257, #31071, #22201, #8618, #1505, #1934, #40960, #14639, #27827, #15061, #14849, #28259, #33563, #13039, #16703, #16487, #29900, #40223, #3987, #6798, #6585, #30331, #17129, #39383, #36999, #26233, #129, #39590, #3144, #7223, #32921, #10025, #13252, #3355, #23205, #16913, #9816, #10657, #338, #36571, #40018, #29470, #29686, #42612, #22996, #27080, #761, #13884, #26439, #36364, #36152, #23850, #3569, #30115, #19953, #33141, #19741, #13459, #26653, #39803, #10235, #23422, #7017, #19527, #16271, #20169, #33359, #3779, #552, #13672, #26864, #10448, #32711, #23640, #36786, #20374, #972, #5057, #7651, #21234, #21448, #17550, #40857, #30967, #30544, #30751, #24712, #24491, #37858, #27936, #8302, #31184, #4411, #1829, #17984, #14957, #11297, #14089, #11728, #37644, #27290, #27506, #24926, #1184, #37428, #34631, #18205, #40427, #7871, #31395, #28155, #41289, #24283, #10870, #14527, #17771, #7434, #8083, #34420, #4839, #24062, #37204, #1614, #14743, #20587, #41065, #27721, #11510, #34209, #17341, #14306, #1397, #21019, #33775, #20802, #4197, #33990, #4625, #40640, #11081, #16018, #9353, #25347, #25134, #6124, #22522, #15174, #12786, #5487, #12154, #41716, #38922, #35695, #19269, #8937, #11943, #5915, #32039, #28587, #35487, #32463, #31831, #38071, #2267, #29214, #21881, #19067, #9146, #2888, #42353, #8511, #38712, #18637, #35059, #2675, #21665, #15809, #34846, #5269, #29005, #22101, #42145, #18421, #31611, #12576, #35275, #2043, #28371, #15388, #25561, #2470, #25769, #41510, #38280, #28800, #8727, #38493, #5708, #15598, #18859, #32248, #22314, #41932, #12363, #26396, #16438, #19482, #23593, #39547, #33090, #19905, #25977, #10192, #9773, #36739, #33523, #22736, #30070, #512, #3737, #13627, #6968, #22953, #20329, #36527, #3946, #29855, #32668, #20124, #3097, #7177, #35902, #17084, #12989, #10402, #293, #19695, #30283, #13203, #722, #39128, #39972, #80, #29425, #3517, #36320, #9562, #13414, #23377, #6339, #9978, #42566, #16867, #39757, #16654, #26186, #26608, #33312, #23157, #16226, #36107, #26820, #6751, #39334, #6541, #32878, #3309, #29636, #1572, #4371, #20760, #24235, #4154, #24018, #24452, #37159, #7395, #10825, #27240, #33949, #17510, #37598, #8042, #21187, #30706, #17297, #17722, #27463, #4582, #20542, #31139, #14260, #37386, #27677, #10611, #14045, #23798, #36953, #17940, #34376, #4792, #20976, #40383, #7606, #14482, #14702, #27891, #40180, #7829, #40598, #1137, #13841, #1352, #40815, #30917, #33731, #30502, #11041, #11255, #27035, #34161, #928, #6473, #20469, #39475, #36875, #26742, #3442, #39683, #7317, #4080, #23724, #26534, #13126, #16791, #20042, #30423, #39896, #13555, #10327, #3234, #26324, #3875, #33447, #27167, #17011, #29991, #13763, #36455, #19615, #19828, #3663, #10117, #33657, #32800, #17218, #16359, #6889, #6677, #33237, #854, #13972, #23297, #9908, #9697, #22876, #29558, #36036, #33013, #436, #13343, #10538, #5, #23084, #23515, #36244, #20260, #36664, #222, #7105, #16579, #29782, #30208, #644, #26951, #40107, #9936, #36065, #25727, #6709, #16608, #42311, #19229, #42100, #13373, #32628, #3264, #2841, #6293, #12733, #36278, #29171, #15975, #25933, #6500, #12945, #13158, #23115, #32207, #6083, #2636, #39082, #16393, #3054, #39505, #9521, #15766, #22691, #22909, #29592, #19861, #28963, #16180, #19436, #26140, #42519, #5868, #32835, #12534, #9726, #38876, #22476, #36, #26352, #23331, #33046, #39292, #3473, #35859, #9307, #19649, #19022, #29377, #35652, #29811, #251, #32419, #26565, #39714, #10149, #14434, #7782, #23752, #23546, #4530, #20926, #13582, #11209, #467, #17038, #13796, #36695, #20072, #24188, #7134, #26978, #30238, #20288, #40138, #33900, #37335, #677, #36483, #10566, #27628, #33476, #4323, #39927, #26774, #10355, #34108, #17672, #36905, #3904, #30020, #1303, #20498, #17461, #30867, #14214, #7350, #33685, #4110, #17251, #30452, #881, #3693, #14000, #40767, #33267, #27195, #16821, #40339, #30660, #10781, #27413, #23970, #37115, #1088, #7559, #20712, #40549, #6920, #10993, #38190, #38402, #34540, #15076, #5177, #4744, #4964, #41627, #41413, #28277, #18331, #28062, #2375, #5394, #18757, #34970, #31947, #11847, #17890, #28707, #25048, #31088, #1739, #41834, #18112, #11629, #25257, #12061, #1521, #31307, #8634, #14655, #15502, #31521, #27844, #1950, #34757, #24407, #21790, #18546, #31735, #2165, #15299, #7988, #21577, #37980, #28496, #8844, #37549, #22002, #8207, #35178, #21140, #34326, #5603, #40976, #41188, #11420, #24614, #37763, #21355, #14865, #24835, #8425, #19596, #22854, #5816, #36221, #9050, #23065, #42051, #39455, #29326, #6030, #19180, #12897, #32156, #19806, #35812, #2793, #9255, #6656, #12684, #15715, #15923, #39243, #12271, #25881, #28914, #3214, #26092, #6244, #12479, #9681, #29124, #22216, #42470, #25468, #9471, #2586, #39035, #3005, #35392, #42681, #38826, #32994, #22639, #42259, #16129, #25672, #32369, #13107, #19388, #18969, #22424, #32579, #36016, #26306, #9890, #3422, #6455, #35602, #32778, #16341, #29539, #16559, #29757, #38613, #17622, #7086, #34058, #26719, #10729, #3644, #39871, #829, #24135, #13951, #10305, #23493, #7505, #14161, #20657, #40495, #27360, #33844, #13738, #36433, #6869, #20020, #413, #3852, #10097, #16771, #202, #33632, #10941, #23274, #20236, #20446, #622, #40287, #30398, #37277, #4269, #4055, #17197, #33213, #29971, #37065, #23921, #13323, #17410, #27144, #30608, #26928, #13533, #36640, #36852, #30185, #7725, #33425, #20872, #16986, #40086, #10516, #23703, #4479, #26512, #7296, #1036, #39661, #2114, #7938, #24563, #40924, #4912, #34490, #31680, #15244, #28443, #1682, #4691, #41358, #24782, #21302, #28225, #41579, #37712, #5551, #8154, #21947, #14601, #11795, #18273, #27791, #31462, #12011, #1896, #11367, #18060, #38139, #25207, #8583, #38349, #8789, #21734, #14811, #24353, #37494, #21088, #31036, #31255, #40712, #5337, #30816, #21523, #35127, #11154, #28007, #8373, #41135, #24998, #15025, #1255, #34915, #11576, #37927, #34276, #14379, #1467, #18492, #27576, #34705, #17840, #5125, #16290, #26251, #15456, #22800, #35964, #39194, #6403, #42419, #15662, #13058, #29276, #39401, #22586, #12219, #23015, #9420, #25411, #38779, #29489, #5768, #3163, #35763, #12427, #9836, #5981, #42628, #36169, #32728, #35552, #22166, #25829, #29071, #18703, #6191, #32317, #38557, #8998, #35340, #19333, #38984, #26042, #19544, #31899, #32525, #2327, #28655, #9205, #2954, #19132, #16081, #12850, #41785, #9628, #2742, #22374, #18921, #32105, #2537, #28863, #12635, #41998, #25622, #15869, #42209, #14107, #3371, #10674, #23868, #27096, #37016, #30348, #3588, #989, #17147, #27309, #10465, #149, #10889, #13269, #30560, #16506, #17358, #36384, #33792, #23655, #358, #40445, #36588, #4215, #24081, #20605, #23440, #10043, #13688, #16934, #6602, #36802, #7240, #19758, #20187, #23224, #40238, #20391, #569, #6817, #33583, #4004, #33377, #29703, #16722, #26880, #7035, #32941, #26458, #39608, #19972, #3797, #29917, #30132, #40035, #777, #33158, #13480, #7456, #39821, #26670, #10253, #13903, #11315, #40874, #38677, #9111, #35451, #8100, #11098, #5671, #31202, #27738, #14327, #15774, #18000, #11526, #15566, #4429, #34226, #41895, #24729, #4642, #37874, #19031, #8319, #17789, #30986, #2431, #22280, #28767, #5877, #32215, #1415, #14546, #21464, #1630, #12329, #25528, #12544, #27954, #2643, #17568, #24507, #14759, #37661, #35240, #18822, #28971, #42110, #21251, #34437, #30769, #4858, #41082, #32006, #37221, #7668, #20821, #21036, #34007, #1200, #27523, #40658, #24301, #37445, #7888, #6718, #22700, #20083, #36288, #33277, #29602, #33056, #19871, #19238, #6929, #22484, #36493, #12743, #10159, #45, #19446, #16831, #12954, #23341, #3702, #39724, #42529, #29180, #32844, #36073, #30030, #29387, #9944, #25735, #39300, #42319, #16618, #39515, #19659, #25942, #26363, #23124, #9738, #35660, #35869, #3273, #26149, #476, #6091, #38886, #32426, #9530, #9316, #22919, #6510, #16402, #39091, #32638, #26574, #16189, #2851, #3064, #6302, #13169, #3482, #15985, #29821, #261, #13382, #30247, #24197, #33693, #11003, #33486, #34334, #37123, #30668, #34118, #23555, #10574, #17681, #1096, #23760, #14223, #37557, #27424, #36913, #7359, #20935, #27636, #4539, #20507, #14008, #4120, #1311, #17259, #686, #39935, #14444, #26990, #30463, #890, #40147, #27203, #37346, #3912, #4752, #7567, #40559, #30877, #36703, #7793, #17046, #20295, #13803, #40776, #24417, #40347, #10790, #7142, #21148, #23980, #11217, #20720, #33911, #4331, #7996, #17470, #17899, #31097, #13592, #26783, #10364, #5824, #27852, #1747, #40986, #8433, #41635, #41421, #35185, #37989, #11428, #24842, #18555, #12071, #5612, #24625, #11858, #15087, #8643, #11638, #34978, #25056, #37772, #21586, #18766, #31745, #5404, #38199, #5186, #22226, #25265, #22012, #15308, #21365, #8216, #28284, #8852, #38411, #34548, #34765, #18979, #18340, #31530, #2384, #31955, #4974, #1958, #2173, #18120, #9058, #21798, #28505, #41198, #38622, #15511, #31315, #28716, #41842, #1530, #14874, #12280, #25476, #14663, #35400, #28071, #22431, #42058, #32164, #9263, #2594, #38834, #28922, #35610, #6037, #15723, #12487, #25681, #8045, #932, #1355, #17300, #17087, #40818, #14485, #7180, #4795, #36742, #10614, #7398, #33734, #39975, #17514, #30073, #27244, #20333, #14048, #20763, #10406, #17725, #27039, #40385, #21191, #27680, #30505, #30286, #11258, #24455, #33526, #515, #3949, #23802, #20546, #725, #13630, #30920, #13844, #4156, #36956, #40183, #10828, #27466, #37602, #24021, #26822, #37162, #34379, #7609, #40601, #33952, #4374, #30710, #23597, #1140, #14263, #11044, #24238, #37389, #7832, #20979, #34166, #4585, #5662, #41245, #14917, #28117, #5449, #25096, #25308, #35231, #35442, #8687, #28759, #27894, #38032, #38242, #18383, #15348, #18600, #2424, #35020, #28546, #8894, #1575, #15131, #31572, #21840, #11900, #17943, #2219, #1788, #15557, #25519, #14704, #22058, #18813, #38453, #31998, #41678, #11686, #31787, #37816, #41027, #2004, #41886, #12115, #11470, #12321, #24671, #38667, #5022, #9103, #22271, #24883, #31142, #5228, #8259, #21405, #34591, #34807, #8475, #18163, #28327, #31357, #21629, #41466, #8614, #32296, #28041, #14191, #27390, #37960, #34522, #18310, #21770, #40527, #41168, #10970, #24166, #8405, #14845, #11607, #40956, #37313, #24386, #8186, #1500, #41392, #7759, #28255, #20903, #11399, #11188, #24593, #34948, #11827, #14634, #1283, #25027, #38170, #34086, #7968, #37527, #31066, #17870, #15057, #5373, #19113, #27822, #30846, #24815, #21333, #4721, #21556, #4508, #21117, #17651, #34306 ),
 .UNSPECIFIED., .F., .F. ) 
 B_SPLINE_CURVE_WITH_KNOTS ( ( 3, 2, 2, 2, 2, 2, 2, 2, 2, 2, 2, 2, 2, 2, 2, 2, 2, 2, 2, 2, 2, 2, 2, 2, 2, 2, 2, 2, 2, 2, 2, 2, 2, 2, 2, 2, 2, 2, 2, 2, 2, 2, 2, 2, 2, 2, 2, 2, 2, 2, 2, 2, 2, 2, 2, 2, 2, 2, 2, 2, 2, 2, 2, 2, 2, 2, 2, 2, 2, 2, 2, 2, 2, 2, 2, 2, 2, 2, 2, 2, 2, 2, 2, 2, 2, 2, 2, 2, 2, 2, 2, 2, 2, 2, 2, 2, 2, 2, 2, 2, 2, 2, 2, 2, 2, 2, 2, 2, 2, 2, 2, 2, 2, 2, 2, 2, 2, 2, 2, 2, 2, 2, 2, 2, 2, 2, 2, 2, 2, 2, 2, 2, 2, 2, 2, 2, 2, 2, 2, 2, 2, 2, 2, 2, 2, 2, 2, 2, 2, 2, 2, 2, 2, 2, 2, 2, 2, 2, 2, 2, 2, 2, 2, 2, 2, 2, 2, 2, 2, 2, 2, 2, 2, 2, 2, 2, 2, 2, 2, 2, 2, 2, 2, 2, 2, 2, 2, 2, 2, 2, 2, 2, 2, 2, 2, 2, 2, 2, 2, 2, 2, 2, 2, 2, 2, 2, 2, 2, 2, 2, 2, 2, 2, 2, 2, 2, 2, 2, 2, 2, 2, 2, 2, 2, 2, 2, 2, 2, 2, 2, 2, 2, 2, 2, 2, 2, 2, 2, 2, 2, 2, 2, 2, 2, 2, 2, 2, 2, 2, 2, 2, 2, 2, 2, 2, 2, 2, 2, 2, 2, 2, 2, 2, 2, 2, 2, 2, 2, 2, 2, 2, 2, 2, 2, 2, 2, 2, 2, 2, 2, 2, 2, 2, 2, 2, 2, 2, 2, 2, 2, 2, 2, 2, 2, 2, 2, 2, 2, 2, 2, 2, 2, 2, 2, 2, 2, 2, 2, 2, 2, 2, 2, 2, 2, 2, 2, 2, 2, 2, 2, 2, 2, 2, 2, 2, 2, 2, 2, 2, 2, 2, 2, 2, 2, 2, 2, 2, 2, 2, 2, 2, 2, 2, 2, 2, 2, 2, 2, 2, 2, 2, 2, 2, 2, 2, 2, 2, 2, 2, 2, 2, 2, 2, 2, 2, 2, 2, 2, 2, 2, 2, 2, 2, 2, 2, 2, 2, 2, 2, 2, 2, 2, 2, 2, 2, 2, 2, 2, 2, 2, 2, 2, 2, 2, 2, 2, 2, 2, 2, 2, 2, 2, 2, 2, 2, 2, 2, 2, 2, 2, 2, 2, 2, 2, 2, 2, 2, 2, 2, 2, 2, 2, 2, 2, 2, 2, 2, 2, 2, 2, 2, 2, 2, 2, 2, 2, 2, 2, 2, 2, 2, 2, 2, 2, 2, 2, 2, 2, 2, 2, 2, 2, 2, 2, 2, 2, 2, 2, 2, 2, 2, 2, 2, 2, 2, 2, 2, 2, 2, 2, 2, 2, 2, 2, 2, 2, 2, 2, 2, 2, 2, 2, 2, 2, 2, 2, 2, 2, 2, 2, 2, 2, 2, 2, 2, 2, 2, 2, 2, 2, 2, 2, 2, 2, 2, 2, 2, 2, 2, 2, 2, 2, 2, 2, 2, 2, 2, 2, 2, 2, 2, 2, 2, 2, 2, 2, 2, 2, 2, 2, 2, 2, 2, 2, 2, 2, 2, 2, 2, 2, 2, 2, 2, 2, 2, 2, 2, 2, 2, 2, 2, 2, 2, 2, 2, 2, 2, 2, 2, 2, 2, 2, 2, 2, 2, 2, 2, 2, 2, 2, 2, 2, 2, 2, 2, 2, 2, 2, 2, 2, 2, 2, 2, 2, 2, 2, 2, 2, 2, 2, 2, 2, 2, 2, 2, 2, 2, 2, 2, 2, 2, 2, 2, 2, 2, 2, 2, 2, 2, 2, 2, 2, 2, 2, 2, 2, 2, 2, 2, 2, 2, 2, 2, 2, 2, 2, 2, 2, 2, 2, 2, 2, 2, 2, 2, 2, 2, 2, 2, 2, 2, 2, 2, 2, 2, 2, 2, 2, 2, 2, 2, 2, 2, 2, 2, 2, 2, 2, 2, 2, 2, 2, 2, 2, 2, 2, 2, 2, 2, 2, 2, 2, 2, 2, 2, 2, 2, 2, 2, 2, 2, 2, 2, 2, 2, 2, 2, 2, 2, 2, 2, 2, 2, 2, 2, 2, 2, 2, 2, 2, 2, 2, 2, 2, 2, 2, 2, 2, 2, 2, 2, 2, 2, 2, 2, 2, 2, 2, 2, 2, 2, 2, 2, 2, 2, 2, 2, 2, 2, 2, 2, 2, 2, 2, 2, 2, 2, 2, 2, 2, 2, 2, 2, 2, 2, 2, 2, 2, 2, 2, 2, 2, 2, 2, 2, 2, 2, 2, 2, 2, 2, 2, 2, 2, 2, 2, 2, 2, 2, 2, 2, 2, 2, 2, 2, 2, 2, 2, 2, 2, 2, 2, 2, 2, 2, 2, 2, 2, 2, 2, 2, 2, 2, 2, 2, 2, 2, 2, 2, 3 ),
 ( 0.000000000000000000, 0.001243781094527363160, 0.002487562189054726321, 0.003731343283582089481, 0.004975124378109452641, 0.006218905472636816235, 0.007462686567164178962, 0.008706467661691542556, 0.009950248756218905283, 0.01119402985074626801, 0.01243781094527363247, 0.01368159203980099520, 0.01492537313432835792, 0.01616915422885572065, 0.01741293532338308511, 0.01865671641791044610, 0.01990049751243781057, 0.02114427860696517503, 0.02238805970149253602, 0.02363184079601990048, 0.02487562189054726494, 0.02611940298507462593, 0.02736318407960199039, 0.02860696517412935486, 0.02985074626865671585, 0.03109452736318408031, 0.03233830845771144130, 0.03358208955223880576, 0.03482587064676617022, 0.03606965174129353469, 0.03731343283582089221, 0.03855721393034825667, 0.03980099502487562113, 0.04104477611940298559, 0.04228855721393035005, 0.04353233830845771452, 0.04477611940298507204, 0.04601990049751243650, 0.04726368159203980096, 0.04850746268656716542, 0.04975124378109452988, 0.05099502487562188741, 0.05223880597014925187, 0.05348258706467661633, 0.05472636815920398079, 0.05597014925373134525, 0.05721393034825870971, 0.05845771144278606724, 0.05970149253731343170, 0.06094527363184079616, 0.06218905472636816062, 0.06343283582089552508, 0.06467661691542288260, 0.06592039800995025400, 0.06716417910447761153, 0.06840796019900496905, 0.06965174129353234045, 0.07089552238805969797, 0.07213930348258706937, 0.07338308457711442689, 0.07462686567164178442, 0.07587064676616915582, 0.07711442786069651334, 0.07835820895522388474, 0.07960199004975124226, 0.08084577114427861366, 0.08208955223880597118, 0.08333333333333332871, 0.08457711442786070011, 0.08582089552238805763, 0.08706467661691542903, 0.08830845771144278655, 0.08955223880597014408, 0.09079601990049751548, 0.09203980099502487300, 0.09328358208955224440, 0.09452736318407960192, 0.09577114427860695944, 0.09701492537313433084, 0.09825870646766168837, 0.09950248756218905977, 0.1007462686567164173, 0.1019900497512437748, 0.1032338308457711462, 0.1044776119402985037, 0.1057213930348258751, 0.1069651741293532327, 0.1082089552238805902, 0.1094527363184079616, 0.1106965174129353191, 0.1119402985074626905, 0.1131840796019900480, 0.1144278606965174194, 0.1156716417910447769, 0.1169154228855721345, 0.1181592039800995059, 0.1194029850746268634, 0.1206467661691542348, 0.1218905472636815923, 0.1231343283582089498, 0.1243781094527363212, 0.1256218905472636926, 0.1268656716417910502, 0.1281094527363184077, 0.1293532338308457652, 0.1305970149253731227, 0.1318407960199005080, 0.1330845771144278655, 0.1343283582089552231, 0.1355721393034825806, 0.1368159203980099381, 0.1380597014925373234, 0.1393034825870646809, 0.1405472636815920384, 0.1417910447761193959, 0.1430348258706467535, 0.1442786069651741387, 0.1455223880597014963, 0.1467661691542288538, 0.1480099502487562113, 0.1492537313432835688, 0.1504975124378109541, 0.1517412935323383116, 0.1529850746268656692, 0.1542288557213930267, 0.1554726368159203842, 0.1567164179104477695, 0.1579601990049751270, 0.1592039800995024845, 0.1604477611940298420, 0.1616915422885572273, 0.1629353233830845848, 0.1641791044776119424, 0.1654228855721392999, 0.1666666666666666574, 0.1679104477611940427, 0.1691542288557214002, 0.1703980099502487577, 0.1716417910447761153, 0.1728855721393034728, 0.1741293532338308581, 0.1753731343283582156, 0.1766169154228855731, 0.1778606965174129306, 0.1791044776119402882, 0.1803482587064676734, 0.1815920398009950310, 0.1828358208955223885, 0.1840796019900497460, 0.1853233830845771035, 0.1865671641791044888, 0.1878109452736318463, 0.1890547263681592038, 0.1902985074626865614, 0.1915422885572139189, 0.1927860696517413042, 0.1940298507462686617, 0.1952736318407960192, 0.1965174129353233767, 0.1977611940298507343, 0.1990049751243781195, 0.2002487562189054771, 0.2014925373134328346, 0.2027363184079601921, 0.2039800995024875496, 0.2052238805970149349, 0.2064676616915422924, 0.2077114427860696499, 0.2089552238805970075, 0.2101990049751243650, 0.2114427860696517503, 0.2126865671641791078, 0.2139303482587064653, 0.2151741293532338228, 0.2164179104477611804, 0.2176616915422885656, 0.2189054726368159232, 0.2201492537313432807, 0.2213930348258706382, 0.2226368159203980235, 0.2238805970149253810, 0.2251243781094527385, 0.2263681592039800961, 0.2276119402985074536, 0.2288557213930348389, 0.2300995024875621964, 0.2313432835820895539, 0.2325870646766169114, 0.2338308457711442689, 0.2350746268656716542, 0.2363184079601990117, 0.2375621890547263693, 0.2388059701492537268, 0.2400497512437810843, 0.2412935323383084696, 0.2425373134328358271, 0.2437810945273631846, 0.2450248756218905422, 0.2462686567164178997, 0.2475124378109452850, 0.2487562189054726425, 0.2500000000000000000, 0.2512437810945273853, 0.2524875621890547150, 0.2537313432835821003, 0.2549751243781094301, 0.2562189054726368154, 0.2574626865671642006, 0.2587064676616915304, 0.2599502487562189157, 0.2611940298507462455, 0.2624378109452736307, 0.2636815920398010160, 0.2649253731343283458, 0.2661691542288557311, 0.2674129353233830608, 0.2686567164179104461, 0.2699004975124378314, 0.2711442786069651611, 0.2723880597014925464, 0.2736318407960198762, 0.2748756218905472615, 0.2761194029850746468, 0.2773631840796019765, 0.2786069651741293618, 0.2798507462686566916, 0.2810945273631840768, 0.2823383084577114621, 0.2835820895522387919, 0.2848258706467661772, 0.2860696517412935069, 0.2873134328358208922, 0.2885572139303482775, 0.2898009950248756073, 0.2910447761194029925, 0.2922885572139303223, 0.2935323383084577076, 0.2947761194029850929, 0.2960199004975124226, 0.2972636815920398079, 0.2985074626865671377, 0.2997512437810945229, 0.3009950248756219082, 0.3022388059701492380, 0.3034825870646766233, 0.3047263681592039530, 0.3059701492537313383, 0.3072139303482587236, 0.3084577114427860534, 0.3097014925373134386, 0.3109452736318407684, 0.3121890547263681537, 0.3134328358208955390, 0.3146766169154228687, 0.3159203980099502540, 0.3171641791044776393, 0.3184079601990049690, 0.3196517412935323543, 0.3208955223880596841, 0.3221393034825870694, 0.3233830845771144546, 0.3246268656716417844, 0.3258706467661691697, 0.3271144278606964995, 0.3283582089552238847, 0.3296019900497512700, 0.3308457711442785998, 0.3320895522388059851, 0.3333333333333333148, 0.3345771144278607001, 0.3358208955223880854, 0.3370646766169154152, 0.3383084577114428004, 0.3395522388059701302, 0.3407960199004975155, 0.3420398009950249008, 0.3432835820895522305, 0.3445273631840796158, 0.3457711442786069456, 0.3470149253731343308, 0.3482587064676617161, 0.3495024875621890459, 0.3507462686567164312, 0.3519900497512437609, 0.3532338308457711462, 0.3544776119402985315, 0.3557213930348258613, 0.3569651741293532465, 0.3582089552238805763, 0.3594527363184079616, 0.3606965174129353469, 0.3619402985074626766, 0.3631840796019900619, 0.3644278606965173917, 0.3656716417910447769, 0.3669154228855721622, 0.3681592039800994920, 0.3694029850746268773, 0.3706467661691542070, 0.3718905472636815923, 0.3731343283582089776, 0.3743781094527363074, 0.3756218905472636926, 0.3768656716417910224, 0.3781094527363184077, 0.3793532338308457930, 0.3805970149253731227, 0.3818407960199005080, 0.3830845771144278378, 0.3843283582089552231, 0.3855721393034826083, 0.3868159203980099381, 0.3880597014925373234, 0.3893034825870646531, 0.3905472636815920384, 0.3917910447761194237, 0.3930348258706467535, 0.3942786069651741387, 0.3955223880597014685, 0.3967661691542288538, 0.3980099502487562391, 0.3992537313432835688, 0.4004975124378109541, 0.4017412935323382839, 0.4029850746268656692, 0.4042288557213930544, 0.4054726368159203842, 0.4067164179104477695, 0.4079601990049750992, 0.4092039800995024845, 0.4104477611940298698, 0.4116915422885571996, 0.4129353233830845848, 0.4141791044776119146, 0.4154228855721392999, 0.4166666666666666297, 0.4179104477611940149, 0.4191542288557214002, 0.4203980099502487300, 0.4216417910447761153, 0.4228855721393035005, 0.4241293532338308303, 0.4253731343283582156, 0.4266169154228855454, 0.4278606965174129306, 0.4291044776119403159, 0.4303482587064676457, 0.4315920398009950310, 0.4328358208955223607, 0.4340796019900497460, 0.4353233830845771313, 0.4365671641791044610, 0.4378109452736318463, 0.4390547263681592316, 0.4402985074626865614, 0.4415422885572139466, 0.4427860696517412764, 0.4440298507462686617, 0.4452736318407960470, 0.4465174129353233767, 0.4477611940298507620, 0.4490049751243780918, 0.4502487562189054771, 0.4514925373134328623, 0.4527363184079601921, 0.4539800995024875774, 0.4552238805970149071, 0.4564676616915422924, 0.4577114427860696777, 0.4589552238805970075, 0.4601990049751243927, 0.4614427860696517225, 0.4626865671641791078, 0.4639303482587064931, 0.4651741293532338228, 0.4664179104477612081, 0.4676616915422885379, 0.4689054726368159232, 0.4701492537313433084, 0.4713930348258706382, 0.4726368159203980235, 0.4738805970149253532, 0.4751243781094527385, 0.4763681592039801238, 0.4776119402985074536, 0.4788557213930348389, 0.4800995024875621686, 0.4813432835820895539, 0.4825870646766169392, 0.4838308457711442689, 0.4850746268656716542, 0.4863184079601989840, 0.4875621890547263693, 0.4888059701492537545, 0.4900497512437810843, 0.4912935323383084696, 0.4925373134328357994, 0.4937810945273631846, 0.4950248756218905699, 0.4962686567164178997, 0.4975124378109452850, 0.4987562189054726147, 0.5000000000000000000, 0.5012437810945273853, 0.5024875621890547706, 0.5037313432835820448, 0.5049751243781094301, 0.5062189054726368154, 0.5074626865671642006, 0.5087064676616915859, 0.5099502487562188602, 0.5111940298507462455, 0.5124378109452736307, 0.5136815920398010160, 0.5149253731343284013, 0.5161691542288556755, 0.5174129353233830608, 0.5186567164179104461, 0.5199004975124378314, 0.5211442786069652167, 0.5223880597014924909, 0.5236318407960198762, 0.5248756218905472615, 0.5261194029850746468, 0.5273631840796020320, 0.5286069651741293063, 0.5298507462686566916, 0.5310945273631840768, 0.5323383084577114621, 0.5335820895522388474, 0.5348258706467661217, 0.5360696517412935069, 0.5373134328358208922, 0.5385572139303482775, 0.5398009950248756628, 0.5410447761194029370, 0.5422885572139303223, 0.5435323383084577076, 0.5447761194029850929, 0.5460199004975124781, 0.5472636815920397524, 0.5485074626865671377, 0.5497512437810945229, 0.5509950248756219082, 0.5522388059701492935, 0.5534825870646765678, 0.5547263681592039530, 0.5559701492537313383, 0.5572139303482587236, 0.5584577114427861089, 0.5597014925373133831, 0.5609452736318407684, 0.5621890547263681537, 0.5634328358208955390, 0.5646766169154229242, 0.5659203980099501985, 0.5671641791044775838, 0.5684079601990049690, 0.5696517412935323543, 0.5708955223880597396, 0.5721393034825870139, 0.5733830845771143991, 0.5746268656716417844, 0.5758706467661691697, 0.5771144278606965550, 0.5783582089552238292, 0.5796019900497512145, 0.5808457711442785998, 0.5820895522388059851, 0.5833333333333333703, 0.5845771144278606446, 0.5858208955223880299, 0.5870646766169154152, 0.5883084577114428004, 0.5895522388059701857, 0.5907960199004974600, 0.5920398009950248452, 0.5932835820895522305, 0.5945273631840796158, 0.5957711442786070011, 0.5970149253731342753, 0.5982587064676616606, 0.5995024875621890459, 0.6007462686567164312, 0.6019900497512438164, 0.6032338308457710907, 0.6044776119402984760, 0.6057213930348258613, 0.6069651741293532465, 0.6082089552238806318, 0.6094527363184079061, 0.6106965174129352913, 0.6119402985074626766, 0.6131840796019900619, 0.6144278606965174472, 0.6156716417910447214, 0.6169154228855721067, 0.6181592039800994920, 0.6194029850746268773, 0.6206467661691542625, 0.6218905472636815368, 0.6231343283582089221, 0.6243781094527363074, 0.6256218905472636926, 0.6268656716417910779, 0.6281094527363184632, 0.6293532338308457375, 0.6305970149253731227, 0.6318407960199005080, 0.6330845771144278933, 0.6343283582089552786, 0.6355721393034825528, 0.6368159203980099381, 0.6380597014925373234, 0.6393034825870647087, 0.6405472636815920939, 0.6417910447761193682, 0.6430348258706467535, 0.6442786069651741387, 0.6455223880597015240, 0.6467661691542289093, 0.6480099502487560725, 0.6492537313432835688, 0.6504975124378109541, 0.6517412935323383394, 0.6529850746268657247, 0.6542288557213929989, 0.6554726368159203842, 0.6567164179104477695, 0.6579601990049751548, 0.6592039800995025400, 0.6604477611940298143, 0.6616915422885571996, 0.6629353233830845848, 0.6641791044776119701, 0.6654228855721393554, 0.6666666666666666297, 0.6679104477611940149, 0.6691542288557214002, 0.6703980099502487855, 0.6716417910447761708, 0.6728855721393034450, 0.6741293532338308303, 0.6753731343283582156, 0.6766169154228856009, 0.6778606965174129861, 0.6791044776119402604, 0.6803482587064676457, 0.6815920398009950310, 0.6828358208955224162, 0.6840796019900498015, 0.6853233830845770758, 0.6865671641791044610, 0.6878109452736318463, 0.6890547263681592316, 0.6902985074626866169, 0.6915422885572138911, 0.6927860696517412764, 0.6940298507462686617, 0.6952736318407960470, 0.6965174129353234322, 0.6977611940298507065, 0.6990049751243780918, 0.7002487562189054771, 0.7014925373134328623, 0.7027363184079602476, 0.7039800995024875219, 0.7052238805970149071, 0.7064676616915422924, 0.7077114427860696777, 0.7089552238805970630, 0.7101990049751243372, 0.7114427860696517225, 0.7126865671641791078, 0.7139303482587064931, 0.7151741293532338783, 0.7164179104477611526, 0.7176616915422885379, 0.7189054726368159232, 0.7201492537313433084, 0.7213930348258706937, 0.7226368159203979680, 0.7238805970149253532, 0.7251243781094527385, 0.7263681592039801238, 0.7276119402985075091, 0.7288557213930347833, 0.7300995024875621686, 0.7313432835820895539, 0.7325870646766169392, 0.7338308457711443245, 0.7350746268656715987, 0.7363184079601989840, 0.7375621890547263693, 0.7388059701492537545, 0.7400497512437811398, 0.7412935323383084141, 0.7425373134328357994, 0.7437810945273631846, 0.7450248756218905699, 0.7462686567164179552, 0.7475124378109452294, 0.7487562189054726147, 0.7500000000000000000, 0.7512437810945273853, 0.7524875621890547706, 0.7537313432835820448, 0.7549751243781094301, 0.7562189054726368154, 0.7574626865671642006, 0.7587064676616915859, 0.7599502487562188602, 0.7611940298507462455, 0.7624378109452736307, 0.7636815920398010160, 0.7649253731343284013, 0.7661691542288556755, 0.7674129353233830608, 0.7686567164179104461, 0.7699004975124378314, 0.7711442786069652167, 0.7723880597014924909, 0.7736318407960198762, 0.7748756218905472615, 0.7761194029850746468, 0.7773631840796020320, 0.7786069651741293063, 0.7798507462686566916, 0.7810945273631840768, 0.7823383084577114621, 0.7835820895522388474, 0.7848258706467661217, 0.7860696517412935069, 0.7873134328358208922, 0.7885572139303482775, 0.7898009950248756628, 0.7910447761194029370, 0.7922885572139303223, 0.7935323383084577076, 0.7947761194029850929, 0.7960199004975124781, 0.7972636815920397524, 0.7985074626865671377, 0.7997512437810945229, 0.8009950248756219082, 0.8022388059701492935, 0.8034825870646765678, 0.8047263681592039530, 0.8059701492537313383, 0.8072139303482587236, 0.8084577114427861089, 0.8097014925373133831, 0.8109452736318407684, 0.8121890547263681537, 0.8134328358208955390, 0.8146766169154229242, 0.8159203980099501985, 0.8171641791044775838, 0.8184079601990049690, 0.8196517412935323543, 0.8208955223880597396, 0.8221393034825870139, 0.8233830845771143991, 0.8246268656716417844, 0.8258706467661691697, 0.8271144278606965550, 0.8283582089552238292, 0.8296019900497512145, 0.8308457711442785998, 0.8320895522388059851, 0.8333333333333332593, 0.8345771144278606446, 0.8358208955223880299, 0.8370646766169154152, 0.8383084577114428004, 0.8395522388059701857, 0.8407960199004974600, 0.8420398009950248452, 0.8432835820895522305, 0.8445273631840796158, 0.8457711442786070011, 0.8470149253731342753, 0.8482587064676616606, 0.8495024875621890459, 0.8507462686567164312, 0.8519900497512438164, 0.8532338308457710907, 0.8544776119402984760, 0.8557213930348258613, 0.8569651741293532465, 0.8582089552238806318, 0.8594527363184079061, 0.8606965174129352913, 0.8619402985074626766, 0.8631840796019900619, 0.8644278606965174472, 0.8656716417910447214, 0.8669154228855721067, 0.8681592039800994920, 0.8694029850746268773, 0.8706467661691542625, 0.8718905472636815368, 0.8731343283582089221, 0.8743781094527363074, 0.8756218905472636926, 0.8768656716417910779, 0.8781094527363184632, 0.8793532338308457375, 0.8805970149253731227, 0.8818407960199005080, 0.8830845771144278933, 0.8843283582089552786, 0.8855721393034825528, 0.8868159203980099381, 0.8880597014925373234, 0.8893034825870647087, 0.8905472636815920939, 0.8917910447761193682, 0.8930348258706467535, 0.8942786069651741387, 0.8955223880597015240, 0.8967661691542289093, 0.8980099502487561836, 0.8992537313432835688, 0.9004975124378109541, 0.9017412935323383394, 0.9029850746268657247, 0.9042288557213929989, 0.9054726368159203842, 0.9067164179104477695, 0.9079601990049751548, 0.9092039800995025400, 0.9104477611940298143, 0.9116915422885571996, 0.9129353233830845848, 0.9141791044776119701, 0.9154228855721393554, 0.9166666666666666297, 0.9179104477611940149, 0.9191542288557214002, 0.9203980099502487855, 0.9216417910447761708, 0.9228855721393034450, 0.9241293532338308303, 0.9253731343283582156, 0.9266169154228856009, 0.9278606965174129861, 0.9291044776119402604, 0.9303482587064676457, 0.9315920398009950310, 0.9328358208955224162, 0.9340796019900498015, 0.9353233830845770758, 0.9365671641791044610, 0.9378109452736318463, 0.9390547263681592316, 0.9402985074626866169, 0.9415422885572138911, 0.9427860696517412764, 0.9440298507462686617, 0.9452736318407960470, 0.9465174129353234322, 0.9477611940298507065, 0.9490049751243780918, 0.9502487562189054771, 0.9514925373134328623, 0.9527363184079602476, 0.9539800995024875219, 0.9552238805970149071, 0.9564676616915422924, 0.9577114427860696777, 0.9589552238805970630, 0.9601990049751243372, 0.9614427860696517225, 0.9626865671641791078, 0.9639303482587064931, 0.9651741293532338783, 0.9664179104477611526, 0.9676616915422885379, 0.9689054726368159232, 0.9701492537313433084, 0.9713930348258706937, 0.9726368159203979680, 0.9738805970149253532, 0.9751243781094527385, 0.9763681592039801238, 0.9776119402985075091, 0.9788557213930347833, 0.9800995024875621686, 0.9813432835820895539, 0.9825870646766169392, 0.9838308457711443245, 0.9850746268656715987, 0.9863184079601989840, 0.9875621890547263693, 0.9888059701492537545, 0.9900497512437811398, 0.9912935323383084141, 0.9925373134328357994, 0.9927075504029140296 ),
 .UNSPECIFIED. ) 
 CURVE ( )  GEOMETRIC_REPRESENTATION_ITEM ( )  RATIONAL_B_SPLINE_CURVE ( ( 1.000000000000000000, 0.8660254037844387076, 1.000000000000000000, 0.8660254037844387076, 1.000000000000000000, 0.8660254037844387076, 1.000000000000000000, 0.8660254037844387076, 1.000000000000000000, 0.8660254037844387076, 1.000000000000000000, 0.8660254037844387076, 1.000000000000000000, 0.8660254037844387076, 1.000000000000000000, 0.8660254037844387076, 1.000000000000000000, 0.8660254037844387076, 1.000000000000000000, 0.8660254037844387076, 1.000000000000000000, 0.8660254037844387076, 1.000000000000000000, 0.8660254037844387076, 1.000000000000000000, 0.8660254037844387076, 1.000000000000000000, 0.8660254037844387076, 1.000000000000000000, 0.8660254037844387076, 1.000000000000000000, 0.8660254037844387076, 1.000000000000000000, 0.8660254037844387076, 1.000000000000000000, 0.8660254037844387076, 1.000000000000000000, 0.8660254037844387076, 1.000000000000000000, 0.8660254037844387076, 1.000000000000000000, 0.8660254037844387076, 1.000000000000000000, 0.8660254037844387076, 1.000000000000000000, 0.8660254037844387076, 1.000000000000000000, 0.8660254037844387076, 1.000000000000000000, 0.8660254037844387076, 1.000000000000000000, 0.8660254037844387076, 1.000000000000000000, 0.8660254037844387076, 1.000000000000000000, 0.8660254037844387076, 1.000000000000000000, 0.8660254037844387076, 1.000000000000000000, 0.8660254037844387076, 1.000000000000000000, 0.8660254037844387076, 1.000000000000000000, 0.8660254037844387076, 1.000000000000000000, 0.8660254037844387076, 1.000000000000000000, 0.8660254037844387076, 1.000000000000000000, 0.8660254037844387076, 1.000000000000000000, 0.8660254037844387076, 1.000000000000000000, 0.8660254037844387076, 1.000000000000000000, 0.8660254037844387076, 1.000000000000000000, 0.8660254037844387076, 1.000000000000000000, 0.8660254037844387076, 1.000000000000000000, 0.8660254037844387076, 1.000000000000000000, 0.8660254037844387076, 1.000000000000000000, 0.8660254037844387076, 1.000000000000000000, 0.8660254037844387076, 1.000000000000000000, 0.8660254037844387076, 1.000000000000000000, 0.8660254037844387076, 1.000000000000000000, 0.8660254037844387076, 1.000000000000000000, 0.8660254037844387076, 1.000000000000000000, 0.8660254037844387076, 1.000000000000000000, 0.8660254037844387076, 1.000000000000000000, 0.8660254037844387076, 1.000000000000000000, 0.8660254037844387076, 1.000000000000000000, 0.8660254037844387076, 1.000000000000000000, 0.8660254037844387076, 1.000000000000000000, 0.8660254037844387076, 1.000000000000000000, 0.8660254037844387076, 1.000000000000000000, 0.8660254037844387076, 1.000000000000000000, 0.8660254037844387076, 1.000000000000000000, 0.8660254037844387076, 1.000000000000000000, 0.8660254037844387076, 1.000000000000000000, 0.8660254037844387076, 1.000000000000000000, 0.8660254037844387076, 1.000000000000000000, 0.8660254037844387076, 1.000000000000000000, 0.8660254037844387076, 1.000000000000000000, 0.8660254037844387076, 1.000000000000000000, 0.8660254037844387076, 1.000000000000000000, 0.8660254037844387076, 1.000000000000000000, 0.8660254037844387076, 1.000000000000000000, 0.8660254037844387076, 1.000000000000000000, 0.8660254037844387076, 1.000000000000000000, 0.8660254037844387076, 1.000000000000000000, 0.8660254037844387076, 1.000000000000000000, 0.8660254037844387076, 1.000000000000000000, 0.8660254037844387076, 1.000000000000000000, 0.8660254037844387076, 1.000000000000000000, 0.8660254037844387076, 1.000000000000000000, 0.8660254037844387076, 1.000000000000000000, 0.8660254037844387076, 1.000000000000000000, 0.8660254037844387076, 1.000000000000000000, 0.8660254037844387076, 1.000000000000000000, 0.8660254037844387076, 1.000000000000000000, 0.8660254037844387076, 1.000000000000000000, 0.8660254037844387076, 1.000000000000000000, 0.8660254037844387076, 1.000000000000000000, 0.8660254037844387076, 1.000000000000000000, 0.8660254037844387076, 1.000000000000000000, 0.8660254037844387076, 1.000000000000000000, 0.8660254037844387076, 1.000000000000000000, 0.8660254037844387076, 1.000000000000000000, 0.8660254037844387076, 1.000000000000000000, 0.8660254037844387076, 1.000000000000000000, 0.8660254037844387076, 1.000000000000000000, 0.8660254037844387076, 1.000000000000000000, 0.8660254037844387076, 1.000000000000000000, 0.8660254037844387076, 1.000000000000000000, 0.8660254037844387076, 1.000000000000000000, 0.8660254037844387076, 1.000000000000000000, 0.8660254037844387076, 1.000000000000000000, 0.8660254037844387076, 1.000000000000000000, 0.8660254037844387076, 1.000000000000000000, 0.8660254037844387076, 1.000000000000000000, 0.8660254037844387076, 1.000000000000000000, 0.8660254037844387076, 1.000000000000000000, 0.8660254037844387076, 1.000000000000000000, 0.8660254037844387076, 1.000000000000000000, 0.8660254037844387076, 1.000000000000000000, 0.8660254037844387076, 1.000000000000000000, 0.8660254037844387076, 1.000000000000000000, 0.8660254037844387076, 1.000000000000000000, 0.8660254037844387076, 1.000000000000000000, 0.8660254037844387076, 1.000000000000000000, 0.8660254037844387076, 1.000000000000000000, 0.8660254037844387076, 1.000000000000000000, 0.8660254037844387076, 1.000000000000000000, 0.8660254037844387076, 1.000000000000000000, 0.8660254037844387076, 1.000000000000000000, 0.8660254037844387076, 1.000000000000000000, 0.8660254037844387076, 1.000000000000000000, 0.8660254037844387076, 1.000000000000000000, 0.8660254037844387076, 1.000000000000000000, 0.8660254037844387076, 1.000000000000000000, 0.8660254037844387076, 1.000000000000000000, 0.8660254037844387076, 1.000000000000000000, 0.8660254037844387076, 1.000000000000000000, 0.8660254037844387076, 1.000000000000000000, 0.8660254037844387076, 1.000000000000000000, 0.8660254037844387076, 1.000000000000000000, 0.8660254037844387076, 1.000000000000000000, 0.8660254037844387076, 1.000000000000000000, 0.8660254037844387076, 1.000000000000000000, 0.8660254037844387076, 1.000000000000000000, 0.8660254037844387076, 1.000000000000000000, 0.8660254037844387076, 1.000000000000000000, 0.8660254037844387076, 1.000000000000000000, 0.8660254037844387076, 1.000000000000000000, 0.8660254037844387076, 1.000000000000000000, 0.8660254037844387076, 1.000000000000000000, 0.8660254037844387076, 1.000000000000000000, 0.8660254037844387076, 1.000000000000000000, 0.8660254037844387076, 1.000000000000000000, 0.8660254037844387076, 1.000000000000000000, 0.8660254037844387076, 1.000000000000000000, 0.8660254037844387076, 1.000000000000000000, 0.8660254037844387076, 1.000000000000000000, 0.8660254037844387076, 1.000000000000000000, 0.8660254037844387076, 1.000000000000000000, 0.8660254037844387076, 1.000000000000000000, 0.8660254037844387076, 1.000000000000000000, 0.8660254037844387076, 1.000000000000000000, 0.8660254037844387076, 1.000000000000000000, 0.8660254037844387076, 1.000000000000000000, 0.8660254037844387076, 1.000000000000000000, 0.8660254037844387076, 1.000000000000000000, 0.8660254037844387076, 1.000000000000000000, 0.8660254037844387076, 1.000000000000000000, 0.8660254037844387076, 1.000000000000000000, 0.8660254037844387076, 1.000000000000000000, 0.8660254037844387076, 1.000000000000000000, 0.8660254037844387076, 1.000000000000000000, 0.8660254037844387076, 1.000000000000000000, 0.8660254037844387076, 1.000000000000000000, 0.8660254037844387076, 1.000000000000000000, 0.8660254037844387076, 1.000000000000000000, 0.8660254037844387076, 1.000000000000000000, 0.8660254037844387076, 1.000000000000000000, 0.8660254037844387076, 1.000000000000000000, 0.8660254037844387076, 1.000000000000000000, 0.8660254037844387076, 1.000000000000000000, 0.8660254037844387076, 1.000000000000000000, 0.8660254037844387076, 1.000000000000000000, 0.8660254037844387076, 1.000000000000000000, 0.8660254037844387076, 1.000000000000000000, 0.8660254037844387076, 1.000000000000000000, 0.8660254037844387076, 1.000000000000000000, 0.8660254037844387076, 1.000000000000000000, 0.8660254037844387076, 1.000000000000000000, 0.8660254037844387076, 1.000000000000000000, 0.8660254037844387076, 1.000000000000000000, 0.8660254037844387076, 1.000000000000000000, 0.8660254037844387076, 1.000000000000000000, 0.8660254037844387076, 1.000000000000000000, 0.8660254037844387076, 1.000000000000000000, 0.8660254037844387076, 1.000000000000000000, 0.8660254037844387076, 1.000000000000000000, 0.8660254037844387076, 1.000000000000000000, 0.8660254037844387076, 1.000000000000000000, 0.8660254037844387076, 1.000000000000000000, 0.8660254037844387076, 1.000000000000000000, 0.8660254037844387076, 1.000000000000000000, 0.8660254037844387076, 1.000000000000000000, 0.8660254037844387076, 1.000000000000000000, 0.8660254037844387076, 1.000000000000000000, 0.8660254037844387076, 1.000000000000000000, 0.8660254037844387076, 1.000000000000000000, 0.8660254037844387076, 1.000000000000000000, 0.8660254037844387076, 1.000000000000000000, 0.8660254037844387076, 1.000000000000000000, 0.8660254037844387076, 1.000000000000000000, 0.8660254037844387076, 1.000000000000000000, 0.8660254037844387076, 1.000000000000000000, 0.8660254037844387076, 1.000000000000000000, 0.8660254037844387076, 1.000000000000000000, 0.8660254037844387076, 1.000000000000000000, 0.8660254037844387076, 1.000000000000000000, 0.8660254037844387076, 1.000000000000000000, 0.8660254037844387076, 1.000000000000000000, 0.8660254037844387076, 1.000000000000000000, 0.8660254037844387076, 1.000000000000000000, 0.8660254037844387076, 1.000000000000000000, 0.8660254037844387076, 1.000000000000000000, 0.8660254037844387076, 1.000000000000000000, 0.8660254037844387076, 1.000000000000000000, 0.8660254037844387076, 1.000000000000000000, 0.8660254037844387076, 1.000000000000000000, 0.8660254037844387076, 1.000000000000000000, 0.8660254037844387076, 1.000000000000000000, 0.8660254037844387076, 1.000000000000000000, 0.8660254037844387076, 1.000000000000000000, 0.8660254037844387076, 1.000000000000000000, 0.8660254037844387076, 1.000000000000000000, 0.8660254037844387076, 1.000000000000000000, 0.8660254037844387076, 1.000000000000000000, 0.8660254037844387076, 1.000000000000000000, 0.8660254037844387076, 1.000000000000000000, 0.8660254037844387076, 1.000000000000000000, 0.8660254037844387076, 1.000000000000000000, 0.8660254037844387076, 1.000000000000000000, 0.8660254037844387076, 1.000000000000000000, 0.8660254037844387076, 1.000000000000000000, 0.8660254037844387076, 1.000000000000000000, 0.8660254037844387076, 1.000000000000000000, 0.8660254037844387076, 1.000000000000000000, 0.8660254037844387076, 1.000000000000000000, 0.8660254037844387076, 1.000000000000000000, 0.8660254037844387076, 1.000000000000000000, 0.8660254037844387076, 1.000000000000000000, 0.8660254037844387076, 1.000000000000000000, 0.8660254037844387076, 1.000000000000000000, 0.8660254037844387076, 1.000000000000000000, 0.8660254037844387076, 1.000000000000000000, 0.8660254037844387076, 1.000000000000000000, 0.8660254037844387076, 1.000000000000000000, 0.8660254037844387076, 1.000000000000000000, 0.8660254037844387076, 1.000000000000000000, 0.8660254037844387076, 1.000000000000000000, 0.8660254037844387076, 1.000000000000000000, 0.8660254037844387076, 1.000000000000000000, 0.8660254037844387076, 1.000000000000000000, 0.8660254037844387076, 1.000000000000000000, 0.8660254037844387076, 1.000000000000000000, 0.8660254037844387076, 1.000000000000000000, 0.8660254037844387076, 1.000000000000000000, 0.8660254037844387076, 1.000000000000000000, 0.8660254037844387076, 1.000000000000000000, 0.8660254037844387076, 1.000000000000000000, 0.8660254037844387076, 1.000000000000000000, 0.8660254037844387076, 1.000000000000000000, 0.8660254037844387076, 1.000000000000000000, 0.8660254037844387076, 1.000000000000000000, 0.8660254037844387076, 1.000000000000000000, 0.8660254037844387076, 1.000000000000000000, 0.8660254037844387076, 1.000000000000000000, 0.8660254037844387076, 1.000000000000000000, 0.8660254037844387076, 1.000000000000000000, 0.8660254037844387076, 1.000000000000000000, 0.8660254037844387076, 1.000000000000000000, 0.8660254037844387076, 1.000000000000000000, 0.8660254037844387076, 1.000000000000000000, 0.8660254037844387076, 1.000000000000000000, 0.8660254037844387076, 1.000000000000000000, 0.8660254037844387076, 1.000000000000000000, 0.8660254037844387076, 1.000000000000000000, 0.8660254037844387076, 1.000000000000000000, 0.8660254037844387076, 1.000000000000000000, 0.8660254037844387076, 1.000000000000000000, 0.8660254037844387076, 1.000000000000000000, 0.8660254037844387076, 1.000000000000000000, 0.8660254037844387076, 1.000000000000000000, 0.8660254037844387076, 1.000000000000000000, 0.8660254037844387076, 1.000000000000000000, 0.8660254037844387076, 1.000000000000000000, 0.8660254037844387076, 1.000000000000000000, 0.8660254037844387076, 1.000000000000000000, 0.8660254037844387076, 1.000000000000000000, 0.8660254037844387076, 1.000000000000000000, 0.8660254037844387076, 1.000000000000000000, 0.8660254037844387076, 1.000000000000000000, 0.8660254037844387076, 1.000000000000000000, 0.8660254037844387076, 1.000000000000000000, 0.8660254037844387076, 1.000000000000000000, 0.8660254037844387076, 1.000000000000000000, 0.8660254037844387076, 1.000000000000000000, 0.8660254037844387076, 1.000000000000000000, 0.8660254037844387076, 1.000000000000000000, 0.8660254037844387076, 1.000000000000000000, 0.8660254037844387076, 1.000000000000000000, 0.8660254037844387076, 1.000000000000000000, 0.8660254037844387076, 1.000000000000000000, 0.8660254037844387076, 1.000000000000000000, 0.8660254037844387076, 1.000000000000000000, 0.8660254037844387076, 1.000000000000000000, 0.8660254037844387076, 1.000000000000000000, 0.8660254037844387076, 1.000000000000000000, 0.8660254037844387076, 1.000000000000000000, 0.8660254037844387076, 1.000000000000000000, 0.8660254037844387076, 1.000000000000000000, 0.8660254037844387076, 1.000000000000000000, 0.8660254037844387076, 1.000000000000000000, 0.8660254037844387076, 1.000000000000000000, 0.8660254037844387076, 1.000000000000000000, 0.8660254037844387076, 1.000000000000000000, 0.8660254037844387076, 1.000000000000000000, 0.8660254037844387076, 1.000000000000000000, 0.8660254037844387076, 1.000000000000000000, 0.8660254037844387076, 1.000000000000000000, 0.8660254037844387076, 1.000000000000000000, 0.8660254037844387076, 1.000000000000000000, 0.8660254037844387076, 1.000000000000000000, 0.8660254037844387076, 1.000000000000000000, 0.8660254037844387076, 1.000000000000000000, 0.8660254037844387076, 1.000000000000000000, 0.8660254037844387076, 1.000000000000000000, 0.8660254037844387076, 1.000000000000000000, 0.8660254037844387076, 1.000000000000000000, 0.8660254037844387076, 1.000000000000000000, 0.8660254037844387076, 1.000000000000000000, 0.8660254037844387076, 1.000000000000000000, 0.8660254037844387076, 1.000000000000000000, 0.8660254037844387076, 1.000000000000000000, 0.8660254037844387076, 1.000000000000000000, 0.8660254037844387076, 1.000000000000000000, 0.8660254037844387076, 1.000000000000000000, 0.8660254037844387076, 1.000000000000000000, 0.8660254037844387076, 1.000000000000000000, 0.8660254037844387076, 1.000000000000000000, 0.8660254037844387076, 1.000000000000000000, 0.8660254037844387076, 1.000000000000000000, 0.8660254037844387076, 1.000000000000000000, 0.8660254037844387076, 1.000000000000000000, 0.8660254037844387076, 1.000000000000000000, 0.8660254037844387076, 1.000000000000000000, 0.8660254037844387076, 1.000000000000000000, 0.8660254037844387076, 1.000000000000000000, 0.8660254037844387076, 1.000000000000000000, 0.8660254037844387076, 1.000000000000000000, 0.8660254037844387076, 1.000000000000000000, 0.8660254037844387076, 1.000000000000000000, 0.8660254037844387076, 1.000000000000000000, 0.8660254037844387076, 1.000000000000000000, 0.8660254037844387076, 1.000000000000000000, 0.8660254037844387076, 1.000000000000000000, 0.8660254037844387076, 1.000000000000000000, 0.8660254037844387076, 1.000000000000000000, 0.8660254037844387076, 1.000000000000000000, 0.8660254037844387076, 1.000000000000000000, 0.8660254037844387076, 1.000000000000000000, 0.8660254037844387076, 1.000000000000000000, 0.8660254037844387076, 1.000000000000000000, 0.8660254037844387076, 1.000000000000000000, 0.8660254037844387076, 1.000000000000000000, 0.8660254037844387076, 1.000000000000000000, 0.8660254037844387076, 1.000000000000000000, 0.8660254037844387076, 1.000000000000000000, 0.8660254037844387076, 1.000000000000000000, 0.8660254037844387076, 1.000000000000000000, 0.8660254037844387076, 1.000000000000000000, 0.8660254037844387076, 1.000000000000000000, 0.8660254037844387076, 1.000000000000000000, 0.8660254037844387076, 1.000000000000000000, 0.8660254037844387076, 1.000000000000000000, 0.8660254037844387076, 1.000000000000000000, 0.8660254037844387076, 1.000000000000000000, 0.8660254037844387076, 1.000000000000000000, 0.8660254037844387076, 1.000000000000000000, 0.8660254037844387076, 1.000000000000000000, 0.8660254037844387076, 1.000000000000000000, 0.8660254037844387076, 1.000000000000000000, 0.8660254037844387076, 1.000000000000000000, 0.8660254037844387076, 1.000000000000000000, 0.8660254037844387076, 1.000000000000000000, 0.8660254037844387076, 1.000000000000000000, 0.8660254037844387076, 1.000000000000000000, 0.8660254037844387076, 1.000000000000000000, 0.8660254037844387076, 1.000000000000000000, 0.8660254037844387076, 1.000000000000000000, 0.8660254037844387076, 1.000000000000000000, 0.8660254037844387076, 1.000000000000000000, 0.8660254037844387076, 1.000000000000000000, 0.8660254037844387076, 1.000000000000000000, 0.8660254037844387076, 1.000000000000000000, 0.8660254037844387076, 1.000000000000000000, 0.8660254037844387076, 1.000000000000000000, 0.8660254037844387076, 1.000000000000000000, 0.8660254037844387076, 1.000000000000000000, 0.8660254037844387076, 1.000000000000000000, 0.8660254037844387076, 1.000000000000000000, 0.8660254037844387076, 1.000000000000000000, 0.8660254037844387076, 1.000000000000000000, 0.8660254037844387076, 1.000000000000000000, 0.8660254037844387076, 1.000000000000000000, 0.8660254037844387076, 1.000000000000000000, 0.8660254037844387076, 1.000000000000000000, 0.8660254037844387076, 1.000000000000000000, 0.8660254037844387076, 1.000000000000000000, 0.8660254037844387076, 1.000000000000000000, 0.8660254037844387076, 1.000000000000000000, 0.8660254037844387076, 1.000000000000000000, 0.8660254037844387076, 1.000000000000000000, 0.8660254037844387076, 1.000000000000000000, 0.8660254037844387076, 1.000000000000000000, 0.8660254037844387076, 1.000000000000000000, 0.8660254037844387076, 1.000000000000000000, 0.8660254037844387076, 1.000000000000000000, 0.8660254037844387076, 1.000000000000000000, 0.8660254037844387076, 1.000000000000000000, 0.8660254037844387076, 1.000000000000000000, 0.8660254037844387076, 1.000000000000000000, 0.8660254037844387076, 1.000000000000000000, 0.8660254037844387076, 1.000000000000000000, 0.8660254037844387076, 1.000000000000000000, 0.8660254037844387076, 1.000000000000000000, 0.8660254037844387076, 1.000000000000000000, 0.8660254037844387076, 1.000000000000000000, 0.8660254037844387076, 1.000000000000000000, 0.8660254037844387076, 1.000000000000000000, 0.8660254037844387076, 1.000000000000000000, 0.8660254037844387076, 1.000000000000000000, 0.8660254037844387076, 1.000000000000000000, 0.8660254037844387076, 1.000000000000000000, 0.8660254037844387076, 1.000000000000000000, 0.8660254037844387076, 1.000000000000000000, 0.8660254037844387076, 1.000000000000000000, 0.8660254037844387076, 1.000000000000000000, 0.8660254037844387076, 1.000000000000000000, 0.8660254037844387076, 1.000000000000000000, 0.8660254037844387076, 1.000000000000000000, 0.8660254037844387076, 1.000000000000000000, 0.8660254037844387076, 1.000000000000000000, 0.8660254037844387076, 1.000000000000000000, 0.8660254037844387076, 1.000000000000000000, 0.8660254037844387076, 1.000000000000000000, 0.8660254037844387076, 1.000000000000000000, 0.8660254037844387076, 1.000000000000000000, 0.8660254037844387076, 1.000000000000000000, 0.8660254037844387076, 1.000000000000000000, 0.8660254037844387076, 1.000000000000000000, 0.8660254037844387076, 1.000000000000000000, 0.8660254037844387076, 1.000000000000000000, 0.8660254037844387076, 1.000000000000000000, 0.8660254037844387076, 1.000000000000000000, 0.8660254037844387076, 1.000000000000000000, 0.8660254037844387076, 1.000000000000000000, 0.8660254037844387076, 1.000000000000000000, 0.8660254037844387076, 1.000000000000000000, 0.8660254037844387076, 1.000000000000000000, 0.8660254037844387076, 1.000000000000000000, 0.8660254037844387076, 1.000000000000000000, 0.8660254037844387076, 1.000000000000000000, 0.8660254037844387076, 1.000000000000000000, 0.8660254037844387076, 1.000000000000000000, 0.8660254037844387076, 1.000000000000000000, 0.8660254037844387076, 1.000000000000000000, 0.8660254037844387076, 1.000000000000000000, 0.8660254037844387076, 1.000000000000000000, 0.8660254037844387076, 1.000000000000000000, 0.8660254037844387076, 1.000000000000000000, 0.8660254037844387076, 1.000000000000000000, 0.8660254037844387076, 1.000000000000000000, 0.8660254037844387076, 1.000000000000000000, 0.8660254037844387076, 1.000000000000000000, 0.8660254037844387076, 1.000000000000000000, 0.8660254037844387076, 1.000000000000000000, 0.8660254037844387076, 1.000000000000000000, 0.8660254037844387076, 1.000000000000000000, 0.8660254037844387076, 1.000000000000000000, 0.8660254037844387076, 1.000000000000000000, 0.8660254037844387076, 1.000000000000000000, 0.8660254037844387076, 1.000000000000000000, 0.8660254037844387076, 1.000000000000000000, 0.8660254037844387076, 1.000000000000000000, 0.8660254037844387076, 1.000000000000000000, 0.8660254037844387076, 1.000000000000000000, 0.8660254037844387076, 1.000000000000000000, 0.8660254037844387076, 1.000000000000000000, 0.8660254037844387076, 1.000000000000000000, 0.8660254037844387076, 1.000000000000000000, 0.8660254037844387076, 1.000000000000000000, 0.8660254037844387076, 1.000000000000000000, 0.8660254037844387076, 1.000000000000000000, 0.8660254037844387076, 1.000000000000000000, 0.8660254037844387076, 1.000000000000000000, 0.8660254037844387076, 1.000000000000000000, 0.8660254037844387076, 1.000000000000000000, 0.8660254037844387076, 1.000000000000000000, 0.8660254037844387076, 1.000000000000000000, 0.8660254037844387076, 1.000000000000000000, 0.8660254037844387076, 1.000000000000000000, 0.8660254037844387076, 1.000000000000000000, 0.8660254037844387076, 1.000000000000000000, 0.8660254037844387076, 1.000000000000000000, 0.8660254037844387076, 1.000000000000000000, 0.8660254037844387076, 1.000000000000000000, 0.8660254037844387076, 1.000000000000000000, 0.8660254037844387076, 1.000000000000000000, 0.8660254037844387076, 1.000000000000000000, 0.8660254037844387076, 1.000000000000000000, 0.8660254037844387076, 1.000000000000000000, 0.8660254037844387076, 1.000000000000000000, 0.8660254037844387076, 1.000000000000000000, 0.8660254037844387076, 1.000000000000000000, 0.8660254037844387076, 1.000000000000000000, 0.8660254037844387076, 1.000000000000000000, 0.8660254037844387076, 1.000000000000000000, 0.8660254037844387076, 1.000000000000000000, 0.8660254037844387076, 1.000000000000000000, 0.8660254037844387076, 1.000000000000000000, 0.8660254037844387076, 1.000000000000000000, 0.8660254037844387076, 1.000000000000000000, 0.8660254037844387076, 1.000000000000000000, 0.8660254037844387076, 1.000000000000000000, 0.8660254037844387076, 1.000000000000000000, 0.8660254037844387076, 1.000000000000000000, 0.8660254037844387076, 1.000000000000000000, 0.8660254037844387076, 1.000000000000000000, 0.8660254037844387076, 1.000000000000000000, 0.8660254037844387076, 1.000000000000000000, 0.8660254037844387076, 1.000000000000000000, 0.8660254037844387076, 1.000000000000000000, 0.8660254037844387076, 1.000000000000000000, 0.8660254037844387076, 1.000000000000000000, 0.8660254037844387076, 1.000000000000000000, 0.8660254037844387076, 1.000000000000000000, 0.8660254037844387076, 1.000000000000000000, 0.8660254037844387076, 1.000000000000000000, 0.8660254037844387076, 1.000000000000000000, 0.8660254037844387076, 1.000000000000000000, 0.8660254037844387076, 1.000000000000000000, 0.8660254037844387076, 1.000000000000000000, 0.8660254037844387076, 1.000000000000000000, 0.8660254037844387076, 1.000000000000000000, 0.8660254037844387076, 1.000000000000000000, 0.8660254037844387076, 1.000000000000000000, 0.8660254037844387076, 1.000000000000000000, 0.8660254037844387076, 1.000000000000000000, 0.8660254037844387076, 1.000000000000000000, 0.8660254037844387076, 1.000000000000000000, 0.8660254037844387076, 1.000000000000000000, 0.8660254037844387076, 1.000000000000000000, 0.8660254037844387076, 1.000000000000000000, 0.8660254037844387076, 1.000000000000000000, 0.8660254037844387076, 1.000000000000000000, 0.8660254037844387076, 1.000000000000000000, 0.8660254037844387076, 1.000000000000000000, 0.8660254037844387076, 1.000000000000000000, 0.8660254037844387076, 1.000000000000000000, 0.8660254037844387076, 1.000000000000000000, 0.8660254037844387076, 1.000000000000000000, 0.8660254037844387076, 1.000000000000000000, 0.8660254037844387076, 1.000000000000000000, 0.8660254037844387076, 1.000000000000000000, 0.8660254037844387076, 1.000000000000000000, 0.8660254037844387076, 1.000000000000000000, 0.8660254037844387076, 1.000000000000000000, 0.8660254037844387076, 1.000000000000000000, 0.8660254037844387076, 1.000000000000000000, 0.8660254037844387076, 1.000000000000000000, 0.8660254037844387076, 1.000000000000000000, 0.8660254037844387076, 1.000000000000000000, 0.8660254037844387076, 1.000000000000000000, 0.8660254037844387076, 1.000000000000000000, 0.8660254037844387076, 1.000000000000000000, 0.8660254037844387076, 1.000000000000000000, 0.8660254037844387076, 1.000000000000000000, 0.8660254037844387076, 1.000000000000000000, 0.8660254037844387076, 1.000000000000000000, 0.8660254037844387076, 1.000000000000000000, 0.8660254037844387076, 1.000000000000000000, 0.8660254037844387076, 1.000000000000000000, 0.8660254037844387076, 1.000000000000000000, 0.8660254037844387076, 1.000000000000000000, 0.8660254037844387076, 1.000000000000000000, 0.8660254037844387076, 1.000000000000000000, 0.8660254037844387076, 1.000000000000000000, 0.8660254037844387076, 1.000000000000000000, 0.8660254037844387076, 1.000000000000000000, 0.8660254037844387076, 1.000000000000000000, 0.8660254037844387076, 1.000000000000000000, 0.8660254037844387076, 1.000000000000000000, 0.8660254037844387076, 1.000000000000000000, 0.8660254037844387076, 1.000000000000000000, 0.8660254037844387076, 1.000000000000000000, 0.8660254037844387076, 1.000000000000000000, 0.8660254037844387076, 1.000000000000000000, 0.8660254037844387076, 1.000000000000000000, 0.8660254037844387076, 1.000000000000000000, 0.8660254037844387076, 1.000000000000000000, 0.8660254037844387076, 1.000000000000000000, 0.8660254037844387076, 1.000000000000000000, 0.8660254037844387076, 1.000000000000000000, 0.8660254037844387076, 1.000000000000000000, 0.8660254037844387076, 1.000000000000000000, 0.8660254037844387076, 1.000000000000000000, 0.8660254037844387076, 1.000000000000000000, 0.8660254037844387076, 1.000000000000000000, 0.8660254037844387076, 1.000000000000000000, 0.8660254037844387076, 1.000000000000000000, 0.8660254037844387076, 1.000000000000000000, 0.8660254037844387076, 1.000000000000000000, 0.8660254037844387076, 1.000000000000000000, 0.8660254037844387076, 1.000000000000000000, 0.8660254037844387076, 1.000000000000000000, 0.8660254037844387076, 1.000000000000000000, 0.8660254037844387076, 1.000000000000000000, 0.8660254037844387076, 1.000000000000000000, 0.8660254037844387076, 1.000000000000000000, 0.8660254037844387076, 1.000000000000000000, 0.8660254037844387076, 1.000000000000000000, 0.8660254037844387076, 1.000000000000000000, 0.8660254037844387076, 1.000000000000000000, 0.8660254037844387076, 1.000000000000000000, 0.8660254037844387076, 1.000000000000000000, 0.8660254037844387076, 1.000000000000000000, 0.8660254037844387076, 1.000000000000000000, 0.8660254037844387076, 1.000000000000000000, 0.8660254037844387076, 1.000000000000000000, 0.8660254037844387076, 1.000000000000000000, 0.8660254037844387076, 1.000000000000000000, 0.8660254037844387076, 1.000000000000000000, 0.8660254037844387076, 1.000000000000000000, 0.8660254037844387076, 1.000000000000000000, 0.8660254037844387076, 1.000000000000000000, 0.8660254037844387076, 1.000000000000000000, 0.8660254037844387076, 1.000000000000000000, 0.8660254037844387076, 1.000000000000000000, 0.8660254037844387076, 1.000000000000000000, 0.8660254037844387076, 1.000000000000000000, 0.8660254037844387076, 1.000000000000000000, 0.8660254037844387076, 1.000000000000000000, 0.8660254037844387076, 1.000000000000000000, 0.8660254037844387076, 1.000000000000000000, 0.8660254037844387076, 1.000000000000000000, 0.8660254037844387076, 1.000000000000000000, 0.8660254037844387076, 1.000000000000000000, 0.8660254037844387076, 1.000000000000000000, 0.8660254037844387076, 1.000000000000000000, 0.8660254037844387076, 1.000000000000000000, 0.8660254037844387076, 1.000000000000000000, 0.8660254037844387076, 1.000000000000000000, 0.8660254037844387076, 1.000000000000000000, 0.8660254037844387076, 1.000000000000000000, 0.8660254037844387076, 1.000000000000000000, 0.8660254037844387076, 1.000000000000000000, 0.8660254037844387076, 1.000000000000000000, 0.8660254037844387076, 1.000000000000000000, 0.8660254037844387076, 1.000000000000000000, 0.8660254037844387076, 1.000000000000000000, 0.8660254037844387076, 1.000000000000000000, 0.8660254037844387076, 1.000000000000000000, 0.8660254037844387076, 1.000000000000000000, 0.8660254037844387076, 1.000000000000000000, 0.8660254037844387076, 1.000000000000000000, 0.8660254037844387076, 1.000000000000000000, 0.8660254037844387076, 1.000000000000000000, 0.8660254037844387076, 1.000000000000000000, 0.8660254037844387076, 1.000000000000000000, 0.8660254037844387076, 1.000000000000000000, 0.8660254037844387076, 1.000000000000000000, 0.8660254037844387076, 1.000000000000000000, 0.8660254037844387076, 1.000000000000000000, 0.8660254037844387076, 1.000000000000000000, 0.8660254037844387076, 1.000000000000000000, 0.8660254037844387076, 1.000000000000000000, 0.8660254037844387076, 1.000000000000000000, 0.8660254037844387076, 1.000000000000000000, 0.8660254037844387076, 1.000000000000000000, 0.8660254037844387076, 1.000000000000000000, 0.8660254037844387076, 1.000000000000000000, 0.8660254037844387076, 1.000000000000000000, 0.8660254037844387076, 1.000000000000000000, 0.8660254037844387076, 1.000000000000000000, 0.8660254037844387076, 1.000000000000000000, 0.8660254037844387076, 1.000000000000000000, 0.8660254037844387076, 1.000000000000000000, 0.8660254037844387076, 1.000000000000000000, 0.8660254037844387076, 1.000000000000000000, 0.8660254037844387076, 1.000000000000000000, 0.8660254037844387076, 1.000000000000000000, 0.8660254037844387076, 1.000000000000000000, 0.8660254037844387076, 1.000000000000000000, 0.8660254037844387076, 1.000000000000000000, 0.8660254037844387076, 1.000000000000000000, 0.8660254037844387076, 1.000000000000000000, 0.8660254037844387076, 1.000000000000000000, 0.8660254037844387076, 1.000000000000000000, 0.8660254037844387076, 1.000000000000000000, 0.8660254037844387076, 1.000000000000000000, 0.8660254037844387076, 1.000000000000000000, 0.8660254037844387076, 1.000000000000000000, 0.8660254037844387076, 1.000000000000000000, 0.8660254037844387076, 1.000000000000000000, 0.8660254037844387076, 1.000000000000000000, 0.8660254037844387076, 1.000000000000000000, 0.8660254037844387076, 1.000000000000000000, 0.8660254037844387076, 1.000000000000000000, 0.8660254037844387076, 1.000000000000000000, 0.8660254037844387076, 1.000000000000000000, 0.8660254037844387076, 1.000000000000000000, 0.8660254037844387076, 1.000000000000000000, 0.8660254037844387076, 1.000000000000000000, 0.8660254037844387076, 1.000000000000000000, 0.8660254037844387076, 1.000000000000000000, 0.8660254037844387076, 1.000000000000000000, 0.8660254037844387076, 1.000000000000000000, 0.8660254037844387076, 1.000000000000000000, 0.8660254037844387076, 1.000000000000000000, 0.8660254037844387076, 1.000000000000000000, 0.8660254037844387076, 1.000000000000000000, 0.8660254037844387076, 1.000000000000000000, 0.8660254037844387076, 1.000000000000000000, 0.8660254037844387076, 1.000000000000000000, 0.8660254037844387076, 1.000000000000000000, 0.8660254037844387076, 1.000000000000000000, 0.8660254037844387076, 1.000000000000000000, 0.8660254037844387076, 1.000000000000000000, 0.8660254037844387076, 1.000000000000000000, 0.8660254037844387076, 1.000000000000000000, 0.8660254037844387076, 1.000000000000000000, 0.8660254037844387076, 1.000000000000000000, 0.8660254037844387076, 1.000000000000000000, 0.8660254037844387076, 1.000000000000000000, 0.8660254037844387076, 1.000000000000000000, 0.8660254037844387076, 1.000000000000000000, 0.8660254037844387076, 1.000000000000000000, 0.8660254037844387076, 1.000000000000000000, 0.8660254037844387076, 1.000000000000000000, 0.8660254037844387076, 1.000000000000000000, 0.8660254037844387076, 1.000000000000000000, 0.8660254037844387076, 1.000000000000000000, 0.8660254037844387076, 1.000000000000000000, 0.8660254037844387076, 1.000000000000000000, 0.8660254037844387076, 1.000000000000000000, 0.8660254037844387076, 1.000000000000000000, 0.8660254037844387076, 1.000000000000000000, 0.8660254037844387076, 1.000000000000000000, 0.8660254037844387076, 1.000000000000000000, 0.8660254037844387076, 1.000000000000000000, 0.8660254037844387076, 1.000000000000000000, 0.8660254037844387076, 1.000000000000000000, 0.8660254037844387076, 1.000000000000000000, 0.8660254037844387076, 1.000000000000000000, 0.8660254037844387076, 1.000000000000000000, 0.8660254037844387076, 1.000000000000000000, 0.8660254037844387076, 1.000000000000000000, 0.8660254037844387076, 1.000000000000000000, 0.8660254037844387076, 1.000000000000000000, 0.8660254037844387076, 1.000000000000000000, 0.8660254037844387076, 1.000000000000000000, 0.8660254037844387076, 1.000000000000000000, 0.8660254037844387076, 1.000000000000000000, 0.8660254037844387076, 1.000000000000000000, 0.8660254037844387076, 1.000000000000000000, 0.8660254037844387076, 1.000000000000000000, 0.8660254037844387076, 1.000000000000000000, 0.8660254037844387076, 1.000000000000000000, 0.8660254037844387076, 1.000000000000000000, 0.8660254037844387076, 1.000000000000000000, 0.8660254037844387076, 1.000000000000000000, 0.8660254037844387076, 1.000000000000000000, 0.8660254037844387076, 1.000000000000000000, 0.8660254037844387076, 1.000000000000000000, 0.8660254037844387076, 1.000000000000000000, 0.8660254037844387076, 1.000000000000000000, 0.8660254037844387076, 1.000000000000000000, 0.8660254037844387076, 1.000000000000000000, 0.8660254037844387076, 1.000000000000000000, 0.8660254037844387076, 1.000000000000000000, 0.8660254037844387076, 1.000000000000000000, 0.8660254037844387076, 1.000000000000000000, 0.8660254037844387076, 1.000000000000000000, 0.8660254037844387076, 1.000000000000000000, 0.8660254037844387076, 1.000000000000000000, 0.8660254037844387076, 1.000000000000000000, 0.8660254037844387076, 1.000000000000000000, 0.8660254037844387076, 1.000000000000000000, 0.8660254037844387076, 1.000000000000000000, 0.8660254037844387076, 1.000000000000000000, 0.8660254037844387076, 1.000000000000000000, 0.8660254037844387076, 1.000000000000000000, 0.8660254037844387076, 1.000000000000000000, 0.8660254037844387076, 1.000000000000000000, 0.8660254037844387076, 1.000000000000000000, 0.8660254037844387076, 1.000000000000000000, 0.8660254037844387076, 1.000000000000000000, 0.8660254037844387076, 1.000000000000000000, 0.8660254037844387076, 1.000000000000000000, 0.8660254037844387076, 1.000000000000000000, 0.8660254037844387076, 1.000000000000000000, 0.8660254037844387076, 1.000000000000000000, 0.9816628268209384167, 0.9683452906431763152 ) ) 
 REPRESENTATION_ITEM ( '' )  );
#7619 = ADVANCED_FACE ( 'NONE', ( #11128 ), #27553, .T. ) ;
#7620 = CARTESIAN_POINT ( 'NONE',  ( -10.81189881249999729, 6.242252689847871849, -149.4062500020484094 ) ) ;
#7621 = CARTESIAN_POINT ( 'NONE',  ( -5.405949406249996869, 9.363379034771805109, -135.8437500020484094 ) ) ;
#7622 = CARTESIAN_POINT ( 'NONE',  ( 9.999999999999998224, 0.000000000000000000, -104.3750000040967763 ) ) ;
#7623 = VERTEX_POINT ( 'NONE', #806 ) ;
#7624 = LINE ( 'NONE', #20994, #2469 ) ;
#7625 = EDGE_LOOP ( 'NONE', ( #39994, #19293, #21103, #27263 ) ) ;
#7626 = ORIENTED_EDGE ( 'NONE', *, *, #4173, .F. ) ;
#7628 = ORIENTED_EDGE ( 'NONE', *, *, #29925, .F. ) ;
#7627 = CARTESIAN_POINT ( 'NONE',  ( -10.81189881249999729, 1.324075727343319199E-15, -111.5937500020483810 ) ) ;
#7629 = EDGE_CURVE ( 'NONE', #17140, #40199, #30407, .T. ) ;
#7630 = CARTESIAN_POINT ( 'NONE',  ( 7.070501591499376803E-16, 11.54700538379251284, -129.5000000040967905 ) ) ;
#7631 = CARTESIAN_POINT ( 'NONE',  ( 10.81189881249999907, 6.242252689847868297, -188.7187500020484094 ) ) ;
#7632 = CC_DESIGN_APPROVAL ( #28088, ( #36593 ) ) ;
#7633 = CARTESIAN_POINT ( 'NONE',  ( -10.81189881249999729, 6.242252689847871849, -39.71875000204835970 ) ) ;
#7634 = CARTESIAN_POINT ( 'NONE',  ( -5.941590193206447879, -8.275517156161180665, 5.985441654281309245E-15 ) ) ;
#7635 = CARTESIAN_POINT ( 'NONE',  ( -9.999999999999998224, 1.224646799147353059E-15, -179.7500000000000284 ) ) ;
#7636 = AXIS2_PLACEMENT_3D ( 'NONE', #30722, #27252, #37398 ) ;
#7637 = CARTESIAN_POINT ( 'NONE',  ( -10.81189881249999729, -6.242252689847864744, -174.4687500020483526 ) ) ;
#7638 = CARTESIAN_POINT ( 'NONE',  ( -10.81189881249999729, 6.242252689847871849, -164.2187500020483810 ) ) ;
#7639 = CARTESIAN_POINT ( 'NONE',  ( 10.00000000000051159, -5.773502691895965988, -76.00000000409676204 ) ) ;
#7640 = CARTESIAN_POINT ( 'NONE',  ( -10.81189881249999729, 1.324075727343319199E-15, -141.5937500020483810 ) ) ;
#7641 = CARTESIAN_POINT ( 'NONE',  ( 5.405949406249992428, -9.363379034771808662, -153.0937500020483810 ) ) ;
#7642 = CARTESIAN_POINT ( 'NONE',  ( -5.000000000000003553, -8.660254037844383745, -93.99999999999998579 ) ) ;
#7643 = CARTESIAN_POINT ( 'NONE',  ( 7.070501591499376803E-16, 11.54700538379251284, -66.50000000409676204 ) ) ;
#7644 = CARTESIAN_POINT ( 'NONE',  ( -4.999999999999996447, 8.660254037844387298, -175.5000000000000284 ) ) ;
#7645 = CARTESIAN_POINT ( 'NONE',  ( -10.81189881249999729, 6.242252689847871849, -90.71875000204838102 ) ) ;
#7646 = CARTESIAN_POINT ( 'NONE',  ( -3.547780718846140324, 10.23789773687130733, -99.99999999999994316 ) ) ;
#7647 = CARTESIAN_POINT ( 'NONE',  ( -10.81189881249999729, 1.324075727343319199E-15, -56.28125000204836681 ) ) ;
#7648 = DIRECTION ( 'NONE',  ( 0.000000000000000000, 0.000000000000000000, 1.000000000000000000 ) ) ;
#7649 = CARTESIAN_POINT ( 'NONE',  ( 5.405949406249999534, 9.363379034771803333, -178.0937500020484094 ) ) ;
#7650 = CARTESIAN_POINT ( 'NONE',  ( -10.81189881249999729, 6.242252689847871849, -123.9062500020483952 ) ) ;
#7651 = CARTESIAN_POINT ( 'NONE',  ( -10.81189881249999729, -6.242252689847864744, -158.1562500020484094 ) ) ;
#7652 = CARTESIAN_POINT ( 'NONE',  ( -4.999999999999996447, 8.660254037844387298, -115.4999999999999858 ) ) ;
#7653 = CARTESIAN_POINT ( 'NONE',  ( -2.293366432827344421E-15, -12.48450537969573659, -51.40625000204837391 ) ) ;
#7654 = CARTESIAN_POINT ( 'NONE',  ( -2.121150477449813534E-15, -11.54700538379251284, -128.7500000040967620 ) ) ;
#7655 = CARTESIAN_POINT ( 'NONE',  ( 9.999999999999996447, -5.773502691896262640, -104.1249999999999858 ) ) ;
#7656 = VERTEX_POINT ( 'NONE', #4455 ) ;
#7657 = CARTESIAN_POINT ( 'NONE',  ( 5.405949406249992428, -9.363379034771808662, -133.7812500020483810 ) ) ;
#7658 = CARTESIAN_POINT ( 'NONE',  ( 4.999999999999992006, -8.660254037844389075, -145.1250000040967905 ) ) ;
#7659 = CARTESIAN_POINT ( 'NONE',  ( -10.81189881249999729, 1.324075727343319199E-15, -150.7812500020483810 ) ) ;
#7660 = CARTESIAN_POINT ( 'NONE',  ( -5.405949406250003975, -9.363379034771801557, -192.5312500020484094 ) ) ;
#7661 = ORIENTED_EDGE ( 'NONE', *, *, #6173, .F. ) ;
#7662 = CARTESIAN_POINT ( 'NONE',  ( -4.999999999999996447, 8.660254037844387298, -50.99999999999996447 ) ) ;
#7663 = CARTESIAN_POINT ( 'NONE',  ( 10.81189881249999551, -6.242252689847874514, -181.4687500020484094 ) ) ;
#7664 = CARTESIAN_POINT ( 'NONE',  ( 7.070501591499377789E-16, 11.54700538379251284, -60.50000000409677625 ) ) ;
#7665 = CARTESIAN_POINT ( 'NONE',  ( -10.00000000000025580, 5.773502691896109873, -152.8750000000000000 ) ) ;
#7666 = DIRECTION ( 'NONE',  ( -1.000000000000000000, 0.000000000000000000, 0.000000000000000000 ) ) ;
#7667 = CARTESIAN_POINT ( 'NONE',  ( 10.81189881249999551, -6.242252689847874514, -79.65625000204838102 ) ) ;
#7668 = CARTESIAN_POINT ( 'NONE',  ( -10.81189881249999729, 6.242252689847871849, -48.90625000204837391 ) ) ;
#7669 = AXIS2_PLACEMENT_3D ( 'NONE', #22746, #35913, #6136 ) ;
#7670 = CARTESIAN_POINT ( 'NONE',  ( 9.999999999999996447, -5.773502691896262640, -50.50000000409676915 ) ) ;
#7671 = CARTESIAN_POINT ( 'NONE',  ( -5.405949406249996869, 9.363379034771805109, -9.843750002048345493 ) ) ;
#7672 = CARTESIAN_POINT ( 'NONE',  ( 0.000000000000000000, 0.000000000000000000, -200.0000000000000000 ) ) ;
#7673 = CARTESIAN_POINT ( 'NONE',  ( 7.644554776091147741E-16, 12.48450537969573659, -178.1562500020484094 ) ) ;
#7674 = CC_DESIGN_APPROVAL ( #30720, ( #4933 ) ) ;
#7675 = CARTESIAN_POINT ( 'NONE',  ( -5.405949406249996869, 9.363379034771805109, -5.531250002048376579 ) ) ;
#7676 = DIRECTION ( 'NONE',  ( -1.000000000000000000, 0.000000000000000000, 0.000000000000000000 ) ) ;
#7677 = DIRECTION ( 'NONE',  ( -0.000000000000000000, -0.000000000000000000, -1.000000000000000000 ) ) ;
#7678 = DIRECTION ( 'NONE',  ( -0.000000000000000000, -0.000000000000000000, -1.000000000000000000 ) ) ;
#7679 = DIRECTION ( 'NONE',  ( 0.000000000000000000, 0.9961946980917455452, -0.08715574274765837404 ) ) ;
#7680 = CARTESIAN_POINT ( 'NONE',  ( 10.00000000000025402, -5.773502691896113426, -163.0000000040967905 ) ) ;
#7682 = VERTEX_POINT ( 'NONE', #14356 ) ;
#7681 = CARTESIAN_POINT ( 'NONE',  ( -10.81189881249999729, 6.242252689847871849, -87.90625000204838102 ) ) ;
#7684 = EDGE_LOOP ( 'NONE', ( #33652, #17316, #37883, #3215 ) ) ;
#7683 = CARTESIAN_POINT ( 'NONE',  ( 7.070501591499376803E-16, 11.54700538379251284, -92.00000000409677625 ) ) ;
#7685 = ORIENTED_EDGE ( 'NONE', *, *, #30937, .F. ) ;
#7686 = CARTESIAN_POINT ( 'NONE',  ( 5.405949406249999534, 9.363379034771803333, -38.59375000204837391 ) ) ;
#7687 = CARTESIAN_POINT ( 'NONE',  ( -2.293366432827344421E-15, -12.48450537969573659, -28.71875000204835615 ) ) ;
#7688 = CARTESIAN_POINT ( 'NONE',  ( 10.81189881249999551, -6.242252689847874514, -15.15625000204837036 ) ) ;
#7689 = CARTESIAN_POINT ( 'NONE',  ( 5.405949406249999534, 9.363379034771803333, -62.59375000204836681 ) ) ;
#7690 = CARTESIAN_POINT ( 'NONE',  ( -4.999999999999996447, 8.660254037844387298, -163.8750000040967905 ) ) ;
#7691 = EDGE_CURVE ( 'NONE', #17801, #23753, #40688, .T. ) ;
#7692 = CARTESIAN_POINT ( 'NONE',  ( -4.999999999999996447, 8.660254037844387298, -44.99999999999998579 ) ) ;
#7693 = CARTESIAN_POINT ( 'NONE',  ( -5.405949406250003975, -9.363379034771801557, -183.3437500020483810 ) ) ;
#7694 = ADVANCED_FACE ( 'NONE', ( #31013 ), #4667, .T. ) ;
#7695 = CARTESIAN_POINT ( 'NONE',  ( 5.405949406249999534, 9.363379034771803333, -169.0937500020484094 ) ) ;
#7696 = VECTOR ( 'NONE', #37669, 1000.000000000000000 ) ;
#7697 = CARTESIAN_POINT ( 'NONE',  ( -10.81189881249999729, 6.242252689847871849, -174.7187500020484379 ) ) ;
#7698 = CARTESIAN_POINT ( 'NONE',  ( 0.000000000000000000, 0.000000000000000000, -200.0000000000000000 ) ) ;
#7699 = DIRECTION ( 'NONE',  ( 1.000000000000000000, 0.000000000000000000, 0.000000000000000000 ) ) ;
#7700 = CARTESIAN_POINT ( 'NONE',  ( 9.999999999999998224, 0.000000000000000000, -104.3750000040967763 ) ) ;
#7701 = DIRECTION ( 'NONE',  ( 1.000000000000000000, 0.000000000000000000, 0.000000000000000000 ) ) ;
#7702 = APPROVAL_PERSON_ORGANIZATION ( #16101, #30950, #25851 ) ;
#7704 = CARTESIAN_POINT ( 'NONE',  ( 10.81189881249999907, 6.242252689847868297, -110.7187500020483810 ) ) ;
#7703 = APPLICATION_CONTEXT ( 'configuration controlled 3d designs of mechanical parts and assemblies' ) ;
#7705 = CYLINDRICAL_SURFACE ( 'NONE', #1809, 9.999999999999998224 ) ;
#7706 = CARTESIAN_POINT ( 'NONE',  ( -10.81189881249999729, 6.242252689847871849, -93.90625000204839523 ) ) ;
#7707 = CARTESIAN_POINT ( 'NONE',  ( -10.81189881249999729, 6.242252689847871849, -98.21875000204838102 ) ) ;
#7708 =( BOUNDED_CURVE ( )  B_SPLINE_CURVE ( 2, ( #15777, #28974, #9320, #40351, #34501, #27206, #33489 ),
 .UNSPECIFIED., .F., .F. ) 
 B_SPLINE_CURVE_WITH_KNOTS ( ( 3, 2, 2, 3 ),
 ( 0.3022388059701494045, 0.3034825870646767343, 0.3047263681592040085, 0.3059701492537313383 ),
 .UNSPECIFIED. ) 
 CURVE ( )  GEOMETRIC_REPRESENTATION_ITEM ( )  RATIONAL_B_SPLINE_CURVE ( ( 0.9999999999999820144, 0.8660254037844566932, 1.000000000000000000, 0.8660254037844387076, 1.000000000000000000, 0.8660254037844387076, 1.000000000000000000 ) ) 
 REPRESENTATION_ITEM ( '' )  );
#7709 = CARTESIAN_POINT ( 'NONE',  ( -10.81189881249999907, -6.242252689847864744, -69.46875000204838102 ) ) ;
#7710 = CARTESIAN_POINT ( 'NONE',  ( -10.81189881249999907, -6.242252689847864744, -77.15625000204836681 ) ) ;
#7711 = CARTESIAN_POINT ( 'NONE',  ( -5.000000000000003553, -8.660254037844383745, -157.3750000040967905 ) ) ;
#7712 = CARTESIAN_POINT ( 'NONE',  ( -9.999999999999998224, 5.773502691896259087, -128.8749999999999716 ) ) ;
#7713 = CARTESIAN_POINT ( 'NONE',  ( 10.81189881249999729, 6.242252689847867408, -160.4062500020483810 ) ) ;
#7714 = CARTESIAN_POINT ( 'NONE',  ( 10.81189881249999907, 6.242252689847868297, -170.9062500020484094 ) ) ;
#7715 = VECTOR ( 'NONE', #28163, 1000.000000000000000 ) ;
#7716 = DIRECTION ( 'NONE',  ( 1.000000000000000000, 0.000000000000000000, -0.000000000000000000 ) ) ;
#7717 = PLANE ( 'NONE',  #14392 ) ;
#7718 = CARTESIAN_POINT ( 'NONE',  ( 5.405949406249992428, -9.363379034771808662, -106.5937500020483810 ) ) ;
#7719 = CARTESIAN_POINT ( 'NONE',  ( -9.999999999999998224, 1.224646799147353059E-15, -18.12500000409675138 ) ) ;
#7720 = CARTESIAN_POINT ( 'NONE',  ( -5.000000000000003553, -8.660254037844383745, -69.99999999999998579 ) ) ;
#7721 = CARTESIAN_POINT ( 'NONE',  ( 10.81189881249999729, 0.000000000000000000, -1.531250002048373249 ) ) ;
#7722 = CARTESIAN_POINT ( 'NONE',  ( -2.121150477449813534E-15, -11.54700538379251284, -79.25000000409677625 ) ) ;
#7723 = CARTESIAN_POINT ( 'NONE',  ( -9.999999999999998224, 1.224646799147353059E-15, -169.2500000000000000 ) ) ;
#7724 = CARTESIAN_POINT ( 'NONE',  ( -10.81189881249999729, 1.324075727343319199E-15, -98.28125000204839523 ) ) ;
#7725 = CARTESIAN_POINT ( 'NONE',  ( 10.81189881249999551, -6.242252689847874514, -81.15625000204842365 ) ) ;
#7726 = CARTESIAN_POINT ( 'NONE',  ( 9.999999999999996447, -5.773502691896262640, -77.50000000409677625 ) ) ;
#7727 = CARTESIAN_POINT ( 'NONE',  ( -10.81189881249999907, -6.242252689847864744, -34.96875000204835260 ) ) ;
#7728 = ORIENTED_EDGE ( 'NONE', *, *, #12285, .T. ) ;
#7729 = CARTESIAN_POINT ( 'NONE',  ( 4.999999999999992006, -8.660254037844389075, -2.249999999999974243 ) ) ;
#7730 = CARTESIAN_POINT ( 'NONE',  ( -10.81189881249999907, -6.242252689847864744, -30.65625000204835970 ) ) ;
#7731 = CARTESIAN_POINT ( 'NONE',  ( 10.81189881249999729, 0.000000000000000000, -11.84375000204834727 ) ) ;
#7732 = CARTESIAN_POINT ( 'NONE',  ( 9.999999999999998224, 0.000000000000000000, -143.0000000000000000 ) ) ;
#7733 = CARTESIAN_POINT ( 'NONE',  ( -2.121150477449813534E-15, -11.54700538379251284, -1.250000004096751827 ) ) ;
#7734 = CARTESIAN_POINT ( 'NONE',  ( -10.81189881249999729, 1.324075727343319199E-15, -132.7812500020483810 ) ) ;
#7735 = AXIS2_PLACEMENT_3D ( 'NONE', #11600, #8398, #21548 ) ;
#7736 = CARTESIAN_POINT ( 'NONE',  ( -10.00000000000000000, -5.773502691896251982, -179.6250000000000284 ) ) ;
#7737 = DIRECTION ( 'NONE',  ( -0.000000000000000000, -0.000000000000000000, 1.000000000000000000 ) ) ;
#7739 = EDGE_LOOP ( 'NONE', ( #17673, #41789, #9274, #16614 ) ) ;
#7738 = CARTESIAN_POINT ( 'NONE',  ( -10.81189881249999907, -6.242252689847864744, -110.1562500020483952 ) ) ;
#7740 = LINE ( 'NONE', #14395, #22093 ) ;
#7741 = ORIENTED_EDGE ( 'NONE', *, *, #41735, .T. ) ;
#7742 = ORIENTED_EDGE ( 'NONE', *, *, #8237, .F. ) ;
#7743 = CARTESIAN_POINT ( 'NONE',  ( -5.405949406249996869, 9.363379034771805109, -34.03125000204837391 ) ) ;
#7744 = DATE_AND_TIME ( #24805, #42124 ) ;
#7745 = VECTOR ( 'NONE', #37993, 1000.000000000000000 ) ;
#7746 = CARTESIAN_POINT ( 'NONE',  ( 10.81189881249999907, 6.242252689847868297, -89.71875000204836681 ) ) ;
#7747 = CARTESIAN_POINT ( 'NONE',  ( -9.999999999999998224, 1.224646799147353059E-15, -196.6250000040967905 ) ) ;
#7748 = EDGE_CURVE ( 'NONE', #36438, #8116, #902, .T. ) ;
#7749 = LINE ( 'NONE', #37305, #13506 ) ;
#7750 = EDGE_CURVE ( 'NONE', #18023, #36127, #24362, .T. ) ;
#7751 =( BOUNDED_CURVE ( )  B_SPLINE_CURVE ( 2, ( #20603, #17145, #20819, #10672, #27094, #34005, #30346 ),
 .UNSPECIFIED., .F., .F. ) 
 B_SPLINE_CURVE_WITH_KNOTS ( ( 3, 2, 2, 3 ),
 ( 0.1679104477611940427, 0.1691542288557214002, 0.1703980099502487855, 0.1716417910447761430 ),
 .UNSPECIFIED. ) 
 CURVE ( )  GEOMETRIC_REPRESENTATION_ITEM ( )  RATIONAL_B_SPLINE_CURVE ( ( 1.000000000000000000, 0.8660254037844387076, 1.000000000000000000, 0.8660254037844387076, 1.000000000000000000, 0.8660254037844357100, 1.000000000000003109 ) ) 
 REPRESENTATION_ITEM ( '' )  );
#7752 = DIRECTION ( 'NONE',  ( -0.000000000000000000, -0.000000000000000000, 1.000000000000000000 ) ) ;
#7753 = CARTESIAN_POINT ( 'NONE',  ( -10.81189881249999907, -6.242252689847864744, -168.6562500020483810 ) ) ;
#7754 = CARTESIAN_POINT ( 'NONE',  ( -9.999999999999998224, 1.224646799147353059E-15, -68.74999999999997158 ) ) ;
#7755 = EDGE_CURVE ( 'NONE', #14989, #27111, #11989, .T. ) ;
#7756 = CARTESIAN_POINT ( 'NONE',  ( -5.405949406249996869, 9.363379034771805109, -126.8437500020483952 ) ) ;
#7757 = PRODUCT_RELATED_PRODUCT_CATEGORY ( 'detail', '', ( #14563 ) ) ;
#7758 = CARTESIAN_POINT ( 'NONE',  ( 7.644554776091147741E-16, 12.48450537969573659, -96.96875000204838102 ) ) ;
#7759 = CARTESIAN_POINT ( 'NONE',  ( -2.293366432827344421E-15, -12.48450537969573659, -3.406250002048348158 ) ) ;
#7760 = FACE_OUTER_BOUND ( 'NONE', #38550, .T. ) ;
#7761 = CARTESIAN_POINT ( 'NONE',  ( 5.405949406249999534, 9.363379034771803333, -97.28125000204839523 ) ) ;
#7762 = CARTESIAN_POINT ( 'NONE',  ( -9.999999999999998224, 1.224646799147353059E-15, -174.1250000040968189 ) ) ;
#7763 = CARTESIAN_POINT ( 'NONE',  ( -10.81189881249999729, 1.324075727343319199E-15, -110.0937500020483810 ) ) ;
#7764 = CARTESIAN_POINT ( 'NONE',  ( 5.405949406249992428, -9.363379034771808662, -175.7812500020484094 ) ) ;
#7765 =( BOUNDED_CURVE ( )  B_SPLINE_CURVE ( 2, ( #17153, #4863, #7462, #20612, #27744, #17795, #30354 ),
 .UNSPECIFIED., .F., .F. ) 
 B_SPLINE_CURVE_WITH_KNOTS ( ( 3, 2, 2, 3 ),
 ( 0.2537313432835822113, 0.2549751243781095411, 0.2562189054726369264, 0.2574626865671643117 ),
 .UNSPECIFIED. ) 
 CURVE ( )  GEOMETRIC_REPRESENTATION_ITEM ( )  RATIONAL_B_SPLINE_CURVE ( ( 0.9999999999999880096, 0.8660254037844506980, 1.000000000000000000, 0.8660254037844387076, 1.000000000000000000, 0.8660254037844267172, 1.000000000000011990 ) ) 
 REPRESENTATION_ITEM ( '' )  );
#7766 = CARTESIAN_POINT ( 'NONE',  ( 0.000000000000000000, 0.000000000000000000, -200.0000000000000000 ) ) ;
#7767 = CARTESIAN_POINT ( 'NONE',  ( -79.99999999999994316, -20.00000000000000711, -160.0000000000000000 ) ) ;
#7768 = CARTESIAN_POINT ( 'NONE',  ( -2.293366432827344421E-15, -12.48450537969573659, -196.9062500020484094 ) ) ;
#7769 = CARTESIAN_POINT ( 'NONE',  ( 5.405949406249992428, -9.363379034771808662, -49.59375000204838102 ) ) ;
#7770 = CARTESIAN_POINT ( 'NONE',  ( 5.405949406249992428, -9.363379034771808662, -42.09375000204837391 ) ) ;
#7771 = CARTESIAN_POINT ( 'NONE',  ( 9.999999999999996447, -5.773502691896262640, -173.5000000040968189 ) ) ;
#7772 = CARTESIAN_POINT ( 'NONE',  ( 10.81189881249999729, 0.000000000000000000, -13.53125000204835615 ) ) ;
#7773 = CARTESIAN_POINT ( 'NONE',  ( 10.81189881249999729, 0.000000000000000000, -17.84375000204835260 ) ) ;
#7774 = CARTESIAN_POINT ( 'NONE',  ( 9.999999999999479527, 5.773502691896553074, -145.8750000000000000 ) ) ;
#7775 = CARTESIAN_POINT ( 'NONE',  ( -10.81189881249999729, 1.324075727343319199E-15, -128.0937500020483810 ) ) ;
#7776 = CARTESIAN_POINT ( 'NONE',  ( -5.000000000000003553, -8.660254037844383745, -99.99999999999998579 ) ) ;
#7777 = CARTESIAN_POINT ( 'NONE',  ( -10.81189881249999907, -6.242252689847864744, -26.15625000204838102 ) ) ;
#7778 = CARTESIAN_POINT ( 'NONE',  ( 9.999999999999998224, 0.000000000000000000, -114.8750000040967905 ) ) ;
#7779 = CARTESIAN_POINT ( 'NONE',  ( -9.999999999999998224, 1.224646799147353059E-15, -200.0000000000000000 ) ) ;
#7780 = CARTESIAN_POINT ( 'NONE',  ( -5.000000000000003553, -8.660254037844383745, -62.49999999999997158 ) ) ;
#7781 = CARTESIAN_POINT ( 'NONE',  ( 7.644554776091147741E-16, 12.48450537969573659, -121.1562500020483952 ) ) ;
#7782 = CARTESIAN_POINT ( 'NONE',  ( -5.405949406250003975, -9.363379034771801557, -111.5312500020483810 ) ) ;
#7783 = ORIENTED_EDGE ( 'NONE', *, *, #20719, .F. ) ;
#7784 = CARTESIAN_POINT ( 'NONE',  ( -4.999999999999996447, 8.660254037844387298, -7.875000004096744277 ) ) ;
#7785 = CARTESIAN_POINT ( 'NONE',  ( -4.999999999999996447, 8.660254037844387298, -99.37500000409679046 ) ) ;
#7786 = CARTESIAN_POINT ( 'NONE',  ( 10.00000000000076916, -5.773502691895816774, -113.1249999999999716 ) ) ;
#7787 = CARTESIAN_POINT ( 'NONE',  ( 10.81189881249999551, -6.242252689847874514, -163.6562500020484094 ) ) ;
#7788 = CARTESIAN_POINT ( 'NONE',  ( 5.405949406249999534, 9.363379034771803333, -58.09375000204835970 ) ) ;
#7790 = EDGE_CURVE ( 'NONE', #17641, #25374, #8560, .T. ) ;
#7789 = ORIENTED_EDGE ( 'NONE', *, *, #18009, .T. ) ;
#7791 = CARTESIAN_POINT ( 'NONE',  ( 10.00000000000000000, 5.773502691896255534, -25.87499999999997868 ) ) ;
#7792 = VECTOR ( 'NONE', #10618, 1000.000000000000000 ) ;
#7793 = CARTESIAN_POINT ( 'NONE',  ( 10.81189881249999729, 6.242252689847867408, -34.40625000204836681 ) ) ;
#7794 = CARTESIAN_POINT ( 'NONE',  ( 9.999999999999998224, 0.000000000000000000, -162.5000000000000000 ) ) ;
#7795 = CARTESIAN_POINT ( 'NONE',  ( 9.999999999999998224, 0.000000000000000000, -15.49999999999995737 ) ) ;
#7796 = CARTESIAN_POINT ( 'NONE',  ( -9.999999999999998224, 5.773502691896259087, -25.75000000409677625 ) ) ;
#7797 = CARTESIAN_POINT ( 'NONE',  ( -10.81189881249999907, -6.242252689847864744, -132.6562500020484094 ) ) ;
#7798 = CYLINDRICAL_SURFACE ( 'NONE', #6260, 9.999999999999998224 ) ;
#7799 = EDGE_LOOP ( 'NONE', ( #37780, #20677, #30661, #7300, #35776, #18181, #41937, #19352, #1106, #29399, #32439, #4763, #37515, #3965, #13074, #2439, #32178, #36375, #31000, #3010, #32162, #163, #19144, #34293, #37175, #14888, #42162, #17994, #20998, #23861, #6678, #6153, #35070, #12238, #12337, #34612, #23298, #5037, #13222, #3359, #33995, #41267, #16394, #19508, #6294, #42646, #40139, #39293, #16889, #13127, #11810, #36399, #27479, #31700, #41294, #17776, #41043, #13178, #33283, #31224, #4169, #14815, #16345, #32634, #5888, #1105, #2606, #19147, #13914, #36451, #20889, #34109, #35146, #10906, #39338, #24239, #41648, #22929, #41351, #16186, #27364, #11848, #12338, #31867, #34851, #12759, #35983, #21908, #20838, #22233, #21047, #24370, #15603, #28448, #39933, #24635, #12396, #21527, #42195, #30460, #1589, #36298, #30147, #20513, #40671, #37121, #12495, #42119, #7367, #314, #28295, #1951, #14773, #2970, #22957, #19668, #3017, #2391, #38144, #20561, #30039, #1642, #22658, #2166, #11971, #24736, #24840, #11171, #24853, #10945, #16823, #3285, #794, #15399, #42378, #14123, #29501, #30253, #35251, #19880, #27054, #16792, #38285, #23240, #12235, #12951, #15826, #42357, #11652, #30144, #38471, #30978, #833, #12946, #21377, #11545, #40515, #19455, #22712, #9483, #17039, #38002, #21023, #7626, #33686, #24408, #22820, #167, #12755, #34494, #34343, #16022, #39418, #6506, #36456, #31588, #11308, #18296, #23814, #38158, #26535, #5038, #11919, #7877, #13599, #3427, #16673, #42643, #2505, #35672, #13437, #4233, #25223, #35089, #30520, #32097, #15730, #14221, #38637, #28915, #16144, #29696, #8012, #4019, #42406, #11327, #41042, #39887, #11214, #21260, #42488, #41028, #1323, #31862, #26733, #38368, #17739, #3853, #24990, #41744, #11381, #21092, #24672, #6390, #17530, #7993, #5761, #22339, #22544, #36700, #25728, #12964, #29758, #22362, #34131, #14124, #14265, #22024, #15263, #15621, #9168, #38526, #20675, #4656, #31417, #4587, #32594, #15649, #34446, #19507, #26206, #24621, #203, #4927, #6456, #42170, #34608, #11688, #3182, #28879, #22910, #33752, #20713, #5464, #26738, #9587, #21858, #26868, #34219, #12704 ) ) ;
#7801 = ORIENTED_EDGE ( 'NONE', *, *, #6146, .T. ) ;
#7800 = ORIENTED_EDGE ( 'NONE', *, *, #22997, .T. ) ;
#7802 = FACE_OUTER_BOUND ( 'NONE', #41194, .T. ) ;
#7803 = CARTESIAN_POINT ( 'NONE',  ( 4.999999999999992006, -8.660254037844389075, -55.12500000409675494 ) ) ;
#7804 = CARTESIAN_POINT ( 'NONE',  ( 10.81189881249999551, -6.242252689847874514, -163.4687500020483810 ) ) ;
#7805 = CARTESIAN_POINT ( 'NONE',  ( -10.81189881249999729, 6.242252689847871849, -195.9062500020484094 ) ) ;
#7806 = CARTESIAN_POINT ( 'NONE',  ( -5.405949406250003975, -9.363379034771801557, -16.84375000204835260 ) ) ;
#7807 = CARTESIAN_POINT ( 'NONE',  ( 0.000000000000000000, 0.000000000000000000, -200.0000000000000000 ) ) ;
#7808 = CARTESIAN_POINT ( 'NONE',  ( 5.405949406249992428, -9.363379034771808662, -147.0937500020483810 ) ) ;
#7809 = CARTESIAN_POINT ( 'NONE',  ( -10.81189881249999907, -6.242252689847864744, -139.9687500020483810 ) ) ;
#7810 = CARTESIAN_POINT ( 'NONE',  ( -5.405949406250003975, -9.363379034771801557, -104.0312500020483810 ) ) ;
#7811 = CARTESIAN_POINT ( 'NONE',  ( 10.81189881249999907, 6.242252689847868297, -116.7187500020483810 ) ) ;
#7812 = CARTESIAN_POINT ( 'NONE',  ( 10.00000000000000000, 5.773502691896255534, -198.7500000040968189 ) ) ;
#7813 = CARTESIAN_POINT ( 'NONE',  ( -5.405949406250003975, -9.363379034771801557, -123.5312500020483952 ) ) ;
#7814 = CARTESIAN_POINT ( 'NONE',  ( -5.405949406250003975, -9.363379034771801557, -10.84375000204834727 ) ) ;
#7815 = CARTESIAN_POINT ( 'NONE',  ( 10.81189881249999551, -6.242252689847874514, -127.4687500020483810 ) ) ;
#7816 = CARTESIAN_POINT ( 'NONE',  ( 9.999999999999998224, 0.000000000000000000, -174.8750000040967905 ) ) ;
#7817 = FACE_OUTER_BOUND ( 'NONE', #27002, .T. ) ;
#7818 = CARTESIAN_POINT ( 'NONE',  ( 10.00000000000000000, 5.773502691896255534, -157.8749999999999716 ) ) ;
#7819 = CARTESIAN_POINT ( 'NONE',  ( 9.999999999999998224, 0.000000000000000000, -16.99999999999996092 ) ) ;
#7820 = EDGE_CURVE ( 'NONE', #437, #22340, #39210, .T. ) ;
#7821 = CARTESIAN_POINT ( 'NONE',  ( -5.405949406249996869, 9.363379034771805109, -75.84375000204838102 ) ) ;
#7822 = CARTESIAN_POINT ( 'NONE',  ( 10.81189881249999907, 6.242252689847868297, -65.71875000204836681 ) ) ;
#7823 = LINE ( 'NONE', #24663, #40788 ) ;
#7824 = CARTESIAN_POINT ( 'NONE',  ( 7.644554776091147741E-16, 12.48450537969573659, -34.15625000204836681 ) ) ;
#7825 = CARTESIAN_POINT ( 'NONE',  ( 5.405949406249999534, 9.363379034771803333, -44.59375000204837391 ) ) ;
#7826 = CARTESIAN_POINT ( 'NONE',  ( -2.121150477449813534E-15, -11.54700538379251284, -110.7500000040967620 ) ) ;
#7827 = CARTESIAN_POINT ( 'NONE',  ( 10.81189881249999729, 0.000000000000000000, -157.3437500020483810 ) ) ;
#7828 = CARTESIAN_POINT ( 'NONE',  ( -9.999999999999998224, 1.224646799147353059E-15, -119.7500000000000000 ) ) ;
#7829 = CARTESIAN_POINT ( 'NONE',  ( -2.293366432827344421E-15, -12.48450537969573659, -129.4062500020483810 ) ) ;
#7830 = CYLINDRICAL_SURFACE ( 'NONE', #31401, 9.999999999999998224 ) ;
#7831 = CARTESIAN_POINT ( 'NONE',  ( 9.999999999999996447, -5.773502691896262640, -86.12499999999998579 ) ) ;
#7832 = CARTESIAN_POINT ( 'NONE',  ( 7.644554776091147741E-16, 12.48450537969573659, -14.65625000204836859 ) ) ;
#7833 = ORIENTED_EDGE ( 'NONE', *, *, #2216, .T. ) ;
#7834 = CARTESIAN_POINT ( 'NONE',  ( 10.81189881249999729, 0.000000000000000000, -105.0312500020483810 ) ) ;
#7835 = CARTESIAN_POINT ( 'NONE',  ( 10.00000000000000000, 5.773502691896255534, -120.7500000040967905 ) ) ;
#7836 = CARTESIAN_POINT ( 'NONE',  ( -2.121150477449813534E-15, -11.54700538379251284, -56.75000000409677625 ) ) ;
#7837 = CARTESIAN_POINT ( 'NONE',  ( 10.00000000000000000, 5.773502691896255534, -32.25000000409675494 ) ) ;
#7838 =( BOUNDED_CURVE ( )  B_SPLINE_CURVE ( 2, ( #7334, #17445, #33462, #14418, #14197, #30222, #40533 ),
 .UNSPECIFIED., .F., .F. ) 
 B_SPLINE_CURVE_WITH_KNOTS ( ( 3, 2, 2, 3 ),
 ( 0.4589552238805971740, 0.4601990049751245593, 0.4614427860696518890, 0.4626865671641792743 ),
 .UNSPECIFIED. ) 
 CURVE ( )  GEOMETRIC_REPRESENTATION_ITEM ( )  RATIONAL_B_SPLINE_CURVE ( ( 0.9999999999999820144, 0.8660254037844566932, 1.000000000000000000, 0.8660254037844387076, 1.000000000000000000, 0.8660254037844207220, 1.000000000000017986 ) ) 
 REPRESENTATION_ITEM ( '' )  );
#7839 = CARTESIAN_POINT ( 'NONE',  ( 5.000000000000000000, 8.660254037844385522, -148.7500000000000000 ) ) ;
#7840 = CARTESIAN_POINT ( 'NONE',  ( -10.81189881249999729, 1.324075727343319199E-15, -42.78125000204838102 ) ) ;
#7841 = CARTESIAN_POINT ( 'NONE',  ( -5.000000000000003553, -8.660254037844383745, -40.37500000409677625 ) ) ;
#7842 = CARTESIAN_POINT ( 'NONE',  ( 10.81189881249999907, 6.242252689847868297, -151.4062500020484094 ) ) ;
#7843 = CARTESIAN_POINT ( 'NONE',  ( -10.81189881249999729, 6.242252689847871849, -126.7187500020483952 ) ) ;
#7844 = DIRECTION ( 'NONE',  ( -0.000000000000000000, -0.000000000000000000, -1.000000000000000000 ) ) ;
#7845 = ORIENTED_EDGE ( 'NONE', *, *, #35988, .F. ) ;
#7846 = CARTESIAN_POINT ( 'NONE',  ( 7.070501591499376803E-16, 11.54700538379251284, -31.62499999999995737 ) ) ;
#7847 = ORIENTED_EDGE ( 'NONE', *, *, #40405, .T. ) ;
#7848 = VERTEX_POINT ( 'NONE', #9182 ) ;
#7850 = ORIENTED_EDGE ( 'NONE', *, *, #11814, .T. ) ;
#7849 = CARTESIAN_POINT ( 'NONE',  ( 7.644554776091147741E-16, 12.48450537969573659, -111.9687500020483952 ) ) ;
#7851 = CARTESIAN_POINT ( 'NONE',  ( 9.999999999999998224, 0.000000000000000000, -41.37500000409677625 ) ) ;
#7852 = CARTESIAN_POINT ( 'NONE',  ( 7.644554776091147741E-16, 12.48450537969573659, -186.9687500020483810 ) ) ;
#7853 = CARTESIAN_POINT ( 'NONE',  ( -2.293366432827344421E-15, -12.48450537969573659, -40.71875000204835260 ) ) ;
#7854 = CARTESIAN_POINT ( 'NONE',  ( -9.999999999999998224, 1.224646799147353059E-15, -153.1250000040967905 ) ) ;
#7855 = CARTESIAN_POINT ( 'NONE',  ( 0.000000000000000000, 0.000000000000000000, -200.0000000000000000 ) ) ;
#7856 = CARTESIAN_POINT ( 'NONE',  ( -10.81189881249999729, -6.242252689847864744, -175.9687500020483526 ) ) ;
#7857 = CARTESIAN_POINT ( 'NONE',  ( 10.81189881249999551, -6.242252689847874514, -164.9687500020484094 ) ) ;
#7858 = CARTESIAN_POINT ( 'NONE',  ( -5.000000000000003553, -8.660254037844383745, -25.37500000409675849 ) ) ;
#7859 = CARTESIAN_POINT ( 'NONE',  ( 10.81189881249999551, -6.242252689847874514, -145.4687500020483810 ) ) ;
#7860 = CARTESIAN_POINT ( 'NONE',  ( 10.81189881249999729, 0.000000000000000000, -151.5312500020484094 ) ) ;
#7861 = CARTESIAN_POINT ( 'NONE',  ( -10.81189881249999729, 1.324075727343319199E-15, -152.0937500020483810 ) ) ;
#7862 = CARTESIAN_POINT ( 'NONE',  ( 4.999999999999992006, -8.660254037844389075, -42.74999999999998579 ) ) ;
#7863 = DIRECTION ( 'NONE',  ( -0.000000000000000000, -0.000000000000000000, -1.000000000000000000 ) ) ;
#7864 = CARTESIAN_POINT ( 'NONE',  ( -9.999999999999998224, 1.224646799147353059E-15, -179.7500000000000284 ) ) ;
#7865 = CARTESIAN_POINT ( 'NONE',  ( -5.405949406250003975, -9.363379034771801557, -85.84375000204836681 ) ) ;
#7866 = LINE ( 'NONE', #34626, #3124 ) ;
#7867 = CARTESIAN_POINT ( 'NONE',  ( -10.81189881249999729, 6.242252689847871849, -57.90625000204838813 ) ) ;
#7868 = CARTESIAN_POINT ( 'NONE',  ( 9.999999999999998224, 0.000000000000000000, -87.87500000409677625 ) ) ;
#7869 = CARTESIAN_POINT ( 'NONE',  ( 10.81189881249999729, 0.000000000000000000, -179.8437500020483810 ) ) ;
#7870 = CARTESIAN_POINT ( 'NONE',  ( -5.405949406249996869, 9.363379034771805109, -116.5312500020483952 ) ) ;
#7871 = CARTESIAN_POINT ( 'NONE',  ( 10.81189881249999729, 6.242252689847867408, -154.4062500020483810 ) ) ;
#7872 = FACE_OUTER_BOUND ( 'NONE', #13813, .T. ) ;
#7873 = CARTESIAN_POINT ( 'NONE',  ( 5.405949406249999534, 9.363379034771803333, -47.78125000204838813 ) ) ;
#7874 = CARTESIAN_POINT ( 'NONE',  ( 9.999999999999998224, 0.000000000000000000, -126.8750000040967905 ) ) ;
#7875 = CARTESIAN_POINT ( 'NONE',  ( -9.999999999999998224, 5.773502691896259087, -106.3749999999999858 ) ) ;
#7876 =( BOUNDED_CURVE ( )  B_SPLINE_CURVE ( 2, ( #37147, #27228, #709, #17928, #36941, #34150, #31126 ),
 .UNSPECIFIED., .F., .F. ) 
 B_SPLINE_CURVE_WITH_KNOTS ( ( 3, 2, 2, 3 ),
 ( 0.1791044776119403437, 0.1803482587064677289, 0.1815920398009950587, 0.1828358208955224162 ),
 .UNSPECIFIED. ) 
 CURVE ( )  GEOMETRIC_REPRESENTATION_ITEM ( )  RATIONAL_B_SPLINE_CURVE ( ( 0.9999999999999940048, 0.8660254037844447028, 1.000000000000000000, 0.8660254037844387076, 1.000000000000000000, 0.8660254037844357100, 1.000000000000003109 ) ) 
 REPRESENTATION_ITEM ( '' )  );
#7877 = ORIENTED_EDGE ( 'NONE', *, *, #631, .F. ) ;
#7878 = CARTESIAN_POINT ( 'NONE',  ( -10.81189881249999729, 6.242252689847871849, -125.4062500020483810 ) ) ;
#7879 = CARTESIAN_POINT ( 'NONE',  ( -5.000000000000003553, -8.660254037844383745, -145.3750000040967905 ) ) ;
#7880 = CARTESIAN_POINT ( 'NONE',  ( 10.81189881249999907, 6.242252689847868297, -178.4062500020484094 ) ) ;
#7881 = VERTEX_POINT ( 'NONE', #28202 ) ;
#7882 = CARTESIAN_POINT ( 'NONE',  ( -10.00000000000000000, -5.773502691896251982, -52.12499999999997158 ) ) ;
#7883 = CARTESIAN_POINT ( 'NONE',  ( -5.405949406249996869, 9.363379034771805109, -170.3437500020484094 ) ) ;
#7884 = CARTESIAN_POINT ( 'NONE',  ( 10.00000000000000000, 5.773502691896255534, -56.25000000409676915 ) ) ;
#7885 = DIRECTION ( 'NONE',  ( -0.000000000000000000, -0.000000000000000000, 1.000000000000000000 ) ) ;
#7886 = CARTESIAN_POINT ( 'NONE',  ( 9.999999999999998224, 0.000000000000000000, -67.99999999999997158 ) ) ;
#7887 = CARTESIAN_POINT ( 'NONE',  ( -2.293366432827344421E-15, -12.48450537969573659, -72.40625000204836681 ) ) ;
#7888 = CARTESIAN_POINT ( 'NONE',  ( 5.405949406249999534, 9.363379034771803333, -47.78125000204838813 ) ) ;
#7889 = ADVANCED_FACE ( 'NONE', ( #21711 ), #35529, .F. ) ;
#7890 = CARTESIAN_POINT ( 'NONE',  ( 7.070501591499377789E-16, 11.54700538379251284, -50.00000000409676204 ) ) ;
#7891 = CARTESIAN_POINT ( 'NONE',  ( -10.81189881249999907, -6.242252689847864744, -7.968750002048358816 ) ) ;
#7892 = CARTESIAN_POINT ( 'NONE',  ( 5.000000000000000000, 8.660254037844385522, -158.1250000040967905 ) ) ;
#7893 = CARTESIAN_POINT ( 'NONE',  ( 10.81189881249999907, 6.242252689847868297, -178.4062500020484094 ) ) ;
#7894 = CARTESIAN_POINT ( 'NONE',  ( -10.81189881249999729, 1.324075727343319199E-15, -8.281250002048350822 ) ) ;
#7895 = CARTESIAN_POINT ( 'NONE',  ( -9.999999999998969713, -5.773502691896847949, -88.12499999999995737 ) ) ;
#7896 = FACE_OUTER_BOUND ( 'NONE', #37238, .T. ) ;
#7897 = LINE ( 'NONE', #14336, #25641 ) ;
#7898 = DIRECTION ( 'NONE',  ( -0.000000000000000000, -0.000000000000000000, 1.000000000000000000 ) ) ;
#7900 = ORIENTED_EDGE ( 'NONE', *, *, #23193, .F. ) ;
#7899 = CARTESIAN_POINT ( 'NONE',  ( 7.644554776091147741E-16, 12.48450537969573659, -82.15625000204838102 ) ) ;
#7901 = CARTESIAN_POINT ( 'NONE',  ( 9.999999999999998224, 0.000000000000000000, -141.8750000040967905 ) ) ;
#7903 = VERTEX_POINT ( 'NONE', #35738 ) ;
#7902 = DIRECTION ( 'NONE',  ( 0.000000000000000000, 0.000000000000000000, 1.000000000000000000 ) ) ;
#7904 = VERTEX_POINT ( 'NONE', #18469 ) ;
#7905 = CARTESIAN_POINT ( 'NONE',  ( 10.81189881249999729, 0.000000000000000000, -40.34375000204837391 ) ) ;
#7906 = CARTESIAN_POINT ( 'NONE',  ( 7.644554776091147741E-16, 12.48450537969573659, -29.46875000204835970 ) ) ;
#7907 = CARTESIAN_POINT ( 'NONE',  ( 10.81189881249999551, -6.242252689847874514, -12.15625000204835793 ) ) ;
#7908 = CARTESIAN_POINT ( 'NONE',  ( 10.81189881249999729, 0.000000000000000000, -61.34375000204836681 ) ) ;
#7909 = CARTESIAN_POINT ( 'NONE',  ( 9.999999999999479527, 5.773502691896553074, -93.37499999999997158 ) ) ;
#7910 = EDGE_CURVE ( 'NONE', #8336, #28565, #2307, .T. ) ;
#7911 = CARTESIAN_POINT ( 'NONE',  ( 4.999999999999992006, -8.660254037844389075, -42.74999999999998579 ) ) ;
#7912 = CARTESIAN_POINT ( 'NONE',  ( -5.405949406249996869, 9.363379034771805109, -185.3437500020483810 ) ) ;
#7913 = CARTESIAN_POINT ( 'NONE',  ( -2.293366432827344421E-15, -12.48450537969573659, -165.2187500020484094 ) ) ;
#7914 = CARTESIAN_POINT ( 'NONE',  ( -5.405949406249996869, 9.363379034771805109, -174.8437500020484094 ) ) ;
#7915 = CARTESIAN_POINT ( 'NONE',  ( 9.999999999999998224, 0.000000000000000000, -132.5000000000000000 ) ) ;
#7916 = DIRECTION ( 'NONE',  ( -0.000000000000000000, -0.000000000000000000, 1.000000000000000000 ) ) ;
#7917 = CARTESIAN_POINT ( 'NONE',  ( -5.000000000000003553, -8.660254037844383745, -104.4999999999999858 ) ) ;
#7918 = CARTESIAN_POINT ( 'NONE',  ( -5.000000000000003553, -8.660254037844383745, -89.87500000409677625 ) ) ;
#7919 = CARTESIAN_POINT ( 'NONE',  ( -5.405949406249996869, 9.363379034771805109, -111.8437500020483810 ) ) ;
#7920 = CYLINDRICAL_SURFACE ( 'NONE', #30768, 9.999999999999998224 ) ;
#7921 = CARTESIAN_POINT ( 'NONE',  ( -10.81189881249999907, -6.242252689847864744, -81.65625000204839523 ) ) ;
#7922 = CARTESIAN_POINT ( 'NONE',  ( -5.405949406250003975, -9.363379034771801557, -100.8437500020483810 ) ) ;
#7923 = CARTESIAN_POINT ( 'NONE',  ( -5.405949406250003975, -9.363379034771801557, -64.84375000204836681 ) ) ;
#7924 = CARTESIAN_POINT ( 'NONE',  ( 5.405949406249999534, 9.363379034771803333, -65.78125000204838102 ) ) ;
#7925 = CARTESIAN_POINT ( 'NONE',  ( -9.999999999999998224, 5.773502691896259087, -150.2500000040968189 ) ) ;
#7926 = CARTESIAN_POINT ( 'NONE',  ( 9.999999999999996447, -5.773502691896262640, -132.6249999999999716 ) ) ;
#7927 = CARTESIAN_POINT ( 'NONE',  ( 5.405949406249992428, -9.363379034771808662, -147.2812500020483810 ) ) ;
#7928 = CARTESIAN_POINT ( 'NONE',  ( 7.644554776091147741E-16, 12.48450537969573659, -173.6562500020483810 ) ) ;
#7929 = FACE_OUTER_BOUND ( 'NONE', #10994, .T. ) ;
#7930 = CARTESIAN_POINT ( 'NONE',  ( 9.999999999999998224, 0.000000000000000000, -182.0000000000000000 ) ) ;
#7931 = CARTESIAN_POINT ( 'NONE',  ( -2.293366432827344421E-15, -12.48450537969573659, -96.21875000204839523 ) ) ;
#7932 = CARTESIAN_POINT ( 'NONE',  ( -9.999999999999998224, 1.224646799147353059E-15, -155.7500000000000000 ) ) ;
#7933 = CARTESIAN_POINT ( 'NONE',  ( -9.999999999999998224, 5.773502691896259087, -73.37499999999997158 ) ) ;
#7934 = CARTESIAN_POINT ( 'NONE',  ( 10.81189881249999551, -6.242252689847874514, -6.156250002048363257 ) ) ;
#7935 = CARTESIAN_POINT ( 'NONE',  ( 10.00000000000000000, 5.773502691896255534, -84.75000000409677625 ) ) ;
#7936 = CARTESIAN_POINT ( 'NONE',  ( -10.00000000000076916, 5.773502691895813221, -115.3749999999999716 ) ) ;
#7937 = CARTESIAN_POINT ( 'NONE',  ( -10.81189881249999729, 6.242252689847871849, -96.90625000204838102 ) ) ;
#7938 = CARTESIAN_POINT ( 'NONE',  ( 10.81189881249999729, 0.000000000000000000, -79.53125000204838102 ) ) ;
#7939 = CARTESIAN_POINT ( 'NONE',  ( 7.070501591499377789E-16, 11.54700538379251284, -78.50000000409677625 ) ) ;
#7940 = CARTESIAN_POINT ( 'NONE',  ( 7.644554776091147741E-16, 12.48450537969573659, -35.46875000204835260 ) ) ;
#7941 = ORIENTED_EDGE ( 'NONE', *, *, #24908, .T. ) ;
#7942 = CARTESIAN_POINT ( 'NONE',  ( 7.070501591499377789E-16, 11.54700538379251284, -4.624999999999958256 ) ) ;
#7943 = CARTESIAN_POINT ( 'NONE',  ( 7.644554776091147741E-16, 12.48450537969573659, -31.15625000204835970 ) ) ;
#7944 = EDGE_CURVE ( 'NONE', #4606, #37408, #40570, .T. ) ;
#7945 = CARTESIAN_POINT ( 'NONE',  ( -10.81189881249999729, 1.324075727343319199E-15, -12.59375000204834905 ) ) ;
#7946 = CARTESIAN_POINT ( 'NONE',  ( 4.999999999999992006, -8.660254037844389075, -94.12500000409677625 ) ) ;
#7947 = CARTESIAN_POINT ( 'NONE',  ( 9.999999999999996447, -5.773502691896262640, -4.000000004096754047 ) ) ;
#7948 = CARTESIAN_POINT ( 'NONE',  ( -10.81189881249999729, 1.324075727343319199E-15, -126.7812500020483668 ) ) ;
#7949 = AXIS2_PLACEMENT_3D ( 'NONE', #5978, #28860, #19129 ) ;
#7950 = CARTESIAN_POINT ( 'NONE',  ( 10.00000000000000000, 5.773502691896255534, -178.8750000000000000 ) ) ;
#7951 = CARTESIAN_POINT ( 'NONE',  ( -10.00000000000051337, 5.773502691895962435, -119.8749999999999858 ) ) ;
#7953 = ORIENTED_EDGE ( 'NONE', *, *, #40732, .F. ) ;
#7952 = CARTESIAN_POINT ( 'NONE',  ( -10.81189881249999729, 1.324075727343319199E-15, -107.2812500020483810 ) ) ;
#7954 = CARTESIAN_POINT ( 'NONE',  ( 9.999999999999998224, 0.000000000000000000, -153.8750000040967905 ) ) ;
#7955 = ORIENTED_EDGE ( 'NONE', *, *, #9727, .T. ) ;
#7956 = ORIENTED_EDGE ( 'NONE', *, *, #32021, .T. ) ;
#7957 = CARTESIAN_POINT ( 'NONE',  ( -2.293366432827344421E-15, -12.48450537969573659, -37.90625000204836681 ) ) ;
#7958 = PERSON_AND_ORGANIZATION ( #11915, #17965 ) ;
#7959 = CARTESIAN_POINT ( 'NONE',  ( 5.405949406249992428, -9.363379034771808662, -85.59375000204836681 ) ) ;
#7960 = DIRECTION ( 'NONE',  ( 1.000000000000000000, 0.000000000000000000, 0.000000000000000000 ) ) ;
#7961 = DIRECTION ( 'NONE',  ( -0.000000000000000000, -0.000000000000000000, 1.000000000000000000 ) ) ;
#7962 =( BOUNDED_CURVE ( )  B_SPLINE_CURVE ( 2, ( #11101, #24304, #37448, #5288, #22327, #2483, #41308 ),
 .UNSPECIFIED., .F., .F. ) 
 B_SPLINE_CURVE_WITH_KNOTS ( ( 3, 2, 2, 3 ),
 ( 0.3171641791044778058, 0.3184079601990050801, 0.3196517412935324653, 0.3208955223880597396 ),
 .UNSPECIFIED. ) 
 CURVE ( )  GEOMETRIC_REPRESENTATION_ITEM ( )  RATIONAL_B_SPLINE_CURVE ( ( 0.9999999999999820144, 0.8660254037844566932, 1.000000000000000000, 0.8660254037844387076, 1.000000000000000000, 0.8660254037844327124, 1.000000000000005995 ) ) 
 REPRESENTATION_ITEM ( '' )  );
#7963 = AXIS2_PLACEMENT_3D ( 'NONE', #12408, #35741, #42608 ) ;
#7964 = CARTESIAN_POINT ( 'NONE',  ( -4.999999999999996447, 8.660254037844387298, -105.3750000040967763 ) ) ;
#7965 = CARTESIAN_POINT ( 'NONE',  ( -2.293366432827344421E-15, -12.48450537969573659, -160.9062500020483810 ) ) ;
#7966 = CARTESIAN_POINT ( 'NONE',  ( -10.81189881249999729, -6.242252689847864744, -127.9687500020483810 ) ) ;
#7967 = CARTESIAN_POINT ( 'NONE',  ( -2.293366432827344421E-15, -12.48450537969573659, -93.21875000204838102 ) ) ;
#7968 = CARTESIAN_POINT ( 'NONE',  ( 5.405949406249992428, -9.363379034771808662, -1.781250002048373471 ) ) ;
#7969 = CARTESIAN_POINT ( 'NONE',  ( -10.81189881249999729, 6.242252689847871849, -194.2187500020483810 ) ) ;
#7970 = CARTESIAN_POINT ( 'NONE',  ( -2.293366432827344421E-15, -12.48450537969573659, -102.4062500020483952 ) ) ;
#7971 = CARTESIAN_POINT ( 'NONE',  ( -9.999999999999998224, 1.224646799147353059E-15, -181.6250000040967905 ) ) ;
#7972 = CARTESIAN_POINT ( 'NONE',  ( 5.405949406249999534, 9.363379034771803333, -107.5937500020483810 ) ) ;
#7973 = CARTESIAN_POINT ( 'NONE',  ( -10.81189881249999729, 1.324075727343319199E-15, -180.7812500020484094 ) ) ;
#7974 = FACE_OUTER_BOUND ( 'NONE', #12536, .T. ) ;
#7975 = CARTESIAN_POINT ( 'NONE',  ( -10.81189881249999907, -6.242252689847864744, -197.1562500020484379 ) ) ;
#7976 = CARTESIAN_POINT ( 'NONE',  ( -10.81189881249999729, -6.242252689847864744, -48.46875000204837391 ) ) ;
#7977 = CARTESIAN_POINT ( 'NONE',  ( -4.999999999999996447, 8.660254037844387298, -171.3750000040968189 ) ) ;
#7978 = CARTESIAN_POINT ( 'NONE',  ( -5.405949406250003975, -9.363379034771801557, -6.531250002048377468 ) ) ;
#7979 = CARTESIAN_POINT ( 'NONE',  ( -2.293366432827344421E-15, -12.48450537969573659, -22.71875000204837391 ) ) ;
#7980 = CARTESIAN_POINT ( 'NONE',  ( -10.00000000000102496, 5.773502691895664007, -53.87499999999993605 ) ) ;
#7981 = CARTESIAN_POINT ( 'NONE',  ( -10.81189881249999907, -6.242252689847864744, -130.9687500020483810 ) ) ;
#7982 = CARTESIAN_POINT ( 'NONE',  ( 9.999999999999998224, 0.000000000000000000, -94.99999999999998579 ) ) ;
#7983 = CARTESIAN_POINT ( 'NONE',  ( 7.644554776091147741E-16, 12.48450537969573659, -31.15625000204835970 ) ) ;
#7984 = CARTESIAN_POINT ( 'NONE',  ( 7.070501591499377789E-16, 11.54700538379251284, -105.5000000040967763 ) ) ;
#7985 = CARTESIAN_POINT ( 'NONE',  ( 9.999999999999998224, 0.000000000000000000, -26.37500000409676204 ) ) ;
#7986 = CARTESIAN_POINT ( 'NONE',  ( -10.00000000000000000, -5.773502691896251982, -50.62499999999997158 ) ) ;
#7987 = CARTESIAN_POINT ( 'NONE',  ( -5.405949406250003975, -9.363379034771801557, -125.0312500020483952 ) ) ;
#7988 = CARTESIAN_POINT ( 'NONE',  ( -10.81189881249999729, 1.324075727343319199E-15, -98.28125000204839523 ) ) ;
#7989 = ORIENTED_EDGE ( 'NONE', *, *, #6218, .F. ) ;
#7990 = CARTESIAN_POINT ( 'NONE',  ( 9.999999999999996447, -5.773502691896262640, -103.0000000040967620 ) ) ;
#7991 = CARTESIAN_POINT ( 'NONE',  ( -10.81189881249999729, 1.324075727343319199E-15, -161.2812500020484094 ) ) ;
#7992 = CARTESIAN_POINT ( 'NONE',  ( 5.405949406249999534, 9.363379034771803333, -55.09375000204835970 ) ) ;
#7993 = ORIENTED_EDGE ( 'NONE', *, *, #18445, .F. ) ;
#7994 = CARTESIAN_POINT ( 'NONE',  ( -4.999999999999996447, 8.660254037844387298, -26.99999999999996803 ) ) ;
#7995 = EDGE_CURVE ( 'NONE', #8341, #32539, #25184, .T. ) ;
#7996 = CARTESIAN_POINT ( 'NONE',  ( -5.405949406249996869, 9.363379034771805109, -32.53125000204837391 ) ) ;
#7997 = CARTESIAN_POINT ( 'NONE',  ( 4.999999999999992006, -8.660254037844389075, -158.2500000000000000 ) ) ;
#7998 = CARTESIAN_POINT ( 'NONE',  ( -9.999999999999998224, 1.224646799147353059E-15, -177.1250000040968189 ) ) ;
#7999 = CARTESIAN_POINT ( 'NONE',  ( -9.999999999999998224, 5.773502691896259087, -24.25000000409677270 ) ) ;
#8000 = EDGE_CURVE ( 'NONE', #41312, #25900, #9706, .T. ) ;
#8001 = AXIS2_PLACEMENT_3D ( 'NONE', #42000, #2539, #35342 ) ;
#8002 =( BOUNDED_CURVE ( )  B_SPLINE_CURVE ( 2, ( #28240, #25014, #4705, #30832, #4495, #17638, #37728 ),
 .UNSPECIFIED., .F., .F. ) 
 B_SPLINE_CURVE_WITH_KNOTS ( ( 3, 2, 2, 3 ),
 ( 0.2985074626865671932, 0.2997512437810946340, 0.3009950248756220192, 0.3022388059701494045 ),
 .UNSPECIFIED. ) 
 CURVE ( )  GEOMETRIC_REPRESENTATION_ITEM ( )  RATIONAL_B_SPLINE_CURVE ( ( 0.9999999999999940048, 0.8660254037844447028, 1.000000000000000000, 0.8660254037844387076, 1.000000000000000000, 0.8660254037844207220, 1.000000000000017986 ) ) 
 REPRESENTATION_ITEM ( '' )  );
#8003 = EDGE_CURVE ( 'NONE', #14981, #15576, #2514, .T. ) ;
#8004 = CARTESIAN_POINT ( 'NONE',  ( 5.405949406249999534, 9.363379034771803333, -133.2812500020483810 ) ) ;
#8005 = CARTESIAN_POINT ( 'NONE',  ( -4.999999999999996447, 8.660254037844387298, -139.8750000040968189 ) ) ;
#8006 = CIRCLE ( 'NONE', #13489, 22.00000000000000711 ) ;
#8007 = CARTESIAN_POINT ( 'NONE',  ( 5.000000000000000000, 8.660254037844385522, -162.6250000040967905 ) ) ;
#8008 = EDGE_LOOP ( 'NONE', ( #41565, #5511, #29074, #28291 ) ) ;
#8009 =( BOUNDED_CURVE ( )  B_SPLINE_CURVE ( 2, ( #6401, #16288, #2952, #6600, #32726, #15660, #32523 ),
 .UNSPECIFIED., .F., .F. ) 
 B_SPLINE_CURVE_WITH_KNOTS ( ( 3, 2, 2, 3 ),
 ( 0.1902985074626866169, 0.1915422885572139744, 0.1927860696517413319, 0.1940298507462686894 ),
 .UNSPECIFIED. ) 
 CURVE ( )  GEOMETRIC_REPRESENTATION_ITEM ( )  RATIONAL_B_SPLINE_CURVE ( ( 0.9999999999999940048, 0.8660254037844447028, 1.000000000000000000, 0.8660254037844387076, 1.000000000000000000, 0.8660254037844357100, 1.000000000000003109 ) ) 
 REPRESENTATION_ITEM ( '' )  );
#8010 = CARTESIAN_POINT ( 'NONE',  ( -5.405949406249996869, 9.363379034771805109, -59.53125000204836681 ) ) ;
#8012 = ORIENTED_EDGE ( 'NONE', *, *, #9538, .F. ) ;
#8011 = EDGE_LOOP ( 'NONE', ( #41801, #17586, #10572, #2294 ) ) ;
#8013 = ADVANCED_FACE ( 'NONE', ( #123 ), #6577, .T. ) ;
#8014 = FACE_OUTER_BOUND ( 'NONE', #41321, .T. ) ;
#8015 = CARTESIAN_POINT ( 'NONE',  ( -9.999999999999998224, 1.224646799147353059E-15, -174.1250000040968189 ) ) ;
#8016 = CARTESIAN_POINT ( 'NONE',  ( -2.293366432827344421E-15, -12.48450537969573659, -165.2187500020484094 ) ) ;
#8017 =( BOUNDED_CURVE ( )  B_SPLINE_CURVE ( 2, ( #18346, #1962, #2178, #26834, #38202, #8647, #21802 ),
 .UNSPECIFIED., .F., .F. ) 
 B_SPLINE_CURVE_WITH_KNOTS ( ( 3, 2, 2, 3 ),
 ( 0.5858208955223881409, 0.5870646766169155262, 0.5883084577114429115, 0.5895522388059702967 ),
 .UNSPECIFIED. ) 
 CURVE ( )  GEOMETRIC_REPRESENTATION_ITEM ( )  RATIONAL_B_SPLINE_CURVE ( ( 0.9999999999999880096, 0.8660254037844506980, 1.000000000000000000, 0.8660254037844387076, 1.000000000000000000, 0.8660254037844267172, 1.000000000000011990 ) ) 
 REPRESENTATION_ITEM ( '' )  );
#8018 = ADVANCED_FACE ( 'NONE', ( #30106 ), #42394, .F. ) ;
#8019 = CARTESIAN_POINT ( 'NONE',  ( -5.405949406249996869, 9.363379034771805109, -193.0312500020484094 ) ) ;
#8020 = CARTESIAN_POINT ( 'NONE',  ( 10.81189881249999729, 0.000000000000000000, -11.84375000204834727 ) ) ;
#8021 = ADVANCED_FACE ( 'NONE', ( #331 ), #29463, .F. ) ;
#8022 = CARTESIAN_POINT ( 'NONE',  ( -5.405949406249996869, 9.363379034771805109, -144.8437500020483810 ) ) ;
#8023 = CARTESIAN_POINT ( 'NONE',  ( 7.644554776091147741E-16, 12.48450537969573659, -132.9687500020483810 ) ) ;
#8024 = CARTESIAN_POINT ( 'NONE',  ( -10.81189881249999729, 1.324075727343319199E-15, -108.7812500020483810 ) ) ;
#8025 = CARTESIAN_POINT ( 'NONE',  ( -2.293366432827344421E-15, -12.48450537969573659, -114.2187500020483668 ) ) ;
#8026 = CARTESIAN_POINT ( 'NONE',  ( -10.81189881249999907, -6.242252689847864744, -0.4687500020483514329 ) ) ;
#8027 = CARTESIAN_POINT ( 'NONE',  ( 5.405949406249999534, 9.363379034771803333, -125.7812500020483668 ) ) ;
#8028 = CARTESIAN_POINT ( 'NONE',  ( 10.81189881249999729, 0.000000000000000000, 0.1562499979516351889 ) ) ;
#8029 = CARTESIAN_POINT ( 'NONE',  ( 5.405949406249992428, -9.363379034771808662, -132.0937500020483810 ) ) ;
#8030 = CARTESIAN_POINT ( 'NONE',  ( -2.121150477449813534E-15, -11.54700538379251284, -166.2500000040968189 ) ) ;
#8031 = CARTESIAN_POINT ( 'NONE',  ( 9.999999999999998224, 0.000000000000000000, -110.3750000040967763 ) ) ;
#8032 = CARTESIAN_POINT ( 'NONE',  ( -2.121150477449813534E-15, -11.54700538379251284, -147.8750000000000000 ) ) ;
#8033 = CARTESIAN_POINT ( 'NONE',  ( -4.999999999999996447, 8.660254037844387298, -23.99999999999996447 ) ) ;
#8034 = CARTESIAN_POINT ( 'NONE',  ( 5.405949406249999534, 9.363379034771803333, -73.09375000204838102 ) ) ;
#8035 = CARTESIAN_POINT ( 'NONE',  ( -5.405949406249996869, 9.363379034771805109, -68.34375000204836681 ) ) ;
#8036 = CARTESIAN_POINT ( 'NONE',  ( -9.999999999999998224, 1.224646799147353059E-15, -76.24999999999998579 ) ) ;
#8037 = CARTESIAN_POINT ( 'NONE',  ( -10.81189881249999729, 6.242252689847871849, -33.90625000204836681 ) ) ;
#8038 = CARTESIAN_POINT ( 'NONE',  ( 7.644554776091147741E-16, 12.48450537969573659, -48.96875000204836681 ) ) ;
#8039 = DIRECTION ( 'NONE',  ( 0.000000000000000000, 0.000000000000000000, -1.000000000000000000 ) ) ;
#8040 = CARTESIAN_POINT ( 'NONE',  ( 7.644554776091147741E-16, 12.48450537969573659, -155.4687500020484094 ) ) ;
#8041 = CARTESIAN_POINT ( 'NONE',  ( -5.000000000000003553, -8.660254037844383745, -125.5000000000000000 ) ) ;
#8042 = CARTESIAN_POINT ( 'NONE',  ( -10.81189881249999729, -6.242252689847864744, -132.6562500020483810 ) ) ;
#8043 = CARTESIAN_POINT ( 'NONE',  ( -1.048820568758768168, 10.15334972493218757, -180.0000000000000000 ) ) ;
#8044 = CARTESIAN_POINT ( 'NONE',  ( 9.999999999999998224, 0.000000000000000000, -76.99999999999998579 ) ) ;
#8045 = CARTESIAN_POINT ( 'NONE',  ( 7.644554776091147741E-16, 12.48450537969573659, -22.15625000204837391 ) ) ;
#8046 = ORIENTED_EDGE ( 'NONE', *, *, #22874, .T. ) ;
#8047 = CARTESIAN_POINT ( 'NONE',  ( 5.405949406249999534, 9.363379034771803333, -101.7812500020483952 ) ) ;
#8048 = CARTESIAN_POINT ( 'NONE',  ( 9.999999999999996447, -5.773502691896262640, -124.0000000040967763 ) ) ;
#8049 = CARTESIAN_POINT ( 'NONE',  ( 7.070501591499377789E-16, 11.54700538379251284, -36.50000000409675494 ) ) ;
#8050 = PRODUCT_DEFINITION_SHAPE ( 'NONE', 'NONE',  #24384 ) ;
#8051 = CARTESIAN_POINT ( 'NONE',  ( -9.999999999999998224, 1.224646799147353059E-15, -130.2499999999999716 ) ) ;
#8052 = CARTESIAN_POINT ( 'NONE',  ( -5.405949406250003975, -9.363379034771801557, -45.53125000204838102 ) ) ;
#8053 = EDGE_CURVE ( 'NONE', #33176, #36280, #5313, .T. ) ;
#8054 = CARTESIAN_POINT ( 'NONE',  ( -9.999999999999834799, -5.773502691896343464, -191.6250000000000000 ) ) ;
#8055 = CARTESIAN_POINT ( 'NONE',  ( -5.405949406250003975, -9.363379034771801557, -152.0312500020484094 ) ) ;
#8056 = CARTESIAN_POINT ( 'NONE',  ( 10.81189881249999907, 6.242252689847868297, -130.2187500020483810 ) ) ;
#8057 = CARTESIAN_POINT ( 'NONE',  ( 9.999999999999998224, 0.000000000000000000, -109.9999999999999858 ) ) ;
#8058 = EDGE_LOOP ( 'NONE', ( #5118, #16560, #17375, #27245 ) ) ;
#8059 = DIRECTION ( 'NONE',  ( 1.000000000000000000, 0.000000000000000000, 0.000000000000000000 ) ) ;
#8060 = ORIENTED_EDGE ( 'NONE', *, *, #25451, .T. ) ;
#8061 = ORIENTED_EDGE ( 'NONE', *, *, #23971, .F. ) ;
#8062 = EDGE_LOOP ( 'NONE', ( #26932, #21159, #427, #37434 ) ) ;
#8063 = EDGE_CURVE ( 'NONE', #34185, #17371, #21311, .T. ) ;
#8064 = CARTESIAN_POINT ( 'NONE',  ( -9.999999999999998224, 1.224646799147353059E-15, -42.12500000409677625 ) ) ;
#8065 = CARTESIAN_POINT ( 'NONE',  ( -10.81189881249999907, -6.242252689847864744, -187.9687500020484094 ) ) ;
#8066 = CARTESIAN_POINT ( 'NONE',  ( 10.81189881249999907, 6.242252689847868297, -37.21875000204835970 ) ) ;
#8067 = CARTESIAN_POINT ( 'NONE',  ( 5.000000000000000000, 8.660254037844385522, -153.6250000040967905 ) ) ;
#8068 = CARTESIAN_POINT ( 'NONE',  ( -5.405949406250003975, -9.363379034771801557, -175.8437500020483810 ) ) ;
#8069 = CARTESIAN_POINT ( 'NONE',  ( 10.81189881249999907, 6.242252689847868297, -160.2187500020483810 ) ) ;
#8070 = DIRECTION ( 'NONE',  ( 1.000000000000000000, 0.000000000000000000, 0.000000000000000000 ) ) ;
#8071 = CARTESIAN_POINT ( 'NONE',  ( -5.405949406249996869, 9.363379034771805109, -143.3437500020483810 ) ) ;
#8072 = CARTESIAN_POINT ( 'NONE',  ( 5.405949406249992428, -9.363379034771808662, -145.7812500020483810 ) ) ;
#8073 = CARTESIAN_POINT ( 'NONE',  ( -5.405949406250003975, -9.363379034771801557, -151.8437500020483810 ) ) ;
#8074 = CARTESIAN_POINT ( 'NONE',  ( 7.070501591499376803E-16, 11.54700538379251284, -134.0000000040967905 ) ) ;
#8075 = CARTESIAN_POINT ( 'NONE',  ( -9.999999999999998224, 1.224646799147353059E-15, -66.12500000409676204 ) ) ;
#8076 = CARTESIAN_POINT ( 'NONE',  ( -9.999999999999998224, 1.224646799147353059E-15, -169.2500000000000000 ) ) ;
#8077 = CARTESIAN_POINT ( 'NONE',  ( -2.293366432827344421E-15, -12.48450537969573659, -90.21875000204838102 ) ) ;
#8078 = CARTESIAN_POINT ( 'NONE',  ( 9.999999999999998224, 0.000000000000000000, -103.9999999999999858 ) ) ;
#8079 = CARTESIAN_POINT ( 'NONE',  ( 5.405949406249999534, 9.363379034771803333, -58.28125000204836681 ) ) ;
#8080 = DIRECTION ( 'NONE',  ( -0.000000000000000000, -0.000000000000000000, -1.000000000000000000 ) ) ;
#8081 = CARTESIAN_POINT ( 'NONE',  ( 10.81189881249999907, 6.242252689847868297, -176.7187500020483810 ) ) ;
#8082 = CARTESIAN_POINT ( 'NONE',  ( -10.81189881249999907, -6.242252689847864744, -116.1562500020483952 ) ) ;
#8083 = CARTESIAN_POINT ( 'NONE',  ( 5.405949406249992428, -9.363379034771808662, -153.2812500020484094 ) ) ;
#8084 =( BOUNDED_CURVE ( )  B_SPLINE_CURVE ( 2, ( #19008, #29157, #22675, #9290, #25712, #29574, #19 ),
 .UNSPECIFIED., .F., .F. ) 
 B_SPLINE_CURVE_WITH_KNOTS ( ( 3, 2, 2, 3 ),
 ( 0.7574626865671643117, 0.7587064676616916969, 0.7599502487562190822, 0.7611940298507464675 ),
 .UNSPECIFIED. ) 
 CURVE ( )  GEOMETRIC_REPRESENTATION_ITEM ( )  RATIONAL_B_SPLINE_CURVE ( ( 0.9999999999999880096, 0.8660254037844506980, 1.000000000000000000, 0.8660254037844387076, 1.000000000000000000, 0.8660254037844148378, 1.000000000000023981 ) ) 
 REPRESENTATION_ITEM ( '' )  );
#8085 = DIRECTION ( 'NONE',  ( -1.000000000000000000, 0.000000000000000000, 0.000000000000000000 ) ) ;
#8086 = CARTESIAN_POINT ( 'NONE',  ( 10.81189881249999729, 0.000000000000000000, -48.03125000204838813 ) ) ;
#8087 = CARTESIAN_POINT ( 'NONE',  ( -4.999999999999996447, 8.660254037844387298, -127.8750000040967905 ) ) ;
#8088 = CARTESIAN_POINT ( 'NONE',  ( 9.999999999999996447, -5.773502691896262640, -105.6249999999999858 ) ) ;
#8089 = ORIENTED_EDGE ( 'NONE', *, *, #34117, .T. ) ;
#8090 = CARTESIAN_POINT ( 'NONE',  ( 10.81189881249999729, 0.000000000000000000, -127.5312500020483952 ) ) ;
#8091 = CARTESIAN_POINT ( 'NONE',  ( 10.00000000000000000, 5.773502691896255534, -146.2500000040967905 ) ) ;
#8092 = CARTESIAN_POINT ( 'NONE',  ( 9.999999999998969713, 5.773502691896851502, -68.25000000409676204 ) ) ;
#8093 = CARTESIAN_POINT ( 'NONE',  ( -5.405949406250003975, -9.363379034771801557, -177.5312500020483810 ) ) ;
#8094 = ORIENTED_EDGE ( 'NONE', *, *, #32906, .F. ) ;
#8095 = CARTESIAN_POINT ( 'NONE',  ( -5.405949406249996869, 9.363379034771805109, -174.8437500020484094 ) ) ;
#8096 = CARTESIAN_POINT ( 'NONE',  ( 9.999999999999996447, -5.773502691896262640, -58.00000000409676915 ) ) ;
#8097 = CARTESIAN_POINT ( 'NONE',  ( -9.999999999999998224, 1.224646799147353059E-15, -97.24999999999998579 ) ) ;
#8098 = CARTESIAN_POINT ( 'NONE',  ( 5.000000000000000000, 8.660254037844385522, -135.6250000040967620 ) ) ;
#8099 = CARTESIAN_POINT ( 'NONE',  ( 5.405949406249992428, -9.363379034771808662, -72.28125000204838102 ) ) ;
#8100 = CARTESIAN_POINT ( 'NONE',  ( -5.405949406249996869, 9.363379034771805109, -55.03125000204836681 ) ) ;
#8101 = CARTESIAN_POINT ( 'NONE',  ( 9.999999999999998224, 0.000000000000000000, -42.87500000409677625 ) ) ;
#8102 = CARTESIAN_POINT ( 'NONE',  ( 10.81189881249999551, -6.242252689847874514, -2.968750002048353931 ) ) ;
#8103 = LINE ( 'NONE', #34011, #26925 ) ;
#8104 = CARTESIAN_POINT ( 'NONE',  ( -2.293366432827344421E-15, -12.48450537969573659, -180.4062500020484379 ) ) ;
#8105 = CARTESIAN_POINT ( 'NONE',  ( 9.999999999999998224, 0.000000000000000000, -128.0000000000000000 ) ) ;
#8106 = DIRECTION ( 'NONE',  ( 0.000000000000000000, 0.9961946980917455452, -0.08715574274765837404 ) ) ;
#8107 = ORIENTED_EDGE ( 'NONE', *, *, #37289, .T. ) ;
#8108 = CARTESIAN_POINT ( 'NONE',  ( -9.999999999999998224, 1.224646799147353059E-15, -154.2500000000000000 ) ) ;
#8109 = LINE ( 'NONE', #17577, #42420 ) ;
#8110 = DIRECTION ( 'NONE',  ( -0.000000000000000000, -0.000000000000000000, 1.000000000000000000 ) ) ;
#8111 = EDGE_CURVE ( 'NONE', #16149, #21857, #24098, .T. ) ;
#8113 = VERTEX_POINT ( 'NONE', #20161 ) ;
#8112 = CARTESIAN_POINT ( 'NONE',  ( -10.81189881249999729, 6.242252689847871849, -86.40625000204836681 ) ) ;
#8115 = ORIENTED_EDGE ( 'NONE', *, *, #23366, .F. ) ;
#8114 = LINE ( 'NONE', #31425, #41298 ) ;
#8116 = VERTEX_POINT ( 'NONE', #33351 ) ;
#8117 = CARTESIAN_POINT ( 'NONE',  ( -10.81189881249999729, 6.242252689847871849, -36.71875000204835970 ) ) ;
#8118 = CARTESIAN_POINT ( 'NONE',  ( -2.293366432827344421E-15, -12.48450537969573659, -30.21875000204834905 ) ) ;
#8119 = CARTESIAN_POINT ( 'NONE',  ( -5.405949406250003975, -9.363379034771801557, -11.03125000204835438 ) ) ;
#8121 = EDGE_LOOP ( 'NONE', ( #2733, #26895, #18228, #32065 ) ) ;
#8120 = CARTESIAN_POINT ( 'NONE',  ( 10.81189881249999551, -6.242252689847874514, -62.96875000204838813 ) ) ;
#8122 = DIRECTION ( 'NONE',  ( -0.000000000000000000, -0.000000000000000000, 1.000000000000000000 ) ) ;
#8123 = CARTESIAN_POINT ( 'NONE',  ( -10.00000000000000000, -5.773502691896251982, -40.12499999999996447 ) ) ;
#8124 = CARTESIAN_POINT ( 'NONE',  ( 10.81189881249999907, 6.242252689847868297, -188.7187500020484094 ) ) ;
#8125 = CARTESIAN_POINT ( 'NONE',  ( -10.81189881249999729, 1.324075727343319199E-15, -165.5937500020484094 ) ) ;
#8126 = EDGE_CURVE ( 'NONE', #22125, #15042, #6451, .T. ) ;
#8127 =( BOUNDED_CURVE ( )  B_SPLINE_CURVE ( 2, ( #8292, #11288, #37635, #8074, #33765, #30536, #1174 ),
 .UNSPECIFIED., .F., .F. ) 
 B_SPLINE_CURVE_WITH_KNOTS ( ( 3, 2, 2, 3 ),
 ( 0.3208955223880597396, 0.3221393034825871804, 0.3233830845771145657, 0.3246268656716419510 ),
 .UNSPECIFIED. ) 
 CURVE ( )  GEOMETRIC_REPRESENTATION_ITEM ( )  RATIONAL_B_SPLINE_CURVE ( ( 0.9999999999999940048, 0.8660254037844447028, 1.000000000000000000, 0.8660254037844387076, 1.000000000000000000, 0.8660254037844207220, 1.000000000000017986 ) ) 
 REPRESENTATION_ITEM ( '' )  );
#8128 = CARTESIAN_POINT ( 'NONE',  ( -4.999999999999996447, 8.660254037844387298, -43.49999999999998579 ) ) ;
#8129 = CARTESIAN_POINT ( 'NONE',  ( -5.000000000000003553, -8.660254037844383745, -193.0000000000000000 ) ) ;
#8130 = LINE ( 'NONE', #34254, #40512 ) ;
#8131 = CYLINDRICAL_SURFACE ( 'NONE', #27308, 9.999999999999998224 ) ;
#8132 = CARTESIAN_POINT ( 'NONE',  ( 4.999999999999992006, -8.660254037844389075, -89.62500000409677625 ) ) ;
#8133 = CARTESIAN_POINT ( 'NONE',  ( -10.81189881249999907, -6.242252689847864744, -114.4687500020483810 ) ) ;
#8134 = DIRECTION ( 'NONE',  ( 0.000000000000000000, 0.000000000000000000, 1.000000000000000000 ) ) ;
#8135 = VECTOR ( 'NONE', #34037, 1000.000000000000000 ) ;
#8136 = CARTESIAN_POINT ( 'NONE',  ( -10.81189881249999907, -6.242252689847864744, -83.15625000204836681 ) ) ;
#8137 = CARTESIAN_POINT ( 'NONE',  ( 10.81189881249999729, 6.242252689847867408, -97.21875000204838102 ) ) ;
#8138 = VECTOR ( 'NONE', #3618, 1000.000000000000000 ) ;
#8139 = CARTESIAN_POINT ( 'NONE',  ( 5.405949406249999534, 9.363379034771803333, -64.09375000204836681 ) ) ;
#8140 = CARTESIAN_POINT ( 'NONE',  ( -5.405949406249996869, 9.363379034771805109, -68.53125000204838102 ) ) ;
#8141 = CARTESIAN_POINT ( 'NONE',  ( -10.00000000000000000, -5.773502691896251982, -154.5000000040967905 ) ) ;
#8142 = CARTESIAN_POINT ( 'NONE',  ( 9.999999999999998224, 0.000000000000000000, -131.0000000000000000 ) ) ;
#8143 = CARTESIAN_POINT ( 'NONE',  ( 5.405949406249992428, -9.363379034771808662, -150.2812500020483810 ) ) ;
#8144 = CARTESIAN_POINT ( 'NONE',  ( 5.405949406249992428, -9.363379034771808662, -162.2812500020484094 ) ) ;
#8145 = CARTESIAN_POINT ( 'NONE',  ( -5.000000000000003553, -8.660254037844383745, -175.0000000000000284 ) ) ;
#8146 = CARTESIAN_POINT ( 'NONE',  ( 5.000000000000000000, 8.660254037844385522, -172.7500000000000284 ) ) ;
#8147 = CARTESIAN_POINT ( 'NONE',  ( -10.81189881249999907, -6.242252689847864744, -97.96875000204838102 ) ) ;
#8148 = CARTESIAN_POINT ( 'NONE',  ( 9.999999999999998224, 0.000000000000000000, -120.8750000040967905 ) ) ;
#8149 = CARTESIAN_POINT ( 'NONE',  ( 4.999999999999992006, -8.660254037844389075, -74.24999999999998579 ) ) ;
#8150 = CARTESIAN_POINT ( 'NONE',  ( -10.81189881249999907, -6.242252689847864744, -198.4687500020484379 ) ) ;
#8151 = CARTESIAN_POINT ( 'NONE',  ( -9.999999999999998224, 5.773502691896259087, -82.75000000409676204 ) ) ;
#8152 = CARTESIAN_POINT ( 'NONE',  ( 4.999999999999992006, -8.660254037844389075, -142.1250000040967905 ) ) ;
#8153 = CARTESIAN_POINT ( 'NONE',  ( -2.293366432827344421E-15, -12.48450537969573659, -93.40625000204839523 ) ) ;
#8154 = CARTESIAN_POINT ( 'NONE',  ( -10.81189881249999729, 6.242252689847871849, -77.40625000204838102 ) ) ;
#8155 = CARTESIAN_POINT ( 'NONE',  ( 10.00000000000000000, 5.773502691896255534, -66.75000000409677625 ) ) ;
#8156 = CARTESIAN_POINT ( 'NONE',  ( -9.999999999998456346, -5.773502691897145489, -59.62499999999995737 ) ) ;
#8157 = CARTESIAN_POINT ( 'NONE',  ( 5.405949406249999534, 9.363379034771803333, -26.59375000204835970 ) ) ;
#8158 = ORIENTED_EDGE ( 'NONE', *, *, #13702, .T. ) ;
#8159 = CARTESIAN_POINT ( 'NONE',  ( -4.999999999999996447, 8.660254037844387298, -4.499999999999976019 ) ) ;
#8160 = CARTESIAN_POINT ( 'NONE',  ( 10.81189881249999907, 6.242252689847868297, -28.40625000204838457 ) ) ;
#8161 = CARTESIAN_POINT ( 'NONE',  ( 5.405949406249992428, -9.363379034771808662, -16.59375000204835260 ) ) ;
#8162 = CARTESIAN_POINT ( 'NONE',  ( 0.000000000000000000, 0.000000000000000000, -170.0000000000000000 ) ) ;
#8163 = CARTESIAN_POINT ( 'NONE',  ( -9.999999999999998224, 1.224646799147353059E-15, -7.625000004096743389 ) ) ;
#8164 = FACE_OUTER_BOUND ( 'NONE', #20948, .T. ) ;
#8165 = CARTESIAN_POINT ( 'NONE',  ( 7.644554776091147741E-16, 12.48450537969573659, -130.1562500020483810 ) ) ;
#8166 = EDGE_CURVE ( 'NONE', #38628, #8276, #13850, .T. ) ;
#8167 = CARTESIAN_POINT ( 'NONE',  ( 7.070501591499377789E-16, 11.54700538379251284, -186.1250000000000000 ) ) ;
#8168 = DIRECTION ( 'NONE',  ( 1.000000000000000000, 0.000000000000000000, 0.000000000000000000 ) ) ;
#8170 = VERTEX_POINT ( 'NONE', #16058 ) ;
#8169 = CARTESIAN_POINT ( 'NONE',  ( 5.405949406249999534, 9.363379034771803333, -113.7812500020483952 ) ) ;
#8171 = DIRECTION ( 'NONE',  ( 1.000000000000000000, 0.000000000000000000, 0.000000000000000000 ) ) ;
#8172 = AXIS2_PLACEMENT_3D ( 'NONE', #29462, #26015, #30105 ) ;
#8173 = EDGE_LOOP ( 'NONE', ( #899, #21050, #39461, #9268 ) ) ;
#8174 = EDGE_LOOP ( 'NONE', ( #31194, #9121, #10151, #31189 ) ) ;
#8175 = CARTESIAN_POINT ( 'NONE',  ( 10.81189881249999729, 0.000000000000000000, -40.53125000204838102 ) ) ;
#8176 = COORDINATED_UNIVERSAL_TIME_OFFSET ( 6, 0, .AHEAD. ) ;
#8177 = CARTESIAN_POINT ( 'NONE',  ( 5.405949406249992428, -9.363379034771808662, -87.09375000204836681 ) ) ;
#8178 = LINE ( 'NONE', #33867, #2240 ) ;
#8179 = FACE_OUTER_BOUND ( 'NONE', #23562, .T. ) ;
#8180 = CARTESIAN_POINT ( 'NONE',  ( -2.121150477449813534E-15, -11.54700538379251284, -32.75000000409675494 ) ) ;
#8181 = CARTESIAN_POINT ( 'NONE',  ( -5.405949406249996869, 9.363379034771805109, -167.5312500020484094 ) ) ;
#8182 = CARTESIAN_POINT ( 'NONE',  ( 5.000000000000000000, 8.660254037844385522, -54.62500000409675494 ) ) ;
#8183 = EDGE_CURVE ( 'NONE', #36337, #3574, #28774, .T. ) ;
#8184 = CARTESIAN_POINT ( 'NONE',  ( -2.293366432827344421E-15, -12.48450537969573659, -124.7187500020483952 ) ) ;
#8185 = CARTESIAN_POINT ( 'NONE',  ( 10.81189881249999551, -6.242252689847874514, -83.96875000204838102 ) ) ;
#8186 = CARTESIAN_POINT ( 'NONE',  ( -10.81189881249999729, 1.324075727343319199E-15, -3.781250002048375247 ) ) ;
#8187 = CARTESIAN_POINT ( 'NONE',  ( 7.644554776091147741E-16, 12.48450537969573659, -195.9687500020484094 ) ) ;
#8188 = CARTESIAN_POINT ( 'NONE',  ( 10.81189881249999551, -6.242252689847874514, -91.65625000204838102 ) ) ;
#8189 = CARTESIAN_POINT ( 'NONE',  ( -10.00000000000000000, -5.773502691896251982, -181.5000000040967905 ) ) ;
#8190 = CARTESIAN_POINT ( 'NONE',  ( 5.405949406249999534, 9.363379034771803333, -170.7812500020484094 ) ) ;
#8191 = CARTESIAN_POINT ( 'NONE',  ( -5.000000000000003553, -8.660254037844383745, -28.37500000409676204 ) ) ;
#8192 = CARTESIAN_POINT ( 'NONE',  ( 10.81189881249999729, 0.000000000000000000, -172.5312500020484094 ) ) ;
#8193 = CARTESIAN_POINT ( 'NONE',  ( 5.405949406249999534, 9.363379034771803333, -188.7812500020484094 ) ) ;
#8194 = CARTESIAN_POINT ( 'NONE',  ( -5.405949406250003975, -9.363379034771801557, -52.84375000204835970 ) ) ;
#8195 = CARTESIAN_POINT ( 'NONE',  ( -4.999999999999996447, 8.660254037844387298, -163.8750000040967905 ) ) ;
#8196 = CARTESIAN_POINT ( 'NONE',  ( -2.293366432827344421E-15, -12.48450537969573659, -10.90625000204838457 ) ) ;
#8197 = CARTESIAN_POINT ( 'NONE',  ( 5.405949406249992428, -9.363379034771808662, -10.59375000204834727 ) ) ;
#8198 = DIRECTION ( 'NONE',  ( -0.000000000000000000, -0.000000000000000000, -1.000000000000000000 ) ) ;
#8199 = CARTESIAN_POINT ( 'NONE',  ( -5.405949406250003975, -9.363379034771801557, -124.8437500020483810 ) ) ;
#8200 = CARTESIAN_POINT ( 'NONE',  ( -5.000000000000003553, -8.660254037844383745, -96.99999999999998579 ) ) ;
#8201 = CARTESIAN_POINT ( 'NONE',  ( 5.405949406249992428, -9.363379034771808662, -19.78125000204836326 ) ) ;
#8202 = CARTESIAN_POINT ( 'NONE',  ( 4.999999999999992006, -8.660254037844389075, -104.6250000040967763 ) ) ;
#8203 = VECTOR ( 'NONE', #4957, 1000.000000000000000 ) ;
#8204 = CARTESIAN_POINT ( 'NONE',  ( -9.999999999999479527, -5.773502691896549521, -150.0000000040967905 ) ) ;
#8205 = CARTESIAN_POINT ( 'NONE',  ( -4.999999999999996447, 8.660254037844387298, -53.99999999999996447 ) ) ;
#8206 = CARTESIAN_POINT ( 'NONE',  ( 10.81189881249999729, 0.000000000000000000, -124.5312500020483952 ) ) ;
#8207 = CARTESIAN_POINT ( 'NONE',  ( 10.81189881249999729, 6.242252689847867408, -97.40625000204839523 ) ) ;
#8208 = ORIENTED_EDGE ( 'NONE', *, *, #4358, .F. ) ;
#8209 = B_SPLINE_CURVE_WITH_KNOTS ( 'NONE', 3,
 ( #27599, #5152, #33869, #1277, #11182, #14628, #24378, #40948, #38581, #41808, #42234, #34940, #25854, #15051, #25021, #21762, #38802, #28248, #6217, #12450, #9024, #31922, #22190, #28471, #2350, #19153, #15272, #8608 ),
 .UNSPECIFIED., .F., .F.,
 ( 4, 2, 2, 2, 2, 2, 2, 2, 2, 2, 2, 2, 2, 4 ),
 ( 1.019784333705586920E-15, 0.001286352574010762471, 0.002572705148020504925, 0.005145410296039989832, 0.006431762870049733370, 0.007718115444059476908, 0.009004468018069223048, 0.01029082059207896659, 0.01286352574009845713, 0.01543623088811794594, 0.01672258346212769295, 0.01800893603613743649, 0.01929528861014718349, 0.02058164118415692703 ),
 .UNSPECIFIED. ) ;
#8210 = CARTESIAN_POINT ( 'NONE',  ( -10.00000000000000000, -5.773502691896251982, -97.50000000409679046 ) ) ;
#8211 = CARTESIAN_POINT ( 'NONE',  ( 9.999999999999998224, 1.224646799147353059E-15, -99.99999999999998579 ) ) ;
#8212 = CARTESIAN_POINT ( 'NONE',  ( 10.81189881249999729, 0.000000000000000000, -166.5312500020484094 ) ) ;
#8213 = CARTESIAN_POINT ( 'NONE',  ( 7.644554776091147741E-16, 12.48450537969573659, -56.46875000204837391 ) ) ;
#8214 = ORIENTED_EDGE ( 'NONE', *, *, #36718, .T. ) ;
#8215 = CARTESIAN_POINT ( 'NONE',  ( -5.000000000000003553, -8.660254037844383745, -21.99999999999996447 ) ) ;
#8216 = CARTESIAN_POINT ( 'NONE',  ( -5.405949406250003975, -9.363379034771801557, -27.53125000204836681 ) ) ;
#8217 = CARTESIAN_POINT ( 'NONE',  ( 5.000000000000000000, 8.660254037844385522, -157.7500000000000000 ) ) ;
#8218 = FACE_OUTER_BOUND ( 'NONE', #30549, .T. ) ;
#8219 = CARTESIAN_POINT ( 'NONE',  ( -9.999999999999998224, 1.224646799147353059E-15, -27.12500000409676204 ) ) ;
#8220 = DIRECTION ( 'NONE',  ( -0.000000000000000000, 1.000000000000000000, -0.000000000000000000 ) ) ;
#8221 = CARTESIAN_POINT ( 'NONE',  ( -10.81189881249999729, 1.324075727343319199E-15, -132.7812500020483810 ) ) ;
#8222 = CARTESIAN_POINT ( 'NONE',  ( -9.999999999999998224, 1.224646799147353059E-15, -200.0000000000000000 ) ) ;
#8223 = CARTESIAN_POINT ( 'NONE',  ( -5.000000000000003553, -8.660254037844383745, -44.87500000409677625 ) ) ;
#8224 = ORIENTED_EDGE ( 'NONE', *, *, #9990, .F. ) ;
#8225 = CARTESIAN_POINT ( 'NONE',  ( 5.405949406249992428, -9.363379034771808662, -63.28125000204837391 ) ) ;
#8226 = CALENDAR_DATE ( 2026, 28, 9 ) ;
#8228 = VERTEX_POINT ( 'NONE', #3979 ) ;
#8227 = ORIENTED_EDGE ( 'NONE', *, *, #22293, .F. ) ;
#8229 = CARTESIAN_POINT ( 'NONE',  ( -2.121150477449813534E-15, -11.54700538379251284, -120.8749999999999858 ) ) ;
#8230 = CARTESIAN_POINT ( 'NONE',  ( -9.999999999999998224, 1.224646799147353059E-15, -141.1250000040967905 ) ) ;
#8231 = CARTESIAN_POINT ( 'NONE',  ( 5.405949406249992428, -9.363379034771808662, -160.5937500020484094 ) ) ;
#8232 = CARTESIAN_POINT ( 'NONE',  ( -10.81189881249999729, 6.242252689847871849, -185.4062500020484094 ) ) ;
#8233 = CARTESIAN_POINT ( 'NONE',  ( 5.405949406249992428, -9.363379034771808662, -16.59375000204835260 ) ) ;
#8234 = VECTOR ( 'NONE', #18693, 1000.000000000000000 ) ;
#8235 = ADVANCED_FACE ( 'NONE', ( #33982 ), #11072, .F. ) ;
#8236 = CARTESIAN_POINT ( 'NONE',  ( 10.81189881249999729, 0.000000000000000000, -148.3437500020483810 ) ) ;
#8237 = EDGE_CURVE ( 'NONE', #15924, #21752, #16877, .T. ) ;
#8238 = CARTESIAN_POINT ( 'NONE',  ( -10.81189881249999729, 6.242252689847871849, -107.4062500020483810 ) ) ;
#8239 = CARTESIAN_POINT ( 'NONE',  ( -5.405949406249996869, 9.363379034771805109, -108.8437500020483810 ) ) ;
#8240 = CARTESIAN_POINT ( 'NONE',  ( -9.999999999999998224, 1.224646799147353059E-15, -161.7500000000000000 ) ) ;
#8241 = CARTESIAN_POINT ( 'NONE',  ( -5.405949406250003975, -9.363379034771801557, -114.5312500020483952 ) ) ;
#8242 = CARTESIAN_POINT ( 'NONE',  ( -10.81189881249999907, -6.242252689847864744, -3.468750002048364145 ) ) ;
#8243 = CARTESIAN_POINT ( 'NONE',  ( 7.644554776091147741E-16, 12.48450537969573659, -128.4687500020483810 ) ) ;
#8244 = CARTESIAN_POINT ( 'NONE',  ( 5.405949406249999534, 9.363379034771803333, -191.7812500020484094 ) ) ;
#8245 = AXIS2_PLACEMENT_3D ( 'NONE', #35799, #39442, #3201 ) ;
#8246 = CARTESIAN_POINT ( 'NONE',  ( 0.000000000000000000, 0.000000000000000000, -99.99999999999998579 ) ) ;
#8247 = CARTESIAN_POINT ( 'NONE',  ( -5.000000000000003553, -8.660254037844383745, -151.0000000000000000 ) ) ;
#8248 = CARTESIAN_POINT ( 'NONE',  ( -2.121150477449813534E-15, -11.54700538379251284, -12.87499999999996803 ) ) ;
#8249 = CARTESIAN_POINT ( 'NONE',  ( 10.81189881249999729, 6.242252689847867408, -79.21875000204839523 ) ) ;
#8250 = CARTESIAN_POINT ( 'NONE',  ( -10.81189881249999729, 6.242252689847871849, -53.21875000204837391 ) ) ;
#8251 = DIRECTION ( 'NONE',  ( -0.000000000000000000, -0.000000000000000000, 1.000000000000000000 ) ) ;
#8252 = CARTESIAN_POINT ( 'NONE',  ( -5.405949406250003975, -9.363379034771801557, -35.03125000204837391 ) ) ;
#8253 = CARTESIAN_POINT ( 'NONE',  ( 10.81189881249999907, 6.242252689847868297, -49.21875000204835970 ) ) ;
#8254 = CARTESIAN_POINT ( 'NONE',  ( 9.999999999999998224, 0.000000000000000000, -137.0000000000000000 ) ) ;
#8255 = CARTESIAN_POINT ( 'NONE',  ( 7.644554776091147741E-16, 12.48450537969573659, -144.9687500020483810 ) ) ;
#8256 = CARTESIAN_POINT ( 'NONE',  ( 9.999999999999996447, -5.773502691896262640, -123.6250000000000000 ) ) ;
#8257 = CARTESIAN_POINT ( 'NONE',  ( 9.999999999999479527, 5.773502691896553074, -42.37499999999997158 ) ) ;
#8258 = CARTESIAN_POINT ( 'NONE',  ( 4.999999999999992006, -8.660254037844389075, -72.74999999999998579 ) ) ;
#8259 = CARTESIAN_POINT ( 'NONE',  ( 10.81189881249999729, 6.242252689847867408, -7.406250002048366810 ) ) ;
#8260 =( BOUNDED_CURVE ( )  B_SPLINE_CURVE ( 2, ( #37508, #11379, #17635, #21538, #30829, #7951, #15259 ),
 .UNSPECIFIED., .F., .F. ) 
 B_SPLINE_CURVE_WITH_KNOTS ( ( 3, 2, 2, 3 ),
 ( 0.3955223880597015795, 0.3967661691542289648, 0.3980099502487563501, 0.3992537313432836799 ),
 .UNSPECIFIED. ) 
 CURVE ( )  GEOMETRIC_REPRESENTATION_ITEM ( )  RATIONAL_B_SPLINE_CURVE ( ( 0.9999999999999880096, 0.8660254037844506980, 1.000000000000000000, 0.8660254037844387076, 1.000000000000000000, 0.8660254037844267172, 1.000000000000011990 ) ) 
 REPRESENTATION_ITEM ( '' )  );
#8261 = EDGE_LOOP ( 'NONE', ( #6257, #30204, #39601, #32374 ) ) ;
#8262 = CARTESIAN_POINT ( 'NONE',  ( 10.81189881249999551, -6.242252689847874514, -100.6562500020483952 ) ) ;
#8263 = CARTESIAN_POINT ( 'NONE',  ( 5.000000000000000000, 8.660254037844385522, -122.1250000040967905 ) ) ;
#8264 = CARTESIAN_POINT ( 'NONE',  ( 7.644554776091147741E-16, 12.48450537969573659, -80.46875000204838102 ) ) ;
#8265 = CARTESIAN_POINT ( 'NONE',  ( 10.00000000000000000, 5.773502691896255534, -33.75000000409674783 ) ) ;
#8266 = CARTESIAN_POINT ( 'NONE',  ( 7.070501591499376803E-16, 11.54700538379251284, -61.62499999999998579 ) ) ;
#8267 = CARTESIAN_POINT ( 'NONE',  ( 10.81189881249999551, -6.242252689847874514, -48.15625000204837391 ) ) ;
#8268 =( BOUNDED_CURVE ( )  B_SPLINE_CURVE ( 2, ( #27736, #1845, #2280, #28599, #14971, #34435, #11313 ),
 .UNSPECIFIED., .F., .F. ) 
 B_SPLINE_CURVE_WITH_KNOTS ( ( 3, 2, 2, 3 ),
 ( 0.3432835820895522860, 0.3445273631840797268, 0.3457711442786070566, 0.3470149253731344974 ),
 .UNSPECIFIED. ) 
 CURVE ( )  GEOMETRIC_REPRESENTATION_ITEM ( )  RATIONAL_B_SPLINE_CURVE ( ( 0.9999999999999940048, 0.8660254037844447028, 1.000000000000000000, 0.8660254037844387076, 1.000000000000000000, 0.8660254037844207220, 1.000000000000017986 ) ) 
 REPRESENTATION_ITEM ( '' )  );
#8269 = FACE_OUTER_BOUND ( 'NONE', #24687, .T. ) ;
#8270 = CARTESIAN_POINT ( 'NONE',  ( 10.81189881249999907, 6.242252689847868297, -142.4062500020484094 ) ) ;
#8271 = AXIS2_PLACEMENT_3D ( 'NONE', #4492, #40509, #23285 ) ;
#8272 = CARTESIAN_POINT ( 'NONE',  ( -5.405949406249996869, 9.363379034771805109, -123.8437500020483952 ) ) ;
#8273 = CARTESIAN_POINT ( 'NONE',  ( 9.999999999998969713, 5.773502691896851502, -3.750000004096736284 ) ) ;
#8274 = ADVANCED_FACE ( 'NONE', ( #17120 ), #10648, .T. ) ;
#8275 = CARTESIAN_POINT ( 'NONE',  ( 9.999999999999998224, 0.000000000000000000, -200.0000000000000000 ) ) ;
#8276 = VERTEX_POINT ( 'NONE', #36991 ) ;
#8277 = VERTEX_POINT ( 'NONE', #7426 ) ;
#8278 = EDGE_LOOP ( 'NONE', ( #15863, #10747, #42471, #36696 ) ) ;
#8279 = CARTESIAN_POINT ( 'NONE',  ( -9.999999999999998224, 1.224646799147353059E-15, -103.2500000000000000 ) ) ;
#8280 = CARTESIAN_POINT ( 'NONE',  ( -5.405949406249996869, 9.363379034771805109, -180.8437500020483810 ) ) ;
#8281 = CARTESIAN_POINT ( 'NONE',  ( -10.81189881249999907, -6.242252689847864744, -36.46875000204835970 ) ) ;
#8282 = CARTESIAN_POINT ( 'NONE',  ( 9.999999999999998224, 1.224646799147353059E-15, -99.99999999999998579 ) ) ;
#8283 = DIRECTION ( 'NONE',  ( 1.000000000000000000, 0.000000000000000000, 0.000000000000000000 ) ) ;
#8284 = EDGE_CURVE ( 'NONE', #23120, #28565, #12229, .T. ) ;
#8285 = CARTESIAN_POINT ( 'NONE',  ( -10.81189881249999729, 6.242252689847871849, -171.7187500020483810 ) ) ;
#8286 = CARTESIAN_POINT ( 'NONE',  ( -10.81189881249999729, 1.324075727343319199E-15, -150.5937500020483810 ) ) ;
#8287 = CARTESIAN_POINT ( 'NONE',  ( -9.999999999999998224, 1.224646799147353059E-15, -112.2499999999999858 ) ) ;
#8288 = CARTESIAN_POINT ( 'NONE',  ( 7.644554776091147741E-16, 12.48450537969573659, -141.9687500020483810 ) ) ;
#8289 = CARTESIAN_POINT ( 'NONE',  ( 5.405949406249999534, 9.363379034771803333, -148.2812500020483810 ) ) ;
#8291 = EDGE_CURVE ( 'NONE', #26792, #32801, #11289, .T. ) ;
#8290 = CARTESIAN_POINT ( 'NONE',  ( 5.405949406249999534, 9.363379034771803333, -157.0937500020483810 ) ) ;
#8292 = CARTESIAN_POINT ( 'NONE',  ( 9.999999999999998224, 0.000000000000000000, -134.3750000040967905 ) ) ;
#8293 = CARTESIAN_POINT ( 'NONE',  ( -10.00000000000051337, 5.773502691895962435, -70.37499999999997158 ) ) ;
#8294 = CARTESIAN_POINT ( 'NONE',  ( 7.070501591499377789E-16, 11.54700538379251284, -171.1250000000000000 ) ) ;
#8295 = AXIS2_PLACEMENT_3D ( 'NONE', #20404, #1425, #41539 ) ;
#8296 = EDGE_CURVE ( 'NONE', #26141, #42072, #21226, .T. ) ;
#8297 = CARTESIAN_POINT ( 'NONE',  ( 7.644554776091147741E-16, 12.48450537969573659, -92.46875000204838102 ) ) ;
#8298 = CARTESIAN_POINT ( 'NONE',  ( 9.999999999999998224, 0.000000000000000000, -180.8750000040967905 ) ) ;
#8299 = CARTESIAN_POINT ( 'NONE',  ( -10.81189881249999729, 1.324075727343319199E-15, -60.78125000204836681 ) ) ;
#8300 = CARTESIAN_POINT ( 'NONE',  ( -2.293366432827344421E-15, -12.48450537969573659, -177.2187500020484094 ) ) ;
#8301 = CARTESIAN_POINT ( 'NONE',  ( -2.293366432827344421E-15, -12.48450537969573659, -115.9062500020483810 ) ) ;
#8302 = CARTESIAN_POINT ( 'NONE',  ( -10.81189881249999729, -6.242252689847864744, -156.6562500020484094 ) ) ;
#8303 = PRODUCT_DEFINITION ( 'UNKNOWN', '', #24948, #36055 ) ;
#8304 = CARTESIAN_POINT ( 'NONE',  ( -9.999999999999998224, 1.224646799147353059E-15, -200.0000000000000000 ) ) ;
#8305 = CARTESIAN_POINT ( 'NONE',  ( 5.405949406249992428, -9.363379034771808662, -40.78125000204838102 ) ) ;
#8306 = CARTESIAN_POINT ( 'NONE',  ( -9.999999999999998224, 5.773502691896259087, -129.2500000040967905 ) ) ;
#8307 = CARTESIAN_POINT ( 'NONE',  ( 10.00000000000000000, 5.773502691896255534, -99.37499999999998579 ) ) ;
#8308 = ORIENTED_EDGE ( 'NONE', *, *, #38527, .F. ) ;
#8309 = CARTESIAN_POINT ( 'NONE',  ( -2.293366432827344421E-15, -12.48450537969573659, -124.9062500020483810 ) ) ;
#8310 = CARTESIAN_POINT ( 'NONE',  ( -2.121150477449813534E-15, -11.54700538379251284, -145.2500000040967905 ) ) ;
#8311 = LINE ( 'NONE', #23694, #26376 ) ;
#8312 = CARTESIAN_POINT ( 'NONE',  ( -5.405949406249996869, 9.363379034771805109, -184.0312500020484094 ) ) ;
#8313 = ORIENTED_EDGE ( 'NONE', *, *, #37146, .F. ) ;
#8314 = CARTESIAN_POINT ( 'NONE',  ( -10.81189881249999729, 6.242252689847871849, -174.7187500020483810 ) ) ;
#8315 = CARTESIAN_POINT ( 'NONE',  ( -2.121150477449813534E-15, -11.54700538379251284, -59.75000000409676915 ) ) ;
#8316 = DIRECTION ( 'NONE',  ( 0.000000000000000000, 0.000000000000000000, 1.000000000000000000 ) ) ;
#8317 = DIRECTION ( 'NONE',  ( 1.000000000000000000, 0.000000000000000000, 0.000000000000000000 ) ) ;
#8318 = CARTESIAN_POINT ( 'NONE',  ( 10.81189881249999907, 6.242252689847868297, -67.40625000204839523 ) ) ;
#8319 = CARTESIAN_POINT ( 'NONE',  ( -2.293366432827344421E-15, -12.48450537969573659, -52.90625000204837391 ) ) ;
#8320 = EDGE_CURVE ( 'NONE', #36297, #27433, #34821, .T. ) ;
#8321 = CARTESIAN_POINT ( 'NONE',  ( 9.999999999999996447, -5.773502691896262640, -41.50000000409676204 ) ) ;
#8322 = CARTESIAN_POINT ( 'NONE',  ( 5.405949406249999534, 9.363379034771803333, -5.593750002048370362 ) ) ;
#8323 = CYLINDRICAL_SURFACE ( 'NONE', #25559, 9.999999999999998224 ) ;
#8324 = CARTESIAN_POINT ( 'NONE',  ( 5.405949406249999534, 9.363379034771803333, -179.7812500020484094 ) ) ;
#8325 = CARTESIAN_POINT ( 'NONE',  ( 9.999999999999479527, 5.773502691896553074, -2.250000004096741613 ) ) ;
#8326 = LINE ( 'NONE', #21042, #9603 ) ;
#8327 = VERTEX_POINT ( 'NONE', #24275 ) ;
#8328 = CARTESIAN_POINT ( 'NONE',  ( 9.999999999998969713, 5.773502691896851502, -17.25000000409673717 ) ) ;
#8329 = LINE ( 'NONE', #18013, #15559 ) ;
#8330 = DIRECTION ( 'NONE',  ( 1.000000000000000000, 0.000000000000000000, 0.000000000000000000 ) ) ;
#8331 = VECTOR ( 'NONE', #18293, 1000.000000000000000 ) ;
#8333 = EDGE_LOOP ( 'NONE', ( #2278, #12553, #14454, #7783 ) ) ;
#8332 = CARTESIAN_POINT ( 'NONE',  ( 10.81189881249999907, 6.242252689847868297, -76.40625000204839523 ) ) ;
#8335 = ORIENTED_EDGE ( 'NONE', *, *, #16447, .T. ) ;
#8334 = CARTESIAN_POINT ( 'NONE',  ( 9.999999999999998224, 0.000000000000000000, -81.49999999999998579 ) ) ;
#8336 = VERTEX_POINT ( 'NONE', #30744 ) ;
#8337 = CARTESIAN_POINT ( 'NONE',  ( 10.81189881249999729, 6.242252689847867408, -37.21875000204835970 ) ) ;
#8338 = CARTESIAN_POINT ( 'NONE',  ( -10.00000000000051337, 5.773502691895962435, -76.75000000409677625 ) ) ;
#8339 = CARTESIAN_POINT ( 'NONE',  ( -10.81189881249999907, -6.242252689847864744, -14.15625000204836859 ) ) ;
#8341 = VERTEX_POINT ( 'NONE', #14297 ) ;
#8340 = CARTESIAN_POINT ( 'NONE',  ( 10.81189881249999907, 6.242252689847868297, -59.71875000204838102 ) ) ;
#8342 = FACE_OUTER_BOUND ( 'NONE', #4289, .T. ) ;
#8343 = CARTESIAN_POINT ( 'NONE',  ( -4.999999999999996447, 8.660254037844387298, -38.99999999999997868 ) ) ;
#8344 = CARTESIAN_POINT ( 'NONE',  ( -10.81189881249999729, 6.242252689847871849, -198.7187500020484379 ) ) ;
#8345 = CARTESIAN_POINT ( 'NONE',  ( 5.405949406249999534, 9.363379034771803333, -173.5937500020484094 ) ) ;
#8346 =( BOUNDED_CURVE ( )  B_SPLINE_CURVE ( 2, ( #22944, #9553, #30060, #2879, #6532, #42344, #25968 ),
 .UNSPECIFIED., .F., .F. ) 
 B_SPLINE_CURVE_WITH_KNOTS ( ( 3, 2, 2, 3 ),
 ( 0.8656716417910450545, 0.8669154228855724398, 0.8681592039800998251, 0.8694029850746272103 ),
 .UNSPECIFIED. ) 
 CURVE ( )  GEOMETRIC_REPRESENTATION_ITEM ( )  RATIONAL_B_SPLINE_CURVE ( ( 0.9999999999999641398, 0.8660254037844745678, 1.000000000000000000, 0.8660254037844387076, 1.000000000000000000, 0.8660254037844028474, 1.000000000000035971 ) ) 
 REPRESENTATION_ITEM ( '' )  );
#8347 = CARTESIAN_POINT ( 'NONE',  ( 7.644554776091147741E-16, 12.48450537969573659, -165.9687500020483810 ) ) ;
#8348 = CARTESIAN_POINT ( 'NONE',  ( 5.405949406249992428, -9.363379034771808662, -175.5937500020484094 ) ) ;
#8349 = CARTESIAN_POINT ( 'NONE',  ( 4.999999999999992006, -8.660254037844389075, -192.7500000000000000 ) ) ;
#8350 = CARTESIAN_POINT ( 'NONE',  ( 7.070501591499376803E-16, 11.54700538379251284, -71.00000000409676204 ) ) ;
#8351 = CARTESIAN_POINT ( 'NONE',  ( -5.000000000000003553, -8.660254037844383745, -197.5000000000000000 ) ) ;
#8352 = CARTESIAN_POINT ( 'NONE',  ( -2.293366432827344421E-15, -12.48450537969573659, -109.7187500020483668 ) ) ;
#8353 = FACE_OUTER_BOUND ( 'NONE', #19291, .T. ) ;
#8354 = CARTESIAN_POINT ( 'NONE',  ( 7.644554776091147741E-16, 12.48450537969573659, -85.15625000204838102 ) ) ;
#8355 = CARTESIAN_POINT ( 'NONE',  ( 7.644554776091147741E-16, 12.48450537969573659, -93.96875000204838102 ) ) ;
#8356 = CARTESIAN_POINT ( 'NONE',  ( -10.81189881249999729, 1.324075727343319199E-15, -60.59375000204836681 ) ) ;
#8357 = CARTESIAN_POINT ( 'NONE',  ( 10.81189881249999551, -6.242252689847874514, -72.15625000204836681 ) ) ;
#8358 = CARTESIAN_POINT ( 'NONE',  ( -10.00000000000000000, -5.773502691896251982, -153.0000000040967905 ) ) ;
#8359 = CARTESIAN_POINT ( 'NONE',  ( -10.00000000000000000, -5.773502691896251982, -125.6249999999999858 ) ) ;
#8360 = CARTESIAN_POINT ( 'NONE',  ( -5.405949406250003975, -9.363379034771801557, -149.0312500020483810 ) ) ;
#8361 = CARTESIAN_POINT ( 'NONE',  ( 10.81189881249999907, 6.242252689847868297, -161.9062500020484094 ) ) ;
#8362 = APPROVAL_PERSON_ORGANIZATION ( #15522, #37034, #8864 ) ;
#8363 = ADVANCED_FACE ( 'NONE', ( #27497 ), #40631, .F. ) ;
#8364 = CARTESIAN_POINT ( 'NONE',  ( 9.999999999999998224, 0.000000000000000000, -174.5000000000000284 ) ) ;
#8365 = DIRECTION ( 'NONE',  ( -0.000000000000000000, -0.000000000000000000, 1.000000000000000000 ) ) ;
#8366 = CARTESIAN_POINT ( 'NONE',  ( -5.405949406250003975, -9.363379034771801557, -94.84375000204838102 ) ) ;
#8367 = ORIENTED_EDGE ( 'NONE', *, *, #29665, .T. ) ;
#8368 = CARTESIAN_POINT ( 'NONE',  ( -10.00000000000000000, -5.773502691896251982, -74.62499999999997158 ) ) ;
#8369 = CARTESIAN_POINT ( 'NONE',  ( -5.405949406249996869, 9.363379034771805109, -198.8437500020484094 ) ) ;
#8370 = CARTESIAN_POINT ( 'NONE',  ( 7.070501591499377789E-16, 11.54700538379251284, -84.50000000409677625 ) ) ;
#8371 = CARTESIAN_POINT ( 'NONE',  ( 7.070501591499376803E-16, 11.54700538379251284, -26.00000000409676915 ) ) ;
#8372 = CARTESIAN_POINT ( 'NONE',  ( -5.405949406249996869, 9.363379034771805109, -95.53125000204838102 ) ) ;
#8373 = CARTESIAN_POINT ( 'NONE',  ( 10.81189881249999551, -6.242252689847874514, -73.65625000204835260 ) ) ;
#8374 = CARTESIAN_POINT ( 'NONE',  ( 9.999999999999998224, 0.000000000000000000, -68.37500000409677625 ) ) ;
#8375 = CARTESIAN_POINT ( 'NONE',  ( -9.999999999999998224, 1.224646799147353059E-15, -112.6250000040967763 ) ) ;
#8376 = CARTESIAN_POINT ( 'NONE',  ( 7.644554776091147741E-16, 12.48450537969573659, -26.46875000204837391 ) ) ;
#8377 = ORIENTED_EDGE ( 'NONE', *, *, #3654, .F. ) ;
#8378 = CARTESIAN_POINT ( 'NONE',  ( 7.070501591499377789E-16, 11.54700538379251284, -0.1249999999999685252 ) ) ;
#8379 = CARTESIAN_POINT ( 'NONE',  ( 7.644554776091147741E-16, 12.48450537969573659, -17.65625000204837391 ) ) ;
#8380 = CARTESIAN_POINT ( 'NONE',  ( -5.405949406250003975, -9.363379034771801557, -16.84375000204835260 ) ) ;
#8381 = CARTESIAN_POINT ( 'NONE',  ( -9.999999999999479527, -5.773502691896549521, -118.5000000040967763 ) ) ;
#8382 = CARTESIAN_POINT ( 'NONE',  ( -10.81189881249999729, 1.324075727343319199E-15, -146.0937500020483810 ) ) ;
#8383 = CARTESIAN_POINT ( 'NONE',  ( -9.999999999999998224, 1.224646799147353059E-15, -50.74999999999996447 ) ) ;
#8384 = DIRECTION ( 'NONE',  ( -0.000000000000000000, -0.000000000000000000, -1.000000000000000000 ) ) ;
#8385 = CARTESIAN_POINT ( 'NONE',  ( -2.293366432827344421E-15, -12.48450537969573659, -130.9062500020483810 ) ) ;
#8386 = CARTESIAN_POINT ( 'NONE',  ( -9.999999999999998224, 1.224646799147353059E-15, -181.2500000000000284 ) ) ;
#8387 = CARTESIAN_POINT ( 'NONE',  ( 7.070501591499376803E-16, 11.54700538379251284, -106.6249999999999858 ) ) ;
#8389 = ORIENTED_EDGE ( 'NONE', *, *, #39645, .F. ) ;
#8388 = CARTESIAN_POINT ( 'NONE',  ( -2.293366432827344421E-15, -12.48450537969573659, -111.4062500020483952 ) ) ;
#8390 = VERTEX_POINT ( 'NONE', #34201 ) ;
#8391 = EDGE_LOOP ( 'NONE', ( #8490, #8089, #40202, #31753 ) ) ;
#8392 = VECTOR ( 'NONE', #25943, 1000.000000000000000 ) ;
#8393 =( BOUNDED_CURVE ( )  B_SPLINE_CURVE ( 2, ( #2250, #15369, #28782, #1813, #5892, #34616, #19049 ),
 .UNSPECIFIED., .F., .F. ) 
 B_SPLINE_CURVE_WITH_KNOTS ( ( 3, 2, 2, 3 ),
 ( 0.4029850746268657802, 0.4042288557213931655, 0.4054726368159204397, 0.4067164179104478250 ),
 .UNSPECIFIED. ) 
 CURVE ( )  GEOMETRIC_REPRESENTATION_ITEM ( )  RATIONAL_B_SPLINE_CURVE ( ( 0.9999999999999880096, 0.8660254037844506980, 1.000000000000000000, 0.8660254037844387076, 1.000000000000000000, 0.8660254037844327124, 1.000000000000005995 ) ) 
 REPRESENTATION_ITEM ( '' )  );
#8394 = CARTESIAN_POINT ( 'NONE',  ( -10.81189881249999729, 1.324075727343319199E-15, -36.78125000204837391 ) ) ;
#8395 = COORDINATED_UNIVERSAL_TIME_OFFSET ( 6, 0, .AHEAD. ) ;
#8396 = LOCAL_TIME ( 11, 57, 6.000000000000000000, #21374 ) ;
#8397 = CARTESIAN_POINT ( 'NONE',  ( -10.81189881249999729, 6.242252689847871849, -89.21875000204836681 ) ) ;
#8398 = DIRECTION ( 'NONE',  ( 0.000000000000000000, -1.000000000000000000, 0.000000000000000000 ) ) ;
#8399 = DIRECTION ( 'NONE',  ( -0.000000000000000000, -0.000000000000000000, 1.000000000000000000 ) ) ;
#8400 = DIRECTION ( 'NONE',  ( -0.000000000000000000, -0.000000000000000000, 1.000000000000000000 ) ) ;
#8401 = CARTESIAN_POINT ( 'NONE',  ( -5.405949406250003975, -9.363379034771801557, -164.0312500020484094 ) ) ;
#8402 = VECTOR ( 'NONE', #57, 1000.000000000000000 ) ;
#8403 = CARTESIAN_POINT ( 'NONE',  ( -10.81189881249999729, 1.324075727343319199E-15, -116.0937500020483810 ) ) ;
#8404 = CARTESIAN_POINT ( 'NONE',  ( -10.81189881249999729, 1.324075727343319199E-15, -89.09375000204838102 ) ) ;
#8405 = CARTESIAN_POINT ( 'NONE',  ( 10.81189881249999729, 0.000000000000000000, -4.531250002048375691 ) ) ;
#8406 = CARTESIAN_POINT ( 'NONE',  ( -2.293366432827344421E-15, -12.48450537969573659, -196.7187500020484094 ) ) ;
#8407 = CARTESIAN_POINT ( 'NONE',  ( 10.81189881249999729, 0.000000000000000000, -94.53125000204838102 ) ) ;
#8408 = CARTESIAN_POINT ( 'NONE',  ( 9.999999999999998224, 0.000000000000000000, -177.8750000040967905 ) ) ;
#8409 = CARTESIAN_POINT ( 'NONE',  ( 7.644554776091147741E-16, 12.48450537969573659, -170.6562500020484094 ) ) ;
#8410 = CARTESIAN_POINT ( 'NONE',  ( -9.999999999999998224, 1.224646799147353059E-15, -103.2500000000000000 ) ) ;
#8411 = CARTESIAN_POINT ( 'NONE',  ( 5.405949406249999534, 9.363379034771803333, -176.7812500020484094 ) ) ;
#8412 = CARTESIAN_POINT ( 'NONE',  ( -10.81189881249999729, 1.324075727343319199E-15, -189.7812500020484094 ) ) ;
#8413 = CARTESIAN_POINT ( 'NONE',  ( 10.81189881249999551, -6.242252689847874514, -53.96875000204838102 ) ) ;
#8414 = CARTESIAN_POINT ( 'NONE',  ( -10.00000000000000000, -5.773502691896251982, -166.5000000040967905 ) ) ;
#8415 = CARTESIAN_POINT ( 'NONE',  ( -10.81189881249999907, -6.242252689847864744, -3.656250002048349046 ) ) ;
#8416 = CARTESIAN_POINT ( 'NONE',  ( -5.405949406249996869, 9.363379034771805109, -11.34375000204834727 ) ) ;
#8417 = CARTESIAN_POINT ( 'NONE',  ( 10.00000000000012257, -5.773502691896187144, -164.5000000040967905 ) ) ;
#8418 = CARTESIAN_POINT ( 'NONE',  ( 10.81189881249999907, 6.242252689847868297, -121.2187500020483952 ) ) ;
#8419 = CARTESIAN_POINT ( 'NONE',  ( -9.999999999999998224, 5.773502691896259087, -98.87499999999998579 ) ) ;
#8420 = CARTESIAN_POINT ( 'NONE',  ( -10.81189881249999729, 1.324075727343319199E-15, -18.78125000204835970 ) ) ;
#8421 = CARTESIAN_POINT ( 'NONE',  ( -4.999999999999996447, 8.660254037844387298, -106.8750000040967763 ) ) ;
#8422 = CARTESIAN_POINT ( 'NONE',  ( 9.999999999998969713, 5.773502691896851502, -82.87499999999995737 ) ) ;
#8423 = CARTESIAN_POINT ( 'NONE',  ( -4.999999999999996447, 8.660254037844387298, -49.49999999999998579 ) ) ;
#8424 = CARTESIAN_POINT ( 'NONE',  ( -5.405949406250003975, -9.363379034771801557, -119.0312500020483952 ) ) ;
#8425 = CARTESIAN_POINT ( 'NONE',  ( 5.405949406249999534, 9.363379034771803333, -95.78125000204838102 ) ) ;
#8426 = ORIENTED_EDGE ( 'NONE', *, *, #26529, .T. ) ;
#8427 = CARTESIAN_POINT ( 'NONE',  ( 4.999999999999992006, -8.660254037844389075, -94.12500000409677625 ) ) ;
#8428 = CYLINDRICAL_SURFACE ( 'NONE', #13259, 20.00000000000000355 ) ;
#8429 = CARTESIAN_POINT ( 'NONE',  ( 5.405949406249992428, -9.363379034771808662, -157.7812500020484094 ) ) ;
#8430 = CARTESIAN_POINT ( 'NONE',  ( 10.81189881249999907, 6.242252689847868297, -46.21875000204837391 ) ) ;
#8431 = VERTEX_POINT ( 'NONE', #4617 ) ;
#8432 = CARTESIAN_POINT ( 'NONE',  ( -2.121150477449813534E-15, -11.54700538379251284, -26.37499999999997868 ) ) ;
#8433 = CARTESIAN_POINT ( 'NONE',  ( 7.644554776091147741E-16, 12.48450537969573659, -31.15625000204835260 ) ) ;
#8434 = CARTESIAN_POINT ( 'NONE',  ( 7.070501591499377789E-16, 11.54700538379251284, -162.1250000000000284 ) ) ;
#8435 = CYLINDRICAL_SURFACE ( 'NONE', #40733, 9.999999999999998224 ) ;
#8436 = CARTESIAN_POINT ( 'NONE',  ( -2.121150477449813534E-15, -11.54700538379251284, -28.25000000409675138 ) ) ;
#8437 = EDGE_CURVE ( 'NONE', #3228, #21146, #34411, .T. ) ;
#8438 = VECTOR ( 'NONE', #41845, 1000.000000000000000 ) ;
#8439 = CARTESIAN_POINT ( 'NONE',  ( 7.070501591499376803E-16, 11.54700538379251284, -168.1250000000000000 ) ) ;
#8440 = CARTESIAN_POINT ( 'NONE',  ( -2.293366432827344421E-15, -12.48450537969573659, -136.9062500020484094 ) ) ;
#8441 = CARTESIAN_POINT ( 'NONE',  ( 8.143302022011770447, 6.762395603866230509, -7.434655202704447971E-15 ) ) ;
#8442 = CARTESIAN_POINT ( 'NONE',  ( -9.999999999999998224, 1.224646799147353059E-15, -188.7500000000000000 ) ) ;
#8443 = ORIENTED_EDGE ( 'NONE', *, *, #30940, .T. ) ;
#8444 = CARTESIAN_POINT ( 'NONE',  ( -10.81189881249999729, 6.242252689847871849, -65.40625000204838102 ) ) ;
#8445 = PERSON_AND_ORGANIZATION ( #11915, #17965 ) ;
#8447 = ORIENTED_EDGE ( 'NONE', *, *, #11980, .T. ) ;
#8446 = ORIENTED_EDGE ( 'NONE', *, *, #11221, .T. ) ;
#8448 = FACE_OUTER_BOUND ( 'NONE', #4796, .T. ) ;
#8449 = AXIS2_PLACEMENT_3D ( 'NONE', #173, #6629, #26275 ) ;
#8450 = DIRECTION ( 'NONE',  ( -0.000000000000000000, -0.000000000000000000, -1.000000000000000000 ) ) ;
#8451 = CARTESIAN_POINT ( 'NONE',  ( 10.81189881249999907, 6.242252689847868297, -155.7187500020483810 ) ) ;
#8452 = CARTESIAN_POINT ( 'NONE',  ( 10.81189881249999729, 0.000000000000000000, -189.0312500020484094 ) ) ;
#8453 = CARTESIAN_POINT ( 'NONE',  ( -10.81189881249999729, 6.242252689847871849, -5.218750002048340164 ) ) ;
#8454 = CARTESIAN_POINT ( 'NONE',  ( -5.405949406250003975, -9.363379034771801557, -148.8437500020483810 ) ) ;
#8455 = CARTESIAN_POINT ( 'NONE',  ( 5.405949406249992428, -9.363379034771808662, -94.78125000204838102 ) ) ;
#8456 = CARTESIAN_POINT ( 'NONE',  ( 5.405949406249999534, 9.363379034771803333, -113.5937500020483810 ) ) ;
#8457 = CARTESIAN_POINT ( 'NONE',  ( 4.999999999999992006, -8.660254037844389075, -161.2500000000000000 ) ) ;
#8458 = CARTESIAN_POINT ( 'NONE',  ( -10.81189881249999729, 6.242252689847871849, -116.4062500020483810 ) ) ;
#8459 = CARTESIAN_POINT ( 'NONE',  ( -10.81189881249999729, 1.324075727343319199E-15, -0.5937500020483654772 ) ) ;
#8460 = CARTESIAN_POINT ( 'NONE',  ( 5.405949406249999534, 9.363379034771803333, -125.5937500020483668 ) ) ;
#8461 = CARTESIAN_POINT ( 'NONE',  ( -5.405949406250003975, -9.363379034771801557, -191.0312500020484094 ) ) ;
#8462 = CARTESIAN_POINT ( 'NONE',  ( -4.999999999999996447, 8.660254037844387298, -178.8750000040967905 ) ) ;
#8463 = CARTESIAN_POINT ( 'NONE',  ( 4.999999999999992006, -8.660254037844389075, -144.7500000000000000 ) ) ;
#8464 = CARTESIAN_POINT ( 'NONE',  ( 9.999999999999998224, 0.000000000000000000, -15.49999999999995737 ) ) ;
#8465 = AXIS2_PLACEMENT_3D ( 'NONE', #17676, #14218, #7563 ) ;
#8466 = CARTESIAN_POINT ( 'NONE',  ( -2.293366432827344421E-15, -12.48450537969573659, -78.21875000204838102 ) ) ;
#8467 = CARTESIAN_POINT ( 'NONE',  ( 5.405949406249999534, 9.363379034771803333, -58.09375000204835970 ) ) ;
#8468 = CARTESIAN_POINT ( 'NONE',  ( 9.999999999999998224, 0.000000000000000000, -189.8750000040967905 ) ) ;
#8469 = CARTESIAN_POINT ( 'NONE',  ( 5.405949406249992428, -9.363379034771808662, -36.28125000204837391 ) ) ;
#8470 = CARTESIAN_POINT ( 'NONE',  ( 5.405949406249999534, 9.363379034771803333, -34.09375000204836681 ) ) ;
#8471 = CARTESIAN_POINT ( 'NONE',  ( -5.405949406249996869, 9.363379034771805109, -146.3437500020483810 ) ) ;
#8472 = CARTESIAN_POINT ( 'NONE',  ( -9.999999999999998224, 5.773502691896259087, -122.8750000000000142 ) ) ;
#8473 = CARTESIAN_POINT ( 'NONE',  ( 10.00000000000000000, 5.773502691896255534, -78.37499999999998579 ) ) ;
#8474 = CARTESIAN_POINT ( 'NONE',  ( -5.405949406250003975, -9.363379034771801557, -141.5312500020483810 ) ) ;
#8475 = CARTESIAN_POINT ( 'NONE',  ( -10.81189881249999729, 6.242252689847871849, -6.906250002048365033 ) ) ;
#8476 = ORIENTED_EDGE ( 'NONE', *, *, #27218, .T. ) ;
#8477 = CARTESIAN_POINT ( 'NONE',  ( 4.999999999999992006, -8.660254037844389075, -164.2500000000000000 ) ) ;
#8478 = CARTESIAN_POINT ( 'NONE',  ( -5.000000000000003553, -8.660254037844383745, -113.8750000040967763 ) ) ;
#8479 = CARTESIAN_POINT ( 'NONE',  ( 9.999999999999998224, 0.000000000000000000, -179.3750000040967905 ) ) ;
#8480 = CARTESIAN_POINT ( 'NONE',  ( 5.405949406249992428, -9.363379034771808662, -78.09375000204838102 ) ) ;
#8481 = CARTESIAN_POINT ( 'NONE',  ( 7.070501591499377789E-16, 11.54700538379251284, -24.50000000409676204 ) ) ;
#8482 = CARTESIAN_POINT ( 'NONE',  ( -9.999999999999998224, 1.224646799147353059E-15, -61.24999999999997158 ) ) ;
#8483 = CARTESIAN_POINT ( 'NONE',  ( -10.81189881249999907, -6.242252689847864744, -41.15625000204836681 ) ) ;
#8484 = CARTESIAN_POINT ( 'NONE',  ( -9.999999999999227285, -5.773502691896698735, -137.6249999999999716 ) ) ;
#8485 = CARTESIAN_POINT ( 'NONE',  ( -10.81189881249999729, 1.324075727343319199E-15, -146.2812500020483810 ) ) ;
#8486 = CARTESIAN_POINT ( 'NONE',  ( -2.293366432827344421E-15, -12.48450537969573659, -127.7187500020483668 ) ) ;
#8488 = ADVANCED_FACE ( 'NONE', ( #31176 ), #14735, .T. ) ;
#8487 = CARTESIAN_POINT ( 'NONE',  ( -9.999999999999998224, 1.224646799147353059E-15, -190.2500000000000000 ) ) ;
#8489 = CARTESIAN_POINT ( 'NONE',  ( -9.999999999999998224, 1.224646799147353059E-15, -6.125000004096770034 ) ) ;
#8490 = ORIENTED_EDGE ( 'NONE', *, *, #21256, .F. ) ;
#8491 = EDGE_LOOP ( 'NONE', ( #18877, #38420, #27482, #13753 ) ) ;
#8492 = VERTEX_POINT ( 'NONE', #25338 ) ;
#8493 = CARTESIAN_POINT ( 'NONE',  ( -10.81189881249999907, -6.242252689847864744, -181.9687500020484094 ) ) ;
#8494 = CARTESIAN_POINT ( 'NONE',  ( -5.405949406250003975, -9.363379034771801557, -31.84375000204836681 ) ) ;
#8495 = DIRECTION ( 'NONE',  ( 1.000000000000000000, 0.000000000000000000, 0.000000000000000000 ) ) ;
#8496 = CARTESIAN_POINT ( 'NONE',  ( 10.81189881249999729, 0.000000000000000000, -175.3437500020483810 ) ) ;
#8497 = CARTESIAN_POINT ( 'NONE',  ( -5.405949406250003975, -9.363379034771801557, -151.8437500020483810 ) ) ;
#8498 = CARTESIAN_POINT ( 'NONE',  ( 5.000000000000000000, 8.660254037844385522, -178.7500000000000284 ) ) ;
#8499 = CARTESIAN_POINT ( 'NONE',  ( -2.293366432827344421E-15, -12.48450537969573659, -130.7187500020483810 ) ) ;
#8500 = CARTESIAN_POINT ( 'NONE',  ( 10.81189881249999551, -6.242252689847874514, -142.6562500020484094 ) ) ;
#8501 =( BOUNDED_CURVE ( )  B_SPLINE_CURVE ( 2, ( #42286, #30584, #40264, #1015, #25906, #39057, #9496 ),
 .UNSPECIFIED., .F., .F. ) 
 B_SPLINE_CURVE_WITH_KNOTS ( ( 3, 2, 2, 3 ),
 ( 0.1194029850746269744, 0.1206467661691543042, 0.1218905472636816062, 0.1231343283582089221 ),
 .UNSPECIFIED. ) 
 CURVE ( )  GEOMETRIC_REPRESENTATION_ITEM ( )  RATIONAL_B_SPLINE_CURVE ( ( 0.9999999999999880096, 0.8660254037844506980, 1.000000000000000000, 0.8660254037844387076, 1.000000000000000000, 0.8660254037844417052, 0.9999999999999970024 ) ) 
 REPRESENTATION_ITEM ( '' )  );
#8502 = CARTESIAN_POINT ( 'NONE',  ( 10.81189881249999729, 6.242252689847867408, -155.7187500020483810 ) ) ;
#8503 = CARTESIAN_POINT ( 'NONE',  ( 5.000000000000000000, 8.660254037844385522, -127.7499999999999716 ) ) ;
#8504 = CARTESIAN_POINT ( 'NONE',  ( 9.999999999999996447, -5.773502691896262640, -170.1250000000000000 ) ) ;
#8505 = CARTESIAN_POINT ( 'NONE',  ( -5.405949406249996869, 9.363379034771805109, -83.34375000204836681 ) ) ;
#8506 = CARTESIAN_POINT ( 'NONE',  ( -9.999999999999998224, 1.224646799147353059E-15, -82.62500000409676204 ) ) ;
#8507 = CARTESIAN_POINT ( 'NONE',  ( 7.644554776091147741E-16, 12.48450537969573659, -56.65625000204838102 ) ) ;
#8508 = CARTESIAN_POINT ( 'NONE',  ( -10.41934351496823830, 1.167130642714232946, -100.0000000000000142 ) ) ;
#8509 = CARTESIAN_POINT ( 'NONE',  ( -10.81189881249999729, 1.324075727343319199E-15, -167.0937500020484094 ) ) ;
#8510 = CARTESIAN_POINT ( 'NONE',  ( 5.405949406249992428, -9.363379034771808662, -117.2812500020483952 ) ) ;
#8511 = CARTESIAN_POINT ( 'NONE',  ( 7.644554776091147741E-16, 12.48450537969573659, -146.6562500020484094 ) ) ;
#8512 = DIRECTION ( 'NONE',  ( -0.000000000000000000, -0.000000000000000000, 1.000000000000000000 ) ) ;
#8513 = CARTESIAN_POINT ( 'NONE',  ( -10.81189881249999729, 1.324075727343319199E-15, -47.28125000204838813 ) ) ;
#8514 = CARTESIAN_POINT ( 'NONE',  ( -2.121150477449813534E-15, -11.54700538379251284, -118.2500000040968047 ) ) ;
#8515 = CARTESIAN_POINT ( 'NONE',  ( 10.00000000000000000, 5.773502691896255534, -96.37499999999998579 ) ) ;
#8516 = ORIENTED_EDGE ( 'NONE', *, *, #38069, .F. ) ;
#8517 = CARTESIAN_POINT ( 'NONE',  ( 10.81189881249999551, -6.242252689847874514, -123.1562500020483952 ) ) ;
#8518 = CARTESIAN_POINT ( 'NONE',  ( 10.00000000000000000, 5.773502691896255534, -147.7500000040967905 ) ) ;
#8519 = CARTESIAN_POINT ( 'NONE',  ( 5.000000000000000000, 8.660254037844385522, -192.6250000040967905 ) ) ;
#8520 = CARTESIAN_POINT ( 'NONE',  ( 10.81189881249999551, -6.242252689847874514, -184.6562500020484094 ) ) ;
#8521 = EDGE_LOOP ( 'NONE', ( #12703, #31423, #32673, #30203, #40185 ) ) ;
#8522 = CARTESIAN_POINT ( 'NONE',  ( 7.644554776091147741E-16, 12.48450537969573659, -170.4687500020483810 ) ) ;
#8523 = CARTESIAN_POINT ( 'NONE',  ( -5.000000000000003553, -8.660254037844383745, -56.87500000409676204 ) ) ;
#8524 = CARTESIAN_POINT ( 'NONE',  ( -5.000000000000003553, -8.660254037844383745, -166.0000000000000000 ) ) ;
#8525 = DIRECTION ( 'NONE',  ( 0.000000000000000000, 0.000000000000000000, 1.000000000000000000 ) ) ;
#8526 = CARTESIAN_POINT ( 'NONE',  ( 5.405949406249992428, -9.363379034771808662, -66.28125000204838102 ) ) ;
#8527 = CARTESIAN_POINT ( 'NONE',  ( 10.00000000000000000, 5.773502691896255534, -45.75000000409676204 ) ) ;
#8528 = CARTESIAN_POINT ( 'NONE',  ( -2.293366432827344421E-15, -12.48450537969573659, -3.218750002048353931 ) ) ;
#8529 = FACE_OUTER_BOUND ( 'NONE', #27731, .T. ) ;
#8530 = CARTESIAN_POINT ( 'NONE',  ( 7.644554776091147741E-16, 12.48450537969573659, -169.1562500020484094 ) ) ;
#8531 = DIRECTION ( 'NONE',  ( 0.6123724356957962467, -0.3535533905932744525, 0.7071067811865456854 ) ) ;
#8533 = EDGE_CURVE ( 'NONE', #107, #19501, #12476, .T. ) ;
#8532 = DIRECTION ( 'NONE',  ( 0.000000000000000000, 0.000000000000000000, -1.000000000000000000 ) ) ;
#8534 = ORIENTED_EDGE ( 'NONE', *, *, #7404, .T. ) ;
#8535 = CARTESIAN_POINT ( 'NONE',  ( 0.000000000000000000, 0.000000000000000000, -99.99999999999998579 ) ) ;
#8536 = EDGE_CURVE ( 'NONE', #16036, #4388, #25743, .T. ) ;
#8537 = LINE ( 'NONE', #22542, #28664 ) ;
#8538 = EDGE_CURVE ( 'NONE', #9539, #34380, #41501, .T. ) ;
#8539 = CARTESIAN_POINT ( 'NONE',  ( -4.999999999999996447, 8.660254037844387298, -195.3750000040967905 ) ) ;
#8541 = EDGE_LOOP ( 'NONE', ( #35824, #22345, #25279, #36449 ) ) ;
#8540 = CARTESIAN_POINT ( 'NONE',  ( 10.81189881249999907, 6.242252689847868297, -77.90625000204836681 ) ) ;
#8542 = CARTESIAN_POINT ( 'NONE',  ( 0.000000000000000000, 0.000000000000000000, 0.000000000000000000 ) ) ;
#8544 = ORIENTED_EDGE ( 'NONE', *, *, #12979, .T. ) ;
#8543 = CARTESIAN_POINT ( 'NONE',  ( -2.121150477449813534E-15, -11.54700538379251284, -119.3749999999999858 ) ) ;
#8545 = CC_DESIGN_DATE_AND_TIME_ASSIGNMENT ( #38160, #18082, ( #20655 ) ) ;
#8546 = EDGE_LOOP ( 'NONE', ( #16230, #29599, #8443, #24742 ) ) ;
#8547 = CARTESIAN_POINT ( 'NONE',  ( 7.644554776091147741E-16, 12.48450537969573659, -36.96875000204835970 ) ) ;
#8548 = CARTESIAN_POINT ( 'NONE',  ( -9.999999999999998224, 1.224646799147353059E-15, -49.24999999999998579 ) ) ;
#8549 = CARTESIAN_POINT ( 'NONE',  ( -2.293366432827344421E-15, -12.48450537969573659, -9.406250002048375691 ) ) ;
#8551 = ORIENTED_EDGE ( 'NONE', *, *, #24095, .T. ) ;
#8550 = CARTESIAN_POINT ( 'NONE',  ( -10.81189881249999729, 6.242252689847871849, -62.21875000204838813 ) ) ;
#8552 = CARTESIAN_POINT ( 'NONE',  ( 0.000000000000000000, 0.000000000000000000, -99.99999999999998579 ) ) ;
#8553 = CARTESIAN_POINT ( 'NONE',  ( -4.999999999999996447, 8.660254037844387298, -37.49999999999997868 ) ) ;
#8554 = EDGE_CURVE ( 'NONE', #41628, #11855, #14090, .T. ) ;
#8555 = CARTESIAN_POINT ( 'NONE',  ( -10.81189881249999729, -6.242252689847864744, -196.9687500020484094 ) ) ;
#8556 = CARTESIAN_POINT ( 'NONE',  ( 10.81189881249999907, 6.242252689847868297, -176.7187500020483810 ) ) ;
#8557 = CARTESIAN_POINT ( 'NONE',  ( 5.405949406249999534, 9.363379034771803333, -154.0937500020483810 ) ) ;
#8558 = DIRECTION ( 'NONE',  ( -1.000000000000000000, 0.000000000000000000, 0.000000000000000000 ) ) ;
#8559 = LINE ( 'NONE', #24974, #41909 ) ;
#8560 = LINE ( 'NONE', #32080, #21927 ) ;
#8561 = EDGE_CURVE ( 'NONE', #32336, #26629, #2303, .T. ) ;
#8562 = CARTESIAN_POINT ( 'NONE',  ( -9.999999999999998224, 1.224646799147353059E-15, -193.2500000000000000 ) ) ;
#8563 = CARTESIAN_POINT ( 'NONE',  ( 7.644554776091147741E-16, 12.48450537969573659, -108.9687500020483952 ) ) ;
#8564 = CARTESIAN_POINT ( 'NONE',  ( 9.999999999999998224, 1.224646799147353059E-15, -99.99999999999998579 ) ) ;
#8565 = CARTESIAN_POINT ( 'NONE',  ( 10.81189881249999551, -6.242252689847874514, -84.15625000204838102 ) ) ;
#8566 = CARTESIAN_POINT ( 'NONE',  ( -5.405949406250003975, -9.363379034771801557, -90.34375000204838102 ) ) ;
#8567 = CARTESIAN_POINT ( 'NONE',  ( -10.81189881249999729, 6.242252689847871849, -66.90625000204839523 ) ) ;
#8568 = CARTESIAN_POINT ( 'NONE',  ( 9.999999999999998224, 0.000000000000000000, -152.3750000040967905 ) ) ;
#8569 = CARTESIAN_POINT ( 'NONE',  ( 7.070501591499377789E-16, 11.54700538379251284, -126.1249999999999858 ) ) ;
#8570 = CARTESIAN_POINT ( 'NONE',  ( 5.405949406249999534, 9.363379034771803333, -154.2812500020484094 ) ) ;
#8571 = CARTESIAN_POINT ( 'NONE',  ( -2.293366432827344421E-15, -12.48450537969573659, -160.9062500020483810 ) ) ;
#8572 = CARTESIAN_POINT ( 'NONE',  ( -2.121150477449813534E-15, -11.54700538379251284, -39.87499999999996447 ) ) ;
#8573 = CARTESIAN_POINT ( 'NONE',  ( 0.000000000000000000, 0.000000000000000000, -169.9999999999999716 ) ) ;
#8574 = CARTESIAN_POINT ( 'NONE',  ( -10.81189881249999907, -6.242252689847864744, -100.9687500020483810 ) ) ;
#8575 = VERTEX_POINT ( 'NONE', #41708 ) ;
#8576 = CARTESIAN_POINT ( 'NONE',  ( -4.999999999999996447, 8.660254037844387298, -65.99999999999997158 ) ) ;
#8577 = CARTESIAN_POINT ( 'NONE',  ( 7.644554776091147741E-16, 12.48450537969573659, -197.4687500020484094 ) ) ;
#8578 = CARTESIAN_POINT ( 'NONE',  ( -9.999999999999998224, 1.224646799147353059E-15, -79.62500000409677625 ) ) ;
#8579 = EDGE_CURVE ( 'NONE', #9067, #38736, #15254, .T. ) ;
#8580 = DIRECTION ( 'NONE',  ( -1.000000000000000000, 0.000000000000000000, 0.000000000000000000 ) ) ;
#8581 = CYLINDRICAL_SURFACE ( 'NONE', #24518, 9.999999999999998224 ) ;
#8582 = CARTESIAN_POINT ( 'NONE',  ( 10.81189881249999907, 6.242252689847868297, -95.90625000204839523 ) ) ;
#8583 = CARTESIAN_POINT ( 'NONE',  ( -10.81189881249999729, 1.324075727343319199E-15, -75.78125000204838102 ) ) ;
#8584 = CARTESIAN_POINT ( 'NONE',  ( 10.00000000000000000, 5.773502691896255534, -65.25000000409677625 ) ) ;
#8585 = CARTESIAN_POINT ( 'NONE',  ( -9.999999999999479527, -5.773502691896549521, -78.00000000409676204 ) ) ;
#8586 = CARTESIAN_POINT ( 'NONE',  ( 10.81189881249999551, -6.242252689847874514, -26.96875000204837391 ) ) ;
#8587 = CARTESIAN_POINT ( 'NONE',  ( -4.999999999999996447, 8.660254037844387298, -100.4999999999999858 ) ) ;
#8588 = CARTESIAN_POINT ( 'NONE',  ( -2.293366432827344421E-15, -12.48450537969573659, -196.9062500020484094 ) ) ;
#8589 = CARTESIAN_POINT ( 'NONE',  ( 5.405949406249992428, -9.363379034771808662, -19.78125000204836326 ) ) ;
#8590 = CARTESIAN_POINT ( 'NONE',  ( 10.81189881249999551, -6.242252689847874514, -5.968750002048344605 ) ) ;
#8591 = CARTESIAN_POINT ( 'NONE',  ( 9.999999999999998224, 0.000000000000000000, -117.8750000040967905 ) ) ;
#8592 = CARTESIAN_POINT ( 'NONE',  ( -10.81189881249999907, -6.242252689847864744, -144.4687500020484094 ) ) ;
#8593 = CARTESIAN_POINT ( 'NONE',  ( 9.999999999999998224, 0.000000000000000000, -192.5000000000000000 ) ) ;
#8594 = CARTESIAN_POINT ( 'NONE',  ( 9.999999999999612754, 5.773502691896477579, -152.2500000040967336 ) ) ;
#8595 = CARTESIAN_POINT ( 'NONE',  ( -5.000000000000003553, -8.660254037844383745, -179.5000000000000000 ) ) ;
#8596 = CARTESIAN_POINT ( 'NONE',  ( -9.999999999999998224, 1.224646799147353059E-15, -3.125000004096767370 ) ) ;
#8598 = EDGE_LOOP ( 'NONE', ( #39309, #11953, #27811, #40894 ) ) ;
#8597 = CARTESIAN_POINT ( 'NONE',  ( -5.405949406249996869, 9.363379034771805109, -100.0312500020483952 ) ) ;
#8599 = CARTESIAN_POINT ( 'NONE',  ( -5.000000000000003553, -8.660254037844383745, -164.5000000000000000 ) ) ;
#8600 = ORIENTED_EDGE ( 'NONE', *, *, #14833, .F. ) ;
#8601 =( BOUNDED_CURVE ( )  B_SPLINE_CURVE ( 2, ( #27138, #4048, #17192, #4263, #37270, #30810, #7932 ),
 .UNSPECIFIED., .F., .F. ) 
 B_SPLINE_CURVE_WITH_KNOTS ( ( 3, 2, 2, 3 ),
 ( 0.2164179104477612636, 0.2176616915422886489, 0.2189054726368160064, 0.2201492537313433639 ),
 .UNSPECIFIED. ) 
 CURVE ( )  GEOMETRIC_REPRESENTATION_ITEM ( )  RATIONAL_B_SPLINE_CURVE ( ( 0.9999999999999910072, 0.8660254037844477004, 1.000000000000000000, 0.8660254037844387076, 1.000000000000000000, 0.8660254037844297148, 1.000000000000008882 ) ) 
 REPRESENTATION_ITEM ( '' )  );
#8602 = ORIENTED_EDGE ( 'NONE', *, *, #16822, .F. ) ;
#8603 = CARTESIAN_POINT ( 'NONE',  ( 5.405949406249992428, -9.363379034771808662, -27.28125000204836681 ) ) ;
#8604 = DATE_AND_TIME ( #41379, #31130 ) ;
#8605 = EDGE_CURVE ( 'NONE', #42167, #10458, #9137, .T. ) ;
#8606 = CARTESIAN_POINT ( 'NONE',  ( -5.405949406249996869, 9.363379034771805109, -83.34375000204836681 ) ) ;
#8607 = DIRECTION ( 'NONE',  ( 1.000000000000000000, -3.469446951953614805E-17, 0.000000000000000000 ) ) ;
#8608 = CARTESIAN_POINT ( 'NONE',  ( 8.660254119780192994, -4.999999858083012505, -99.99999999999998579 ) ) ;
#8609 = CARTESIAN_POINT ( 'NONE',  ( 9.999999999999227285, 5.773502691896701400, -105.7500000040967620 ) ) ;
#8610 = CARTESIAN_POINT ( 'NONE',  ( 10.81189881249999729, 0.000000000000000000, -166.5312500020484094 ) ) ;
#8611 = CARTESIAN_POINT ( 'NONE',  ( -4.999999999999996447, 8.660254037844387298, -10.87500000409674605 ) ) ;
#8612 = CARTESIAN_POINT ( 'NONE',  ( -2.293366432827344421E-15, -12.48450537969573659, -117.2187500020483668 ) ) ;
#8613 = CARTESIAN_POINT ( 'NONE',  ( 10.81189881249999551, -6.242252689847874514, -86.96875000204838102 ) ) ;
#8614 = CARTESIAN_POINT ( 'NONE',  ( 10.81189881249999551, -6.242252689847874514, -6.156250002048360592 ) ) ;
#8615 = CARTESIAN_POINT ( 'NONE',  ( -10.81189881249999729, 6.242252689847871849, -195.7187500020484379 ) ) ;
#8616 = CARTESIAN_POINT ( 'NONE',  ( 10.81189881249999729, 0.000000000000000000, -96.03125000204838102 ) ) ;
#8617 = CARTESIAN_POINT ( 'NONE',  ( 9.999999999999996447, -5.773502691896262640, -178.0000000040967905 ) ) ;
#8618 = CARTESIAN_POINT ( 'NONE',  ( -5.405949406249996869, 9.363379034771805109, -167.5312500020484094 ) ) ;
#8619 = CARTESIAN_POINT ( 'NONE',  ( 7.070501591499376803E-16, 11.54700538379251284, -102.5000000040967905 ) ) ;
#8620 = CARTESIAN_POINT ( 'NONE',  ( -10.81189881249999729, 1.324075727343319199E-15, -174.7812500020484094 ) ) ;
#8621 = CARTESIAN_POINT ( 'NONE',  ( -10.81189881249999907, -6.242252689847864744, -185.1562500020484094 ) ) ;
#8622 = CARTESIAN_POINT ( 'NONE',  ( 7.644554776091147741E-16, 12.48450537969573659, -45.96875000204837391 ) ) ;
#8623 = CARTESIAN_POINT ( 'NONE',  ( -9.999999999999998224, 5.773502691896259087, -166.7500000040967905 ) ) ;
#8624 = CARTESIAN_POINT ( 'NONE',  ( 10.81189881249999907, 6.242252689847868297, -4.406250002048352599 ) ) ;
#8625 = CARTESIAN_POINT ( 'NONE',  ( 10.81189881249999551, -6.242252689847874514, -13.46875000204836503 ) ) ;
#8626 = CARTESIAN_POINT ( 'NONE',  ( 9.999999999999998224, 0.000000000000000000, -164.3750000040967905 ) ) ;
#8627 = CARTESIAN_POINT ( 'NONE',  ( 10.81189881249999551, -6.242252689847874514, -124.4687500020483952 ) ) ;
#8628 = CARTESIAN_POINT ( 'NONE',  ( 4.999999999999992006, -8.660254037844389075, -90.74999999999998579 ) ) ;
#8629 = CARTESIAN_POINT ( 'NONE',  ( 5.405949406249999534, 9.363379034771803333, -17.78125000204835970 ) ) ;
#8630 = CARTESIAN_POINT ( 'NONE',  ( -5.000000000000003553, -8.660254037844383745, -106.3750000040967763 ) ) ;
#8631 = FACE_OUTER_BOUND ( 'NONE', #20079, .T. ) ;
#8632 = CARTESIAN_POINT ( 'NONE',  ( 10.00000000000000000, 5.773502691896255534, -51.37499999999997868 ) ) ;
#8633 = CARTESIAN_POINT ( 'NONE',  ( -10.81189881249999907, -6.242252689847864744, -116.1562500020483952 ) ) ;
#8634 = CARTESIAN_POINT ( 'NONE',  ( -10.81189881249999729, 6.242252689847871849, -99.90625000204839523 ) ) ;
#8635 = ORIENTED_EDGE ( 'NONE', *, *, #17172, .T. ) ;
#8636 = AXIS2_PLACEMENT_3D ( 'NONE', #38260, #38689, #15578 ) ;
#8637 = CARTESIAN_POINT ( 'NONE',  ( -10.00000000000000000, -5.773502691896251982, -94.50000000409677625 ) ) ;
#8638 = CARTESIAN_POINT ( 'NONE',  ( -4.999999999999996447, 8.660254037844387298, -28.87500000409676204 ) ) ;
#8639 = CARTESIAN_POINT ( 'NONE',  ( -10.81189881249999729, 6.242252689847871849, -155.4062500020483810 ) ) ;
#8640 = CARTESIAN_POINT ( 'NONE',  ( 5.405949406249992428, -9.363379034771808662, -49.59375000204838102 ) ) ;
#8641 = ORIENTED_EDGE ( 'NONE', *, *, #56, .F. ) ;
#8642 = CARTESIAN_POINT ( 'NONE',  ( 10.00000000000000000, 5.773502691896255534, -27.37499999999998579 ) ) ;
#8643 = CARTESIAN_POINT ( 'NONE',  ( -5.405949406249996869, 9.363379034771805109, -29.53125000204837036 ) ) ;
#8644 = CARTESIAN_POINT ( 'NONE',  ( -5.000000000000003553, -8.660254037844383745, -157.0000000000000000 ) ) ;
#8645 = CARTESIAN_POINT ( 'NONE',  ( -5.000000000000003553, -8.660254037844383745, -20.87500000409675494 ) ) ;
#8646 =( BOUNDED_CURVE ( )  B_SPLINE_CURVE ( 2, ( #15464, #22177, #35349, #29714, #16299, #32736, #32949 ),
 .UNSPECIFIED., .F., .F. ) 
 B_SPLINE_CURVE_WITH_KNOTS ( ( 3, 2, 2, 3 ),
 ( 0.6753731343283584376, 0.6766169154228858229, 0.6778606965174133192, 0.6791044776119405935 ),
 .UNSPECIFIED. ) 
 CURVE ( )  GEOMETRIC_REPRESENTATION_ITEM ( )  RATIONAL_B_SPLINE_CURVE ( ( 0.9999999999999761302, 0.8660254037844625774, 1.000000000000000000, 0.8660254037844387076, 1.000000000000000000, 0.8660254037844028474, 1.000000000000035971 ) ) 
 REPRESENTATION_ITEM ( '' )  );
#8647 = CARTESIAN_POINT ( 'NONE',  ( 10.00000000000051159, -5.773502691895965988, -80.50000000409674783 ) ) ;
#8648 = CARTESIAN_POINT ( 'NONE',  ( -10.81189881249999907, -6.242252689847864744, -122.1562500020484094 ) ) ;
#8649 = CARTESIAN_POINT ( 'NONE',  ( -10.00000000000076916, 5.773502691895813221, -110.8749999999999574 ) ) ;
#8650 = DIRECTION ( 'NONE',  ( -0.000000000000000000, -0.000000000000000000, -1.000000000000000000 ) ) ;
#8651 = AXIS2_PLACEMENT_3D ( 'NONE', #22061, #28761, #29379 ) ;
#8652 = ORIENTED_EDGE ( 'NONE', *, *, #25059, .T. ) ;
#8653 =( BOUNDED_CURVE ( )  B_SPLINE_CURVE ( 2, ( #7160, #10594, #20106, #35886, #19468, #32653, #42550 ),
 .UNSPECIFIED., .F., .F. ) 
 B_SPLINE_CURVE_WITH_KNOTS ( ( 3, 2, 2, 3 ),
 ( 0.3992537313432836799, 0.4004975124378110651, 0.4017412935323383949, 0.4029850746268657802 ),
 .UNSPECIFIED. ) 
 CURVE ( )  GEOMETRIC_REPRESENTATION_ITEM ( )  RATIONAL_B_SPLINE_CURVE ( ( 0.9999999999999880096, 0.8660254037844506980, 1.000000000000000000, 0.8660254037844387076, 1.000000000000000000, 0.8660254037844267172, 1.000000000000011990 ) ) 
 REPRESENTATION_ITEM ( '' )  );
#8654 = CARTESIAN_POINT ( 'NONE',  ( 10.81189881249999729, 0.000000000000000000, -63.03125000204837391 ) ) ;
#8655 = DATE_AND_TIME ( #8226, #20725 ) ;
#8656 = EDGE_CURVE ( 'NONE', #27948, #6661, #16624, .T. ) ;
#8657 = CARTESIAN_POINT ( 'NONE',  ( -5.405949406250003975, -9.363379034771801557, -108.3437500020483810 ) ) ;
#8659 = ORIENTED_EDGE ( 'NONE', *, *, #39837, .T. ) ;
#8658 = VERTEX_POINT ( 'NONE', #8718 ) ;
#8660 = DIRECTION ( 'NONE',  ( -0.000000000000000000, -0.000000000000000000, -1.000000000000000000 ) ) ;
#8661 = CARTESIAN_POINT ( 'NONE',  ( 10.81189881249999551, -6.242252689847874514, -157.4687500020484094 ) ) ;
#8662 = CARTESIAN_POINT ( 'NONE',  ( -10.81189881249999907, -6.242252689847864744, -188.1562500020484094 ) ) ;
#8663 = CARTESIAN_POINT ( 'NONE',  ( 5.405949406249999534, 9.363379034771803333, -5.593750002048370362 ) ) ;
#8664 = CARTESIAN_POINT ( 'NONE',  ( 10.81189881249999729, 6.242252689847867408, -136.2187500020483810 ) ) ;
#8665 = CARTESIAN_POINT ( 'NONE',  ( -10.81189881249999907, -6.242252689847864744, -108.4687500020483810 ) ) ;
#8666 = CARTESIAN_POINT ( 'NONE',  ( -4.999999999999996447, 8.660254037844387298, -55.49999999999996447 ) ) ;
#8667 = CARTESIAN_POINT ( 'NONE',  ( 5.405949406249999534, 9.363379034771803333, -119.7812500020483952 ) ) ;
#8668 = CARTESIAN_POINT ( 'NONE',  ( 5.405949406249992428, -9.363379034771808662, -0.09375000204836503315 ) ) ;
#8670 = EDGE_CURVE ( 'NONE', #23066, #10458, #3420, .T. ) ;
#8669 = CARTESIAN_POINT ( 'NONE',  ( -5.405949406249996869, 9.363379034771805109, -125.3437500020483952 ) ) ;
#8671 = CARTESIAN_POINT ( 'NONE',  ( 10.81189881249999551, -6.242252689847874514, -190.6562500020484094 ) ) ;
#8672 = CARTESIAN_POINT ( 'NONE',  ( -4.999999999999996447, 8.660254037844387298, -157.5000000000000000 ) ) ;
#8673 = CARTESIAN_POINT ( 'NONE',  ( 7.070501591499377789E-16, 11.54700538379251284, -145.6250000000000284 ) ) ;
#8674 = CARTESIAN_POINT ( 'NONE',  ( -9.999999999999998224, 5.773502691896259087, -8.874999999999966249 ) ) ;
#8675 = CARTESIAN_POINT ( 'NONE',  ( 10.81189881249999551, -6.242252689847874514, -64.46875000204838102 ) ) ;
#8676 = CARTESIAN_POINT ( 'NONE',  ( 10.81189881249999729, 0.000000000000000000, -55.34375000204835970 ) ) ;
#8677 = CARTESIAN_POINT ( 'NONE',  ( -4.999999999999996447, 8.660254037844387298, -184.8750000040967905 ) ) ;
#8678 = CARTESIAN_POINT ( 'NONE',  ( -2.293366432827344421E-15, -12.48450537969573659, -27.40625000204838102 ) ) ;
#8679 = CARTESIAN_POINT ( 'NONE',  ( 10.81189881249999551, -6.242252689847874514, -40.46875000204835970 ) ) ;
#8680 = CARTESIAN_POINT ( 'NONE',  ( 10.00000000000025402, -5.773502691896113426, -163.0000000040967905 ) ) ;
#8681 = CARTESIAN_POINT ( 'NONE',  ( -10.81189881249999907, -6.242252689847864744, -142.9687500020484094 ) ) ;
#8682 = CARTESIAN_POINT ( 'NONE',  ( -9.999999999999998224, 1.224646799147353059E-15, -115.2499999999999858 ) ) ;
#8683 = CARTESIAN_POINT ( 'NONE',  ( 9.999999999999998224, 0.000000000000000000, -82.99999999999997158 ) ) ;
#8684 = CIRCLE ( 'NONE', #26592, 45.00000000000000711 ) ;
#8685 = CARTESIAN_POINT ( 'NONE',  ( 9.999999999999996447, -5.773502691896262640, -72.62499999999995737 ) ) ;
#8686 = CARTESIAN_POINT ( 'NONE',  ( 10.81189881249999551, -6.242252689847874514, -138.1562500020484094 ) ) ;
#8687 = CARTESIAN_POINT ( 'NONE',  ( -5.405949406249996869, 9.363379034771805109, -13.03125000204835615 ) ) ;
#8688 = ORIENTED_EDGE ( 'NONE', *, *, #8000, .F. ) ;
#8689 = CIRCLE ( 'NONE', #432, 10.00000000000000178 ) ;
#8690 = CARTESIAN_POINT ( 'NONE',  ( 7.070501591499377789E-16, 11.54700538379251284, -113.0000000040967905 ) ) ;
#8691 = CARTESIAN_POINT ( 'NONE',  ( -2.121150477449813534E-15, -11.54700538379251284, -86.75000000409677625 ) ) ;
#8692 = CARTESIAN_POINT ( 'NONE',  ( 10.81189881249999729, 0.000000000000000000, -76.34375000204838102 ) ) ;
#8693 = CARTESIAN_POINT ( 'NONE',  ( -9.999999999999998224, 5.773502691896259087, -47.87499999999996447 ) ) ;
#8694 = CARTESIAN_POINT ( 'NONE',  ( 9.999999999999998224, 0.000000000000000000, -29.37500000409676204 ) ) ;
#8695 = CIRCLE ( 'NONE', #1815, 14.99999999999998579 ) ;
#8696 = CARTESIAN_POINT ( 'NONE',  ( 9.999999999999998224, 0.000000000000000000, -75.49999999999998579 ) ) ;
#8697 = CARTESIAN_POINT ( 'NONE',  ( 7.644554776091147741E-16, 12.48450537969573659, -41.65625000204837391 ) ) ;
#8698 = DIRECTION ( 'NONE',  ( -0.000000000000000000, -0.000000000000000000, 1.000000000000000000 ) ) ;
#8699 = CARTESIAN_POINT ( 'NONE',  ( -10.81189881249999729, 6.242252689847871849, -146.4062500020484094 ) ) ;
#8700 = CARTESIAN_POINT ( 'NONE',  ( 10.81189881249999729, 0.000000000000000000, -124.3437500020483952 ) ) ;
#8701 = DIRECTION ( 'NONE',  ( -0.000000000000000000, -0.000000000000000000, 1.000000000000000000 ) ) ;
#8702 = CARTESIAN_POINT ( 'NONE',  ( 10.00000000000051159, -5.773502691895965988, -120.6250000000000000 ) ) ;
#8703 = ORIENTED_EDGE ( 'NONE', *, *, #4732, .T. ) ;
#8704 = EDGE_CURVE ( 'NONE', #14015, #36368, #6684, .T. ) ;
#8705 = ORIENTED_EDGE ( 'NONE', *, *, #26212, .T. ) ;
#8706 = ORIENTED_EDGE ( 'NONE', *, *, #5846, .T. ) ;
#8707 = CARTESIAN_POINT ( 'NONE',  ( -9.999999999999998224, 1.224646799147353059E-15, -40.24999999999997868 ) ) ;
#8708 = CARTESIAN_POINT ( 'NONE',  ( -2.293366432827344421E-15, -12.48450537969573659, -178.7187500020484094 ) ) ;
#8709 = CARTESIAN_POINT ( 'NONE',  ( 5.405949406249999534, 9.363379034771803333, -29.59375000204836326 ) ) ;
#8710 = LINE ( 'NONE', #37841, #12941 ) ;
#8711 = CARTESIAN_POINT ( 'NONE',  ( 10.81189881249999729, 6.242252689847867408, -167.7187500020483526 ) ) ;
#8712 = CARTESIAN_POINT ( 'NONE',  ( -10.81189881249999729, 6.242252689847871849, -155.2187500020483810 ) ) ;
#8713 = CARTESIAN_POINT ( 'NONE',  ( 0.000000000000000000, 0.000000000000000000, -200.0000000000000000 ) ) ;
#8714 = CARTESIAN_POINT ( 'NONE',  ( -2.293366432827344421E-15, -12.48450537969573659, -135.2187500020483810 ) ) ;
#8715 = CARTESIAN_POINT ( 'NONE',  ( -5.405949406249996869, 9.363379034771805109, -142.0312500020483810 ) ) ;
#8716 = CARTESIAN_POINT ( 'NONE',  ( -5.405949406249996869, 9.363379034771805109, -149.3437500020483810 ) ) ;
#8717 = CYLINDRICAL_SURFACE ( 'NONE', #17785, 9.999999999999998224 ) ;
#8718 = CARTESIAN_POINT ( 'NONE',  ( 9.999999999999998224, 0.000000000000000000, -81.49999999999998579 ) ) ;
#8719 = CARTESIAN_POINT ( 'NONE',  ( 10.00000000000000000, 5.773502691896255534, -174.3750000000000000 ) ) ;
#8720 = CARTESIAN_POINT ( 'NONE',  ( -10.81189881249999729, 1.324075727343319199E-15, -78.59375000204838102 ) ) ;
#8721 = CYLINDRICAL_SURFACE ( 'NONE', #38268, 9.999999999999998224 ) ;
#8722 = CARTESIAN_POINT ( 'NONE',  ( 10.81189881249999729, 0.000000000000000000, -48.03125000204838813 ) ) ;
#8723 = CARTESIAN_POINT ( 'NONE',  ( -9.999999999999998224, 1.224646799147353059E-15, -133.2499999999999716 ) ) ;
#8724 = EDGE_CURVE ( 'NONE', #22389, #12029, #26177, .T. ) ;
#8725 = CARTESIAN_POINT ( 'NONE',  ( -10.81189881249999729, 6.242252689847871849, -167.2187500020483810 ) ) ;
#8726 = CARTESIAN_POINT ( 'NONE',  ( -5.405949406249996869, 9.363379034771805109, -112.0312500020483810 ) ) ;
#8727 = CARTESIAN_POINT ( 'NONE',  ( -5.405949406249996869, 9.363379034771805109, -143.5312500020483810 ) ) ;
#8728 = CARTESIAN_POINT ( 'NONE',  ( -9.999999999999998224, 1.224646799147353059E-15, -195.1250000040967905 ) ) ;
#8729 = CARTESIAN_POINT ( 'NONE',  ( 7.644554776091147741E-16, 12.48450537969573659, -47.65625000204837391 ) ) ;
#8730 = CARTESIAN_POINT ( 'NONE',  ( 9.999999999999996447, -5.773502691896262640, -125.5000000040967763 ) ) ;
#8731 = CARTESIAN_POINT ( 'NONE',  ( 9.999999999999996447, -5.773502691896262640, -99.62500000000000000 ) ) ;
#8732 = ORIENTED_EDGE ( 'NONE', *, *, #6620, .T. ) ;
#8733 = CARTESIAN_POINT ( 'NONE',  ( -10.81189881249999729, -6.242252689847864744, -128.1562500020483810 ) ) ;
#8734 = CARTESIAN_POINT ( 'NONE',  ( -10.00000000000000000, -5.773502691896251982, -142.5000000040967905 ) ) ;
#8735 = LINE ( 'NONE', #24720, #28468 ) ;
#8736 = CARTESIAN_POINT ( 'NONE',  ( -5.405949406250003975, -9.363379034771801557, -183.5312500020484094 ) ) ;
#8737 = ORIENTED_EDGE ( 'NONE', *, *, #22756, .T. ) ;
#8738 = CARTESIAN_POINT ( 'NONE',  ( -5.405949406249996869, 9.363379034771805109, -173.3437500020484094 ) ) ;
#8739 = CARTESIAN_POINT ( 'NONE',  ( -10.00000000000000000, -5.773502691896251982, -46.50000000409676915 ) ) ;
#8740 = CARTESIAN_POINT ( 'NONE',  ( 0.000000000000000000, 0.000000000000000000, -200.0000000000000000 ) ) ;
#8741 = CARTESIAN_POINT ( 'NONE',  ( 10.81189881249999729, 0.000000000000000000, -72.03125000204838102 ) ) ;
#8742 = CARTESIAN_POINT ( 'NONE',  ( -9.999999999999998224, 5.773502691896259087, -42.25000000409676204 ) ) ;
#8743 = DIRECTION ( 'NONE',  ( -0.000000000000000000, -0.000000000000000000, -1.000000000000000000 ) ) ;
#8744 = CARTESIAN_POINT ( 'NONE',  ( -10.81189881249999729, 1.324075727343319199E-15, -167.2812500020484094 ) ) ;
#8745 = CARTESIAN_POINT ( 'NONE',  ( -9.999999999999998224, 1.224646799147353059E-15, -1.625000004096766038 ) ) ;
#8746 = ORIENTED_EDGE ( 'NONE', *, *, #40574, .T. ) ;
#8747 = FACE_OUTER_BOUND ( 'NONE', #12503, .T. ) ;
#8748 = CARTESIAN_POINT ( 'NONE',  ( -11.54700538379251817, 20.00000000000000355, 49.99999999999998579 ) ) ;
#8749 = CARTESIAN_POINT ( 'NONE',  ( -4.999999999999996447, 8.660254037844387298, -136.8750000040967905 ) ) ;
#8751 = ORIENTED_EDGE ( 'NONE', *, *, #30651, .F. ) ;
#8750 = CARTESIAN_POINT ( 'NONE',  ( -5.405949406250003975, -9.363379034771801557, -81.53125000204839523 ) ) ;
#8752 = EDGE_LOOP ( 'NONE', ( #18216, #6519, #15813, #40254 ) ) ;
#8753 = ORIENTED_EDGE ( 'NONE', *, *, #34357, .T. ) ;
#8754 =( BOUNDED_CURVE ( )  B_SPLINE_CURVE ( 2, ( #37291, #30620, #33646, #26524, #4069, #13963, #29771 ),
 .UNSPECIFIED., .F., .F. ) 
 B_SPLINE_CURVE_WITH_KNOTS ( ( 3, 2, 2, 3 ),
 ( 0.07089552238805976736, 0.07213930348258713876, 0.07338308457711449628, 0.07462686567164185381 ),
 .UNSPECIFIED. ) 
 CURVE ( )  GEOMETRIC_REPRESENTATION_ITEM ( )  RATIONAL_B_SPLINE_CURVE ( ( 0.9999999999999925615, 0.8660254037844461461, 1.000000000000000000, 0.8660254037844387076, 1.000000000000000000, 0.8660254037844312691, 1.000000000000007550 ) ) 
 REPRESENTATION_ITEM ( '' )  );
#8755 = CARTESIAN_POINT ( 'NONE',  ( 10.81189881249999729, 0.000000000000000000, -31.34375000204836681 ) ) ;
#8756 = CARTESIAN_POINT ( 'NONE',  ( 0.000000000000000000, 0.000000000000000000, -217.0000000000000853 ) ) ;
#8757 = CARTESIAN_POINT ( 'NONE',  ( -5.405949406250003975, -9.363379034771801557, -3.531250002048374803 ) ) ;
#8759 = ORIENTED_EDGE ( 'NONE', *, *, #37817, .F. ) ;
#8758 = CARTESIAN_POINT ( 'NONE',  ( -5.405949406250003975, -9.363379034771801557, -52.84375000204835970 ) ) ;
#8760 = CARTESIAN_POINT ( 'NONE',  ( 9.999999999999998224, 0.000000000000000000, -3.499999999999975131 ) ) ;
#8761 = CARTESIAN_POINT ( 'NONE',  ( 10.00000000000000000, 5.773502691896255534, -36.37499999999996447 ) ) ;
#8762 = CARTESIAN_POINT ( 'NONE',  ( -2.293366432827344421E-15, -12.48450537969573659, -184.7187500020484094 ) ) ;
#8763 = CARTESIAN_POINT ( 'NONE',  ( -10.81189881249999729, 6.242252689847871849, -177.7187500020483810 ) ) ;
#8764 = CARTESIAN_POINT ( 'NONE',  ( -2.293366432827344421E-15, -12.48450537969573659, -159.2187500020483810 ) ) ;
#8765 = CARTESIAN_POINT ( 'NONE',  ( 5.405949406249992428, -9.363379034771808662, -171.0937500020484094 ) ) ;
#8766 = FACE_OUTER_BOUND ( 'NONE', #7099, .T. ) ;
#8767 = CARTESIAN_POINT ( 'NONE',  ( 9.999999999999998224, 0.000000000000000000, -132.5000000000000000 ) ) ;
#8768 = CARTESIAN_POINT ( 'NONE',  ( 10.00000000000000000, 5.773502691896255534, -195.3750000000000284 ) ) ;
#8769 = CARTESIAN_POINT ( 'NONE',  ( 5.405949406249992428, -9.363379034771808662, -102.0937500020483810 ) ) ;
#8770 = CARTESIAN_POINT ( 'NONE',  ( 0.000000000000000000, 0.000000000000000000, -200.0000000000000000 ) ) ;
#8771 = CARTESIAN_POINT ( 'NONE',  ( 10.81189881249999729, 0.000000000000000000, -79.53125000204838102 ) ) ;
#8772 = EDGE_CURVE ( 'NONE', #21146, #4172, #25761, .T. ) ;
#8773 = CARTESIAN_POINT ( 'NONE',  ( -5.405949406249996869, 9.363379034771805109, -95.34375000204838102 ) ) ;
#8774 = ADVANCED_FACE ( 'NONE', ( #19684 ), #3727, .T. ) ;
#8775 = CARTESIAN_POINT ( 'NONE',  ( -5.405949406249996869, 9.363379034771805109, -71.53125000204838102 ) ) ;
#8776 = CARTESIAN_POINT ( 'NONE',  ( 7.070501591499377789E-16, 11.54700538379251284, -149.0000000040968189 ) ) ;
#8777 = CARTESIAN_POINT ( 'NONE',  ( 5.000000000000000000, 8.660254037844385522, -123.2500000000000000 ) ) ;
#8778 = CARTESIAN_POINT ( 'NONE',  ( 10.81189881249999729, 0.000000000000000000, -151.5312500020484094 ) ) ;
#8779 = CARTESIAN_POINT ( 'NONE',  ( 7.644554776091147741E-16, 12.48450537969573659, -166.1562500020483810 ) ) ;
#8780 = CARTESIAN_POINT ( 'NONE',  ( 9.999999999999479527, 5.773502691896553074, -98.25000000409676204 ) ) ;
#8781 = CARTESIAN_POINT ( 'NONE',  ( 0.000000000000000000, 0.000000000000000000, -200.0000000000000000 ) ) ;
#8782 = CARTESIAN_POINT ( 'NONE',  ( 5.405949406249992428, -9.363379034771808662, -96.09375000204838102 ) ) ;
#8783 = EDGE_LOOP ( 'NONE', ( #25068, #30998, #1304, #11437 ) ) ;
#8784 = CARTESIAN_POINT ( 'NONE',  ( 7.070501591499377789E-16, 11.54700538379251284, -63.12499999999997158 ) ) ;
#8785 = CARTESIAN_POINT ( 'NONE',  ( 7.644554776091147741E-16, 12.48450537969573659, -195.9687500020484094 ) ) ;
#8786 = CARTESIAN_POINT ( 'NONE',  ( 9.999999999999996447, -5.773502691896262640, -73.00000000409676204 ) ) ;
#8787 = CARTESIAN_POINT ( 'NONE',  ( -9.999999999999998224, 1.224646799147353059E-15, -175.6250000040968189 ) ) ;
#8788 = CARTESIAN_POINT ( 'NONE',  ( 5.405949406249999534, 9.363379034771803333, -89.78125000204838102 ) ) ;
#8789 = CARTESIAN_POINT ( 'NONE',  ( -5.405949406250003975, -9.363379034771801557, -75.53125000204838102 ) ) ;
#8790 = CARTESIAN_POINT ( 'NONE',  ( 9.999999999999996447, -5.773502691896262640, -68.50000000409677625 ) ) ;
#8791 = DIRECTION ( 'NONE',  ( -0.000000000000000000, -0.000000000000000000, -1.000000000000000000 ) ) ;
#8792 = CARTESIAN_POINT ( 'NONE',  ( -5.405949406250003975, -9.363379034771801557, -27.34375000204835970 ) ) ;
#8793 = ORIENTED_EDGE ( 'NONE', *, *, #40131, .T. ) ;
#8794 = CARTESIAN_POINT ( 'NONE',  ( 10.81189881249999907, 6.242252689847868297, -193.4062500020484094 ) ) ;
#8795 = CARTESIAN_POINT ( 'NONE',  ( -2.293366432827344421E-15, -12.48450537969573659, -16.90625000204837391 ) ) ;
#8796 = CARTESIAN_POINT ( 'NONE',  ( -5.405949406250003975, -9.363379034771801557, -3.343750002048367698 ) ) ;
#8797 = CARTESIAN_POINT ( 'NONE',  ( 0.000000000000000000, 0.000000000000000000, -200.0000000000000000 ) ) ;
#8798 = EDGE_CURVE ( 'NONE', #15872, #4341, #6743, .T. ) ;
#8799 = CARTESIAN_POINT ( 'NONE',  ( 4.999999999999992006, -8.660254037844389075, -107.6250000040967763 ) ) ;
#8800 = LINE ( 'NONE', #38790, #30059 ) ;
#8801 = CARTESIAN_POINT ( 'NONE',  ( 9.999999999999998224, 0.000000000000000000, -173.0000000000000284 ) ) ;
#8802 = CARTESIAN_POINT ( 'NONE',  ( 9.999999999999998224, 0.000000000000000000, -176.3750000040967905 ) ) ;
#8804 = ORIENTED_EDGE ( 'NONE', *, *, #36914, .T. ) ;
#8803 = CARTESIAN_POINT ( 'NONE',  ( 10.81189881249999551, -6.242252689847874514, -103.6562500020483668 ) ) ;
#8805 = CARTESIAN_POINT ( 'NONE',  ( 7.070501591499376803E-16, 11.54700538379251284, -170.0000000040967905 ) ) ;
#8806 = EDGE_CURVE ( 'NONE', #38258, #25635, #22963, .T. ) ;
#8807 = ORIENTED_EDGE ( 'NONE', *, *, #31113, .T. ) ;
#8808 = EDGE_LOOP ( 'NONE', ( #13232, #15418, #36641, #23217 ) ) ;
#8809 = CARTESIAN_POINT ( 'NONE',  ( 10.81189881249999907, 6.242252689847868297, -28.40625000204838813 ) ) ;
#8810 = APPROVAL_DATE_TIME ( #9021, #5371 ) ;
#8811 = CARTESIAN_POINT ( 'NONE',  ( -10.81189881249999907, -6.242252689847864744, -81.46875000204838102 ) ) ;
#8812 = FACE_OUTER_BOUND ( 'NONE', #15212, .T. ) ;
#8813 = CIRCLE ( 'NONE', #35678, 35.00000000000000711 ) ;
#8814 = VECTOR ( 'NONE', #4454, 1000.000000000000000 ) ;
#8815 = CARTESIAN_POINT ( 'NONE',  ( 10.81189881249999729, 0.000000000000000000, -199.3437500020484094 ) ) ;
#8816 = CARTESIAN_POINT ( 'NONE',  ( -5.000000000000003553, -8.660254037844383745, -127.3750000040967905 ) ) ;
#8817 = CARTESIAN_POINT ( 'NONE',  ( 7.644554776091147741E-16, 12.48450537969573659, -164.6562500020484094 ) ) ;
#8818 = CARTESIAN_POINT ( 'NONE',  ( 5.000000000000000000, 8.660254037844385522, -12.62500000409674783 ) ) ;
#8819 = DIRECTION ( 'NONE',  ( -0.000000000000000000, -0.000000000000000000, 1.000000000000000000 ) ) ;
#8820 = CARTESIAN_POINT ( 'NONE',  ( 10.81189881249999729, 0.000000000000000000, -127.3437500020483952 ) ) ;
#8821 = EDGE_CURVE ( 'NONE', #15268, #12639, #21051, .T. ) ;
#8822 = CARTESIAN_POINT ( 'NONE',  ( -5.405949406249996869, 9.363379034771805109, -119.3437500020483810 ) ) ;
#8823 = CARTESIAN_POINT ( 'NONE',  ( -2.293366432827344421E-15, -12.48450537969573659, -85.71875000204838102 ) ) ;
#8824 = CARTESIAN_POINT ( 'NONE',  ( -2.293366432827344421E-15, -12.48450537969573659, -193.7187500020484094 ) ) ;
#8825 = CARTESIAN_POINT ( 'NONE',  ( 7.644554776091147741E-16, 12.48450537969573659, -89.65625000204839523 ) ) ;
#8826 = CARTESIAN_POINT ( 'NONE',  ( 5.000000000000000000, 8.660254037844385522, -173.1250000040968189 ) ) ;
#8827 = CARTESIAN_POINT ( 'NONE',  ( -5.405949406250003975, -9.363379034771801557, -168.5312500020484094 ) ) ;
#8828 = EDGE_CURVE ( 'NONE', #14871, #4606, #8346, .T. ) ;
#8829 = CARTESIAN_POINT ( 'NONE',  ( 9.999999999999998224, 0.000000000000000000, -102.8750000040967763 ) ) ;
#8830 = CARTESIAN_POINT ( 'NONE',  ( -10.81189881249999729, 1.324075727343319199E-15, -171.7812500020484094 ) ) ;
#8831 = CARTESIAN_POINT ( 'NONE',  ( -5.405949406250003975, -9.363379034771801557, -191.0312500020484094 ) ) ;
#8832 = CARTESIAN_POINT ( 'NONE',  ( 10.81189881249999729, 6.242252689847867408, -41.71875000204835260 ) ) ;
#8833 = ADVANCED_FACE ( 'NONE', ( #3300 ), #26387, .T. ) ;
#8834 = CARTESIAN_POINT ( 'NONE',  ( -10.00000000000000000, -5.773502691896251982, -168.0000000040967905 ) ) ;
#8835 = CARTESIAN_POINT ( 'NONE',  ( 10.81189881249999907, 6.242252689847868297, -1.406250002048370584 ) ) ;
#8836 = CARTESIAN_POINT ( 'NONE',  ( -10.81189881249999729, 1.324075727343319199E-15, -11.09375000204834727 ) ) ;
#8837 = CARTESIAN_POINT ( 'NONE',  ( 0.000000000000000000, 0.000000000000000000, -99.99999999999998579 ) ) ;
#8838 = CARTESIAN_POINT ( 'NONE',  ( 5.405949406249992428, -9.363379034771808662, -124.5937500020483952 ) ) ;
#8839 = CARTESIAN_POINT ( 'NONE',  ( 10.00000000000000000, 5.773502691896255534, -90.37499999999998579 ) ) ;
#8840 = CARTESIAN_POINT ( 'NONE',  ( 7.644554776091147741E-16, 12.48450537969573659, -23.65625000204838102 ) ) ;
#8841 = CARTESIAN_POINT ( 'NONE',  ( 9.999999999999996447, -5.773502691896262640, -103.0000000040967620 ) ) ;
#8842 = CARTESIAN_POINT ( 'NONE',  ( -5.000000000000003553, -8.660254037844383745, -149.8750000040967905 ) ) ;
#8843 = CARTESIAN_POINT ( 'NONE',  ( 10.81189881249999729, 0.000000000000000000, -120.0312500020483952 ) ) ;
#8844 = CARTESIAN_POINT ( 'NONE',  ( 5.405949406249992428, -9.363379034771808662, -97.78125000204839523 ) ) ;
#8845 = ORIENTED_EDGE ( 'NONE', *, *, #35327, .F. ) ;
#8846 = CARTESIAN_POINT ( 'NONE',  ( 7.070501591499377789E-16, 11.54700538379251284, -95.00000000409677625 ) ) ;
#8847 = CARTESIAN_POINT ( 'NONE',  ( -9.999999999999998224, 1.224646799147353059E-15, -134.7499999999999716 ) ) ;
#8848 = CARTESIAN_POINT ( 'NONE',  ( 5.405949406249992428, -9.363379034771808662, -159.2812500020484094 ) ) ;
#8849 = CARTESIAN_POINT ( 'NONE',  ( -5.405949406250003975, -9.363379034771801557, -48.34375000204838102 ) ) ;
#8850 = VERTEX_POINT ( 'NONE', #36098 ) ;
#8851 = CARTESIAN_POINT ( 'NONE',  ( -5.000000000000003553, -8.660254037844383745, -15.99999999999995914 ) ) ;
#8852 = CARTESIAN_POINT ( 'NONE',  ( 5.405949406249992428, -9.363379034771808662, -27.28125000204836681 ) ) ;
#8853 = CARTESIAN_POINT ( 'NONE',  ( 10.00000000000000000, 5.773502691896255534, -151.8750000000000000 ) ) ;
#8854 = VECTOR ( 'NONE', #7008, 1000.000000000000000 ) ;
#8855 =( BOUNDED_CURVE ( )  B_SPLINE_CURVE ( 2, ( #14804, #17404, #17834, #40489, #34484, #24128, #4906 ),
 .UNSPECIFIED., .F., .F. ) 
 B_SPLINE_CURVE_WITH_KNOTS ( ( 3, 2, 2, 3 ),
 ( 0.9402985074626868389, 0.9415422885572141132, 0.9427860696517416095, 0.9440298507462689948 ),
 .UNSPECIFIED. ) 
 CURVE ( )  GEOMETRIC_REPRESENTATION_ITEM ( )  RATIONAL_B_SPLINE_CURVE ( ( 0.9999999999999761302, 0.8660254037844625774, 1.000000000000000000, 0.8660254037844387076, 1.000000000000000000, 0.8660254037844028474, 1.000000000000035971 ) ) 
 REPRESENTATION_ITEM ( '' )  );
#8856 = CARTESIAN_POINT ( 'NONE',  ( -9.999999999999998224, 1.224646799147353059E-15, -16.62500000409675138 ) ) ;
#8857 = EDGE_CURVE ( 'NONE', #30728, #33393, #2044, .T. ) ;
#8858 = CARTESIAN_POINT ( 'NONE',  ( 9.999999999999996447, -5.773502691896262640, -195.6250000000000284 ) ) ;
#8860 = ORIENTED_EDGE ( 'NONE', *, *, #30592, .F. ) ;
#8859 = CARTESIAN_POINT ( 'NONE',  ( 5.405949406249999534, 9.363379034771803333, -128.7812500020483810 ) ) ;
#8861 = CARTESIAN_POINT ( 'NONE',  ( 4.999999999999992006, -8.660254037844389075, -188.2500000000000000 ) ) ;
#8862 = ORIENTED_EDGE ( 'NONE', *, *, #31488, .T. ) ;
#8863 = CARTESIAN_POINT ( 'NONE',  ( -5.405949406250003975, -9.363379034771801557, -56.03125000204836681 ) ) ;
#8864 = APPROVAL_ROLE ( '' ) ;
#8865 = CARTESIAN_POINT ( 'NONE',  ( -5.405949406249996869, 9.363379034771805109, -107.3437500020483810 ) ) ;
#8867 = ORIENTED_EDGE ( 'NONE', *, *, #30852, .F. ) ;
#8866 = ORIENTED_EDGE ( 'NONE', *, *, #28211, .T. ) ;
#8868 = CYLINDRICAL_SURFACE ( 'NONE', #16246, 9.999999999999998224 ) ;
#8869 = CARTESIAN_POINT ( 'NONE',  ( -9.999999999999998224, 1.224646799147353059E-15, -164.7500000000000000 ) ) ;
#8870 = CARTESIAN_POINT ( 'NONE',  ( 5.405949406249992428, -9.363379034771808662, -159.0937500020484094 ) ) ;
#8871 = CARTESIAN_POINT ( 'NONE',  ( 10.81189881249999551, -6.242252689847874514, -192.1562500020484094 ) ) ;
#8872 = CARTESIAN_POINT ( 'NONE',  ( 10.81189881249999729, 0.000000000000000000, -5.843750002048370362 ) ) ;
#8873 = CARTESIAN_POINT ( 'NONE',  ( -2.293366432827344421E-15, -12.48450537969573659, -142.7187500020483810 ) ) ;
#8874 = VECTOR ( 'NONE', #39498, 1000.000000000000000 ) ;
#8875 = PERSON ( 'NAUO-PER4', 'UNSPECIFIED', 'UNSPECIFIED', ('UNSPECIFIED'), ('UNSPECIFIED'), ('UNSPECIFIED') ) ;
#8876 = CARTESIAN_POINT ( 'NONE',  ( 10.81189881249999907, 6.242252689847868297, -109.2187500020483810 ) ) ;
#8877 = CARTESIAN_POINT ( 'NONE',  ( 5.405949406249992428, -9.363379034771808662, -118.7812500020483952 ) ) ;
#8878 = CARTESIAN_POINT ( 'NONE',  ( -2.121150477449813534E-15, -11.54700538379251284, -193.2500000040968473 ) ) ;
#8879 = CARTESIAN_POINT ( 'NONE',  ( -2.293366432827344421E-15, -12.48450537969573659, -123.2187500020483952 ) ) ;
#8880 = CARTESIAN_POINT ( 'NONE',  ( -5.405949406249996869, 9.363379034771805109, -194.5312500020484094 ) ) ;
#8881 = CARTESIAN_POINT ( 'NONE',  ( 9.999999999999998224, 0.000000000000000000, -5.375000004096769146 ) ) ;
#8882 = CARTESIAN_POINT ( 'NONE',  ( -9.999999999999998224, 5.773502691896259087, -146.8750000000000000 ) ) ;
#8883 = CARTESIAN_POINT ( 'NONE',  ( 10.00000000000000000, 5.773502691896255534, -15.37499999999997335 ) ) ;
#8884 = CARTESIAN_POINT ( 'NONE',  ( 5.405949406249992428, -9.363379034771808662, -67.59375000204836681 ) ) ;
#8885 = CARTESIAN_POINT ( 'NONE',  ( -5.405949406250003975, -9.363379034771801557, -57.34375000204835970 ) ) ;
#8886 = CARTESIAN_POINT ( 'NONE',  ( 9.999999999999998224, 0.000000000000000000, -186.8750000040967905 ) ) ;
#8887 = CARTESIAN_POINT ( 'NONE',  ( -10.81189881249999729, 6.242252689847871849, -24.90625000204838813 ) ) ;
#8888 = CARTESIAN_POINT ( 'NONE',  ( -10.81189881249999907, -6.242252689847864744, -36.46875000204835260 ) ) ;
#8889 = CARTESIAN_POINT ( 'NONE',  ( 0.000000000000000000, 0.000000000000000000, -169.9999999999999716 ) ) ;
#8890 = CARTESIAN_POINT ( 'NONE',  ( -5.405949406249996869, 9.363379034771805109, -147.8437500020483810 ) ) ;
#8891 = CARTESIAN_POINT ( 'NONE',  ( 7.070501591499377789E-16, 11.54700538379251284, -117.1249999999999858 ) ) ;
#8892 = CARTESIAN_POINT ( 'NONE',  ( -9.999999999999998224, 1.224646799147353059E-15, -77.74999999999998579 ) ) ;
#8893 = CARTESIAN_POINT ( 'NONE',  ( -10.81189881249999907, -6.242252689847864744, -138.6562500020484094 ) ) ;
#8894 = CARTESIAN_POINT ( 'NONE',  ( 7.644554776091147741E-16, 12.48450537969573659, -11.65625000204835438 ) ) ;
#8895 = ORIENTED_EDGE ( 'NONE', *, *, #4965, .F. ) ;
#8896 =( BOUNDED_SURFACE ( )  B_SPLINE_SURFACE ( 1, 2, ( 
 ( #20904, #10547, #40114, #33879, #27607, #40747, #23732, #36883, #7329, #33665, #14635, #31714, #21118, #42400, #5374, #1931, #28478, #4722, #31501, #25028, #40957, #8406, #31288, #34523, #38171, #17871, #12043, #8187, #2935, #8615, #2145, #11400, #29256, #16064, #34307, #31067, #15280, #41609, #18311, #24594, #37743, #7969, #25239, #21334, #38383, #8824, #21771, #27823, #34949, #1501, #24387, #5159, #41393, #21981, #4946, #18093, #1717, #14846, #37961, #35159, #18525, #5585, #28042, #41169, #11608, #15058, #24816, #18738, #31930, #37528, #21557, #34737, #28256, #11828, #13038, #16486, #22995, #3567, #13457, #3143, #26232, #39174, #19740, #10233, #10023, #3776, #6584, #22781, #17126, #550, #12831, #26437, #9608, #23203, #39588, #19951, #20372, #26651, #39801, #13250, #16701, #33357, #6795, #36362, #26022, #29897, #23420, #33139, #9815, #7220, #36569, #33561, #3353, #3985, #36784, #7015, #19526, #32920, #30329, #36151, #40016, #128, #35942, #336, #29685, #20167, #32710, #6384, #16911, #30113, #13669, #16270, #26862, #29469, #10446, #23638, #42611, #39380, #970, #11508, #14525, #37426, #14087, #1395, #1182, #21017, #40424, #14303, #31182, #27288, #20584, #27934, #14741, #36997, #40638, #10868, #7869, #40855, #24059, #5055, #27719, #37202, #34207, #27503, #11295, #30963, #41063, #37642, #34418, #10655, #7649, #24710, #20800, #24489, #37856, #33988, #4195, #8300, #18203, #11079, #1612, #8081, #21232, #21445, #4836, #34629, #17982, #759, #13882, #33773, #27078, #4409, #4623, #40221, #17548, #23847, #7432, #17339, #30542, #30749, #24281, #17769, #9144, #18635, #15807, #25767, #2673, #5485, #34844, #38491, #41713, #9351, #18857, #35273, #5706, #24924, #21663, #38710, #28153, #6122, #12361, #8935, #35485, #11726, #22099, #32037, #5267, #15386, #38278, #41508, #2466, #38068, #19065, #15172, #22520, #15596, #22312, #18419, #35693, #31393, #32246, #28798, #35057, #5912, #1827, #38920, #28584, #29002, #42143, #12574, #2265, #31829, #14955, #28369, #25132, #41930, #41287, #8725, #8509, #21879, #31609, #11940, #25558, #2041, #12152, #25345, #39755, #13412, #39545, #510, #12783, #6539, #9976, #30068, #3515, #19692, #26184, #6965, #42563, #16223, #29423, #6749, #26394, #16865, #3307, #26605, #3095, #13625, #29212, #39331, #29634, #20122, #33087, #19903, #33310, #10190, #3735, #16652, #23375, #29853, #39126, #2886, #32666, #13201, #32460, #19480, #26818, #16016, #39970, #6337, #35900, #9560, #16435, #36525, #32876, #10400, #23590, #36737, #36105, #22734, #23155, #77, #19267, #291, #36318, #42351, #25975, #12987, #9771, #22951, #24667, #30915, #27461, #11253, #30281, #14258, #7827, #23796, #33947, #14042, #17295, #20974, #720, #37596, #33729, #27889, #34159, #14480, #36951, #11466, #41022, #8040, #4579, #10823, #40813, #7175, #14700, #4369, #21184, #34374, #4790, #20758, #7604, #20327, #4152, #926, #17720, #17938, #27238, #33521, #40381, #3944, #30500, #1350, #31137, #24016, #27675, #24450, #1570, #40596, #17082, #13839, #37157, #11039, #27033, #40177, #17508, #30703, #10609, #1135, #24233, #37384, #7393, #20540, #35435, #21835, #2419, #21623, #5863, #5017, #15125, #15343, #38236, #35226, #25303, #22266, #31993, #28753, #18158, #18378, #19017, #38028, #8890, #9098, #31567, #41240, #32202, #12529, #2629, #15551, #41880, #31353, #1999, #15761, #8471, #22053, #28959, #28320, #11678, #42095, #37810, #5444, #25514, #5657, #38447, #8255, #12316, #38662, #18805, #21401, #34587, #14913, #1783, #34802, #31782, #28113, #5222, #24878, #41461, #11896, #25091, #8681, #35015, #18595, #2212, #28541, #41673, #12108, #39706, #42512, #29166, #32827, #36060, #3687, #13152, #29586, #29, #19224, #15970, #33038, #22470, #460, #6702, #3258, #29805, #6077, #16385, #26346, #42306, #9721, #32623, #35854, #39499, #32414, #13367, #9516, #16815, #9930, #3467, #12728, #30014, #25722, #26559, #23109, #29371, #16602, #38871, #33261, #22904, #10143, #23323, #36478, #39287, #26135, #9300, #22686, #19432, #36271, #6912, #3048, #35647, #16176, #2836, #6288, #19854, #20066, #12939, #245, #25925, #39077, #6494, #19643, #7128, #876, #4315, #24400, #40542, #13992, #20492, #1296, #36899, #10560, #23746, #1081, #20705, #11202, #40333, #20918, #40130, #37541, #23538, #33677, #33893, #27189, #10986, #14207, #21131, #7981, #24181, #20282, #4104, #31081, #7343, #40760, #10775, #39920, #17454, #17245, #27406, #33471, #34320, #37108, #30445, #23964, #4737, #7552, #17032, #30650, #37328, #17883, #7775, #13789, #13576, #34100, #4522, #26972, #17666, #30860, #14427, #27620, #26767, #10350, #36688, #3897, #30231, #671, #37754, #41406, #41181, #38183, #41621, #28055, #5810, #2157, #11620, #11412, #8199, #35172, #8838, #8627, #18105, #31300, #27837, #31941, #14858, #21994, #18750, #12055, #34534, #25251, #21348, #22210, #25041, #18537, #5597, #24606, #24828, #4958, #1732, #15068, #41828, #15292, #2369, #37974, #34750, #8418, #21783, #21569, #28489, #15495, #28701, #28269, #5170, #18324, #31513, #1943, #11840, #34963, #5386, #38396, #31728, #12265, #40969, #25461, #38606, #9045, #35385, #18963, #1514, #14648, #19800, #32150, #2998, #15709, #29320, #16123, #39237, #39653, #32772, #3208, #32572, #36010, #9884, #26086, #42463, #2580, #6447, #16334, #9675, #29117, #26506, #42675, #10090, #22633, #32987, #29533, #35806, #23058, #6862, #23268, #12892, #3416, #16553, #29751, #22848, #19589, #36427, #15916, #25874, #13101, #196, #39029, #28908, #9464, #42045, #42253, #26300, #13317, #6238, #39449, #36214, #6650, #12471, #25666, #38820, #19382, #9248, #22418, #35596, #6024, #19174, #32363, #12678, #2787, #16980, #7497, #27137, #17614, #4047, #27353, #3845, #30809, #29965, #40079, #40280, #20440, #17403, #20650, #4472, #14153, #10934, #405, #616, #1248, #20230, #33837, #34050, #13732, #23485, #14372, #37487, #30390, #7718, #4262, #30601, #27569, #40488, #20866, #1030, #24127, #37269, #39865, #3638, #33419, #13944, #33207, #30178, #40704, #16765, #11147, #7080, #36634, #10299, #17191, #24346, #7288, #20014, #13526, #26713, #36845, #26921, #10721, #823, #10510, #23697, #23914, #37058, #33625, #40918, #15237, #4685, #25403, #31672, #28217, #12004, #31029, #15018, #8574, #24555, #34697, #14803, #18052, #21724, #1460, #38340, #34483, #28646, #34907, #28435, #37705, #12210, #41776, #41350, #4905, #5329, #21939, #41571, #21516, #14593, #27783, #11360, #8147, #11569, #31247, #11787, #18484, #21295, #1675, #34269, #27999, #2106, #5117, #25199, #41129, #17833, #7931, #8782, #21081, #18266, #24775, #31455, #1889, #24989, #15448, #35119, #5543, #8366, #38131, #18695, #31891, #2319, #37920, #12842, #39186, #16074, #35543, #32931, #6395, #3364, #29063, #16497, #19750, #35954, #2529, #15862, #13262, #19124, #23007, #25821, #22158, #29267, #2731, #9620, #15654, #29695, #19322, #42201, #5973, #141, #38976, #41990, #12627, #22792, #36161, #9412, #38771, #6594, #19536, #32517, #9197, #32720, #22576, #42411, #32309, #35755, #26244, #22366, #28854, #38549, #9825, #32096, #6183, #2946, #26033, #3153, #16282, #8990, #29479, #42620, #5760, #12419, #13050, #39393, #35333, #25613, #18913, #10034, #14709, #39812, #33784, #981, #23860, #16714, #37008, #3580, #5027, #7232, #769, #4207, #36373, #23432, #19964, #13470, #40027, #24676, #40231, #27899, #10244, #16923, #26662, #27088, #36580, #6809, #33150, #17350, #30554, #20382, #348, #7027, #23216, #41032, #20179, #11475, #37822, #7443, #29909, #20597, #33369, #18168, #33573, #13895, #8264, #3789, #30124, #560, #13681, #10457, #21410, #10666, #34596, #26872, #23648, #36794, #3995, #17139, #31362, #1793, #26448, #30340, #39600, #8480, #21634, #15136, #18604, #25101, #5666, #15563, #5235, #28333, #41250, #21845, #12326, #12121, #5874, #8692, #24888, #19235, #2640, #14923, #28551, #11692, #25313, #41683, #22064, #22481, #28764, #41892, #15353, #18819, #35448, #8899, #38458, #28122, #32003, #25524, #35236, #11906, #9313, #38673, #35657, #5454, #6088, #38882, #9108, #34812, #35024, #32423, #38247, #42105, #2226, #38037, #2428, #31792, #22276, #18387, #31577, #19028, #32212, #15771, #2009, #28968, #41471, #12540, #25732, #472, #16398, #3060, #13587, #16613, #39511, #16185, #3478, #3268, #23119, #42525, #29598, #33272, #29382, #22696, #30026, #16827, #39087, #41, #12950, #9940, #257, #26145, #7139, #39296, #12738, #9526, #36488, #10155, #36284, #19441, #32633, #29177, #3698, #9733, #23336, #20078, #13378, #35865, #26570, #6298, #23551, #26358, #19866, #6925, #25938, #22914, #36069, #6505, #13164, #26780, #29816, #39932, #19655, #32840, #6714, #33052, #39719, #10359, #36699, #20292, #2847, #15980, #42316, #26984, #33690, #37120, #886, #24194, #34114, #23757, #4116, #17043, #40344, #30873, #30665, #24413, #27200, #683, #37768, #21145, #33483, #4328, #30243, #1093, #17466, #40556, #40982, #4536, #17678, #33906, #37342, #11213, #27420, #14220, #3909, #7788, #1308, #11000, #30459, #27849, #14441, #11425, #23976, #24620, #14660, #27633, #40143, #10787, #8213, #14005, #17895, #20716, #13800, #20932, #7564, #40772, #10571, #36910, #37554, #7992, #34331, #7356, #4749, #20503, #31094, #1527, #17256, #34975, #21583, #32161, #35182, #15305, #34761, #22007, #21795, #41632, #18337, #5399, #9055, #5183, #41193, #5821, #35397, #14870, #18551, #31526, #28502, #18763, #1955, #25678, #5608, #28281, #12483, #15081, #31952, #2591, #41418, #2381, #41839, #15508, #12068, #15720, #28067, #8640, #25262, #28918, #28713, #31741, #11854, #22222, #25053, #38196, #2170, #8849, #38407, #18976, #12277, #25473, #38618, #42055, #31312, #38830, #21362, #34545, #4971, #18117, #1744, #11634, #24839, #37986, #8430, #6873, #9476, #23069, #23278, #32584, #12688, #33217, #26723, #19601, #39665, #36225, #9894, #36437, #29761, #10101, #6660, #207, #19810, #29128, #35607, #22644, #3219, #22428, #35816, #3648, #6034, #20025, #39039, #25885, #42263, #36021, #13327, #39247, #16775, #29975, #418, #26097, #6249, #16344, #32782, #13538, #39460, #13111, #26310, #2797, #19392, #16564, #19184, #9260, #32998, #29543, #26517, #32373, #42686, #3426, #3009, #6459, #16133, #29331, #15927, #42473, #12901, #9684, #22858, #40499, #4483, #26931, #1471, #17843, #40716, #24139, #832, #30820, #14605, #4694, #37068, #11157, #24356, #37498, #10732, #40290, #39876, #23705, #33636, #37280, #7940, #4058, #10309, #21091, #7727, #3856, #17200, #23497, #20449, #34279, #27147, #36645, #30611, #30401, #10944, #16991, #31039, #20660, #13954, #36856, #7090, #23924, #625, #7510, #20875, #20240, #33848, #40089, #33429, #34061, #4272, #10520, #17625, #17413, #1039, #7299, #14164, #27579, #27363, #30189, #13741, #1258, #14382, #25001, #24786, #21739, #25210, #11578, #32108, #28447, #37930, #37715, #34493, #18707, #35131, #34918, #1685, #14814, #11369, #15459, #41139, #5554, #2330, #38353, #18063, #8792, #4915, #5771, #8586, #2117, #31901, #8157, #8376, #21305, #28011, #41361, #25415, #41582, #28658, #21526, #18276, #34708, #5340, #5129, #12014, #41788, #12223, #11798, #31259, #31466, #1899, #15028, #28228, #38143, #18495, #21950, #31683, #15247, #24566, #38560, #9001, #22169, #35343, #18924, #2540, #27795, #40926, #15666, #29278, #42001, #12852, #42422, #22802, #23226, #16293, #29491, #16083, #19546, #36171, #9631, #26044, #28867, #32730, #42630, #35967, #12638, #10046, #26254, #36386, #6193, #6819, #13060, #19337, #6606, #33160, #19974, #39196, #16508, #29706, #13272, #6405, #3166, #12429, #42211, #9422, #39403, #151, #22588, #25625, #35765, #38782, #25831, #9839, #26461, #32527, #23017, #19760, #32943, #3373, #39610, #9208, #2956, #22378, #35555, #5983, #19134, #32319, #2745, #38986, #15871, #29073, #33794, #10677, #1205, #30350, #10891, #30134, #14329, #13483, #23657, #23870, #4006, #991, #4219, #30771, #40447, #37223, #26672, #26882, #27526, #3799, #17361, #17570, #40037, #7037, #40660, #21038, #13905, #34010, #30562, #14109, #11100, #24084, #4431, #27312, #7671, #20823, #23442, #29919, #16937, #40240, #16724, #572, #24303, #361, #37447, #33379, #20190, #36590, #780, #7891, #33585, #3592, #39823, #10256, #20393, #13690, #37018, #27098, #10467, #36805, #7458, #20608, #7243, #17149, #28173, #17792, #15192, #1849, #8322, #11745, #1417, #37878, #5077, #11317, #41085, #4860, #21253, #18223, #30989, #38088, #37663, #31630, #31413, #41307, #24510, #34228, #2063, #8528, #14549, #8102, #21467, #4644, #18002, #27740, #34441, #40877, #34649, #14975, #11528, #21683, #31204, #24945, #1632, #14761, #27956, #34865, #5287, #24731, #18439, #8026, #17495, #33931, #4354, #23576, #20314, #37369, #26805, #4776, #11024 ),
 ( #40583, #7812, #24218, #7590, #11239, #36723, #17279, #20743, #40798, #14244, #30484, #36936, #17706, #10596, #27017, #40164, #30688, #37142, #27657, #14028, #20960, #13824, #24438, #39956, #7379, #1120, #913, #27447, #34146, #14467, #4564, #30901, #10387, #23782, #37581, #30266, #1336, #21170, #20525, #33507, #34360, #30052, #40368, #498, #13613, #7162, #3931, #17069, #705, #33713, #4138, #27224, #10809, #24002, #5218, #32198, #38658, #19013, #2415, #9095, #31989, #38024, #1779, #31563, #12104, #31349, #18374, #42092, #14909, #28955, #1996, #34798, #8468, #2208, #22262, #5440, #2625, #12525, #15757, #35010, #21619, #25299, #28537, #38867, #5653, #22049, #35222, #11674, #15121, #25510, #28108, #35643, #41875, #38442, #35431, #41236, #8886, #18801, #28316, #15340, #25087, #41457, #15547, #24874, #5859, #11892, #9296, #28749, #25718, #38232, #22466, #18154, #8677, #12312, #21831, #18592, #31778, #41669, #3254, #6908, #20062, #3683, #19639, #6491, #10346, #32619, #42508, #3463, #33257, #12934, #23534, #26131, #39916, #3044, #16598, #16811, #39284, #29801, #26555, #241, #26343, #30010, #42302, #36056, #39495, #456, #33034, #32823, #9717, #36474, #29367, #16172, #22900, #36267, #13148, #13572, #16380, #13363, #29582, #26763, #15966, #25, #9926, #23105, #39703, #6698, #6072, #10139, #23319, #29162, #19849, #19220, #6284, #32410, #2832, #12724, #9511, #25921, #39073, #22682, #35850, #19429, #1077, #4311, #14644, #24177, #40538, #10982, #30227, #26968, #1293, #33467, #11408, #17662, #14203, #40756, #17028, #27402, #37324, #10556, #20701, #872, #4100, #7771, #667, #24396, #20488, #27833, #20914, #14423, #23742, #40965, #36684, #37537, #34097, #40329, #27616, #7124, #1510, #33889, #7977, #21127, #34316, #7548, #37104, #20279, #33674, #30441, #4518, #4733, #13988, #3893, #27185, #13785, #17241, #30856, #17880, #10771, #11198, #31077, #40126, #36895, #7339, #23960, #17450, #30646, #35381, #8834, #25037, #31509, #12261, #5167, #21565, #34746, #12051, #31724, #22206, #8623, #31938, #8414, #5806, #34530, #1939, #2153, #38179, #21990, #25247, #9041, #18746, #15492, #4954, #18320, #18959, #24824, #38392, #38602, #15065, #28051, #32146, #42041, #8195, #2365, #5593, #11616, #2576, #28697, #25457, #35168, #41824, #15705, #1728, #21344, #37970, #18533, #37751, #28265, #28904, #18101, #24602, #41402, #41177, #14854, #21779, #31296, #11836, #34959, #5382, #15288, #28485, #41617, #29113, #39234, #19379, #22629, #26296, #35592, #192, #39025, #33781, #13097, #19796, #42249, #17347, #4204, #13313, #39445, #16119, #3412, #30551, #20593, #9671, #26502, #39649, #10663, #26082, #12888, #12468, #9461, #6234, #9880, #23856, #32568, #25662, #2994, #38817, #35802, #23054, #37005, #29316, #36210, #32983, #6646, #32768, #7440, #6020, #42460, #3204, #9244, #16549, #22844, #36006, #22414, #6443, #19585, #16330, #42671, #29529, #19170, #29747, #32359, #2783, #15912, #12674, #25870, #21242, #1404, #41072, #31191, #28162, #37865, #34639, #10877, #24292, #41296, #1191, #14750, #14964, #37436, #4418, #24934, #18429, #27298, #21455, #24719, #30758, #11735, #5065, #1838, #27945, #18213, #11517, #20811, #40433, #14313, #37651, #14096, #27513, #38078, #24069, #8518, #40647, #17558, #33997, #27728, #31403, #30974, #21671, #34854, #5276, #17778, #11089, #8091, #11305, #978, #1621, #4847, #17991, #37211, #7879, #8310, #7658, #21026, #34216, #34427, #4632, #14534, #40864, #24499, #22529, #38928, #25568, #5494, #18644, #15182, #19274, #2275, #9360, #6131, #29011, #21888, #42151, #8734, #9568, #12370, #5922, #35702, #41520, #28593, #25141, #31838, #2476, #29220, #2681, #32470, #15396, #22108, #41724, #9154, #12162, #28378, #32047, #38501, #2894, #25354, #8944, #35282, #19073, #38720, #42359, #15605, #16024, #5715, #12792, #11950, #18867, #22321, #28807, #12582, #32254, #25984, #25775, #39136, #38288, #41939, #22742, #35496, #15815, #35908, #6345, #35067, #31618, #2051, #3104, #39978, #518, #6547, #33529, #10409, #20337, #3742, #23601, #33317, #39340, #16232, #32884, #13420, #32675, #19701, #728, #29432, #30289, #3315, #36114, #9779, #3524, #36746, #6757, #3952, #13847, #17090, #36326, #22959, #26615, #29861, #40187, #6974, #23384, #36533, #12996, #16445, #26825, #42573, #36959, #13633, #39764, #7183, #26192, #10198, #20129, #29643, #16660, #26403, #87, #16872, #13209, #27043, #39553, #10617, #30077, #23805, #9984, #19488, #23163, #19911, #33098, #299, #1358, #20549, #7612, #31360, #4159, #18166, #37165, #24025, #27247, #34169, #27897, #37392, #34594, #1791, #21408, #24241, #10831, #14488, #17728, #28120, #37605, #11261, #24458, #935, #40388, #14707, #17304, #24886, #31145, #27683, #11473, #30508, #40821, #8048, #20766, #4589, #14267, #17517, #21195, #14052, #37820, #33955, #41248, #34382, #41030, #4377, #11690, #7401, #8263, #4798, #11047, #24674, #33738, #14921, #30923, #5025, #30715, #1143, #20983, #7835, #27469, #40604, #17947, #1578, #38880, #31790, #12736, #2224, #29175, #21843, #5872, #6086, #15351, #19026, #15769, #32210, #15561, #19233, #31575, #2638, #12538, #25730, #21632, #38456, #28549, #9311, #18602, #35022, #5452, #25522, #2427, #35655, #22062, #28966, #41681, #32422, #5233, #12119, #28762, #8897, #35446, #38671, #22479, #42103, #2845, #18385, #25311, #15978, #38245, #9106, #42314, #35234, #41469, #38035, #8478, #34810, #2007, #15134, #25099, #28331, #11904, #8690, #22274, #5665, #18817, #32001, #41890, #12324, #10358, #13162, #9524, #16612, #32838, #26568, #3058, #33481, #6712, #16396, #22912, #20291, #26356, #29380, #29596, #10153, #23549, #39509, #26143, #36697, #39717, #19864, #39295, #23334, #9939, #3476, #36067, #23117, #13585, #9731, #16183, #7137, #39930, #19439, #36282, #6503, #33050, #36487, #19653, #30241, #6923, #3267, #35863, #32631, #16825, #33270, #29814, #42523, #12948, #22694, #26778, #39, #3696, #470, #20076, #255, #30023, #13376, #3907, #17041, #681, #25936, #6297, #39085, #7354, #884, #27417, #11422, #27630, #14657, #40342, #4326, #34111, #7990, #31091, #14003, #27846, #34328, #40553, #20501, #33688, #4114, #27198, #17464, #23974, #4533, #14438, #17254, #10784, #40141, #20714, #11211, #10997, #4746, #7562, #23755, #18114, #1524, #13798, #24191, #10569, #37339, #7785, #20929, #21359, #40769, #24410, #14217, #30663, #30870, #17675, #30457, #26982, #1306, #37551, #21142, #37118, #8210, #17892, #34542, #1091, #4968, #37765, #40979, #33904, #24616, #31309, #36908, #37983, #34759, #9052, #41190, #19182, #25470, #22004, #5818, #24837, #8846, #2378, #18334, #28499, #8637, #11851, #15505, #8427, #32158, #28279, #22426, #28710, #22219, #31523, #6032, #35605, #2588, #41836, #5396, #35394, #1741, #9258, #41629, #15717, #28916, #42053, #15302, #2167, #14867, #41415, #38193, #12274, #12481, #21792, #28064, #34972, #11631, #25050, #38615, #25676, #18548, #18973, #38828, #21580, #35180, #5180, #1952, #15078, #31738, #12065, #25259, #38404, #5605, #18760, #31949, #29329, #42472, #19808, #39458, #29973, #16343, #39663, #16131, #416, #42261, #9683, #9892, #32780, #29759, #32996, #16773, #26515, #23276, #12686, #12899, #13536, #32582, #3424, #3646, #26095, #35814, #26721, #7088, #15925, #10099, #13325, #19390, #39874, #36435, #33215, #16562, #6871, #205, #9474, #29126, #3007, #26308, #2795, #39245, #10307, #25884, #23495, #22856, #6247, #22642, #29541, #20023, #19599, #36643, #32371, #39037, #6457, #36019, #23067, #42684, #3217, #13109, #36223, #6658, #11368, #4056, #30818, #31037, #13952, #1256, #40714, #14380, #40497, #1469, #13739, #27577, #37496, #7939, #3854, #20658, #27145, #21089, #831, #17198, #30399, #7726, #27361, #17841, #4270, #11155, #40288, #14603, #30187, #10730, #10942, #33846, #17623, #20873, #4692, #24354, #34277, #623, #23922, #27793, #20447, #34059, #40925, #37066, #23704, #24564, #37713, #16989, #20238, #33427, #7297, #26929, #40087, #10518, #4481, #36854, #33634, #7508, #17411, #30609, #14162, #1037, #24137, #37278, #4913, #18922, #37928, #24784, #28009, #34916, #28656, #38141, #35341, #2538, #22167, #24999, #11577, #15245, #18493, #28865, #38351, #12012, #25208, #1683, #41137, #15457, #18061, #25623, #31900, #28445, #12221, #31257, #41580, #8790, #8374, #5338, #15026, #18274, #21948, #14812, #38558, #34706, #41999, #35129, #41786, #21524, #12428, #8155, #8999, #5552, #11796, #25413, #21303, #15664, #31681, #5769, #32106, #34492, #21737, #8584, #5127, #31464, #1897, #18705, #28226, #41359, #2115, #2328, #29277, #35764, #33159, #39195, #42210, #42421, #23016, #36385, #9630, #38985, #6818, #9838, #32729, #9421, #39402, #22801, #16292, #6192, #35966, #26460, #22587, #15870, #23225, #10045, #32318, #6404, #19336, #3165, #36170, #32526, #360, #6605, #2955, #5982, #2744, #29705, #3372, #29490, #12637, #25830, #22376, #39609, #16082, #16507, #13271, #19759, #29072, #32942, #12851, #16723, #19545, #13059, #150, #19133, #26043, #42629, #26252, #19973, #3591, #29918, #13482, #38780, #9206, #35553, #20822, #1203, #26881, #40659, #4430, #40239, #20189, #33378, #3798, #40036, #30349, #36804, #17360, #27311, #16936, #10466, #10255, #33584, #24082, #23869, #17569, #20392, #36589, #30987, #14328, #26671, #10676, #23441, #37017, #7457, #33793, #34227, #40446, #10890, #27097, #779, #990, #30561, #30133, #39822, #14108, #37222, #4218, #23656, #21037, #7670, #4643, #17148, #17791, #7890, #34009, #571, #4005, #1416, #7242, #11099, #13904, #7036, #30770, #20606, #27524, #13689, #24302, #37446, #28389, #29182, #37876, #18001, #39093, #32639, #40876, #35662, #38297, #1631, #42322, #6093, #15986, #41529, #19240, #11959, #34439, #11316, #27955, #8527, #27739, #14760, #9532, #24509, #25944, #41084, #31203, #4859, #41306, #32429, #1848, #12745, #22702, #35870, #31412, #11527, #21682, #24944, #6303, #2061, #18438, #31629, #8101, #24730, #22487, #37662, #14548, #8742, #34864, #2853, #21252, #5286, #15191, #8321, #11744, #21466, #34648, #25149, #5076, #19448, #18222, #14974, #28172, #38087, #32847, #7361, #23762, #3914, #30033, #6721, #36705, #20509, #10576, #263, #17048, #30249, #687, #16620, #3484, #3066, #29604, #39517, #478, #13805, #9946, #16192, #23126, #36916, #47, #13594, #26994, #36290, #26785, #23557, #39936, #23344, #40148, #39302, #10366, #20297, #33488, #29390, #29823, #19873, #42531, #26365, #13171, #33058, #33279, #10161, #12956, #13384, #7144, #26576, #26151, #9740, #39726, #36495, #6931, #22921, #3704, #36075, #6512, #19661, #3275, #20085, #16404, #16833, #34122, #40562, #21368, #14226, #30671, #1099, #21151, #40779, #31318, #17684, #40989, #17474, #1750, #892, #11006, #11220, #4542, #31100, #34338, #18123, #27855, #24628, #14010, #27428, #14878, #33914, #4755, #4977, #24200, #37125, #28074, #8436, #17261, #11431, #14666, #20723, #41202, #37775, #34551, #17904, #8219, #1533, #10793, #30465, #4333, #27639, #4122, #37349, #11641, #27205, #24845, #7796, #7570, #23983, #30881, #37992, #20939, #33694, #40349, #1315, #14447, #24420, #37560, #7999, #42267, #9060, #25478, #38625, #15089, #11861, #28924, #18343, #39043, #2596, #41844, #25683, #1961, #28718, #22228, #38201, #5614, #28507, #31747, #35402, #28286, #9265, #5408, #12693, #5827, #42061, #8645, #25889, #21589, #22433, #18981, #25267, #12490, #34768, #29133, #18768, #35612, #6039, #19189, #35187, #22015, #5189, #18557, #15310, #32166, #32378, #41637, #31532, #12073, #41423, #2175, #15725, #2803, #38413, #38836, #15932, #25058, #12283, #21800, #34980, #8856, #31957, #2386, #15513, #26938, #33222, #29766, #13543, #32588, #16569, #10107, #26101, #36232, #16348, #19606, #23283, #3014, #39882, #36025, #30195, #36444, #16780, #39252, #13748, #633, #10317, #6879, #13115, #423, #9480, #16998, #6665, #23503, #36652, #7095, #23074, #9899, #22648, #6463, #3224, #20031, #20246, #29548, #35821, #40775, #6253, #32786, #3653, #33436, #26314, #29980, #26729, #3862, #212, #19396, #16137, #29336, #42478, #12905, #9688, #19815, #39465, #22862, #33004, #3432, #13332, #39670, #26522, #37721, #24147, #4699, #23930, #8163, #7305, #17420, #17631, #40505, #37504, #27585, #24573, #34284, #31046, #20455, #20667, #21312, #40295, #11164, #11375, #33854, #839, #34500, #14819, #23711, #17849, #21097, #27153, #4921, #1477, #40933, #24363, #14612, #7947, #17206, #36862, #10738, #34068, #10527, #37074, #18069, #33643, #31266, #7517, #13960, #30408, #37287, #27801, #27370, #1692, #40095, #4065, #14170, #4278, #4489, #7733, #30617, #40723, #1264, #14388, #1045, #10951, #20881, #30826, #37938, #32325, #15672, #28017, #41589, #11585, #25217, #12021, #35137, #35562, #28665 ) ),
 .UNSPECIFIED., .F., .F., .F. ) 
 B_SPLINE_SURFACE_WITH_KNOTS ( ( 2, 2 ),
 ( 3, 2, 2, 2, 2, 2, 2, 2, 2, 2, 2, 2, 2, 2, 2, 2, 2, 2, 2, 2, 2, 2, 2, 2, 2, 2, 2, 2, 2, 2, 2, 2, 2, 2, 2, 2, 2, 2, 2, 2, 2, 2, 2, 2, 2, 2, 2, 2, 2, 2, 2, 2, 2, 2, 2, 2, 2, 2, 2, 2, 2, 2, 2, 2, 2, 2, 2, 2, 2, 2, 2, 2, 2, 2, 2, 2, 2, 2, 2, 2, 2, 2, 2, 2, 2, 2, 2, 2, 2, 2, 2, 2, 2, 2, 2, 2, 2, 2, 2, 2, 2, 2, 2, 2, 2, 2, 2, 2, 2, 2, 2, 2, 2, 2, 2, 2, 2, 2, 2, 2, 2, 2, 2, 2, 2, 2, 2, 2, 2, 2, 2, 2, 2, 2, 2, 2, 2, 2, 2, 2, 2, 2, 2, 2, 2, 2, 2, 2, 2, 2, 2, 2, 2, 2, 2, 2, 2, 2, 2, 2, 2, 2, 2, 2, 2, 2, 2, 2, 2, 2, 2, 2, 2, 2, 2, 2, 2, 2, 2, 2, 2, 2, 2, 2, 2, 2, 2, 2, 2, 2, 2, 2, 2, 2, 2, 2, 2, 2, 2, 2, 2, 2, 2, 2, 2, 2, 2, 2, 2, 2, 2, 2, 2, 2, 2, 2, 2, 2, 2, 2, 2, 2, 2, 2, 2, 2, 2, 2, 2, 2, 2, 2, 2, 2, 2, 2, 2, 2, 2, 2, 2, 2, 2, 2, 2, 2, 2, 2, 2, 2, 2, 2, 2, 2, 2, 2, 2, 2, 2, 2, 2, 2, 2, 2, 2, 2, 2, 2, 2, 2, 2, 2, 2, 2, 2, 2, 2, 2, 2, 2, 2, 2, 2, 2, 2, 2, 2, 2, 2, 2, 2, 2, 2, 2, 2, 2, 2, 2, 2, 2, 2, 2, 2, 2, 2, 2, 2, 2, 2, 2, 2, 2, 2, 2, 2, 2, 2, 2, 2, 2, 2, 2, 2, 2, 2, 2, 2, 2, 2, 2, 2, 2, 2, 2, 2, 2, 2, 2, 2, 2, 2, 2, 2, 2, 2, 2, 2, 2, 2, 2, 2, 2, 2, 2, 2, 2, 2, 2, 2, 2, 2, 2, 2, 2, 2, 2, 2, 2, 2, 2, 2, 2, 2, 2, 2, 2, 2, 2, 2, 2, 2, 2, 2, 2, 2, 2, 2, 2, 2, 2, 2, 2, 2, 2, 2, 2, 2, 2, 2, 2, 2, 2, 2, 2, 2, 2, 2, 2, 2, 2, 2, 2, 2, 2, 2, 2, 2, 2, 2, 2, 2, 2, 2, 2, 2, 2, 2, 2, 2, 2, 2, 2, 2, 2, 2, 2, 2, 2, 2, 2, 2, 2, 2, 2, 2, 2, 2, 2, 2, 2, 2, 2, 2, 2, 2, 2, 2, 2, 2, 2, 2, 2, 2, 2, 2, 2, 2, 2, 2, 2, 2, 2, 2, 2, 2, 2, 2, 2, 2, 2, 2, 2, 2, 2, 2, 2, 2, 2, 2, 2, 2, 2, 2, 2, 2, 2, 2, 2, 2, 2, 2, 2, 2, 2, 2, 2, 2, 2, 2, 2, 2, 2, 2, 2, 2, 2, 2, 2, 2, 2, 2, 2, 2, 2, 2, 2, 2, 2, 2, 2, 2, 2, 2, 2, 2, 2, 2, 2, 2, 2, 2, 2, 2, 2, 2, 2, 2, 2, 2, 2, 2, 2, 2, 2, 2, 2, 2, 2, 2, 2, 2, 2, 2, 2, 2, 2, 2, 2, 2, 2, 2, 2, 2, 2, 2, 2, 2, 2, 2, 2, 2, 2, 2, 2, 2, 2, 2, 2, 2, 2, 2, 2, 2, 2, 2, 2, 2, 2, 2, 2, 2, 2, 2, 2, 2, 2, 2, 2, 2, 2, 2, 2, 2, 2, 2, 2, 2, 2, 2, 2, 2, 2, 2, 2, 2, 2, 2, 2, 2, 2, 2, 2, 2, 2, 2, 2, 2, 2, 2, 2, 2, 2, 2, 2, 2, 2, 2, 2, 2, 2, 2, 2, 2, 2, 2, 2, 2, 2, 2, 2, 2, 2, 2, 2, 2, 2, 2, 2, 2, 2, 2, 2, 2, 2, 2, 2, 2, 2, 2, 2, 2, 2, 2, 2, 2, 2, 2, 2, 2, 2, 2, 2, 2, 2, 2, 2, 2, 2, 2, 2, 2, 2, 2, 2, 2, 2, 2, 2, 2, 2, 2, 2, 2, 2, 2, 2, 2, 2, 2, 2, 2, 2, 2, 2, 2, 2, 2, 2, 2, 2, 2, 2, 2, 2, 2, 2, 2, 2, 2, 2, 2, 2, 2, 2, 2, 2, 2, 2, 2, 2, 2, 2, 2, 2, 2, 2, 2, 2, 2, 2, 2, 2, 2, 2, 2, 2, 2, 2, 2, 2, 2, 2, 2, 2, 2, 2, 2, 2, 2, 2, 2, 2, 2, 2, 2, 2, 2, 2, 2, 2, 2, 2, 2, 2, 2, 2, 2, 2, 2, 2, 3 ),
 ( 0.000000000000000000, 1.000000000000000000 ),
 ( 0.000000000000000000, 0.001243781094527363160, 0.002487562189054726321, 0.003731343283582089481, 0.004975124378109452641, 0.006218905472636816235, 0.007462686567164178962, 0.008706467661691542556, 0.009950248756218905283, 0.01119402985074626801, 0.01243781094527363247, 0.01368159203980099520, 0.01492537313432835792, 0.01616915422885572065, 0.01741293532338308511, 0.01865671641791044610, 0.01990049751243781057, 0.02114427860696517503, 0.02238805970149253602, 0.02363184079601990048, 0.02487562189054726494, 0.02611940298507462593, 0.02736318407960199039, 0.02860696517412935486, 0.02985074626865671585, 0.03109452736318408031, 0.03233830845771144130, 0.03358208955223880576, 0.03482587064676617022, 0.03606965174129353469, 0.03731343283582089221, 0.03855721393034825667, 0.03980099502487562113, 0.04104477611940298559, 0.04228855721393035005, 0.04353233830845771452, 0.04477611940298507204, 0.04601990049751243650, 0.04726368159203980096, 0.04850746268656716542, 0.04975124378109452988, 0.05099502487562188741, 0.05223880597014925187, 0.05348258706467661633, 0.05472636815920398079, 0.05597014925373134525, 0.05721393034825870971, 0.05845771144278606724, 0.05970149253731343170, 0.06094527363184079616, 0.06218905472636816062, 0.06343283582089552508, 0.06467661691542288260, 0.06592039800995025400, 0.06716417910447761153, 0.06840796019900496905, 0.06965174129353234045, 0.07089552238805969797, 0.07213930348258706937, 0.07338308457711442689, 0.07462686567164178442, 0.07587064676616915582, 0.07711442786069651334, 0.07835820895522388474, 0.07960199004975124226, 0.08084577114427861366, 0.08208955223880597118, 0.08333333333333332871, 0.08457711442786070011, 0.08582089552238805763, 0.08706467661691542903, 0.08830845771144278655, 0.08955223880597014408, 0.09079601990049751548, 0.09203980099502487300, 0.09328358208955224440, 0.09452736318407960192, 0.09577114427860695944, 0.09701492537313433084, 0.09825870646766168837, 0.09950248756218905977, 0.1007462686567164173, 0.1019900497512437748, 0.1032338308457711462, 0.1044776119402985037, 0.1057213930348258751, 0.1069651741293532327, 0.1082089552238805902, 0.1094527363184079616, 0.1106965174129353191, 0.1119402985074626905, 0.1131840796019900480, 0.1144278606965174194, 0.1156716417910447769, 0.1169154228855721345, 0.1181592039800995059, 0.1194029850746268634, 0.1206467661691542348, 0.1218905472636815923, 0.1231343283582089498, 0.1243781094527363212, 0.1256218905472636926, 0.1268656716417910502, 0.1281094527363184077, 0.1293532338308457652, 0.1305970149253731227, 0.1318407960199005080, 0.1330845771144278655, 0.1343283582089552231, 0.1355721393034825806, 0.1368159203980099381, 0.1380597014925373234, 0.1393034825870646809, 0.1405472636815920384, 0.1417910447761193959, 0.1430348258706467535, 0.1442786069651741387, 0.1455223880597014963, 0.1467661691542288538, 0.1480099502487562113, 0.1492537313432835688, 0.1504975124378109541, 0.1517412935323383116, 0.1529850746268656692, 0.1542288557213930267, 0.1554726368159203842, 0.1567164179104477695, 0.1579601990049751270, 0.1592039800995024845, 0.1604477611940298420, 0.1616915422885572273, 0.1629353233830845848, 0.1641791044776119424, 0.1654228855721392999, 0.1666666666666666574, 0.1679104477611940427, 0.1691542288557214002, 0.1703980099502487577, 0.1716417910447761153, 0.1728855721393034728, 0.1741293532338308581, 0.1753731343283582156, 0.1766169154228855731, 0.1778606965174129306, 0.1791044776119402882, 0.1803482587064676734, 0.1815920398009950310, 0.1828358208955223885, 0.1840796019900497460, 0.1853233830845771035, 0.1865671641791044888, 0.1878109452736318463, 0.1890547263681592038, 0.1902985074626865614, 0.1915422885572139189, 0.1927860696517413042, 0.1940298507462686617, 0.1952736318407960192, 0.1965174129353233767, 0.1977611940298507343, 0.1990049751243781195, 0.2002487562189054771, 0.2014925373134328346, 0.2027363184079601921, 0.2039800995024875496, 0.2052238805970149349, 0.2064676616915422924, 0.2077114427860696499, 0.2089552238805970075, 0.2101990049751243650, 0.2114427860696517503, 0.2126865671641791078, 0.2139303482587064653, 0.2151741293532338228, 0.2164179104477611804, 0.2176616915422885656, 0.2189054726368159232, 0.2201492537313432807, 0.2213930348258706382, 0.2226368159203980235, 0.2238805970149253810, 0.2251243781094527385, 0.2263681592039800961, 0.2276119402985074536, 0.2288557213930348389, 0.2300995024875621964, 0.2313432835820895539, 0.2325870646766169114, 0.2338308457711442689, 0.2350746268656716542, 0.2363184079601990117, 0.2375621890547263693, 0.2388059701492537268, 0.2400497512437810843, 0.2412935323383084696, 0.2425373134328358271, 0.2437810945273631846, 0.2450248756218905422, 0.2462686567164178997, 0.2475124378109452850, 0.2487562189054726425, 0.2500000000000000000, 0.2512437810945273853, 0.2524875621890547150, 0.2537313432835821003, 0.2549751243781094301, 0.2562189054726368154, 0.2574626865671642006, 0.2587064676616915304, 0.2599502487562189157, 0.2611940298507462455, 0.2624378109452736307, 0.2636815920398010160, 0.2649253731343283458, 0.2661691542288557311, 0.2674129353233830608, 0.2686567164179104461, 0.2699004975124378314, 0.2711442786069651611, 0.2723880597014925464, 0.2736318407960198762, 0.2748756218905472615, 0.2761194029850746468, 0.2773631840796019765, 0.2786069651741293618, 0.2798507462686566916, 0.2810945273631840768, 0.2823383084577114621, 0.2835820895522387919, 0.2848258706467661772, 0.2860696517412935069, 0.2873134328358208922, 0.2885572139303482775, 0.2898009950248756073, 0.2910447761194029925, 0.2922885572139303223, 0.2935323383084577076, 0.2947761194029850929, 0.2960199004975124226, 0.2972636815920398079, 0.2985074626865671377, 0.2997512437810945229, 0.3009950248756219082, 0.3022388059701492380, 0.3034825870646766233, 0.3047263681592039530, 0.3059701492537313383, 0.3072139303482587236, 0.3084577114427860534, 0.3097014925373134386, 0.3109452736318407684, 0.3121890547263681537, 0.3134328358208955390, 0.3146766169154228687, 0.3159203980099502540, 0.3171641791044776393, 0.3184079601990049690, 0.3196517412935323543, 0.3208955223880596841, 0.3221393034825870694, 0.3233830845771144546, 0.3246268656716417844, 0.3258706467661691697, 0.3271144278606964995, 0.3283582089552238847, 0.3296019900497512700, 0.3308457711442785998, 0.3320895522388059851, 0.3333333333333333148, 0.3345771144278607001, 0.3358208955223880854, 0.3370646766169154152, 0.3383084577114428004, 0.3395522388059701302, 0.3407960199004975155, 0.3420398009950249008, 0.3432835820895522305, 0.3445273631840796158, 0.3457711442786069456, 0.3470149253731343308, 0.3482587064676617161, 0.3495024875621890459, 0.3507462686567164312, 0.3519900497512437609, 0.3532338308457711462, 0.3544776119402985315, 0.3557213930348258613, 0.3569651741293532465, 0.3582089552238805763, 0.3594527363184079616, 0.3606965174129353469, 0.3619402985074626766, 0.3631840796019900619, 0.3644278606965173917, 0.3656716417910447769, 0.3669154228855721622, 0.3681592039800994920, 0.3694029850746268773, 0.3706467661691542070, 0.3718905472636815923, 0.3731343283582089776, 0.3743781094527363074, 0.3756218905472636926, 0.3768656716417910224, 0.3781094527363184077, 0.3793532338308457930, 0.3805970149253731227, 0.3818407960199005080, 0.3830845771144278378, 0.3843283582089552231, 0.3855721393034826083, 0.3868159203980099381, 0.3880597014925373234, 0.3893034825870646531, 0.3905472636815920384, 0.3917910447761194237, 0.3930348258706467535, 0.3942786069651741387, 0.3955223880597014685, 0.3967661691542288538, 0.3980099502487562391, 0.3992537313432835688, 0.4004975124378109541, 0.4017412935323382839, 0.4029850746268656692, 0.4042288557213930544, 0.4054726368159203842, 0.4067164179104477695, 0.4079601990049750992, 0.4092039800995024845, 0.4104477611940298698, 0.4116915422885571996, 0.4129353233830845848, 0.4141791044776119146, 0.4154228855721392999, 0.4166666666666666852, 0.4179104477611940149, 0.4191542288557214002, 0.4203980099502487300, 0.4216417910447761153, 0.4228855721393035005, 0.4241293532338308303, 0.4253731343283582156, 0.4266169154228855454, 0.4278606965174129306, 0.4291044776119403159, 0.4303482587064676457, 0.4315920398009950310, 0.4328358208955223607, 0.4340796019900497460, 0.4353233830845771313, 0.4365671641791044610, 0.4378109452736318463, 0.4390547263681592316, 0.4402985074626865614, 0.4415422885572139466, 0.4427860696517412764, 0.4440298507462686617, 0.4452736318407960470, 0.4465174129353233767, 0.4477611940298507620, 0.4490049751243780918, 0.4502487562189054771, 0.4514925373134328623, 0.4527363184079601921, 0.4539800995024875774, 0.4552238805970149071, 0.4564676616915422924, 0.4577114427860696777, 0.4589552238805970075, 0.4601990049751243927, 0.4614427860696517225, 0.4626865671641791078, 0.4639303482587064931, 0.4651741293532338228, 0.4664179104477612081, 0.4676616915422885379, 0.4689054726368159232, 0.4701492537313433084, 0.4713930348258706382, 0.4726368159203980235, 0.4738805970149253532, 0.4751243781094527385, 0.4763681592039801238, 0.4776119402985074536, 0.4788557213930348389, 0.4800995024875621686, 0.4813432835820895539, 0.4825870646766169392, 0.4838308457711442689, 0.4850746268656716542, 0.4863184079601989840, 0.4875621890547263693, 0.4888059701492537545, 0.4900497512437810843, 0.4912935323383084696, 0.4925373134328357994, 0.4937810945273631846, 0.4950248756218905699, 0.4962686567164178997, 0.4975124378109452850, 0.4987562189054726147, 0.5000000000000000000, 0.5012437810945273853, 0.5024875621890547706, 0.5037313432835820448, 0.5049751243781094301, 0.5062189054726368154, 0.5074626865671642006, 0.5087064676616915859, 0.5099502487562188602, 0.5111940298507462455, 0.5124378109452736307, 0.5136815920398010160, 0.5149253731343284013, 0.5161691542288556755, 0.5174129353233830608, 0.5186567164179104461, 0.5199004975124378314, 0.5211442786069652167, 0.5223880597014924909, 0.5236318407960198762, 0.5248756218905472615, 0.5261194029850746468, 0.5273631840796020320, 0.5286069651741293063, 0.5298507462686566916, 0.5310945273631840768, 0.5323383084577114621, 0.5335820895522388474, 0.5348258706467661217, 0.5360696517412935069, 0.5373134328358208922, 0.5385572139303482775, 0.5398009950248756628, 0.5410447761194029370, 0.5422885572139303223, 0.5435323383084577076, 0.5447761194029850929, 0.5460199004975124781, 0.5472636815920397524, 0.5485074626865671377, 0.5497512437810945229, 0.5509950248756219082, 0.5522388059701492935, 0.5534825870646765678, 0.5547263681592039530, 0.5559701492537313383, 0.5572139303482587236, 0.5584577114427861089, 0.5597014925373133831, 0.5609452736318407684, 0.5621890547263681537, 0.5634328358208955390, 0.5646766169154229242, 0.5659203980099501985, 0.5671641791044775838, 0.5684079601990049690, 0.5696517412935323543, 0.5708955223880597396, 0.5721393034825870139, 0.5733830845771143991, 0.5746268656716417844, 0.5758706467661691697, 0.5771144278606965550, 0.5783582089552238292, 0.5796019900497512145, 0.5808457711442785998, 0.5820895522388059851, 0.5833333333333333703, 0.5845771144278606446, 0.5858208955223880299, 0.5870646766169154152, 0.5883084577114428004, 0.5895522388059701857, 0.5907960199004974600, 0.5920398009950248452, 0.5932835820895522305, 0.5945273631840796158, 0.5957711442786070011, 0.5970149253731342753, 0.5982587064676616606, 0.5995024875621890459, 0.6007462686567164312, 0.6019900497512438164, 0.6032338308457710907, 0.6044776119402984760, 0.6057213930348258613, 0.6069651741293532465, 0.6082089552238806318, 0.6094527363184079061, 0.6106965174129352913, 0.6119402985074626766, 0.6131840796019900619, 0.6144278606965174472, 0.6156716417910447214, 0.6169154228855721067, 0.6181592039800994920, 0.6194029850746268773, 0.6206467661691542625, 0.6218905472636815368, 0.6231343283582089221, 0.6243781094527363074, 0.6256218905472636926, 0.6268656716417910779, 0.6281094527363184632, 0.6293532338308457375, 0.6305970149253731227, 0.6318407960199005080, 0.6330845771144278933, 0.6343283582089552786, 0.6355721393034825528, 0.6368159203980099381, 0.6380597014925373234, 0.6393034825870647087, 0.6405472636815920939, 0.6417910447761193682, 0.6430348258706467535, 0.6442786069651741387, 0.6455223880597015240, 0.6467661691542289093, 0.6480099502487561836, 0.6492537313432835688, 0.6504975124378109541, 0.6517412935323383394, 0.6529850746268657247, 0.6542288557213929989, 0.6554726368159203842, 0.6567164179104477695, 0.6579601990049751548, 0.6592039800995025400, 0.6604477611940298143, 0.6616915422885571996, 0.6629353233830845848, 0.6641791044776119701, 0.6654228855721393554, 0.6666666666666666297, 0.6679104477611940149, 0.6691542288557214002, 0.6703980099502487855, 0.6716417910447761708, 0.6728855721393034450, 0.6741293532338308303, 0.6753731343283582156, 0.6766169154228856009, 0.6778606965174129861, 0.6791044776119402604, 0.6803482587064676457, 0.6815920398009950310, 0.6828358208955224162, 0.6840796019900498015, 0.6853233830845770758, 0.6865671641791044610, 0.6878109452736318463, 0.6890547263681592316, 0.6902985074626866169, 0.6915422885572138911, 0.6927860696517412764, 0.6940298507462686617, 0.6952736318407960470, 0.6965174129353234322, 0.6977611940298507065, 0.6990049751243780918, 0.7002487562189054771, 0.7014925373134328623, 0.7027363184079602476, 0.7039800995024875219, 0.7052238805970149071, 0.7064676616915422924, 0.7077114427860696777, 0.7089552238805970630, 0.7101990049751243372, 0.7114427860696517225, 0.7126865671641791078, 0.7139303482587064931, 0.7151741293532338783, 0.7164179104477611526, 0.7176616915422885379, 0.7189054726368159232, 0.7201492537313433084, 0.7213930348258706937, 0.7226368159203979680, 0.7238805970149253532, 0.7251243781094527385, 0.7263681592039801238, 0.7276119402985075091, 0.7288557213930347833, 0.7300995024875621686, 0.7313432835820895539, 0.7325870646766169392, 0.7338308457711443245, 0.7350746268656715987, 0.7363184079601989840, 0.7375621890547263693, 0.7388059701492537545, 0.7400497512437811398, 0.7412935323383084141, 0.7425373134328357994, 0.7437810945273631846, 0.7450248756218905699, 0.7462686567164179552, 0.7475124378109452294, 0.7487562189054726147, 0.7500000000000000000, 0.7512437810945273853, 0.7524875621890547706, 0.7537313432835820448, 0.7549751243781094301, 0.7562189054726368154, 0.7574626865671642006, 0.7587064676616915859, 0.7599502487562188602, 0.7611940298507462455, 0.7624378109452736307, 0.7636815920398010160, 0.7649253731343284013, 0.7661691542288556755, 0.7674129353233830608, 0.7686567164179104461, 0.7699004975124378314, 0.7711442786069652167, 0.7723880597014924909, 0.7736318407960198762, 0.7748756218905472615, 0.7761194029850746468, 0.7773631840796020320, 0.7786069651741293063, 0.7798507462686566916, 0.7810945273631840768, 0.7823383084577114621, 0.7835820895522388474, 0.7848258706467661217, 0.7860696517412935069, 0.7873134328358208922, 0.7885572139303482775, 0.7898009950248756628, 0.7910447761194029370, 0.7922885572139303223, 0.7935323383084577076, 0.7947761194029850929, 0.7960199004975124781, 0.7972636815920397524, 0.7985074626865671377, 0.7997512437810945229, 0.8009950248756219082, 0.8022388059701492935, 0.8034825870646765678, 0.8047263681592039530, 0.8059701492537313383, 0.8072139303482587236, 0.8084577114427861089, 0.8097014925373133831, 0.8109452736318407684, 0.8121890547263681537, 0.8134328358208955390, 0.8146766169154229242, 0.8159203980099501985, 0.8171641791044775838, 0.8184079601990049690, 0.8196517412935323543, 0.8208955223880597396, 0.8221393034825870139, 0.8233830845771143991, 0.8246268656716417844, 0.8258706467661691697, 0.8271144278606965550, 0.8283582089552238292, 0.8296019900497512145, 0.8308457711442785998, 0.8320895522388059851, 0.8333333333333333703, 0.8345771144278606446, 0.8358208955223880299, 0.8370646766169154152, 0.8383084577114428004, 0.8395522388059701857, 0.8407960199004974600, 0.8420398009950248452, 0.8432835820895522305, 0.8445273631840796158, 0.8457711442786070011, 0.8470149253731342753, 0.8482587064676616606, 0.8495024875621890459, 0.8507462686567164312, 0.8519900497512438164, 0.8532338308457710907, 0.8544776119402984760, 0.8557213930348258613, 0.8569651741293532465, 0.8582089552238806318, 0.8594527363184079061, 0.8606965174129352913, 0.8619402985074626766, 0.8631840796019900619, 0.8644278606965174472, 0.8656716417910447214, 0.8669154228855721067, 0.8681592039800994920, 0.8694029850746268773, 0.8706467661691542625, 0.8718905472636815368, 0.8731343283582089221, 0.8743781094527363074, 0.8756218905472636926, 0.8768656716417910779, 0.8781094527363184632, 0.8793532338308457375, 0.8805970149253731227, 0.8818407960199005080, 0.8830845771144278933, 0.8843283582089552786, 0.8855721393034825528, 0.8868159203980099381, 0.8880597014925373234, 0.8893034825870647087, 0.8905472636815920939, 0.8917910447761193682, 0.8930348258706467535, 0.8942786069651741387, 0.8955223880597015240, 0.8967661691542289093, 0.8980099502487561836, 0.8992537313432835688, 0.9004975124378109541, 0.9017412935323383394, 0.9029850746268657247, 0.9042288557213929989, 0.9054726368159203842, 0.9067164179104477695, 0.9079601990049751548, 0.9092039800995025400, 0.9104477611940298143, 0.9116915422885571996, 0.9129353233830845848, 0.9141791044776119701, 0.9154228855721393554, 0.9166666666666666297, 0.9179104477611940149, 0.9191542288557214002, 0.9203980099502487855, 0.9216417910447761708, 0.9228855721393034450, 0.9241293532338308303, 0.9253731343283582156, 0.9266169154228856009, 0.9278606965174129861, 0.9291044776119402604, 0.9303482587064676457, 0.9315920398009950310, 0.9328358208955224162, 0.9340796019900498015, 0.9353233830845770758, 0.9365671641791044610, 0.9378109452736318463, 0.9390547263681592316, 0.9402985074626866169, 0.9415422885572138911, 0.9427860696517412764, 0.9440298507462686617, 0.9452736318407960470, 0.9465174129353234322, 0.9477611940298507065, 0.9490049751243780918, 0.9502487562189054771, 0.9514925373134328623, 0.9527363184079602476, 0.9539800995024875219, 0.9552238805970149071, 0.9564676616915422924, 0.9577114427860696777, 0.9589552238805970630, 0.9601990049751243372, 0.9614427860696517225, 0.9626865671641791078, 0.9639303482587064931, 0.9651741293532338783, 0.9664179104477611526, 0.9676616915422885379, 0.9689054726368159232, 0.9701492537313433084, 0.9713930348258706937, 0.9726368159203979680, 0.9738805970149253532, 0.9751243781094527385, 0.9763681592039801238, 0.9776119402985075091, 0.9788557213930347833, 0.9800995024875621686, 0.9813432835820895539, 0.9825870646766169392, 0.9838308457711443245, 0.9850746268656715987, 0.9863184079601989840, 0.9875621890547263693, 0.9888059701492537545, 0.9900497512437811398, 0.9912935323383084141, 0.9925373134328357994, 0.9937810945273631846, 0.9950248756218905699 ),
 .UNSPECIFIED. ) 
 GEOMETRIC_REPRESENTATION_ITEM ( )  RATIONAL_B_SPLINE_SURFACE ( (
 ( 1.000000000000000000, 0.8660254037844387076, 1.000000000000000000, 0.8660254037844387076, 1.000000000000000000, 0.8660254037844387076, 1.000000000000000000, 0.8660254037844387076, 1.000000000000000000, 0.8660254037844387076, 1.000000000000000000, 0.8660254037844387076, 1.000000000000000000, 0.8660254037844387076, 1.000000000000000000, 0.8660254037844387076, 1.000000000000000000, 0.8660254037844387076, 1.000000000000000000, 0.8660254037844387076, 1.000000000000000000, 0.8660254037844387076, 1.000000000000000000, 0.8660254037844387076, 1.000000000000000000, 0.8660254037844387076, 1.000000000000000000, 0.8660254037844387076, 1.000000000000000000, 0.8660254037844387076, 1.000000000000000000, 0.8660254037844387076, 1.000000000000000000, 0.8660254037844387076, 1.000000000000000000, 0.8660254037844387076, 1.000000000000000000, 0.8660254037844387076, 1.000000000000000000, 0.8660254037844387076, 1.000000000000000000, 0.8660254037844387076, 1.000000000000000000, 0.8660254037844387076, 1.000000000000000000, 0.8660254037844387076, 1.000000000000000000, 0.8660254037844387076, 1.000000000000000000, 0.8660254037844387076, 1.000000000000000000, 0.8660254037844387076, 1.000000000000000000, 0.8660254037844387076, 1.000000000000000000, 0.8660254037844387076, 1.000000000000000000, 0.8660254037844387076, 1.000000000000000000, 0.8660254037844387076, 1.000000000000000000, 0.8660254037844387076, 1.000000000000000000, 0.8660254037844387076, 1.000000000000000000, 0.8660254037844387076, 1.000000000000000000, 0.8660254037844387076, 1.000000000000000000, 0.8660254037844387076, 1.000000000000000000, 0.8660254037844387076, 1.000000000000000000, 0.8660254037844387076, 1.000000000000000000, 0.8660254037844387076, 1.000000000000000000, 0.8660254037844387076, 1.000000000000000000, 0.8660254037844387076, 1.000000000000000000, 0.8660254037844387076, 1.000000000000000000, 0.8660254037844387076, 1.000000000000000000, 0.8660254037844387076, 1.000000000000000000, 0.8660254037844387076, 1.000000000000000000, 0.8660254037844387076, 1.000000000000000000, 0.8660254037844387076, 1.000000000000000000, 0.8660254037844387076, 1.000000000000000000, 0.8660254037844387076, 1.000000000000000000, 0.8660254037844387076, 1.000000000000000000, 0.8660254037844387076, 1.000000000000000000, 0.8660254037844387076, 1.000000000000000000, 0.8660254037844387076, 1.000000000000000000, 0.8660254037844387076, 1.000000000000000000, 0.8660254037844387076, 1.000000000000000000, 0.8660254037844387076, 1.000000000000000000, 0.8660254037844387076, 1.000000000000000000, 0.8660254037844387076, 1.000000000000000000, 0.8660254037844387076, 1.000000000000000000, 0.8660254037844387076, 1.000000000000000000, 0.8660254037844387076, 1.000000000000000000, 0.8660254037844387076, 1.000000000000000000, 0.8660254037844387076, 1.000000000000000000, 0.8660254037844387076, 1.000000000000000000, 0.8660254037844387076, 1.000000000000000000, 0.8660254037844387076, 1.000000000000000000, 0.8660254037844387076, 1.000000000000000000, 0.8660254037844387076, 1.000000000000000000, 0.8660254037844387076, 1.000000000000000000, 0.8660254037844387076, 1.000000000000000000, 0.8660254037844387076, 1.000000000000000000, 0.8660254037844387076, 1.000000000000000000, 0.8660254037844387076, 1.000000000000000000, 0.8660254037844387076, 1.000000000000000000, 0.8660254037844387076, 1.000000000000000000, 0.8660254037844387076, 1.000000000000000000, 0.8660254037844387076, 1.000000000000000000, 0.8660254037844387076, 1.000000000000000000, 0.8660254037844387076, 1.000000000000000000, 0.8660254037844387076, 1.000000000000000000, 0.8660254037844387076, 1.000000000000000000, 0.8660254037844387076, 1.000000000000000000, 0.8660254037844387076, 1.000000000000000000, 0.8660254037844387076, 1.000000000000000000, 0.8660254037844387076, 1.000000000000000000, 0.8660254037844387076, 1.000000000000000000, 0.8660254037844387076, 1.000000000000000000, 0.8660254037844387076, 1.000000000000000000, 0.8660254037844387076, 1.000000000000000000, 0.8660254037844387076, 1.000000000000000000, 0.8660254037844387076, 1.000000000000000000, 0.8660254037844387076, 1.000000000000000000, 0.8660254037844387076, 1.000000000000000000, 0.8660254037844387076, 1.000000000000000000, 0.8660254037844387076, 1.000000000000000000, 0.8660254037844387076, 1.000000000000000000, 0.8660254037844387076, 1.000000000000000000, 0.8660254037844387076, 1.000000000000000000, 0.8660254037844387076, 1.000000000000000000, 0.8660254037844387076, 1.000000000000000000, 0.8660254037844387076, 1.000000000000000000, 0.8660254037844387076, 1.000000000000000000, 0.8660254037844387076, 1.000000000000000000, 0.8660254037844387076, 1.000000000000000000, 0.8660254037844387076, 1.000000000000000000, 0.8660254037844387076, 1.000000000000000000, 0.8660254037844387076, 1.000000000000000000, 0.8660254037844387076, 1.000000000000000000, 0.8660254037844387076, 1.000000000000000000, 0.8660254037844387076, 1.000000000000000000, 0.8660254037844387076, 1.000000000000000000, 0.8660254037844387076, 1.000000000000000000, 0.8660254037844387076, 1.000000000000000000, 0.8660254037844387076, 1.000000000000000000, 0.8660254037844387076, 1.000000000000000000, 0.8660254037844387076, 1.000000000000000000, 0.8660254037844387076, 1.000000000000000000, 0.8660254037844387076, 1.000000000000000000, 0.8660254037844387076, 1.000000000000000000, 0.8660254037844387076, 1.000000000000000000, 0.8660254037844387076, 1.000000000000000000, 0.8660254037844387076, 1.000000000000000000, 0.8660254037844387076, 1.000000000000000000, 0.8660254037844387076, 1.000000000000000000, 0.8660254037844387076, 1.000000000000000000, 0.8660254037844387076, 1.000000000000000000, 0.8660254037844387076, 1.000000000000000000, 0.8660254037844387076, 1.000000000000000000, 0.8660254037844387076, 1.000000000000000000, 0.8660254037844387076, 1.000000000000000000, 0.8660254037844387076, 1.000000000000000000, 0.8660254037844387076, 1.000000000000000000, 0.8660254037844387076, 1.000000000000000000, 0.8660254037844387076, 1.000000000000000000, 0.8660254037844387076, 1.000000000000000000, 0.8660254037844387076, 1.000000000000000000, 0.8660254037844387076, 1.000000000000000000, 0.8660254037844387076, 1.000000000000000000, 0.8660254037844387076, 1.000000000000000000, 0.8660254037844387076, 1.000000000000000000, 0.8660254037844387076, 1.000000000000000000, 0.8660254037844387076, 1.000000000000000000, 0.8660254037844387076, 1.000000000000000000, 0.8660254037844387076, 1.000000000000000000, 0.8660254037844387076, 1.000000000000000000, 0.8660254037844387076, 1.000000000000000000, 0.8660254037844387076, 1.000000000000000000, 0.8660254037844387076, 1.000000000000000000, 0.8660254037844387076, 1.000000000000000000, 0.8660254037844387076, 1.000000000000000000, 0.8660254037844387076, 1.000000000000000000, 0.8660254037844387076, 1.000000000000000000, 0.8660254037844387076, 1.000000000000000000, 0.8660254037844387076, 1.000000000000000000, 0.8660254037844387076, 1.000000000000000000, 0.8660254037844387076, 1.000000000000000000, 0.8660254037844387076, 1.000000000000000000, 0.8660254037844387076, 1.000000000000000000, 0.8660254037844387076, 1.000000000000000000, 0.8660254037844387076, 1.000000000000000000, 0.8660254037844387076, 1.000000000000000000, 0.8660254037844387076, 1.000000000000000000, 0.8660254037844387076, 1.000000000000000000, 0.8660254037844387076, 1.000000000000000000, 0.8660254037844387076, 1.000000000000000000, 0.8660254037844387076, 1.000000000000000000, 0.8660254037844387076, 1.000000000000000000, 0.8660254037844387076, 1.000000000000000000, 0.8660254037844387076, 1.000000000000000000, 0.8660254037844387076, 1.000000000000000000, 0.8660254037844387076, 1.000000000000000000, 0.8660254037844387076, 1.000000000000000000, 0.8660254037844387076, 1.000000000000000000, 0.8660254037844387076, 1.000000000000000000, 0.8660254037844387076, 1.000000000000000000, 0.8660254037844387076, 1.000000000000000000, 0.8660254037844387076, 1.000000000000000000, 0.8660254037844387076, 1.000000000000000000, 0.8660254037844387076, 1.000000000000000000, 0.8660254037844387076, 1.000000000000000000, 0.8660254037844387076, 1.000000000000000000, 0.8660254037844387076, 1.000000000000000000, 0.8660254037844387076, 1.000000000000000000, 0.8660254037844387076, 1.000000000000000000, 0.8660254037844387076, 1.000000000000000000, 0.8660254037844387076, 1.000000000000000000, 0.8660254037844387076, 1.000000000000000000, 0.8660254037844387076, 1.000000000000000000, 0.8660254037844387076, 1.000000000000000000, 0.8660254037844387076, 1.000000000000000000, 0.8660254037844387076, 1.000000000000000000, 0.8660254037844387076, 1.000000000000000000, 0.8660254037844387076, 1.000000000000000000, 0.8660254037844387076, 1.000000000000000000, 0.8660254037844387076, 1.000000000000000000, 0.8660254037844387076, 1.000000000000000000, 0.8660254037844387076, 1.000000000000000000, 0.8660254037844387076, 1.000000000000000000, 0.8660254037844387076, 1.000000000000000000, 0.8660254037844387076, 1.000000000000000000, 0.8660254037844387076, 1.000000000000000000, 0.8660254037844387076, 1.000000000000000000, 0.8660254037844387076, 1.000000000000000000, 0.8660254037844387076, 1.000000000000000000, 0.8660254037844387076, 1.000000000000000000, 0.8660254037844387076, 1.000000000000000000, 0.8660254037844387076, 1.000000000000000000, 0.8660254037844387076, 1.000000000000000000, 0.8660254037844387076, 1.000000000000000000, 0.8660254037844387076, 1.000000000000000000, 0.8660254037844387076, 1.000000000000000000, 0.8660254037844387076, 1.000000000000000000, 0.8660254037844387076, 1.000000000000000000, 0.8660254037844387076, 1.000000000000000000, 0.8660254037844387076, 1.000000000000000000, 0.8660254037844387076, 1.000000000000000000, 0.8660254037844387076, 1.000000000000000000, 0.8660254037844387076, 1.000000000000000000, 0.8660254037844387076, 1.000000000000000000, 0.8660254037844387076, 1.000000000000000000, 0.8660254037844387076, 1.000000000000000000, 0.8660254037844387076, 1.000000000000000000, 0.8660254037844387076, 1.000000000000000000, 0.8660254037844387076, 1.000000000000000000, 0.8660254037844387076, 1.000000000000000000, 0.8660254037844387076, 1.000000000000000000, 0.8660254037844387076, 1.000000000000000000, 0.8660254037844387076, 1.000000000000000000, 0.8660254037844387076, 1.000000000000000000, 0.8660254037844387076, 1.000000000000000000, 0.8660254037844387076, 1.000000000000000000, 0.8660254037844387076, 1.000000000000000000, 0.8660254037844387076, 1.000000000000000000, 0.8660254037844387076, 1.000000000000000000, 0.8660254037844387076, 1.000000000000000000, 0.8660254037844387076, 1.000000000000000000, 0.8660254037844387076, 1.000000000000000000, 0.8660254037844387076, 1.000000000000000000, 0.8660254037844387076, 1.000000000000000000, 0.8660254037844387076, 1.000000000000000000, 0.8660254037844387076, 1.000000000000000000, 0.8660254037844387076, 1.000000000000000000, 0.8660254037844387076, 1.000000000000000000, 0.8660254037844387076, 1.000000000000000000, 0.8660254037844387076, 1.000000000000000000, 0.8660254037844387076, 1.000000000000000000, 0.8660254037844387076, 1.000000000000000000, 0.8660254037844387076, 1.000000000000000000, 0.8660254037844387076, 1.000000000000000000, 0.8660254037844387076, 1.000000000000000000, 0.8660254037844387076, 1.000000000000000000, 0.8660254037844387076, 1.000000000000000000, 0.8660254037844387076, 1.000000000000000000, 0.8660254037844387076, 1.000000000000000000, 0.8660254037844387076, 1.000000000000000000, 0.8660254037844387076, 1.000000000000000000, 0.8660254037844387076, 1.000000000000000000, 0.8660254037844387076, 1.000000000000000000, 0.8660254037844387076, 1.000000000000000000, 0.8660254037844387076, 1.000000000000000000, 0.8660254037844387076, 1.000000000000000000, 0.8660254037844387076, 1.000000000000000000, 0.8660254037844387076, 1.000000000000000000, 0.8660254037844387076, 1.000000000000000000, 0.8660254037844387076, 1.000000000000000000, 0.8660254037844387076, 1.000000000000000000, 0.8660254037844387076, 1.000000000000000000, 0.8660254037844387076, 1.000000000000000000, 0.8660254037844387076, 1.000000000000000000, 0.8660254037844387076, 1.000000000000000000, 0.8660254037844387076, 1.000000000000000000, 0.8660254037844387076, 1.000000000000000000, 0.8660254037844387076, 1.000000000000000000, 0.8660254037844387076, 1.000000000000000000, 0.8660254037844387076, 1.000000000000000000, 0.8660254037844387076, 1.000000000000000000, 0.8660254037844387076, 1.000000000000000000, 0.8660254037844387076, 1.000000000000000000, 0.8660254037844387076, 1.000000000000000000, 0.8660254037844387076, 1.000000000000000000, 0.8660254037844387076, 1.000000000000000000, 0.8660254037844387076, 1.000000000000000000, 0.8660254037844387076, 1.000000000000000000, 0.8660254037844387076, 1.000000000000000000, 0.8660254037844387076, 1.000000000000000000, 0.8660254037844387076, 1.000000000000000000, 0.8660254037844387076, 1.000000000000000000, 0.8660254037844387076, 1.000000000000000000, 0.8660254037844387076, 1.000000000000000000, 0.8660254037844387076, 1.000000000000000000, 0.8660254037844387076, 1.000000000000000000, 0.8660254037844387076, 1.000000000000000000, 0.8660254037844387076, 1.000000000000000000, 0.8660254037844387076, 1.000000000000000000, 0.8660254037844387076, 1.000000000000000000, 0.8660254037844387076, 1.000000000000000000, 0.8660254037844387076, 1.000000000000000000, 0.8660254037844387076, 1.000000000000000000, 0.8660254037844387076, 1.000000000000000000, 0.8660254037844387076, 1.000000000000000000, 0.8660254037844387076, 1.000000000000000000, 0.8660254037844387076, 1.000000000000000000, 0.8660254037844387076, 1.000000000000000000, 0.8660254037844387076, 1.000000000000000000, 0.8660254037844387076, 1.000000000000000000, 0.8660254037844387076, 1.000000000000000000, 0.8660254037844387076, 1.000000000000000000, 0.8660254037844387076, 1.000000000000000000, 0.8660254037844387076, 1.000000000000000000, 0.8660254037844387076, 1.000000000000000000, 0.8660254037844387076, 1.000000000000000000, 0.8660254037844387076, 1.000000000000000000, 0.8660254037844387076, 1.000000000000000000, 0.8660254037844387076, 1.000000000000000000, 0.8660254037844387076, 1.000000000000000000, 0.8660254037844387076, 1.000000000000000000, 0.8660254037844387076, 1.000000000000000000, 0.8660254037844387076, 1.000000000000000000, 0.8660254037844387076, 1.000000000000000000, 0.8660254037844387076, 1.000000000000000000, 0.8660254037844387076, 1.000000000000000000, 0.8660254037844387076, 1.000000000000000000, 0.8660254037844387076, 1.000000000000000000, 0.8660254037844387076, 1.000000000000000000, 0.8660254037844387076, 1.000000000000000000, 0.8660254037844387076, 1.000000000000000000, 0.8660254037844387076, 1.000000000000000000, 0.8660254037844387076, 1.000000000000000000, 0.8660254037844387076, 1.000000000000000000, 0.8660254037844387076, 1.000000000000000000, 0.8660254037844387076, 1.000000000000000000, 0.8660254037844387076, 1.000000000000000000, 0.8660254037844387076, 1.000000000000000000, 0.8660254037844387076, 1.000000000000000000, 0.8660254037844387076, 1.000000000000000000, 0.8660254037844387076, 1.000000000000000000, 0.8660254037844387076, 1.000000000000000000, 0.8660254037844387076, 1.000000000000000000, 0.8660254037844387076, 1.000000000000000000, 0.8660254037844387076, 1.000000000000000000, 0.8660254037844387076, 1.000000000000000000, 0.8660254037844387076, 1.000000000000000000, 0.8660254037844387076, 1.000000000000000000, 0.8660254037844387076, 1.000000000000000000, 0.8660254037844387076, 1.000000000000000000, 0.8660254037844387076, 1.000000000000000000, 0.8660254037844387076, 1.000000000000000000, 0.8660254037844387076, 1.000000000000000000, 0.8660254037844387076, 1.000000000000000000, 0.8660254037844387076, 1.000000000000000000, 0.8660254037844387076, 1.000000000000000000, 0.8660254037844387076, 1.000000000000000000, 0.8660254037844387076, 1.000000000000000000, 0.8660254037844387076, 1.000000000000000000, 0.8660254037844387076, 1.000000000000000000, 0.8660254037844387076, 1.000000000000000000, 0.8660254037844387076, 1.000000000000000000, 0.8660254037844387076, 1.000000000000000000, 0.8660254037844387076, 1.000000000000000000, 0.8660254037844387076, 1.000000000000000000, 0.8660254037844387076, 1.000000000000000000, 0.8660254037844387076, 1.000000000000000000, 0.8660254037844387076, 1.000000000000000000, 0.8660254037844387076, 1.000000000000000000, 0.8660254037844387076, 1.000000000000000000, 0.8660254037844387076, 1.000000000000000000, 0.8660254037844387076, 1.000000000000000000, 0.8660254037844387076, 1.000000000000000000, 0.8660254037844387076, 1.000000000000000000, 0.8660254037844387076, 1.000000000000000000, 0.8660254037844387076, 1.000000000000000000, 0.8660254037844387076, 1.000000000000000000, 0.8660254037844387076, 1.000000000000000000, 0.8660254037844387076, 1.000000000000000000, 0.8660254037844387076, 1.000000000000000000, 0.8660254037844387076, 1.000000000000000000, 0.8660254037844387076, 1.000000000000000000, 0.8660254037844387076, 1.000000000000000000, 0.8660254037844387076, 1.000000000000000000, 0.8660254037844387076, 1.000000000000000000, 0.8660254037844387076, 1.000000000000000000, 0.8660254037844387076, 1.000000000000000000, 0.8660254037844387076, 1.000000000000000000, 0.8660254037844387076, 1.000000000000000000, 0.8660254037844387076, 1.000000000000000000, 0.8660254037844387076, 1.000000000000000000, 0.8660254037844387076, 1.000000000000000000, 0.8660254037844387076, 1.000000000000000000, 0.8660254037844387076, 1.000000000000000000, 0.8660254037844387076, 1.000000000000000000, 0.8660254037844387076, 1.000000000000000000, 0.8660254037844387076, 1.000000000000000000, 0.8660254037844387076, 1.000000000000000000, 0.8660254037844387076, 1.000000000000000000, 0.8660254037844387076, 1.000000000000000000, 0.8660254037844387076, 1.000000000000000000, 0.8660254037844387076, 1.000000000000000000, 0.8660254037844387076, 1.000000000000000000, 0.8660254037844387076, 1.000000000000000000, 0.8660254037844387076, 1.000000000000000000, 0.8660254037844387076, 1.000000000000000000, 0.8660254037844387076, 1.000000000000000000, 0.8660254037844387076, 1.000000000000000000, 0.8660254037844387076, 1.000000000000000000, 0.8660254037844387076, 1.000000000000000000, 0.8660254037844387076, 1.000000000000000000, 0.8660254037844387076, 1.000000000000000000, 0.8660254037844387076, 1.000000000000000000, 0.8660254037844387076, 1.000000000000000000, 0.8660254037844387076, 1.000000000000000000, 0.8660254037844387076, 1.000000000000000000, 0.8660254037844387076, 1.000000000000000000, 0.8660254037844387076, 1.000000000000000000, 0.8660254037844387076, 1.000000000000000000, 0.8660254037844387076, 1.000000000000000000, 0.8660254037844387076, 1.000000000000000000, 0.8660254037844387076, 1.000000000000000000, 0.8660254037844387076, 1.000000000000000000, 0.8660254037844387076, 1.000000000000000000, 0.8660254037844387076, 1.000000000000000000, 0.8660254037844387076, 1.000000000000000000, 0.8660254037844387076, 1.000000000000000000, 0.8660254037844387076, 1.000000000000000000, 0.8660254037844387076, 1.000000000000000000, 0.8660254037844387076, 1.000000000000000000, 0.8660254037844387076, 1.000000000000000000, 0.8660254037844387076, 1.000000000000000000, 0.8660254037844387076, 1.000000000000000000, 0.8660254037844387076, 1.000000000000000000, 0.8660254037844387076, 1.000000000000000000, 0.8660254037844387076, 1.000000000000000000, 0.8660254037844387076, 1.000000000000000000, 0.8660254037844387076, 1.000000000000000000, 0.8660254037844387076, 1.000000000000000000, 0.8660254037844387076, 1.000000000000000000, 0.8660254037844387076, 1.000000000000000000, 0.8660254037844387076, 1.000000000000000000, 0.8660254037844387076, 1.000000000000000000, 0.8660254037844387076, 1.000000000000000000, 0.8660254037844387076, 1.000000000000000000, 0.8660254037844387076, 1.000000000000000000, 0.8660254037844387076, 1.000000000000000000, 0.8660254037844387076, 1.000000000000000000, 0.8660254037844387076, 1.000000000000000000, 0.8660254037844387076, 1.000000000000000000, 0.8660254037844387076, 1.000000000000000000, 0.8660254037844387076, 1.000000000000000000, 0.8660254037844387076, 1.000000000000000000, 0.8660254037844387076, 1.000000000000000000, 0.8660254037844387076, 1.000000000000000000, 0.8660254037844387076, 1.000000000000000000, 0.8660254037844387076, 1.000000000000000000, 0.8660254037844387076, 1.000000000000000000, 0.8660254037844387076, 1.000000000000000000, 0.8660254037844387076, 1.000000000000000000, 0.8660254037844387076, 1.000000000000000000, 0.8660254037844387076, 1.000000000000000000, 0.8660254037844387076, 1.000000000000000000, 0.8660254037844387076, 1.000000000000000000, 0.8660254037844387076, 1.000000000000000000, 0.8660254037844387076, 1.000000000000000000, 0.8660254037844387076, 1.000000000000000000, 0.8660254037844387076, 1.000000000000000000, 0.8660254037844387076, 1.000000000000000000, 0.8660254037844387076, 1.000000000000000000, 0.8660254037844387076, 1.000000000000000000, 0.8660254037844387076, 1.000000000000000000, 0.8660254037844387076, 1.000000000000000000, 0.8660254037844387076, 1.000000000000000000, 0.8660254037844387076, 1.000000000000000000, 0.8660254037844387076, 1.000000000000000000, 0.8660254037844387076, 1.000000000000000000, 0.8660254037844387076, 1.000000000000000000, 0.8660254037844387076, 1.000000000000000000, 0.8660254037844387076, 1.000000000000000000, 0.8660254037844387076, 1.000000000000000000, 0.8660254037844387076, 1.000000000000000000, 0.8660254037844387076, 1.000000000000000000, 0.8660254037844387076, 1.000000000000000000, 0.8660254037844387076, 1.000000000000000000, 0.8660254037844387076, 1.000000000000000000, 0.8660254037844387076, 1.000000000000000000, 0.8660254037844387076, 1.000000000000000000, 0.8660254037844387076, 1.000000000000000000, 0.8660254037844387076, 1.000000000000000000, 0.8660254037844387076, 1.000000000000000000, 0.8660254037844387076, 1.000000000000000000, 0.8660254037844387076, 1.000000000000000000, 0.8660254037844387076, 1.000000000000000000, 0.8660254037844387076, 1.000000000000000000, 0.8660254037844387076, 1.000000000000000000, 0.8660254037844387076, 1.000000000000000000, 0.8660254037844387076, 1.000000000000000000, 0.8660254037844387076, 1.000000000000000000, 0.8660254037844387076, 1.000000000000000000, 0.8660254037844387076, 1.000000000000000000, 0.8660254037844387076, 1.000000000000000000, 0.8660254037844387076, 1.000000000000000000, 0.8660254037844387076, 1.000000000000000000, 0.8660254037844387076, 1.000000000000000000, 0.8660254037844387076, 1.000000000000000000, 0.8660254037844387076, 1.000000000000000000, 0.8660254037844387076, 1.000000000000000000, 0.8660254037844387076, 1.000000000000000000, 0.8660254037844387076, 1.000000000000000000, 0.8660254037844387076, 1.000000000000000000, 0.8660254037844387076, 1.000000000000000000, 0.8660254037844387076, 1.000000000000000000, 0.8660254037844387076, 1.000000000000000000, 0.8660254037844387076, 1.000000000000000000, 0.8660254037844387076, 1.000000000000000000, 0.8660254037844387076, 1.000000000000000000, 0.8660254037844387076, 1.000000000000000000, 0.8660254037844387076, 1.000000000000000000, 0.8660254037844387076, 1.000000000000000000, 0.8660254037844387076, 1.000000000000000000, 0.8660254037844387076, 1.000000000000000000, 0.8660254037844387076, 1.000000000000000000, 0.8660254037844387076, 1.000000000000000000, 0.8660254037844387076, 1.000000000000000000, 0.8660254037844387076, 1.000000000000000000, 0.8660254037844387076, 1.000000000000000000, 0.8660254037844387076, 1.000000000000000000, 0.8660254037844387076, 1.000000000000000000, 0.8660254037844387076, 1.000000000000000000, 0.8660254037844387076, 1.000000000000000000, 0.8660254037844387076, 1.000000000000000000, 0.8660254037844387076, 1.000000000000000000, 0.8660254037844387076, 1.000000000000000000, 0.8660254037844387076, 1.000000000000000000, 0.8660254037844387076, 1.000000000000000000, 0.8660254037844387076, 1.000000000000000000, 0.8660254037844387076, 1.000000000000000000, 0.8660254037844387076, 1.000000000000000000, 0.8660254037844387076, 1.000000000000000000, 0.8660254037844387076, 1.000000000000000000, 0.8660254037844387076, 1.000000000000000000, 0.8660254037844387076, 1.000000000000000000, 0.8660254037844387076, 1.000000000000000000, 0.8660254037844387076, 1.000000000000000000, 0.8660254037844387076, 1.000000000000000000, 0.8660254037844387076, 1.000000000000000000, 0.8660254037844387076, 1.000000000000000000, 0.8660254037844387076, 1.000000000000000000, 0.8660254037844387076, 1.000000000000000000, 0.8660254037844387076, 1.000000000000000000, 0.8660254037844387076, 1.000000000000000000, 0.8660254037844387076, 1.000000000000000000, 0.8660254037844387076, 1.000000000000000000, 0.8660254037844387076, 1.000000000000000000, 0.8660254037844387076, 1.000000000000000000, 0.8660254037844387076, 1.000000000000000000, 0.8660254037844387076, 1.000000000000000000, 0.8660254037844387076, 1.000000000000000000, 0.8660254037844387076, 1.000000000000000000, 0.8660254037844387076, 1.000000000000000000, 0.8660254037844387076, 1.000000000000000000, 0.8660254037844387076, 1.000000000000000000, 0.8660254037844387076, 1.000000000000000000, 0.8660254037844387076, 1.000000000000000000, 0.8660254037844387076, 1.000000000000000000, 0.8660254037844387076, 1.000000000000000000, 0.8660254037844387076, 1.000000000000000000, 0.8660254037844387076, 1.000000000000000000, 0.8660254037844387076, 1.000000000000000000, 0.8660254037844387076, 1.000000000000000000, 0.8660254037844387076, 1.000000000000000000, 0.8660254037844387076, 1.000000000000000000, 0.8660254037844387076, 1.000000000000000000, 0.8660254037844387076, 1.000000000000000000, 0.8660254037844387076, 1.000000000000000000, 0.8660254037844387076, 1.000000000000000000, 0.8660254037844387076, 1.000000000000000000, 0.8660254037844387076, 1.000000000000000000, 0.8660254037844387076, 1.000000000000000000, 0.8660254037844387076, 1.000000000000000000, 0.8660254037844387076, 1.000000000000000000, 0.8660254037844387076, 1.000000000000000000, 0.8660254037844387076, 1.000000000000000000, 0.8660254037844387076, 1.000000000000000000, 0.8660254037844387076, 1.000000000000000000, 0.8660254037844387076, 1.000000000000000000, 0.8660254037844387076, 1.000000000000000000, 0.8660254037844387076, 1.000000000000000000, 0.8660254037844387076, 1.000000000000000000, 0.8660254037844387076, 1.000000000000000000, 0.8660254037844387076, 1.000000000000000000, 0.8660254037844387076, 1.000000000000000000, 0.8660254037844387076, 1.000000000000000000, 0.8660254037844387076, 1.000000000000000000, 0.8660254037844387076, 1.000000000000000000, 0.8660254037844387076, 1.000000000000000000, 0.8660254037844387076, 1.000000000000000000, 0.8660254037844387076, 1.000000000000000000, 0.8660254037844387076, 1.000000000000000000, 0.8660254037844387076, 1.000000000000000000, 0.8660254037844387076, 1.000000000000000000, 0.8660254037844387076, 1.000000000000000000, 0.8660254037844387076, 1.000000000000000000, 0.8660254037844387076, 1.000000000000000000, 0.8660254037844387076, 1.000000000000000000, 0.8660254037844387076, 1.000000000000000000, 0.8660254037844387076, 1.000000000000000000, 0.8660254037844387076, 1.000000000000000000, 0.8660254037844387076, 1.000000000000000000, 0.8660254037844387076, 1.000000000000000000, 0.8660254037844387076, 1.000000000000000000, 0.8660254037844387076, 1.000000000000000000, 0.8660254037844387076, 1.000000000000000000, 0.8660254037844387076, 1.000000000000000000, 0.8660254037844387076, 1.000000000000000000, 0.8660254037844387076, 1.000000000000000000, 0.8660254037844387076, 1.000000000000000000, 0.8660254037844387076, 1.000000000000000000, 0.8660254037844387076, 1.000000000000000000, 0.8660254037844387076, 1.000000000000000000, 0.8660254037844387076, 1.000000000000000000, 0.8660254037844387076, 1.000000000000000000, 0.8660254037844387076, 1.000000000000000000, 0.8660254037844387076, 1.000000000000000000, 0.8660254037844387076, 1.000000000000000000, 0.8660254037844387076, 1.000000000000000000, 0.8660254037844387076, 1.000000000000000000, 0.8660254037844387076, 1.000000000000000000, 0.8660254037844387076, 1.000000000000000000, 0.8660254037844387076, 1.000000000000000000, 0.8660254037844387076, 1.000000000000000000, 0.8660254037844387076, 1.000000000000000000, 0.8660254037844387076, 1.000000000000000000, 0.8660254037844387076, 1.000000000000000000, 0.8660254037844387076, 1.000000000000000000, 0.8660254037844387076, 1.000000000000000000, 0.8660254037844387076, 1.000000000000000000, 0.8660254037844387076, 1.000000000000000000, 0.8660254037844387076, 1.000000000000000000, 0.8660254037844387076, 1.000000000000000000, 0.8660254037844387076, 1.000000000000000000, 0.8660254037844387076, 1.000000000000000000, 0.8660254037844387076, 1.000000000000000000, 0.8660254037844387076, 1.000000000000000000, 0.8660254037844387076, 1.000000000000000000, 0.8660254037844387076, 1.000000000000000000, 0.8660254037844387076, 1.000000000000000000, 0.8660254037844387076, 1.000000000000000000, 0.8660254037844387076, 1.000000000000000000, 0.8660254037844387076, 1.000000000000000000, 0.8660254037844387076, 1.000000000000000000, 0.8660254037844387076, 1.000000000000000000, 0.8660254037844387076, 1.000000000000000000, 0.8660254037844387076, 1.000000000000000000, 0.8660254037844387076, 1.000000000000000000, 0.8660254037844387076, 1.000000000000000000, 0.8660254037844387076, 1.000000000000000000, 0.8660254037844387076, 1.000000000000000000, 0.8660254037844387076, 1.000000000000000000, 0.8660254037844387076, 1.000000000000000000, 0.8660254037844387076, 1.000000000000000000, 0.8660254037844387076, 1.000000000000000000, 0.8660254037844387076, 1.000000000000000000, 0.8660254037844387076, 1.000000000000000000, 0.8660254037844387076, 1.000000000000000000, 0.8660254037844387076, 1.000000000000000000, 0.8660254037844387076, 1.000000000000000000, 0.8660254037844387076, 1.000000000000000000, 0.8660254037844387076, 1.000000000000000000, 0.8660254037844387076, 1.000000000000000000, 0.8660254037844387076, 1.000000000000000000, 0.8660254037844387076, 1.000000000000000000, 0.8660254037844387076, 1.000000000000000000, 0.8660254037844387076, 1.000000000000000000, 0.8660254037844387076, 1.000000000000000000, 0.8660254037844387076, 1.000000000000000000, 0.8660254037844387076, 1.000000000000000000, 0.8660254037844387076, 1.000000000000000000, 0.8660254037844387076, 1.000000000000000000, 0.8660254037844387076, 1.000000000000000000, 0.8660254037844387076, 1.000000000000000000, 0.8660254037844387076, 1.000000000000000000, 0.8660254037844387076, 1.000000000000000000, 0.8660254037844387076, 1.000000000000000000, 0.8660254037844387076, 1.000000000000000000, 0.8660254037844387076, 1.000000000000000000, 0.8660254037844387076, 1.000000000000000000, 0.8660254037844387076, 1.000000000000000000, 0.8660254037844387076, 1.000000000000000000, 0.8660254037844387076, 1.000000000000000000, 0.8660254037844387076, 1.000000000000000000, 0.8660254037844387076, 1.000000000000000000, 0.8660254037844387076, 1.000000000000000000, 0.8660254037844387076, 1.000000000000000000, 0.8660254037844387076, 1.000000000000000000, 0.8660254037844387076, 1.000000000000000000, 0.8660254037844387076, 1.000000000000000000, 0.8660254037844387076, 1.000000000000000000, 0.8660254037844387076, 1.000000000000000000, 0.8660254037844387076, 1.000000000000000000, 0.8660254037844387076, 1.000000000000000000, 0.8660254037844387076, 1.000000000000000000, 0.8660254037844387076, 1.000000000000000000, 0.8660254037844387076, 1.000000000000000000, 0.8660254037844387076, 1.000000000000000000, 0.8660254037844387076, 1.000000000000000000, 0.8660254037844387076, 1.000000000000000000, 0.8660254037844387076, 1.000000000000000000, 0.8660254037844387076, 1.000000000000000000, 0.8660254037844387076, 1.000000000000000000, 0.8660254037844387076, 1.000000000000000000, 0.8660254037844387076, 1.000000000000000000, 0.8660254037844387076, 1.000000000000000000, 0.8660254037844387076, 1.000000000000000000, 0.8660254037844387076, 1.000000000000000000, 0.8660254037844387076, 1.000000000000000000, 0.8660254037844387076, 1.000000000000000000, 0.8660254037844387076, 1.000000000000000000, 0.8660254037844387076, 1.000000000000000000, 0.8660254037844387076, 1.000000000000000000, 0.8660254037844387076, 1.000000000000000000, 0.8660254037844387076, 1.000000000000000000, 0.8660254037844387076, 1.000000000000000000, 0.8660254037844387076, 1.000000000000000000, 0.8660254037844387076, 1.000000000000000000, 0.8660254037844387076, 1.000000000000000000, 0.8660254037844387076, 1.000000000000000000, 0.8660254037844387076, 1.000000000000000000, 0.8660254037844387076, 1.000000000000000000, 0.8660254037844387076, 1.000000000000000000, 0.8660254037844387076, 1.000000000000000000, 0.8660254037844387076, 1.000000000000000000, 0.8660254037844387076, 1.000000000000000000, 0.8660254037844387076, 1.000000000000000000, 0.8660254037844387076, 1.000000000000000000, 0.8660254037844387076, 1.000000000000000000, 0.8660254037844387076, 1.000000000000000000, 0.8660254037844387076, 1.000000000000000000, 0.8660254037844387076, 1.000000000000000000, 0.8660254037844387076, 1.000000000000000000, 0.8660254037844387076, 1.000000000000000000, 0.8660254037844387076, 1.000000000000000000, 0.8660254037844387076, 1.000000000000000000, 0.8660254037844387076, 1.000000000000000000, 0.8660254037844387076, 1.000000000000000000, 0.8660254037844387076, 1.000000000000000000, 0.8660254037844387076, 1.000000000000000000, 0.8660254037844387076, 1.000000000000000000, 0.8660254037844387076, 1.000000000000000000, 0.8660254037844387076, 1.000000000000000000, 0.8660254037844387076, 1.000000000000000000, 0.8660254037844387076, 1.000000000000000000, 0.8660254037844387076, 1.000000000000000000, 0.8660254037844387076, 1.000000000000000000, 0.8660254037844387076, 1.000000000000000000, 0.8660254037844387076, 1.000000000000000000, 0.8660254037844387076, 1.000000000000000000, 0.8660254037844387076, 1.000000000000000000, 0.8660254037844387076, 1.000000000000000000, 0.8660254037844387076, 1.000000000000000000, 0.8660254037844387076, 1.000000000000000000, 0.8660254037844387076, 1.000000000000000000, 0.8660254037844387076, 1.000000000000000000, 0.8660254037844387076, 1.000000000000000000, 0.8660254037844387076, 1.000000000000000000, 0.8660254037844387076, 1.000000000000000000, 0.8660254037844387076, 1.000000000000000000, 0.8660254037844387076, 1.000000000000000000, 0.8660254037844387076, 1.000000000000000000, 0.8660254037844387076, 1.000000000000000000, 0.8660254037844387076, 1.000000000000000000, 0.8660254037844387076, 1.000000000000000000, 0.8660254037844387076, 1.000000000000000000, 0.8660254037844387076, 1.000000000000000000, 0.8660254037844387076, 1.000000000000000000, 0.8660254037844387076, 1.000000000000000000, 0.8660254037844387076, 1.000000000000000000, 0.8660254037844387076, 1.000000000000000000, 0.8660254037844387076, 1.000000000000000000, 0.8660254037844387076, 1.000000000000000000, 0.8660254037844387076, 1.000000000000000000, 0.8660254037844387076, 1.000000000000000000, 0.8660254037844387076, 1.000000000000000000, 0.8660254037844387076, 1.000000000000000000, 0.8660254037844387076, 1.000000000000000000, 0.8660254037844387076, 1.000000000000000000, 0.8660254037844387076, 1.000000000000000000, 0.8660254037844387076, 1.000000000000000000, 0.8660254037844387076, 1.000000000000000000, 0.8660254037844387076, 1.000000000000000000, 0.8660254037844387076, 1.000000000000000000, 0.8660254037844387076, 1.000000000000000000, 0.8660254037844387076, 1.000000000000000000, 0.8660254037844387076, 1.000000000000000000, 0.8660254037844387076, 1.000000000000000000, 0.8660254037844387076, 1.000000000000000000, 0.8660254037844387076, 1.000000000000000000, 0.8660254037844387076, 1.000000000000000000, 0.8660254037844387076, 1.000000000000000000, 0.8660254037844387076, 1.000000000000000000, 0.8660254037844387076, 1.000000000000000000, 0.8660254037844387076, 1.000000000000000000, 0.8660254037844387076, 1.000000000000000000, 0.8660254037844387076, 1.000000000000000000, 0.8660254037844387076, 1.000000000000000000),
 ( 1.000000000000000000, 0.8660254037844387076, 1.000000000000000000, 0.8660254037844387076, 1.000000000000000000, 0.8660254037844387076, 1.000000000000000000, 0.8660254037844387076, 1.000000000000000000, 0.8660254037844387076, 1.000000000000000000, 0.8660254037844387076, 1.000000000000000000, 0.8660254037844387076, 1.000000000000000000, 0.8660254037844387076, 1.000000000000000000, 0.8660254037844387076, 1.000000000000000000, 0.8660254037844387076, 1.000000000000000000, 0.8660254037844387076, 1.000000000000000000, 0.8660254037844387076, 1.000000000000000000, 0.8660254037844387076, 1.000000000000000000, 0.8660254037844387076, 1.000000000000000000, 0.8660254037844387076, 1.000000000000000000, 0.8660254037844387076, 1.000000000000000000, 0.8660254037844387076, 1.000000000000000000, 0.8660254037844387076, 1.000000000000000000, 0.8660254037844387076, 1.000000000000000000, 0.8660254037844387076, 1.000000000000000000, 0.8660254037844387076, 1.000000000000000000, 0.8660254037844387076, 1.000000000000000000, 0.8660254037844387076, 1.000000000000000000, 0.8660254037844387076, 1.000000000000000000, 0.8660254037844387076, 1.000000000000000000, 0.8660254037844387076, 1.000000000000000000, 0.8660254037844387076, 1.000000000000000000, 0.8660254037844387076, 1.000000000000000000, 0.8660254037844387076, 1.000000000000000000, 0.8660254037844387076, 1.000000000000000000, 0.8660254037844387076, 1.000000000000000000, 0.8660254037844387076, 1.000000000000000000, 0.8660254037844387076, 1.000000000000000000, 0.8660254037844387076, 1.000000000000000000, 0.8660254037844387076, 1.000000000000000000, 0.8660254037844387076, 1.000000000000000000, 0.8660254037844387076, 1.000000000000000000, 0.8660254037844387076, 1.000000000000000000, 0.8660254037844387076, 1.000000000000000000, 0.8660254037844387076, 1.000000000000000000, 0.8660254037844387076, 1.000000000000000000, 0.8660254037844387076, 1.000000000000000000, 0.8660254037844387076, 1.000000000000000000, 0.8660254037844387076, 1.000000000000000000, 0.8660254037844387076, 1.000000000000000000, 0.8660254037844387076, 1.000000000000000000, 0.8660254037844387076, 1.000000000000000000, 0.8660254037844387076, 1.000000000000000000, 0.8660254037844387076, 1.000000000000000000, 0.8660254037844387076, 1.000000000000000000, 0.8660254037844387076, 1.000000000000000000, 0.8660254037844387076, 1.000000000000000000, 0.8660254037844387076, 1.000000000000000000, 0.8660254037844387076, 1.000000000000000000, 0.8660254037844387076, 1.000000000000000000, 0.8660254037844387076, 1.000000000000000000, 0.8660254037844387076, 1.000000000000000000, 0.8660254037844387076, 1.000000000000000000, 0.8660254037844387076, 1.000000000000000000, 0.8660254037844387076, 1.000000000000000000, 0.8660254037844387076, 1.000000000000000000, 0.8660254037844387076, 1.000000000000000000, 0.8660254037844387076, 1.000000000000000000, 0.8660254037844387076, 1.000000000000000000, 0.8660254037844387076, 1.000000000000000000, 0.8660254037844387076, 1.000000000000000000, 0.8660254037844387076, 1.000000000000000000, 0.8660254037844387076, 1.000000000000000000, 0.8660254037844387076, 1.000000000000000000, 0.8660254037844387076, 1.000000000000000000, 0.8660254037844387076, 1.000000000000000000, 0.8660254037844387076, 1.000000000000000000, 0.8660254037844387076, 1.000000000000000000, 0.8660254037844387076, 1.000000000000000000, 0.8660254037844387076, 1.000000000000000000, 0.8660254037844387076, 1.000000000000000000, 0.8660254037844387076, 1.000000000000000000, 0.8660254037844387076, 1.000000000000000000, 0.8660254037844387076, 1.000000000000000000, 0.8660254037844387076, 1.000000000000000000, 0.8660254037844387076, 1.000000000000000000, 0.8660254037844387076, 1.000000000000000000, 0.8660254037844387076, 1.000000000000000000, 0.8660254037844387076, 1.000000000000000000, 0.8660254037844387076, 1.000000000000000000, 0.8660254037844387076, 1.000000000000000000, 0.8660254037844387076, 1.000000000000000000, 0.8660254037844387076, 1.000000000000000000, 0.8660254037844387076, 1.000000000000000000, 0.8660254037844387076, 1.000000000000000000, 0.8660254037844387076, 1.000000000000000000, 0.8660254037844387076, 1.000000000000000000, 0.8660254037844387076, 1.000000000000000000, 0.8660254037844387076, 1.000000000000000000, 0.8660254037844387076, 1.000000000000000000, 0.8660254037844387076, 1.000000000000000000, 0.8660254037844387076, 1.000000000000000000, 0.8660254037844387076, 1.000000000000000000, 0.8660254037844387076, 1.000000000000000000, 0.8660254037844387076, 1.000000000000000000, 0.8660254037844387076, 1.000000000000000000, 0.8660254037844387076, 1.000000000000000000, 0.8660254037844387076, 1.000000000000000000, 0.8660254037844387076, 1.000000000000000000, 0.8660254037844387076, 1.000000000000000000, 0.8660254037844387076, 1.000000000000000000, 0.8660254037844387076, 1.000000000000000000, 0.8660254037844387076, 1.000000000000000000, 0.8660254037844387076, 1.000000000000000000, 0.8660254037844387076, 1.000000000000000000, 0.8660254037844387076, 1.000000000000000000, 0.8660254037844387076, 1.000000000000000000, 0.8660254037844387076, 1.000000000000000000, 0.8660254037844387076, 1.000000000000000000, 0.8660254037844387076, 1.000000000000000000, 0.8660254037844387076, 1.000000000000000000, 0.8660254037844387076, 1.000000000000000000, 0.8660254037844387076, 1.000000000000000000, 0.8660254037844387076, 1.000000000000000000, 0.8660254037844387076, 1.000000000000000000, 0.8660254037844387076, 1.000000000000000000, 0.8660254037844387076, 1.000000000000000000, 0.8660254037844387076, 1.000000000000000000, 0.8660254037844387076, 1.000000000000000000, 0.8660254037844387076, 1.000000000000000000, 0.8660254037844387076, 1.000000000000000000, 0.8660254037844387076, 1.000000000000000000, 0.8660254037844387076, 1.000000000000000000, 0.8660254037844387076, 1.000000000000000000, 0.8660254037844387076, 1.000000000000000000, 0.8660254037844387076, 1.000000000000000000, 0.8660254037844387076, 1.000000000000000000, 0.8660254037844387076, 1.000000000000000000, 0.8660254037844387076, 1.000000000000000000, 0.8660254037844387076, 1.000000000000000000, 0.8660254037844387076, 1.000000000000000000, 0.8660254037844387076, 1.000000000000000000, 0.8660254037844387076, 1.000000000000000000, 0.8660254037844387076, 1.000000000000000000, 0.8660254037844387076, 1.000000000000000000, 0.8660254037844387076, 1.000000000000000000, 0.8660254037844387076, 1.000000000000000000, 0.8660254037844387076, 1.000000000000000000, 0.8660254037844387076, 1.000000000000000000, 0.8660254037844387076, 1.000000000000000000, 0.8660254037844387076, 1.000000000000000000, 0.8660254037844387076, 1.000000000000000000, 0.8660254037844387076, 1.000000000000000000, 0.8660254037844387076, 1.000000000000000000, 0.8660254037844387076, 1.000000000000000000, 0.8660254037844387076, 1.000000000000000000, 0.8660254037844387076, 1.000000000000000000, 0.8660254037844387076, 1.000000000000000000, 0.8660254037844387076, 1.000000000000000000, 0.8660254037844387076, 1.000000000000000000, 0.8660254037844387076, 1.000000000000000000, 0.8660254037844387076, 1.000000000000000000, 0.8660254037844387076, 1.000000000000000000, 0.8660254037844387076, 1.000000000000000000, 0.8660254037844387076, 1.000000000000000000, 0.8660254037844387076, 1.000000000000000000, 0.8660254037844387076, 1.000000000000000000, 0.8660254037844387076, 1.000000000000000000, 0.8660254037844387076, 1.000000000000000000, 0.8660254037844387076, 1.000000000000000000, 0.8660254037844387076, 1.000000000000000000, 0.8660254037844387076, 1.000000000000000000, 0.8660254037844387076, 1.000000000000000000, 0.8660254037844387076, 1.000000000000000000, 0.8660254037844387076, 1.000000000000000000, 0.8660254037844387076, 1.000000000000000000, 0.8660254037844387076, 1.000000000000000000, 0.8660254037844387076, 1.000000000000000000, 0.8660254037844387076, 1.000000000000000000, 0.8660254037844387076, 1.000000000000000000, 0.8660254037844387076, 1.000000000000000000, 0.8660254037844387076, 1.000000000000000000, 0.8660254037844387076, 1.000000000000000000, 0.8660254037844387076, 1.000000000000000000, 0.8660254037844387076, 1.000000000000000000, 0.8660254037844387076, 1.000000000000000000, 0.8660254037844387076, 1.000000000000000000, 0.8660254037844387076, 1.000000000000000000, 0.8660254037844387076, 1.000000000000000000, 0.8660254037844387076, 1.000000000000000000, 0.8660254037844387076, 1.000000000000000000, 0.8660254037844387076, 1.000000000000000000, 0.8660254037844387076, 1.000000000000000000, 0.8660254037844387076, 1.000000000000000000, 0.8660254037844387076, 1.000000000000000000, 0.8660254037844387076, 1.000000000000000000, 0.8660254037844387076, 1.000000000000000000, 0.8660254037844387076, 1.000000000000000000, 0.8660254037844387076, 1.000000000000000000, 0.8660254037844387076, 1.000000000000000000, 0.8660254037844387076, 1.000000000000000000, 0.8660254037844387076, 1.000000000000000000, 0.8660254037844387076, 1.000000000000000000, 0.8660254037844387076, 1.000000000000000000, 0.8660254037844387076, 1.000000000000000000, 0.8660254037844387076, 1.000000000000000000, 0.8660254037844387076, 1.000000000000000000, 0.8660254037844387076, 1.000000000000000000, 0.8660254037844387076, 1.000000000000000000, 0.8660254037844387076, 1.000000000000000000, 0.8660254037844387076, 1.000000000000000000, 0.8660254037844387076, 1.000000000000000000, 0.8660254037844387076, 1.000000000000000000, 0.8660254037844387076, 1.000000000000000000, 0.8660254037844387076, 1.000000000000000000, 0.8660254037844387076, 1.000000000000000000, 0.8660254037844387076, 1.000000000000000000, 0.8660254037844387076, 1.000000000000000000, 0.8660254037844387076, 1.000000000000000000, 0.8660254037844387076, 1.000000000000000000, 0.8660254037844387076, 1.000000000000000000, 0.8660254037844387076, 1.000000000000000000, 0.8660254037844387076, 1.000000000000000000, 0.8660254037844387076, 1.000000000000000000, 0.8660254037844387076, 1.000000000000000000, 0.8660254037844387076, 1.000000000000000000, 0.8660254037844387076, 1.000000000000000000, 0.8660254037844387076, 1.000000000000000000, 0.8660254037844387076, 1.000000000000000000, 0.8660254037844387076, 1.000000000000000000, 0.8660254037844387076, 1.000000000000000000, 0.8660254037844387076, 1.000000000000000000, 0.8660254037844387076, 1.000000000000000000, 0.8660254037844387076, 1.000000000000000000, 0.8660254037844387076, 1.000000000000000000, 0.8660254037844387076, 1.000000000000000000, 0.8660254037844387076, 1.000000000000000000, 0.8660254037844387076, 1.000000000000000000, 0.8660254037844387076, 1.000000000000000000, 0.8660254037844387076, 1.000000000000000000, 0.8660254037844387076, 1.000000000000000000, 0.8660254037844387076, 1.000000000000000000, 0.8660254037844387076, 1.000000000000000000, 0.8660254037844387076, 1.000000000000000000, 0.8660254037844387076, 1.000000000000000000, 0.8660254037844387076, 1.000000000000000000, 0.8660254037844387076, 1.000000000000000000, 0.8660254037844387076, 1.000000000000000000, 0.8660254037844387076, 1.000000000000000000, 0.8660254037844387076, 1.000000000000000000, 0.8660254037844387076, 1.000000000000000000, 0.8660254037844387076, 1.000000000000000000, 0.8660254037844387076, 1.000000000000000000, 0.8660254037844387076, 1.000000000000000000, 0.8660254037844387076, 1.000000000000000000, 0.8660254037844387076, 1.000000000000000000, 0.8660254037844387076, 1.000000000000000000, 0.8660254037844387076, 1.000000000000000000, 0.8660254037844387076, 1.000000000000000000, 0.8660254037844387076, 1.000000000000000000, 0.8660254037844387076, 1.000000000000000000, 0.8660254037844387076, 1.000000000000000000, 0.8660254037844387076, 1.000000000000000000, 0.8660254037844387076, 1.000000000000000000, 0.8660254037844387076, 1.000000000000000000, 0.8660254037844387076, 1.000000000000000000, 0.8660254037844387076, 1.000000000000000000, 0.8660254037844387076, 1.000000000000000000, 0.8660254037844387076, 1.000000000000000000, 0.8660254037844387076, 1.000000000000000000, 0.8660254037844387076, 1.000000000000000000, 0.8660254037844387076, 1.000000000000000000, 0.8660254037844387076, 1.000000000000000000, 0.8660254037844387076, 1.000000000000000000, 0.8660254037844387076, 1.000000000000000000, 0.8660254037844387076, 1.000000000000000000, 0.8660254037844387076, 1.000000000000000000, 0.8660254037844387076, 1.000000000000000000, 0.8660254037844387076, 1.000000000000000000, 0.8660254037844387076, 1.000000000000000000, 0.8660254037844387076, 1.000000000000000000, 0.8660254037844387076, 1.000000000000000000, 0.8660254037844387076, 1.000000000000000000, 0.8660254037844387076, 1.000000000000000000, 0.8660254037844387076, 1.000000000000000000, 0.8660254037844387076, 1.000000000000000000, 0.8660254037844387076, 1.000000000000000000, 0.8660254037844387076, 1.000000000000000000, 0.8660254037844387076, 1.000000000000000000, 0.8660254037844387076, 1.000000000000000000, 0.8660254037844387076, 1.000000000000000000, 0.8660254037844387076, 1.000000000000000000, 0.8660254037844387076, 1.000000000000000000, 0.8660254037844387076, 1.000000000000000000, 0.8660254037844387076, 1.000000000000000000, 0.8660254037844387076, 1.000000000000000000, 0.8660254037844387076, 1.000000000000000000, 0.8660254037844387076, 1.000000000000000000, 0.8660254037844387076, 1.000000000000000000, 0.8660254037844387076, 1.000000000000000000, 0.8660254037844387076, 1.000000000000000000, 0.8660254037844387076, 1.000000000000000000, 0.8660254037844387076, 1.000000000000000000, 0.8660254037844387076, 1.000000000000000000, 0.8660254037844387076, 1.000000000000000000, 0.8660254037844387076, 1.000000000000000000, 0.8660254037844387076, 1.000000000000000000, 0.8660254037844387076, 1.000000000000000000, 0.8660254037844387076, 1.000000000000000000, 0.8660254037844387076, 1.000000000000000000, 0.8660254037844387076, 1.000000000000000000, 0.8660254037844387076, 1.000000000000000000, 0.8660254037844387076, 1.000000000000000000, 0.8660254037844387076, 1.000000000000000000, 0.8660254037844387076, 1.000000000000000000, 0.8660254037844387076, 1.000000000000000000, 0.8660254037844387076, 1.000000000000000000, 0.8660254037844387076, 1.000000000000000000, 0.8660254037844387076, 1.000000000000000000, 0.8660254037844387076, 1.000000000000000000, 0.8660254037844387076, 1.000000000000000000, 0.8660254037844387076, 1.000000000000000000, 0.8660254037844387076, 1.000000000000000000, 0.8660254037844387076, 1.000000000000000000, 0.8660254037844387076, 1.000000000000000000, 0.8660254037844387076, 1.000000000000000000, 0.8660254037844387076, 1.000000000000000000, 0.8660254037844387076, 1.000000000000000000, 0.8660254037844387076, 1.000000000000000000, 0.8660254037844387076, 1.000000000000000000, 0.8660254037844387076, 1.000000000000000000, 0.8660254037844387076, 1.000000000000000000, 0.8660254037844387076, 1.000000000000000000, 0.8660254037844387076, 1.000000000000000000, 0.8660254037844387076, 1.000000000000000000, 0.8660254037844387076, 1.000000000000000000, 0.8660254037844387076, 1.000000000000000000, 0.8660254037844387076, 1.000000000000000000, 0.8660254037844387076, 1.000000000000000000, 0.8660254037844387076, 1.000000000000000000, 0.8660254037844387076, 1.000000000000000000, 0.8660254037844387076, 1.000000000000000000, 0.8660254037844387076, 1.000000000000000000, 0.8660254037844387076, 1.000000000000000000, 0.8660254037844387076, 1.000000000000000000, 0.8660254037844387076, 1.000000000000000000, 0.8660254037844387076, 1.000000000000000000, 0.8660254037844387076, 1.000000000000000000, 0.8660254037844387076, 1.000000000000000000, 0.8660254037844387076, 1.000000000000000000, 0.8660254037844387076, 1.000000000000000000, 0.8660254037844387076, 1.000000000000000000, 0.8660254037844387076, 1.000000000000000000, 0.8660254037844387076, 1.000000000000000000, 0.8660254037844387076, 1.000000000000000000, 0.8660254037844387076, 1.000000000000000000, 0.8660254037844387076, 1.000000000000000000, 0.8660254037844387076, 1.000000000000000000, 0.8660254037844387076, 1.000000000000000000, 0.8660254037844387076, 1.000000000000000000, 0.8660254037844387076, 1.000000000000000000, 0.8660254037844387076, 1.000000000000000000, 0.8660254037844387076, 1.000000000000000000, 0.8660254037844387076, 1.000000000000000000, 0.8660254037844387076, 1.000000000000000000, 0.8660254037844387076, 1.000000000000000000, 0.8660254037844387076, 1.000000000000000000, 0.8660254037844387076, 1.000000000000000000, 0.8660254037844387076, 1.000000000000000000, 0.8660254037844387076, 1.000000000000000000, 0.8660254037844387076, 1.000000000000000000, 0.8660254037844387076, 1.000000000000000000, 0.8660254037844387076, 1.000000000000000000, 0.8660254037844387076, 1.000000000000000000, 0.8660254037844387076, 1.000000000000000000, 0.8660254037844387076, 1.000000000000000000, 0.8660254037844387076, 1.000000000000000000, 0.8660254037844387076, 1.000000000000000000, 0.8660254037844387076, 1.000000000000000000, 0.8660254037844387076, 1.000000000000000000, 0.8660254037844387076, 1.000000000000000000, 0.8660254037844387076, 1.000000000000000000, 0.8660254037844387076, 1.000000000000000000, 0.8660254037844387076, 1.000000000000000000, 0.8660254037844387076, 1.000000000000000000, 0.8660254037844387076, 1.000000000000000000, 0.8660254037844387076, 1.000000000000000000, 0.8660254037844387076, 1.000000000000000000, 0.8660254037844387076, 1.000000000000000000, 0.8660254037844387076, 1.000000000000000000, 0.8660254037844387076, 1.000000000000000000, 0.8660254037844387076, 1.000000000000000000, 0.8660254037844387076, 1.000000000000000000, 0.8660254037844387076, 1.000000000000000000, 0.8660254037844387076, 1.000000000000000000, 0.8660254037844387076, 1.000000000000000000, 0.8660254037844387076, 1.000000000000000000, 0.8660254037844387076, 1.000000000000000000, 0.8660254037844387076, 1.000000000000000000, 0.8660254037844387076, 1.000000000000000000, 0.8660254037844387076, 1.000000000000000000, 0.8660254037844387076, 1.000000000000000000, 0.8660254037844387076, 1.000000000000000000, 0.8660254037844387076, 1.000000000000000000, 0.8660254037844387076, 1.000000000000000000, 0.8660254037844387076, 1.000000000000000000, 0.8660254037844387076, 1.000000000000000000, 0.8660254037844387076, 1.000000000000000000, 0.8660254037844387076, 1.000000000000000000, 0.8660254037844387076, 1.000000000000000000, 0.8660254037844387076, 1.000000000000000000, 0.8660254037844387076, 1.000000000000000000, 0.8660254037844387076, 1.000000000000000000, 0.8660254037844387076, 1.000000000000000000, 0.8660254037844387076, 1.000000000000000000, 0.8660254037844387076, 1.000000000000000000, 0.8660254037844387076, 1.000000000000000000, 0.8660254037844387076, 1.000000000000000000, 0.8660254037844387076, 1.000000000000000000, 0.8660254037844387076, 1.000000000000000000, 0.8660254037844387076, 1.000000000000000000, 0.8660254037844387076, 1.000000000000000000, 0.8660254037844387076, 1.000000000000000000, 0.8660254037844387076, 1.000000000000000000, 0.8660254037844387076, 1.000000000000000000, 0.8660254037844387076, 1.000000000000000000, 0.8660254037844387076, 1.000000000000000000, 0.8660254037844387076, 1.000000000000000000, 0.8660254037844387076, 1.000000000000000000, 0.8660254037844387076, 1.000000000000000000, 0.8660254037844387076, 1.000000000000000000, 0.8660254037844387076, 1.000000000000000000, 0.8660254037844387076, 1.000000000000000000, 0.8660254037844387076, 1.000000000000000000, 0.8660254037844387076, 1.000000000000000000, 0.8660254037844387076, 1.000000000000000000, 0.8660254037844387076, 1.000000000000000000, 0.8660254037844387076, 1.000000000000000000, 0.8660254037844387076, 1.000000000000000000, 0.8660254037844387076, 1.000000000000000000, 0.8660254037844387076, 1.000000000000000000, 0.8660254037844387076, 1.000000000000000000, 0.8660254037844387076, 1.000000000000000000, 0.8660254037844387076, 1.000000000000000000, 0.8660254037844387076, 1.000000000000000000, 0.8660254037844387076, 1.000000000000000000, 0.8660254037844387076, 1.000000000000000000, 0.8660254037844387076, 1.000000000000000000, 0.8660254037844387076, 1.000000000000000000, 0.8660254037844387076, 1.000000000000000000, 0.8660254037844387076, 1.000000000000000000, 0.8660254037844387076, 1.000000000000000000, 0.8660254037844387076, 1.000000000000000000, 0.8660254037844387076, 1.000000000000000000, 0.8660254037844387076, 1.000000000000000000, 0.8660254037844387076, 1.000000000000000000, 0.8660254037844387076, 1.000000000000000000, 0.8660254037844387076, 1.000000000000000000, 0.8660254037844387076, 1.000000000000000000, 0.8660254037844387076, 1.000000000000000000, 0.8660254037844387076, 1.000000000000000000, 0.8660254037844387076, 1.000000000000000000, 0.8660254037844387076, 1.000000000000000000, 0.8660254037844387076, 1.000000000000000000, 0.8660254037844387076, 1.000000000000000000, 0.8660254037844387076, 1.000000000000000000, 0.8660254037844387076, 1.000000000000000000, 0.8660254037844387076, 1.000000000000000000, 0.8660254037844387076, 1.000000000000000000, 0.8660254037844387076, 1.000000000000000000, 0.8660254037844387076, 1.000000000000000000, 0.8660254037844387076, 1.000000000000000000, 0.8660254037844387076, 1.000000000000000000, 0.8660254037844387076, 1.000000000000000000, 0.8660254037844387076, 1.000000000000000000, 0.8660254037844387076, 1.000000000000000000, 0.8660254037844387076, 1.000000000000000000, 0.8660254037844387076, 1.000000000000000000, 0.8660254037844387076, 1.000000000000000000, 0.8660254037844387076, 1.000000000000000000, 0.8660254037844387076, 1.000000000000000000, 0.8660254037844387076, 1.000000000000000000, 0.8660254037844387076, 1.000000000000000000, 0.8660254037844387076, 1.000000000000000000, 0.8660254037844387076, 1.000000000000000000, 0.8660254037844387076, 1.000000000000000000, 0.8660254037844387076, 1.000000000000000000, 0.8660254037844387076, 1.000000000000000000, 0.8660254037844387076, 1.000000000000000000, 0.8660254037844387076, 1.000000000000000000, 0.8660254037844387076, 1.000000000000000000, 0.8660254037844387076, 1.000000000000000000, 0.8660254037844387076, 1.000000000000000000, 0.8660254037844387076, 1.000000000000000000, 0.8660254037844387076, 1.000000000000000000, 0.8660254037844387076, 1.000000000000000000, 0.8660254037844387076, 1.000000000000000000, 0.8660254037844387076, 1.000000000000000000, 0.8660254037844387076, 1.000000000000000000, 0.8660254037844387076, 1.000000000000000000, 0.8660254037844387076, 1.000000000000000000, 0.8660254037844387076, 1.000000000000000000, 0.8660254037844387076, 1.000000000000000000, 0.8660254037844387076, 1.000000000000000000, 0.8660254037844387076, 1.000000000000000000, 0.8660254037844387076, 1.000000000000000000, 0.8660254037844387076, 1.000000000000000000, 0.8660254037844387076, 1.000000000000000000, 0.8660254037844387076, 1.000000000000000000, 0.8660254037844387076, 1.000000000000000000, 0.8660254037844387076, 1.000000000000000000, 0.8660254037844387076, 1.000000000000000000, 0.8660254037844387076, 1.000000000000000000, 0.8660254037844387076, 1.000000000000000000, 0.8660254037844387076, 1.000000000000000000, 0.8660254037844387076, 1.000000000000000000, 0.8660254037844387076, 1.000000000000000000, 0.8660254037844387076, 1.000000000000000000, 0.8660254037844387076, 1.000000000000000000, 0.8660254037844387076, 1.000000000000000000, 0.8660254037844387076, 1.000000000000000000, 0.8660254037844387076, 1.000000000000000000, 0.8660254037844387076, 1.000000000000000000, 0.8660254037844387076, 1.000000000000000000, 0.8660254037844387076, 1.000000000000000000, 0.8660254037844387076, 1.000000000000000000, 0.8660254037844387076, 1.000000000000000000, 0.8660254037844387076, 1.000000000000000000, 0.8660254037844387076, 1.000000000000000000, 0.8660254037844387076, 1.000000000000000000, 0.8660254037844387076, 1.000000000000000000, 0.8660254037844387076, 1.000000000000000000, 0.8660254037844387076, 1.000000000000000000, 0.8660254037844387076, 1.000000000000000000, 0.8660254037844387076, 1.000000000000000000, 0.8660254037844387076, 1.000000000000000000, 0.8660254037844387076, 1.000000000000000000, 0.8660254037844387076, 1.000000000000000000, 0.8660254037844387076, 1.000000000000000000, 0.8660254037844387076, 1.000000000000000000, 0.8660254037844387076, 1.000000000000000000, 0.8660254037844387076, 1.000000000000000000, 0.8660254037844387076, 1.000000000000000000, 0.8660254037844387076, 1.000000000000000000, 0.8660254037844387076, 1.000000000000000000, 0.8660254037844387076, 1.000000000000000000, 0.8660254037844387076, 1.000000000000000000, 0.8660254037844387076, 1.000000000000000000, 0.8660254037844387076, 1.000000000000000000, 0.8660254037844387076, 1.000000000000000000, 0.8660254037844387076, 1.000000000000000000, 0.8660254037844387076, 1.000000000000000000, 0.8660254037844387076, 1.000000000000000000, 0.8660254037844387076, 1.000000000000000000, 0.8660254037844387076, 1.000000000000000000, 0.8660254037844387076, 1.000000000000000000, 0.8660254037844387076, 1.000000000000000000, 0.8660254037844387076, 1.000000000000000000, 0.8660254037844387076, 1.000000000000000000, 0.8660254037844387076, 1.000000000000000000, 0.8660254037844387076, 1.000000000000000000, 0.8660254037844387076, 1.000000000000000000, 0.8660254037844387076, 1.000000000000000000, 0.8660254037844387076, 1.000000000000000000, 0.8660254037844387076, 1.000000000000000000, 0.8660254037844387076, 1.000000000000000000, 0.8660254037844387076, 1.000000000000000000, 0.8660254037844387076, 1.000000000000000000, 0.8660254037844387076, 1.000000000000000000, 0.8660254037844387076, 1.000000000000000000, 0.8660254037844387076, 1.000000000000000000, 0.8660254037844387076, 1.000000000000000000, 0.8660254037844387076, 1.000000000000000000, 0.8660254037844387076, 1.000000000000000000, 0.8660254037844387076, 1.000000000000000000, 0.8660254037844387076, 1.000000000000000000, 0.8660254037844387076, 1.000000000000000000, 0.8660254037844387076, 1.000000000000000000, 0.8660254037844387076, 1.000000000000000000, 0.8660254037844387076, 1.000000000000000000, 0.8660254037844387076, 1.000000000000000000, 0.8660254037844387076, 1.000000000000000000, 0.8660254037844387076, 1.000000000000000000, 0.8660254037844387076, 1.000000000000000000, 0.8660254037844387076, 1.000000000000000000, 0.8660254037844387076, 1.000000000000000000, 0.8660254037844387076, 1.000000000000000000, 0.8660254037844387076, 1.000000000000000000, 0.8660254037844387076, 1.000000000000000000, 0.8660254037844387076, 1.000000000000000000, 0.8660254037844387076, 1.000000000000000000, 0.8660254037844387076, 1.000000000000000000, 0.8660254037844387076, 1.000000000000000000, 0.8660254037844387076, 1.000000000000000000, 0.8660254037844387076, 1.000000000000000000, 0.8660254037844387076, 1.000000000000000000, 0.8660254037844387076, 1.000000000000000000, 0.8660254037844387076, 1.000000000000000000, 0.8660254037844387076, 1.000000000000000000, 0.8660254037844387076, 1.000000000000000000, 0.8660254037844387076, 1.000000000000000000, 0.8660254037844387076, 1.000000000000000000, 0.8660254037844387076, 1.000000000000000000, 0.8660254037844387076, 1.000000000000000000, 0.8660254037844387076, 1.000000000000000000, 0.8660254037844387076, 1.000000000000000000, 0.8660254037844387076, 1.000000000000000000, 0.8660254037844387076, 1.000000000000000000, 0.8660254037844387076, 1.000000000000000000, 0.8660254037844387076, 1.000000000000000000, 0.8660254037844387076, 1.000000000000000000, 0.8660254037844387076, 1.000000000000000000, 0.8660254037844387076, 1.000000000000000000, 0.8660254037844387076, 1.000000000000000000, 0.8660254037844387076, 1.000000000000000000, 0.8660254037844387076, 1.000000000000000000, 0.8660254037844387076, 1.000000000000000000, 0.8660254037844387076, 1.000000000000000000, 0.8660254037844387076, 1.000000000000000000, 0.8660254037844387076, 1.000000000000000000, 0.8660254037844387076, 1.000000000000000000, 0.8660254037844387076, 1.000000000000000000, 0.8660254037844387076, 1.000000000000000000, 0.8660254037844387076, 1.000000000000000000, 0.8660254037844387076, 1.000000000000000000, 0.8660254037844387076, 1.000000000000000000, 0.8660254037844387076, 1.000000000000000000, 0.8660254037844387076, 1.000000000000000000, 0.8660254037844387076, 1.000000000000000000, 0.8660254037844387076, 1.000000000000000000, 0.8660254037844387076, 1.000000000000000000, 0.8660254037844387076, 1.000000000000000000, 0.8660254037844387076, 1.000000000000000000, 0.8660254037844387076, 1.000000000000000000, 0.8660254037844387076, 1.000000000000000000, 0.8660254037844387076, 1.000000000000000000, 0.8660254037844387076, 1.000000000000000000, 0.8660254037844387076, 1.000000000000000000, 0.8660254037844387076, 1.000000000000000000, 0.8660254037844387076, 1.000000000000000000, 0.8660254037844387076, 1.000000000000000000, 0.8660254037844387076, 1.000000000000000000, 0.8660254037844387076, 1.000000000000000000, 0.8660254037844387076, 1.000000000000000000, 0.8660254037844387076, 1.000000000000000000, 0.8660254037844387076, 1.000000000000000000, 0.8660254037844387076, 1.000000000000000000, 0.8660254037844387076, 1.000000000000000000, 0.8660254037844387076, 1.000000000000000000, 0.8660254037844387076, 1.000000000000000000, 0.8660254037844387076, 1.000000000000000000, 0.8660254037844387076, 1.000000000000000000, 0.8660254037844387076, 1.000000000000000000, 0.8660254037844387076, 1.000000000000000000, 0.8660254037844387076, 1.000000000000000000, 0.8660254037844387076, 1.000000000000000000, 0.8660254037844387076, 1.000000000000000000, 0.8660254037844387076, 1.000000000000000000, 0.8660254037844387076, 1.000000000000000000, 0.8660254037844387076, 1.000000000000000000, 0.8660254037844387076, 1.000000000000000000, 0.8660254037844387076, 1.000000000000000000, 0.8660254037844387076, 1.000000000000000000, 0.8660254037844387076, 1.000000000000000000, 0.8660254037844387076, 1.000000000000000000, 0.8660254037844387076, 1.000000000000000000, 0.8660254037844387076, 1.000000000000000000, 0.8660254037844387076, 1.000000000000000000, 0.8660254037844387076, 1.000000000000000000, 0.8660254037844387076, 1.000000000000000000, 0.8660254037844387076, 1.000000000000000000, 0.8660254037844387076, 1.000000000000000000, 0.8660254037844387076, 1.000000000000000000, 0.8660254037844387076, 1.000000000000000000, 0.8660254037844387076, 1.000000000000000000, 0.8660254037844387076, 1.000000000000000000, 0.8660254037844387076, 1.000000000000000000, 0.8660254037844387076, 1.000000000000000000, 0.8660254037844387076, 1.000000000000000000, 0.8660254037844387076, 1.000000000000000000, 0.8660254037844387076, 1.000000000000000000, 0.8660254037844387076, 1.000000000000000000, 0.8660254037844387076, 1.000000000000000000, 0.8660254037844387076, 1.000000000000000000, 0.8660254037844387076, 1.000000000000000000, 0.8660254037844387076, 1.000000000000000000, 0.8660254037844387076, 1.000000000000000000, 0.8660254037844387076, 1.000000000000000000, 0.8660254037844387076, 1.000000000000000000, 0.8660254037844387076, 1.000000000000000000, 0.8660254037844387076, 1.000000000000000000, 0.8660254037844387076, 1.000000000000000000, 0.8660254037844387076, 1.000000000000000000, 0.8660254037844387076, 1.000000000000000000, 0.8660254037844387076, 1.000000000000000000, 0.8660254037844387076, 1.000000000000000000, 0.8660254037844387076, 1.000000000000000000, 0.8660254037844387076, 1.000000000000000000, 0.8660254037844387076, 1.000000000000000000, 0.8660254037844387076, 1.000000000000000000, 0.8660254037844387076, 1.000000000000000000, 0.8660254037844387076, 1.000000000000000000, 0.8660254037844387076, 1.000000000000000000, 0.8660254037844387076, 1.000000000000000000, 0.8660254037844387076, 1.000000000000000000, 0.8660254037844387076, 1.000000000000000000, 0.8660254037844387076, 1.000000000000000000, 0.8660254037844387076, 1.000000000000000000, 0.8660254037844387076, 1.000000000000000000, 0.8660254037844387076, 1.000000000000000000, 0.8660254037844387076, 1.000000000000000000, 0.8660254037844387076, 1.000000000000000000, 0.8660254037844387076, 1.000000000000000000, 0.8660254037844387076, 1.000000000000000000, 0.8660254037844387076, 1.000000000000000000, 0.8660254037844387076, 1.000000000000000000, 0.8660254037844387076, 1.000000000000000000, 0.8660254037844387076, 1.000000000000000000, 0.8660254037844387076, 1.000000000000000000, 0.8660254037844387076, 1.000000000000000000, 0.8660254037844387076, 1.000000000000000000, 0.8660254037844387076, 1.000000000000000000, 0.8660254037844387076, 1.000000000000000000, 0.8660254037844387076, 1.000000000000000000, 0.8660254037844387076, 1.000000000000000000, 0.8660254037844387076, 1.000000000000000000, 0.8660254037844387076, 1.000000000000000000, 0.8660254037844387076, 1.000000000000000000, 0.8660254037844387076, 1.000000000000000000, 0.8660254037844387076, 1.000000000000000000, 0.8660254037844387076, 1.000000000000000000, 0.8660254037844387076, 1.000000000000000000, 0.8660254037844387076, 1.000000000000000000, 0.8660254037844387076, 1.000000000000000000, 0.8660254037844387076, 1.000000000000000000, 0.8660254037844387076, 1.000000000000000000, 0.8660254037844387076, 1.000000000000000000, 0.8660254037844387076, 1.000000000000000000, 0.8660254037844387076, 1.000000000000000000, 0.8660254037844387076, 1.000000000000000000, 0.8660254037844387076, 1.000000000000000000, 0.8660254037844387076, 1.000000000000000000, 0.8660254037844387076, 1.000000000000000000, 0.8660254037844387076, 1.000000000000000000, 0.8660254037844387076, 1.000000000000000000, 0.8660254037844387076, 1.000000000000000000, 0.8660254037844387076, 1.000000000000000000, 0.8660254037844387076, 1.000000000000000000, 0.8660254037844387076, 1.000000000000000000, 0.8660254037844387076, 1.000000000000000000, 0.8660254037844387076, 1.000000000000000000, 0.8660254037844387076, 1.000000000000000000, 0.8660254037844387076, 1.000000000000000000, 0.8660254037844387076, 1.000000000000000000, 0.8660254037844387076, 1.000000000000000000, 0.8660254037844387076, 1.000000000000000000, 0.8660254037844387076, 1.000000000000000000, 0.8660254037844387076, 1.000000000000000000, 0.8660254037844387076, 1.000000000000000000, 0.8660254037844387076, 1.000000000000000000, 0.8660254037844387076, 1.000000000000000000, 0.8660254037844387076, 1.000000000000000000, 0.8660254037844387076, 1.000000000000000000, 0.8660254037844387076, 1.000000000000000000, 0.8660254037844387076, 1.000000000000000000, 0.8660254037844387076, 1.000000000000000000, 0.8660254037844387076, 1.000000000000000000, 0.8660254037844387076, 1.000000000000000000, 0.8660254037844387076, 1.000000000000000000, 0.8660254037844387076, 1.000000000000000000, 0.8660254037844387076, 1.000000000000000000, 0.8660254037844387076, 1.000000000000000000, 0.8660254037844387076, 1.000000000000000000, 0.8660254037844387076, 1.000000000000000000, 0.8660254037844387076, 1.000000000000000000, 0.8660254037844387076, 1.000000000000000000, 0.8660254037844387076, 1.000000000000000000, 0.8660254037844387076, 1.000000000000000000, 0.8660254037844387076, 1.000000000000000000, 0.8660254037844387076, 1.000000000000000000, 0.8660254037844387076, 1.000000000000000000, 0.8660254037844387076, 1.000000000000000000, 0.8660254037844387076, 1.000000000000000000, 0.8660254037844387076, 1.000000000000000000, 0.8660254037844387076, 1.000000000000000000, 0.8660254037844387076, 1.000000000000000000, 0.8660254037844387076, 1.000000000000000000, 0.8660254037844387076, 1.000000000000000000, 0.8660254037844387076, 1.000000000000000000, 0.8660254037844387076, 1.000000000000000000, 0.8660254037844387076, 1.000000000000000000, 0.8660254037844387076, 1.000000000000000000, 0.8660254037844387076, 1.000000000000000000, 0.8660254037844387076, 1.000000000000000000, 0.8660254037844387076, 1.000000000000000000, 0.8660254037844387076, 1.000000000000000000, 0.8660254037844387076, 1.000000000000000000, 0.8660254037844387076, 1.000000000000000000, 0.8660254037844387076, 1.000000000000000000, 0.8660254037844387076, 1.000000000000000000, 0.8660254037844387076, 1.000000000000000000, 0.8660254037844387076, 1.000000000000000000, 0.8660254037844387076, 1.000000000000000000, 0.8660254037844387076, 1.000000000000000000, 0.8660254037844387076, 1.000000000000000000) ) ) 
 REPRESENTATION_ITEM ( '' )  SURFACE ( )  );
#8897 = CARTESIAN_POINT ( 'NONE',  ( -9.999999999999998224, 5.773502691896259087, -115.7500000040967763 ) ) ;
#8898 = CARTESIAN_POINT ( 'NONE',  ( -9.999999999999998224, 1.224646799147353059E-15, -39.12500000409676915 ) ) ;
#8899 = CARTESIAN_POINT ( 'NONE',  ( -5.405949406249996869, 9.363379034771805109, -74.34375000204838102 ) ) ;
#8900 = CARTESIAN_POINT ( 'NONE',  ( 7.070501591499377789E-16, 11.54700538379251284, -39.12499999999996447 ) ) ;
#8901 = EDGE_CURVE ( 'NONE', #1054, #27758, #21322, .T. ) ;
#8902 = CARTESIAN_POINT ( 'NONE',  ( 9.999999999999996447, -5.773502691896262640, -29.50000000409675494 ) ) ;
#8903 = CARTESIAN_POINT ( 'NONE',  ( -10.00000000000051337, 5.773502691895962435, -118.7500000040967763 ) ) ;
#8904 = CARTESIAN_POINT ( 'NONE',  ( -5.405949406249996869, 9.363379034771805109, -37.03125000204837391 ) ) ;
#8905 =( BOUNDED_CURVE ( )  B_SPLINE_CURVE ( 2, ( #27015, #26803, #13188, #29410, #23361, #13611, #16422 ),
 .UNSPECIFIED., .F., .F. ) 
 B_SPLINE_CURVE_WITH_KNOTS ( ( 3, 2, 2, 3 ),
 ( 0.4141791044776120256, 0.4154228855721394109, 0.4166666666666667962, 0.4179104477611941260 ),
 .UNSPECIFIED. ) 
 CURVE ( )  GEOMETRIC_REPRESENTATION_ITEM ( )  RATIONAL_B_SPLINE_CURVE ( ( 0.9999999999999880096, 0.8660254037844506980, 1.000000000000000000, 0.8660254037844387076, 1.000000000000000000, 0.8660254037844267172, 1.000000000000011990 ) ) 
 REPRESENTATION_ITEM ( '' )  );
#8906 = CARTESIAN_POINT ( 'NONE',  ( -9.999999999999998224, 1.224646799147353059E-15, -43.24999999999998579 ) ) ;
#8907 = CARTESIAN_POINT ( 'NONE',  ( -2.293366432827344421E-15, -12.48450537969573659, -142.9062500020483810 ) ) ;
#8908 = CARTESIAN_POINT ( 'NONE',  ( -5.405949406249996869, 9.363379034771805109, -146.5312500020483810 ) ) ;
#8909 = CARTESIAN_POINT ( 'NONE',  ( -7.959047257566134870E-15, 125.0000000000000000, 42.49999999999999289 ) ) ;
#8910 = VECTOR ( 'NONE', #12818, 1000.000000000000000 ) ;
#8911 = CARTESIAN_POINT ( 'NONE',  ( -9.999999999999998224, 1.224646799147353059E-15, -178.2500000000000284 ) ) ;
#8912 = VERTEX_POINT ( 'NONE', #17285 ) ;
#8913 = AXIS2_PLACEMENT_3D ( 'NONE', #3363, #16496, #23568 ) ;
#8914 = ORIENTED_EDGE ( 'NONE', *, *, #23902, .T. ) ;
#8915 = VERTEX_POINT ( 'NONE', #21175 ) ;
#8916 = CARTESIAN_POINT ( 'NONE',  ( 7.070501591499376803E-16, 11.54700538379251284, -135.5000000040967905 ) ) ;
#8917 = CARTESIAN_POINT ( 'NONE',  ( 5.405949406249992428, -9.363379034771808662, -184.5937500020483810 ) ) ;
#8918 = CIRCLE ( 'NONE', #16462, 25.00000000000000000 ) ;
#8919 = CARTESIAN_POINT ( 'NONE',  ( -2.293366432827344421E-15, -12.48450537969573659, -28.71875000204835615 ) ) ;
#8920 = CARTESIAN_POINT ( 'NONE',  ( -9.999999999999998224, 1.224646799147353059E-15, -130.6250000040967620 ) ) ;
#8921 = CARTESIAN_POINT ( 'NONE',  ( -10.81189881249999729, 1.324075727343319199E-15, -164.0937500020484094 ) ) ;
#8922 = CARTESIAN_POINT ( 'NONE',  ( 5.405949406249999534, 9.363379034771803333, -152.5937500020483810 ) ) ;
#8923 = CARTESIAN_POINT ( 'NONE',  ( 10.90460581041948984, 0.09205482696659748887, -1.027162637006526080E-30 ) ) ;
#8924 = CARTESIAN_POINT ( 'NONE',  ( -2.293366432827344421E-15, -12.48450537969573659, -133.7187500020483810 ) ) ;
#8925 = CARTESIAN_POINT ( 'NONE',  ( -10.81189881249999907, -6.242252689847864744, -137.1562500020483810 ) ) ;
#8926 = CARTESIAN_POINT ( 'NONE',  ( 7.070501591499376803E-16, 11.54700538379251284, -104.0000000040967763 ) ) ;
#8927 = CARTESIAN_POINT ( 'NONE',  ( 5.405949406249999534, 9.363379034771803333, -149.5937500020483810 ) ) ;
#8928 = CARTESIAN_POINT ( 'NONE',  ( -4.999999999999996447, 8.660254037844387298, -129.0000000000000000 ) ) ;
#8929 = CARTESIAN_POINT ( 'NONE',  ( -4.999999999999996447, 8.660254037844387298, -183.0000000000000000 ) ) ;
#8930 = CARTESIAN_POINT ( 'NONE',  ( -10.00000000000000000, -5.773502691896251982, -172.1250000000000284 ) ) ;
#8931 = CARTESIAN_POINT ( 'NONE',  ( 7.644554776091147741E-16, 12.48450537969573659, -77.46875000204838102 ) ) ;
#8932 = CARTESIAN_POINT ( 'NONE',  ( 4.999999999999992006, -8.660254037844389075, -113.6250000040967763 ) ) ;
#8933 = CARTESIAN_POINT ( 'NONE',  ( 10.81189881249999729, 0.000000000000000000, -52.53125000204835970 ) ) ;
#8934 = CARTESIAN_POINT ( 'NONE',  ( -9.999999999999998224, 1.224646799147353059E-15, -149.7500000000000000 ) ) ;
#8935 = CARTESIAN_POINT ( 'NONE',  ( -10.81189881249999729, 6.242252689847871849, -171.7187500020483810 ) ) ;
#8936 = CARTESIAN_POINT ( 'NONE',  ( 4.999999999999992006, -8.660254037844389075, -138.7499999999999716 ) ) ;
#8937 = CARTESIAN_POINT ( 'NONE',  ( 10.81189881249999551, -6.242252689847874514, -148.6562500020484094 ) ) ;
#8938 = CARTESIAN_POINT ( 'NONE',  ( 0.000000000000000000, 0.000000000000000000, -99.99999999999998579 ) ) ;
#8939 = CARTESIAN_POINT ( 'NONE',  ( 5.405949406249999534, 9.363379034771803333, -37.28125000204837391 ) ) ;
#8940 = CARTESIAN_POINT ( 'NONE',  ( -9.999999999999998224, 5.773502691896259087, -123.2500000040967763 ) ) ;
#8941 = CARTESIAN_POINT ( 'NONE',  ( 9.999999999999998224, 0.000000000000000000, -97.99999999999998579 ) ) ;
#8942 = ORIENTED_EDGE ( 'NONE', *, *, #41083, .T. ) ;
#8943 = CARTESIAN_POINT ( 'NONE',  ( 10.81189881249999729, 0.000000000000000000, -115.5312500020483952 ) ) ;
#8944 = CARTESIAN_POINT ( 'NONE',  ( -9.999999999999998224, 1.224646799147353059E-15, -139.6250000040967905 ) ) ;
#8945 = DIRECTION ( 'NONE',  ( -0.000000000000000000, -0.000000000000000000, 1.000000000000000000 ) ) ;
#8946 = VECTOR ( 'NONE', #786, 1000.000000000000000 ) ;
#8947 = CARTESIAN_POINT ( 'NONE',  ( 7.644554776091147741E-16, 12.48450537969573659, -176.6562500020484094 ) ) ;
#8948 = CARTESIAN_POINT ( 'NONE',  ( 9.999999999999998224, 0.000000000000000000, -53.37500000409675494 ) ) ;
#8949 = CARTESIAN_POINT ( 'NONE',  ( 10.00000000000025402, -5.773502691896113426, -155.1250000000000000 ) ) ;
#8950 = CARTESIAN_POINT ( 'NONE',  ( -2.293366432827344421E-15, -12.48450537969573659, -64.90625000204838102 ) ) ;
#8951 = VECTOR ( 'NONE', #16868, 1000.000000000000000 ) ;
#8952 = CARTESIAN_POINT ( 'NONE',  ( 0.000000000000000000, 0.000000000000000000, -200.0000000000000000 ) ) ;
#8953 = CARTESIAN_POINT ( 'NONE',  ( 5.405949406249999534, 9.363379034771803333, -172.2812500020484094 ) ) ;
#8954 = CYLINDRICAL_SURFACE ( 'NONE', #29780, 9.999999999999998224 ) ;
#8955 = CARTESIAN_POINT ( 'NONE',  ( 0.000000000000000000, 0.000000000000000000, -200.0000000000000000 ) ) ;
#8957 = VERTEX_POINT ( 'NONE', #36942 ) ;
#8956 = EDGE_CURVE ( 'NONE', #5520, #13539, #22708, .T. ) ;
#8958 = FACE_OUTER_BOUND ( 'NONE', #21755, .T. ) ;
#8959 = CARTESIAN_POINT ( 'NONE',  ( 4.999999999999992006, -8.660254037844389075, -52.12500000409675494 ) ) ;
#8961 = VERTEX_POINT ( 'NONE', #14471 ) ;
#8960 = CARTESIAN_POINT ( 'NONE',  ( -5.405949406249996869, 9.363379034771805109, -76.03125000204838102 ) ) ;
#8962 = EDGE_LOOP ( 'NONE', ( #2746, #9472, #12597, #23988 ) ) ;
#8963 =( BOUNDED_CURVE ( )  B_SPLINE_CURVE ( 2, ( #31034, #18271, #28005, #8371, #14599, #40922, #11365 ),
 .UNSPECIFIED., .F., .F. ) 
 B_SPLINE_CURVE_WITH_KNOTS ( ( 3, 2, 2, 3 ),
 ( 0.8582089552238808539, 0.8594527363184081281, 0.8606965174129356244, 0.8619402985074630097 ),
 .UNSPECIFIED. ) 
 CURVE ( )  GEOMETRIC_REPRESENTATION_ITEM ( )  RATIONAL_B_SPLINE_CURVE ( ( 0.9999999999999761302, 0.8660254037844625774, 1.000000000000000000, 0.8660254037844387076, 1.000000000000000000, 0.8660254037844028474, 1.000000000000035971 ) ) 
 REPRESENTATION_ITEM ( '' )  );
#8964 = VERTEX_POINT ( 'NONE', #34365 ) ;
#8965 = CARTESIAN_POINT ( 'NONE',  ( -10.81189881249999729, -6.242252689847864744, -28.96875000204835615 ) ) ;
#8966 = CARTESIAN_POINT ( 'NONE',  ( -5.405949406250003975, -9.363379034771801557, -6.531250002048377468 ) ) ;
#8968 = ORIENTED_EDGE ( 'NONE', *, *, #40000, .T. ) ;
#8967 = CARTESIAN_POINT ( 'NONE',  ( 10.81189881249999907, 6.242252689847868297, -55.21875000204836681 ) ) ;
#8969 = CARTESIAN_POINT ( 'NONE',  ( -9.999999999999998224, 1.224646799147353059E-15, -112.6250000040967763 ) ) ;
#8970 = CARTESIAN_POINT ( 'NONE',  ( -5.000000000000003553, -8.660254037844383745, -35.49999999999997868 ) ) ;
#8971 = CARTESIAN_POINT ( 'NONE',  ( -5.405949406249996869, 9.363379034771805109, -188.3437500020483810 ) ) ;
#8972 = CARTESIAN_POINT ( 'NONE',  ( 10.81189881249999551, -6.242252689847874514, -179.9687500020484094 ) ) ;
#8973 = CARTESIAN_POINT ( 'NONE',  ( -5.405949406250003975, -9.363379034771801557, -160.8437500020484094 ) ) ;
#8974 = CARTESIAN_POINT ( 'NONE',  ( -10.81189881249999729, 6.242252689847871849, -170.2187500020483810 ) ) ;
#8975 = CARTESIAN_POINT ( 'NONE',  ( -4.999999999999996447, 8.660254037844387298, -124.5000000000000000 ) ) ;
#8976 = CARTESIAN_POINT ( 'NONE',  ( 10.00000000000000000, 5.773502691896255534, -132.3750000000000000 ) ) ;
#8977 = CARTESIAN_POINT ( 'NONE',  ( -9.999999999999998224, 5.773502691896259087, -197.8750000000000000 ) ) ;
#8978 = CARTESIAN_POINT ( 'NONE',  ( -5.405949406250003975, -9.363379034771801557, -108.3437500020483810 ) ) ;
#8979 = CARTESIAN_POINT ( 'NONE',  ( -5.000000000000003553, -8.660254037844383745, -47.87500000409677625 ) ) ;
#8980 = CARTESIAN_POINT ( 'NONE',  ( 7.644554776091147741E-16, 12.48450537969573659, -76.15625000204839523 ) ) ;
#8981 = CARTESIAN_POINT ( 'NONE',  ( -10.81189881249999729, 6.242252689847871849, -90.71875000204838102 ) ) ;
#8982 = CARTESIAN_POINT ( 'NONE',  ( 10.81189881249999729, 0.000000000000000000, -63.03125000204837391 ) ) ;
#8983 = CARTESIAN_POINT ( 'NONE',  ( 4.999999999999992006, -8.660254037844389075, -148.1250000040967905 ) ) ;
#8984 = CARTESIAN_POINT ( 'NONE',  ( 9.999999999999998224, 0.000000000000000000, -122.0000000000000000 ) ) ;
#8985 = EDGE_LOOP ( 'NONE', ( #26781, #4177, #32898, #19504 ) ) ;
#8986 = CARTESIAN_POINT ( 'NONE',  ( -10.81189881249999729, 6.242252689847871849, -140.4062500020484094 ) ) ;
#8987 = CARTESIAN_POINT ( 'NONE',  ( 5.405949406249992428, -9.363379034771808662, -159.2812500020484094 ) ) ;
#8988 = DIRECTION ( 'NONE',  ( -0.000000000000000000, -0.000000000000000000, 1.000000000000000000 ) ) ;
#8989 = CARTESIAN_POINT ( 'NONE',  ( 9.999999999999998224, 0.000000000000000000, -200.0000000000000000 ) ) ;
#8990 = CARTESIAN_POINT ( 'NONE',  ( -5.405949406250003975, -9.363379034771801557, -87.34375000204836681 ) ) ;
#8991 = VERTEX_POINT ( 'NONE', #37149 ) ;
#8992 = CARTESIAN_POINT ( 'NONE',  ( -4.999999999999996447, 8.660254037844387298, -64.49999999999997158 ) ) ;
#8993 = CARTESIAN_POINT ( 'NONE',  ( 10.81189881249999729, 0.000000000000000000, -194.8437500020484094 ) ) ;
#8994 = CARTESIAN_POINT ( 'NONE',  ( -4.999999999999996447, 8.660254037844387298, -73.87500000409677625 ) ) ;
#8995 = CARTESIAN_POINT ( 'NONE',  ( -4.999999999999996447, 8.660254037844387298, -102.0000000000000000 ) ) ;
#8996 = DIRECTION ( 'NONE',  ( -0.000000000000000000, -0.000000000000000000, 1.000000000000000000 ) ) ;
#8997 = CARTESIAN_POINT ( 'NONE',  ( 7.644554776091147741E-16, 12.48450537969573659, -95.65625000204838102 ) ) ;
#8998 = CARTESIAN_POINT ( 'NONE',  ( 7.644554776091147741E-16, 12.48450537969573659, -67.15625000204839523 ) ) ;
#8999 = CARTESIAN_POINT ( 'NONE',  ( 5.000000000000000000, 8.660254037844385522, -66.62500000409676204 ) ) ;
#9000 = CARTESIAN_POINT ( 'NONE',  ( 0.000000000000000000, 0.000000000000000000, -99.99999999999998579 ) ) ;
#9001 = CARTESIAN_POINT ( 'NONE',  ( -10.81189881249999907, -6.242252689847864744, -22.96875000204837036 ) ) ;
#9002 = ORIENTED_EDGE ( 'NONE', *, *, #25949, .F. ) ;
#9003 = CARTESIAN_POINT ( 'NONE',  ( 10.81189881249999907, 6.242252689847868297, -191.9062500020484094 ) ) ;
#9004 = AXIS2_PLACEMENT_3D ( 'NONE', #5783, #2759, #32121 ) ;
#9005 = CARTESIAN_POINT ( 'NONE',  ( 10.81189881249999729, 0.000000000000000000, -22.53125000204836326 ) ) ;
#9006 = CARTESIAN_POINT ( 'NONE',  ( 10.81189881249999729, 0.000000000000000000, -8.843750002048345493 ) ) ;
#9007 = CARTESIAN_POINT ( 'NONE',  ( -10.00000000000025580, 5.773502691896109873, -186.2500000040967905 ) ) ;
#9008 = CARTESIAN_POINT ( 'NONE',  ( 0.000000000000000000, 0.000000000000000000, -99.99999999999998579 ) ) ;
#9009 = CARTESIAN_POINT ( 'NONE',  ( 9.999999999999998224, 0.000000000000000000, -159.8750000040967905 ) ) ;
#9010 =( BOUNDED_CURVE ( )  B_SPLINE_CURVE ( 2, ( #3207, #9044, #6446, #39028, #42044, #13100, #16333 ),
 .UNSPECIFIED., .F., .F. ) 
 B_SPLINE_CURVE_WITH_KNOTS ( ( 3, 2, 2, 3 ),
 ( 0.3619402985074628432, 0.3631840796019901729, 0.3644278606965175027, 0.3656716417910448325 ),
 .UNSPECIFIED. ) 
 CURVE ( )  GEOMETRIC_REPRESENTATION_ITEM ( )  RATIONAL_B_SPLINE_CURVE ( ( 0.9999999999999820144, 0.8660254037844566932, 1.000000000000000000, 0.8660254037844387076, 1.000000000000000000, 0.8660254037844327124, 1.000000000000005995 ) ) 
 REPRESENTATION_ITEM ( '' )  );
#9011 = CARTESIAN_POINT ( 'NONE',  ( 7.070501591499377789E-16, 11.54700538379251284, -172.6249999999999716 ) ) ;
#9012 = DIRECTION ( 'NONE',  ( 1.000000000000000000, 0.000000000000000000, 0.000000000000000000 ) ) ;
#9014 = ORIENTED_EDGE ( 'NONE', *, *, #1558, .T. ) ;
#9013 = CARTESIAN_POINT ( 'NONE',  ( -10.81189881249999907, -6.242252689847864744, -104.1562500020483668 ) ) ;
#9015 = FACE_OUTER_BOUND ( 'NONE', #19294, .T. ) ;
#9016 = EDGE_CURVE ( 'NONE', #32390, #14564, #27369, .T. ) ;
#9017 = EDGE_LOOP ( 'NONE', ( #32592, #14618, #20037, #8895, #33117 ) ) ;
#9018 = EDGE_CURVE ( 'NONE', #28714, #4880, #41968, .T. ) ;
#9019 = ORIENTED_EDGE ( 'NONE', *, *, #33581, .F. ) ;
#9020 = CARTESIAN_POINT ( 'NONE',  ( -10.81189881249999729, 1.324075727343319199E-15, -29.28125000204837036 ) ) ;
#9021 = DATE_AND_TIME ( #6423, #3577 ) ;
#9022 = CARTESIAN_POINT ( 'NONE',  ( -5.405949406250003975, -9.363379034771801557, -79.84375000204838102 ) ) ;
#9023 = CARTESIAN_POINT ( 'NONE',  ( -9.999999999999998224, 1.224646799147353059E-15, -4.625000004096769146 ) ) ;
#9024 = CARTESIAN_POINT ( 'NONE',  ( 10.13602244787124995, -1.019214064432307332, -99.99999999999994316 ) ) ;
#9025 = CARTESIAN_POINT ( 'NONE',  ( 5.000000000000000000, 8.660254037844385522, -69.62500000409677625 ) ) ;
#9026 = CARTESIAN_POINT ( 'NONE',  ( -4.999999999999996447, 8.660254037844387298, -129.0000000000000000 ) ) ;
#9027 = CARTESIAN_POINT ( 'NONE',  ( 7.644554776091147741E-16, 12.48450537969573659, -152.6562500020484094 ) ) ;
#9028 = CARTESIAN_POINT ( 'NONE',  ( 7.070501591499377789E-16, 11.54700538379251284, -11.00000000409676382 ) ) ;
#9029 = CARTESIAN_POINT ( 'NONE',  ( 0.000000000000000000, 0.000000000000000000, -99.99999999999998579 ) ) ;
#9030 = CARTESIAN_POINT ( 'NONE',  ( -5.000000000000003553, -8.660254037844383745, -74.87500000409677625 ) ) ;
#9031 = CARTESIAN_POINT ( 'NONE',  ( -10.81189881249999729, 1.324075727343319199E-15, -128.0937500020483810 ) ) ;
#9032 = CARTESIAN_POINT ( 'NONE',  ( 5.405949406249999534, 9.363379034771803333, -119.5937500020483810 ) ) ;
#9033 = CARTESIAN_POINT ( 'NONE',  ( 7.644554776091147741E-16, 12.48450537969573659, -81.96875000204839523 ) ) ;
#9034 = CARTESIAN_POINT ( 'NONE',  ( -10.81189881249999907, -6.242252689847864744, -92.15625000204839523 ) ) ;
#9035 = CARTESIAN_POINT ( 'NONE',  ( -9.999999999999998224, 1.224646799147353059E-15, -171.1250000040968189 ) ) ;
#9036 = CARTESIAN_POINT ( 'NONE',  ( -10.81189881249999729, 1.324075727343319199E-15, -168.7812500020484094 ) ) ;
#9037 = CYLINDRICAL_SURFACE ( 'NONE', #8245, 9.999999999999998224 ) ;
#9038 = CARTESIAN_POINT ( 'NONE',  ( -2.293366432827344421E-15, -12.48450537969573659, -177.4062500020484379 ) ) ;
#9039 = CARTESIAN_POINT ( 'NONE',  ( -10.81189881249999729, 6.242252689847871849, -185.4062500020484094 ) ) ;
#9040 = CARTESIAN_POINT ( 'NONE',  ( -2.293366432827344421E-15, -12.48450537969573659, -46.71875000204835970 ) ) ;
#9041 = CARTESIAN_POINT ( 'NONE',  ( 7.070501591499377789E-16, 11.54700538379251284, -165.5000000040967905 ) ) ;
#9042 = CARTESIAN_POINT ( 'NONE',  ( -9.999999999999998224, 1.224646799147353059E-15, -85.62500000409677625 ) ) ;
#9043 = CARTESIAN_POINT ( 'NONE',  ( 10.81189881249999551, -6.242252689847874514, -11.96875000204836326 ) ) ;
#9044 = CARTESIAN_POINT ( 'NONE',  ( -9.999999999999227285, -5.773502691896698735, -127.1249999999999574 ) ) ;
#9045 = CARTESIAN_POINT ( 'NONE',  ( -2.293366432827344421E-15, -12.48450537969573659, -118.7187500020483952 ) ) ;
#9046 = CARTESIAN_POINT ( 'NONE',  ( 7.070501591499377789E-16, 11.54700538379251284, -90.12499999999997158 ) ) ;
#9047 = CARTESIAN_POINT ( 'NONE',  ( 5.405949406249992428, -9.363379034771808662, -16.78125000204835970 ) ) ;
#9048 = CARTESIAN_POINT ( 'NONE',  ( 9.999999999999996447, -5.773502691896262640, -101.5000000040967905 ) ) ;
#9049 = CARTESIAN_POINT ( 'NONE',  ( -10.81189881249999907, -6.242252689847864744, -119.1562500020484237 ) ) ;
#9050 = CARTESIAN_POINT ( 'NONE',  ( -10.81189881249999729, -6.242252689847864744, -95.15625000204839523 ) ) ;
#9051 = ORIENTED_EDGE ( 'NONE', *, *, #8704, .T. ) ;
#9052 = CARTESIAN_POINT ( 'NONE',  ( -5.000000000000003553, -8.660254037844383745, -95.87500000409677625 ) ) ;
#9053 = CARTESIAN_POINT ( 'NONE',  ( -10.00000000000102496, 5.773502691895664007, -4.374999999999930722 ) ) ;
#9054 = CARTESIAN_POINT ( 'NONE',  ( -5.405949406249996869, 9.363379034771805109, -158.5312500020484094 ) ) ;
#9055 = CARTESIAN_POINT ( 'NONE',  ( -2.293366432827344421E-15, -12.48450537969573659, -52.71875000204837391 ) ) ;
#9056 = ORIENTED_EDGE ( 'NONE', *, *, #17227, .T. ) ;
#9057 = CARTESIAN_POINT ( 'NONE',  ( 9.999999999999998224, 0.000000000000000000, -21.49999999999996447 ) ) ;
#9058 = CARTESIAN_POINT ( 'NONE',  ( 10.81189881249999551, -6.242252689847874514, -25.65625000204838813 ) ) ;
#9059 = CARTESIAN_POINT ( 'NONE',  ( 5.000000000000000000, 8.660254037844385522, -150.2500000000000000 ) ) ;
#9060 = CARTESIAN_POINT ( 'NONE',  ( -10.00000000000000000, -5.773502691896251982, -24.00000000409677270 ) ) ;
#9061 = SECURITY_CLASSIFICATION ( '', '', #29556 ) ;
#9062 = CARTESIAN_POINT ( 'NONE',  ( -9.999999999999998224, 1.224646799147353059E-15, -120.1250000040967905 ) ) ;
#9064 = ORIENTED_EDGE ( 'NONE', *, *, #41763, .T. ) ;
#9063 = CARTESIAN_POINT ( 'NONE',  ( -10.81189881249999729, 6.242252689847871849, -126.9062500020483810 ) ) ;
#9065 = DIRECTION ( 'NONE',  ( 0.000000000000000000, -0.000000000000000000, 1.000000000000000000 ) ) ;
#9066 = ADVANCED_FACE ( 'NONE', ( #7817 ), #30906, .F. ) ;
#9067 = VERTEX_POINT ( 'NONE', #27229 ) ;
#9068 = EDGE_CURVE ( 'NONE', #37209, #32336, #3670, .T. ) ;
#9069 = CARTESIAN_POINT ( 'NONE',  ( -2.293366432827344421E-15, -12.48450537969573659, -51.40625000204838102 ) ) ;
#9070 = CALENDAR_DATE ( 2026, 28, 9 ) ;
#9071 = CARTESIAN_POINT ( 'NONE',  ( -10.81189881249999729, 6.242252689847871849, -104.2187500020483810 ) ) ;
#9073 = ORIENTED_EDGE ( 'NONE', *, *, #12694, .T. ) ;
#9072 = ORIENTED_EDGE ( 'NONE', *, *, #9834, .F. ) ;
#9074 = DIRECTION ( 'NONE',  ( -0.000000000000000000, -0.000000000000000000, 1.000000000000000000 ) ) ;
#9075 = CC_DESIGN_PERSON_AND_ORGANIZATION_ASSIGNMENT ( #28293, #20353, ( #15921 ) ) ;
#9076 = CARTESIAN_POINT ( 'NONE',  ( 7.070501591499376803E-16, 11.54700538379251284, -171.1250000000000000 ) ) ;
#9077 = CARTESIAN_POINT ( 'NONE',  ( -10.81189881249999907, -6.242252689847864744, -156.4687500020484379 ) ) ;
#9078 = CARTESIAN_POINT ( 'NONE',  ( 10.81189881249999907, 6.242252689847868297, -190.4062500020484094 ) ) ;
#9079 = CARTESIAN_POINT ( 'NONE',  ( -10.81189881249999729, 6.242252689847871849, -3.718750002048365477 ) ) ;
#9080 = DIRECTION ( 'NONE',  ( 1.000000000000000000, 0.000000000000000000, 0.000000000000000000 ) ) ;
#9081 = CARTESIAN_POINT ( 'NONE',  ( 10.81189881249999551, -6.242252689847874514, -137.9687500020483810 ) ) ;
#9082 = CARTESIAN_POINT ( 'NONE',  ( -10.81189881249999729, 6.242252689847871849, -108.7187500020483810 ) ) ;
#9083 = CYLINDRICAL_SURFACE ( 'NONE', #19422, 9.999999999999998224 ) ;
#9084 = CARTESIAN_POINT ( 'NONE',  ( 5.405949406249999534, 9.363379034771803333, -113.7812500020483952 ) ) ;
#9085 = CARTESIAN_POINT ( 'NONE',  ( -5.000000000000003553, -8.660254037844383745, -196.3750000040967905 ) ) ;
#9086 = CARTESIAN_POINT ( 'NONE',  ( 5.405949406249999534, 9.363379034771803333, -119.5937500020483810 ) ) ;
#9087 = CARTESIAN_POINT ( 'NONE',  ( 10.81189881249999729, 6.242252689847867408, -194.9062500020484094 ) ) ;
#9088 = CARTESIAN_POINT ( 'NONE',  ( -9.999999999999998224, 1.224646799147353059E-15, -6.125000004096770034 ) ) ;
#9089 = CARTESIAN_POINT ( 'NONE',  ( -2.121150477449813534E-15, -11.54700538379251284, -137.3750000000000000 ) ) ;
#9090 = CARTESIAN_POINT ( 'NONE',  ( 7.070501591499377789E-16, 11.54700538379251284, -16.62499999999997158 ) ) ;
#9091 = EDGE_CURVE ( 'NONE', #20035, #2553, #21573, .T. ) ;
#9092 = APPROVAL_PERSON_ORGANIZATION ( #5787, #5371, #19149 ) ;
#9093 = CARTESIAN_POINT ( 'NONE',  ( 10.81189881249999729, 6.242252689847867408, -65.71875000204836681 ) ) ;
#9094 = CARTESIAN_POINT ( 'NONE',  ( 7.644554776091147741E-16, 12.48450537969573659, -53.46875000204837391 ) ) ;
#9095 = CARTESIAN_POINT ( 'NONE',  ( 9.999999999999996447, -5.773502691896262640, -191.5000000040968189 ) ) ;
#9096 = CARTESIAN_POINT ( 'NONE',  ( -10.81189881249999729, 6.242252689847871849, -26.40625000204837747 ) ) ;
#9097 = CARTESIAN_POINT ( 'NONE',  ( 10.81189881249999729, 0.000000000000000000, -35.84375000204836681 ) ) ;
#9098 = CARTESIAN_POINT ( 'NONE',  ( -10.81189881249999729, 6.242252689847871849, -147.7187500020484094 ) ) ;
#9099 = CARTESIAN_POINT ( 'NONE',  ( 10.00000000000000000, 5.773502691896255534, -115.8749999999999858 ) ) ;
#9100 =( BOUNDED_CURVE ( )  B_SPLINE_CURVE ( 2, ( #20191, #19547, #3167, #3593, #7038, #16725, #26673 ),
 .UNSPECIFIED., .F., .F. ) 
 B_SPLINE_CURVE_WITH_KNOTS ( ( 3, 2, 2, 3 ),
 ( 0.3022388059701494045, 0.3034825870646767343, 0.3047263681592040085, 0.3059701492537313383 ),
 .UNSPECIFIED. ) 
 CURVE ( )  GEOMETRIC_REPRESENTATION_ITEM ( )  RATIONAL_B_SPLINE_CURVE ( ( 0.9999999999999820144, 0.8660254037844566932, 1.000000000000000000, 0.8660254037844387076, 1.000000000000000000, 0.8660254037844387076, 1.000000000000000000 ) ) 
 REPRESENTATION_ITEM ( '' )  );
#9101 = CARTESIAN_POINT ( 'NONE',  ( 9.999999999999998224, 0.000000000000000000, -63.49999999999997158 ) ) ;
#9102 = CARTESIAN_POINT ( 'NONE',  ( 5.405949406249992428, -9.363379034771808662, -142.7812500020483810 ) ) ;
#9103 = CARTESIAN_POINT ( 'NONE',  ( -5.405949406250003975, -9.363379034771801557, -8.031250002048350822 ) ) ;
#9104 = ORIENTED_EDGE ( 'NONE', *, *, #4578, .F. ) ;
#9105 = CARTESIAN_POINT ( 'NONE',  ( 9.999999999999998224, 0.000000000000000000, -164.0000000000000000 ) ) ;
#9106 = CARTESIAN_POINT ( 'NONE',  ( 7.070501591499377789E-16, 11.54700538379251284, -114.5000000040967905 ) ) ;
#9107 = CARTESIAN_POINT ( 'NONE',  ( -9.999999999999998224, 1.224646799147353059E-15, -8.749999999999952038 ) ) ;
#9108 = CARTESIAN_POINT ( 'NONE',  ( -10.81189881249999729, 6.242252689847871849, -72.71875000204835260 ) ) ;
#9109 = CARTESIAN_POINT ( 'NONE',  ( 7.070501591499377789E-16, 11.54700538379251284, -43.62499999999996447 ) ) ;
#9110 = CARTESIAN_POINT ( 'NONE',  ( 10.00000000000000000, 5.773502691896255534, -23.25000000409677270 ) ) ;
#9111 = CARTESIAN_POINT ( 'NONE',  ( 5.405949406249999534, 9.363379034771803333, -55.28125000204836681 ) ) ;
#9112 = CARTESIAN_POINT ( 'NONE',  ( -1.040834085586084257E-14, -20.00000000000000355, 22.49999999999999289 ) ) ;
#9113 = CARTESIAN_POINT ( 'NONE',  ( -2.293366432827344421E-15, -12.48450537969573659, -37.90625000204836681 ) ) ;
#9114 = CARTESIAN_POINT ( 'NONE',  ( -8.660254037844447694, 15.00000000000010836, 49.99999999999998579 ) ) ;
#9115 = CARTESIAN_POINT ( 'NONE',  ( 10.81189881249999551, -6.242252689847874514, -148.6562500020484094 ) ) ;
#9116 = CARTESIAN_POINT ( 'NONE',  ( -10.81189881249999729, 6.242252689847871849, -152.4062500020483810 ) ) ;
#9117 = CARTESIAN_POINT ( 'NONE',  ( 7.070501591499376803E-16, 11.54700538379251284, -78.50000000409677625 ) ) ;
#9118 = CARTESIAN_POINT ( 'NONE',  ( 4.999999999999992006, -8.660254037844389075, -57.74999999999997158 ) ) ;
#9119 = ORIENTED_EDGE ( 'NONE', *, *, #19327, .F. ) ;
#9120 = ORIENTED_EDGE ( 'NONE', *, *, #25986, .T. ) ;
#9121 = ORIENTED_EDGE ( 'NONE', *, *, #3109, .T. ) ;
#9122 = DIRECTION ( 'NONE',  ( 0.000000000000000000, 0.000000000000000000, 1.000000000000000000 ) ) ;
#9123 = CARTESIAN_POINT ( 'NONE',  ( 10.81189881249999551, -6.242252689847874514, -182.9687500020484094 ) ) ;
#9124 = AXIS2_PLACEMENT_3D ( 'NONE', #41725, #38502, #39137 ) ;
#9126 = EDGE_CURVE ( 'NONE', #13498, #36973, #11082, .T. ) ;
#9125 = CARTESIAN_POINT ( 'NONE',  ( 10.81189881249999729, 0.000000000000000000, -31.34375000204836681 ) ) ;
#9127 = CARTESIAN_POINT ( 'NONE',  ( 9.999999999999998224, 0.000000000000000000, -114.4999999999999858 ) ) ;
#9128 = CARTESIAN_POINT ( 'NONE',  ( -10.81189881249999729, 1.324075727343319199E-15, -167.0937500020484094 ) ) ;
#9129 = CARTESIAN_POINT ( 'NONE',  ( 5.405949406249992428, -9.363379034771808662, -151.5937500020483810 ) ) ;
#9130 = LINE ( 'NONE', #18623, #41739 ) ;
#9131 = CARTESIAN_POINT ( 'NONE',  ( -5.405949406250003975, -9.363379034771801557, -136.8437500020484094 ) ) ;
#9132 = CARTESIAN_POINT ( 'NONE',  ( 10.81189881249999907, 6.242252689847868297, -140.9062500020484094 ) ) ;
#9133 = CARTESIAN_POINT ( 'NONE',  ( 10.81189881249999551, -6.242252689847874514, -17.96875000204837036 ) ) ;
#9134 = CARTESIAN_POINT ( 'NONE',  ( -5.405949406249996869, 9.363379034771805109, -144.8437500020483810 ) ) ;
#9135 = CARTESIAN_POINT ( 'NONE',  ( 0.000000000000000000, 0.000000000000000000, -99.99999999999998579 ) ) ;
#9136 =( BOUNDED_CURVE ( )  B_SPLINE_CURVE ( 2, ( #14254, #17716, #37592, #33943, #30911, #27671, #31133 ),
 .UNSPECIFIED., .F., .F. ) 
 B_SPLINE_CURVE_WITH_KNOTS ( ( 3, 2, 2, 3 ),
 ( 0.8917910447761197013, 0.8930348258706470865, 0.8942786069651743608, 0.8955223880597017461 ),
 .UNSPECIFIED. ) 
 CURVE ( )  GEOMETRIC_REPRESENTATION_ITEM ( )  RATIONAL_B_SPLINE_CURVE ( ( 0.9999999999999641398, 0.8660254037844745678, 1.000000000000000000, 0.8660254037844387076, 1.000000000000000000, 0.8660254037844148378, 1.000000000000023981 ) ) 
 REPRESENTATION_ITEM ( '' )  );
#9137 = LINE ( 'NONE', #2259, #30271 ) ;
#9138 = CARTESIAN_POINT ( 'NONE',  ( 10.00000000000000000, 5.773502691896255534, -163.8750000000000000 ) ) ;
#9139 = CARTESIAN_POINT ( 'NONE',  ( 5.405949406249999534, 9.363379034771803333, -83.59375000204836681 ) ) ;
#9140 = CARTESIAN_POINT ( 'NONE',  ( -2.121150477449813534E-15, -11.54700538379251284, -113.7500000040967763 ) ) ;
#9141 = CARTESIAN_POINT ( 'NONE',  ( -5.405949406249996869, 9.363379034771805109, -47.53125000204838813 ) ) ;
#9142 = CARTESIAN_POINT ( 'NONE',  ( 10.81189881249999907, 6.242252689847868297, -59.71875000204838102 ) ) ;
#9143 = CARTESIAN_POINT ( 'NONE',  ( -4.999999999999996447, 8.660254037844387298, -90.37500000409677625 ) ) ;
#9144 = CARTESIAN_POINT ( 'NONE',  ( 5.405949406249992428, -9.363379034771808662, -174.0937500020484094 ) ) ;
#9145 = CARTESIAN_POINT ( 'NONE',  ( 7.070501591499377789E-16, 11.54700538379251284, -135.1250000000000000 ) ) ;
#9146 = CARTESIAN_POINT ( 'NONE',  ( 10.81189881249999729, 0.000000000000000000, -147.0312500020483810 ) ) ;
#9147 = DIRECTION ( 'NONE',  ( -1.000000000000000000, 0.000000000000000000, 0.000000000000000000 ) ) ;
#9148 = CARTESIAN_POINT ( 'NONE',  ( -10.81189881249999907, -6.242252689847864744, -38.15625000204835970 ) ) ;
#9149 = CARTESIAN_POINT ( 'NONE',  ( -5.000000000000003553, -8.660254037844383745, -121.3750000040967905 ) ) ;
#9150 = CARTESIAN_POINT ( 'NONE',  ( -10.00000000000000000, -5.773502691896251982, -98.62499999999998579 ) ) ;
#9151 = ORIENTED_EDGE ( 'NONE', *, *, #29092, .F. ) ;
#9152 =( BOUNDED_CURVE ( )  B_SPLINE_CURVE ( 2, ( #42152, #42360, #6548, #2276, #19074, #2682, #35283 ),
 .UNSPECIFIED., .F., .F. ) 
 B_SPLINE_CURVE_WITH_KNOTS ( ( 3, 2, 2, 3 ),
 ( 0.7500000000000001110, 0.7512437810945274963, 0.7524875621890549926, 0.7537313432835822669 ),
 .UNSPECIFIED. ) 
 CURVE ( )  GEOMETRIC_REPRESENTATION_ITEM ( )  RATIONAL_B_SPLINE_CURVE ( ( 0.9999999999999880096, 0.8660254037844506980, 1.000000000000000000, 0.8660254037844387076, 1.000000000000000000, 0.8660254037844148378, 1.000000000000023981 ) ) 
 REPRESENTATION_ITEM ( '' )  );
#9153 = CARTESIAN_POINT ( 'NONE',  ( 10.81189881249999551, -6.242252689847874514, -115.6562500020483810 ) ) ;
#9154 = CARTESIAN_POINT ( 'NONE',  ( 9.999999999999996447, -5.773502691896262640, -140.5000000040967905 ) ) ;
#9155 = CARTESIAN_POINT ( 'NONE',  ( 10.81189881249999551, -6.242252689847874514, -174.1562500020484094 ) ) ;
#9156 = CARTESIAN_POINT ( 'NONE',  ( 4.999999999999992006, -8.660254037844389075, -46.12500000409677625 ) ) ;
#9157 = CARTESIAN_POINT ( 'NONE',  ( -10.81189881249999729, 6.242252689847871849, -63.90625000204838813 ) ) ;
#9158 = CARTESIAN_POINT ( 'NONE',  ( 5.000000000000000000, 8.660254037844385522, -84.24999999999997158 ) ) ;
#9159 = CARTESIAN_POINT ( 'NONE',  ( -10.81189881249999729, 6.242252689847871849, -170.4062500020484094 ) ) ;
#9160 = CARTESIAN_POINT ( 'NONE',  ( -9.999999999999998224, 1.224646799147353059E-15, -106.6250000040967763 ) ) ;
#9161 = CARTESIAN_POINT ( 'NONE',  ( -4.999999999999996447, 8.660254037844387298, -64.49999999999997158 ) ) ;
#9162 = ORIENTED_EDGE ( 'NONE', *, *, #42504, .F. ) ;
#9163 = CARTESIAN_POINT ( 'NONE',  ( -10.00000000000051337, 5.773502691895962435, -123.2500000040967763 ) ) ;
#9164 = DIRECTION ( 'NONE',  ( 1.000000000000000000, 0.000000000000000000, 0.000000000000000000 ) ) ;
#9166 = ORIENTED_EDGE ( 'NONE', *, *, #10072, .T. ) ;
#9165 = CARTESIAN_POINT ( 'NONE',  ( 10.81189881249999907, 6.242252689847868297, -80.90625000204839523 ) ) ;
#9168 = ORIENTED_EDGE ( 'NONE', *, *, #8561, .F. ) ;
#9167 = CARTESIAN_POINT ( 'NONE',  ( -5.000000000000003553, -8.660254037844383745, -119.5000000000000000 ) ) ;
#9169 = ORIENTED_EDGE ( 'NONE', *, *, #36496, .T. ) ;
#9170 = CARTESIAN_POINT ( 'NONE',  ( -2.293366432827344421E-15, -12.48450537969573659, -33.21875000204834549 ) ) ;
#9171 = CARTESIAN_POINT ( 'NONE',  ( -10.00000000000000000, -5.773502691896252870, -171.0000000040967905 ) ) ;
#9172 = CARTESIAN_POINT ( 'NONE',  ( -10.81189881249999729, 1.324075727343319199E-15, -8.281250002048350822 ) ) ;
#9174 = EDGE_LOOP ( 'NONE', ( #39456, #3783, #36548, #35412 ) ) ;
#9173 = CARTESIAN_POINT ( 'NONE',  ( 5.405949406249992428, -9.363379034771808662, -55.59375000204835970 ) ) ;
#9175 = FACE_OUTER_BOUND ( 'NONE', #41140, .T. ) ;
#9176 = CARTESIAN_POINT ( 'NONE',  ( -4.999999999999996447, 8.660254037844387298, -28.49999999999997158 ) ) ;
#9177 = CARTESIAN_POINT ( 'NONE',  ( -10.81189881249999729, -6.242252689847864744, -186.4687500020484094 ) ) ;
#9178 = CARTESIAN_POINT ( 'NONE',  ( 10.81189881249999551, -6.242252689847874514, -175.4687500020484094 ) ) ;
#9179 = CARTESIAN_POINT ( 'NONE',  ( -5.405949406249996869, 9.363379034771805109, -155.3437500020483810 ) ) ;
#9180 = CARTESIAN_POINT ( 'NONE',  ( -10.81189881249999729, 1.324075727343319199E-15, -168.5937500020484094 ) ) ;
#9181 = CARTESIAN_POINT ( 'NONE',  ( 9.999999999999998224, 0.000000000000000000, -18.87500000409675494 ) ) ;
#9182 = CARTESIAN_POINT ( 'NONE',  ( 9.999999999999998224, 0.000000000000000000, -162.8750000040967905 ) ) ;
#9183 = CARTESIAN_POINT ( 'NONE',  ( -10.00000000000000000, -5.773502691896251982, -193.1250000000000284 ) ) ;
#9184 = CARTESIAN_POINT ( 'NONE',  ( 5.405949406249999534, 9.363379034771803333, -109.0937500020483810 ) ) ;
#9185 = CARTESIAN_POINT ( 'NONE',  ( -9.999999999999998224, 1.224646799147353059E-15, -64.62500000409676204 ) ) ;
#9186 = CARTESIAN_POINT ( 'NONE',  ( -2.293366432827344421E-15, -12.48450537969573659, -78.40625000204838102 ) ) ;
#9187 = CARTESIAN_POINT ( 'NONE',  ( -10.81189881249999729, -6.242252689847864744, -94.96875000204838102 ) ) ;
#9188 = CARTESIAN_POINT ( 'NONE',  ( -10.81189881249999729, 1.324075727343319199E-15, -62.28125000204837391 ) ) ;
#9189 = CARTESIAN_POINT ( 'NONE',  ( 9.999999999999998224, 0.000000000000000000, -147.8750000040967905 ) ) ;
#9190 = CARTESIAN_POINT ( 'NONE',  ( -10.00000000000000000, -5.773502691896251982, -119.6249999999999858 ) ) ;
#9191 = EDGE_CURVE ( 'NONE', #31697, #39083, #27112, .T. ) ;
#9192 = ORIENTED_EDGE ( 'NONE', *, *, #5615, .T. ) ;
#9193 = CARTESIAN_POINT ( 'NONE',  ( 10.81189881249999729, 0.000000000000000000, -144.0312500020483810 ) ) ;
#9194 = CARTESIAN_POINT ( 'NONE',  ( 5.405949406249992428, -9.363379034771808662, -157.7812500020484094 ) ) ;
#9195 = CARTESIAN_POINT ( 'NONE',  ( -5.405949406249996869, 9.363379034771805109, -194.5312500020484094 ) ) ;
#9196 = DIRECTION ( 'NONE',  ( -0.000000000000000000, -0.000000000000000000, -1.000000000000000000 ) ) ;
#9197 = CARTESIAN_POINT ( 'NONE',  ( 7.644554776091147741E-16, 12.48450537969573659, -89.46875000204838102 ) ) ;
#9198 = ORIENTED_EDGE ( 'NONE', *, *, #26935, .T. ) ;
#9199 = CARTESIAN_POINT ( 'NONE',  ( 10.00000000000000000, 5.773502691896255534, -64.87499999999998579 ) ) ;
#9200 = CARTESIAN_POINT ( 'NONE',  ( -5.405949406249996869, 9.363379034771805109, -186.8437500020483810 ) ) ;
#9201 = CARTESIAN_POINT ( 'NONE',  ( -2.121150477449813534E-15, -11.54700538379251284, -76.25000000409677625 ) ) ;
#9202 = CARTESIAN_POINT ( 'NONE',  ( 4.999999999999992006, -8.660254037844389075, -116.6250000040967905 ) ) ;
#9203 = FACE_OUTER_BOUND ( 'NONE', #14753, .T. ) ;
#9204 = CARTESIAN_POINT ( 'NONE',  ( 10.81189881249999551, -6.242252689847874514, -82.65625000204836681 ) ) ;
#9205 = CARTESIAN_POINT ( 'NONE',  ( 10.81189881249999729, 6.242252689847867408, -65.90625000204839523 ) ) ;
#9206 = CARTESIAN_POINT ( 'NONE',  ( 9.999999999999998224, 0.000000000000000000, -56.37500000409676204 ) ) ;
#9207 = CARTESIAN_POINT ( 'NONE',  ( -10.00000000000051337, 5.773502691895962435, -93.25000000409676204 ) ) ;
#9208 = CARTESIAN_POINT ( 'NONE',  ( -10.81189881249999907, -6.242252689847864744, -15.46875000204836503 ) ) ;
#9209 = CARTESIAN_POINT ( 'NONE',  ( -5.405949406249996869, 9.363379034771805109, -191.5312500020484094 ) ) ;
#9210 = CARTESIAN_POINT ( 'NONE',  ( -2.293366432827344421E-15, -12.48450537969573659, -19.90625000204837391 ) ) ;
#9211 = CARTESIAN_POINT ( 'NONE',  ( 5.405949406249999534, 9.363379034771803333, -2.593750002048367254 ) ) ;
#9212 = CARTESIAN_POINT ( 'NONE',  ( 9.999999999999479527, 5.773502691896553074, -140.2500000040967620 ) ) ;
#9213 =( BOUNDED_CURVE ( )  B_SPLINE_CURVE ( 2, ( #36799, #36585, #17355, #29914, #33579, #3585, #13475 ),
 .UNSPECIFIED., .F., .F. ) 
 B_SPLINE_CURVE_WITH_KNOTS ( ( 3, 2, 2, 3 ),
 ( 0.1380597014925373234, 0.1393034825870646809, 0.1405472636815920384, 0.1417910447761193959 ),
 .UNSPECIFIED. ) 
 CURVE ( )  GEOMETRIC_REPRESENTATION_ITEM ( )  RATIONAL_B_SPLINE_CURVE ( ( 1.000000000000000000, 0.8660254037844387076, 1.000000000000000000, 0.8660254037844387076, 1.000000000000000000, 0.8660254037844387076, 1.000000000000000000 ) ) 
 REPRESENTATION_ITEM ( '' )  );
#9214 = CARTESIAN_POINT ( 'NONE',  ( -9.999999999999998224, 1.224646799147353059E-15, -108.1250000040967763 ) ) ;
#9215 = DIRECTION ( 'NONE',  ( 1.000000000000000000, 0.000000000000000000, 0.000000000000000000 ) ) ;
#9216 = EDGE_CURVE ( 'NONE', #1967, #25696, #653, .T. ) ;
#9217 = CARTESIAN_POINT ( 'NONE',  ( 7.070501591499377789E-16, 11.54700538379251284, -174.1250000000000000 ) ) ;
#9218 = CARTESIAN_POINT ( 'NONE',  ( 9.999999999999998224, 0.000000000000000000, -1.999999999999974021 ) ) ;
#9220 = ORIENTED_EDGE ( 'NONE', *, *, #39923, .F. ) ;
#9219 = CARTESIAN_POINT ( 'NONE',  ( 7.644554776091147741E-16, 12.48450537969573659, -98.65625000204838102 ) ) ;
#9221 = ADVANCED_FACE ( 'NONE', ( #31127 ), #25505, .T. ) ;
#9222 = CARTESIAN_POINT ( 'NONE',  ( 5.000000000000000000, 8.660254037844385522, -37.74999999999997868 ) ) ;
#9223 = ORIENTED_EDGE ( 'NONE', *, *, #16683, .T. ) ;
#9224 = ORIENTED_EDGE ( 'NONE', *, *, #9538, .T. ) ;
#9225 = CARTESIAN_POINT ( 'NONE',  ( -10.81189881249999729, 1.324075727343319199E-15, -26.28125000204836681 ) ) ;
#9226 = CALENDAR_DATE ( 2026, 28, 9 ) ;
#9227 = CARTESIAN_POINT ( 'NONE',  ( 10.81189881249999907, 6.242252689847868297, -77.71875000204838102 ) ) ;
#9228 = CARTESIAN_POINT ( 'NONE',  ( 9.999999999999866773, -5.773502691896336358, -173.1250000000000000 ) ) ;
#9229 = FACE_OUTER_BOUND ( 'NONE', #38797, .T. ) ;
#9230 = CARTESIAN_POINT ( 'NONE',  ( -1.040834085586084257E-14, -139.9999999999999716, 22.49999999999999289 ) ) ;
#9231 = CARTESIAN_POINT ( 'NONE',  ( -9.999999999999998224, 1.224646799147353059E-15, -49.24999999999998579 ) ) ;
#9232 = CARTESIAN_POINT ( 'NONE',  ( 5.405949406249992428, -9.363379034771808662, -154.7812500020484094 ) ) ;
#9233 = CARTESIAN_POINT ( 'NONE',  ( -4.999999999999996447, 8.660254037844387298, -9.375000004096744277 ) ) ;
#9234 = DIRECTION ( 'NONE',  ( 0.000000000000000000, 0.000000000000000000, 1.000000000000000000 ) ) ;
#9235 = CARTESIAN_POINT ( 'NONE',  ( -5.405949406249996869, 9.363379034771805109, -131.3437500020484094 ) ) ;
#9236 = CARTESIAN_POINT ( 'NONE',  ( 10.81189881249999551, -6.242252689847874514, -99.15625000204838102 ) ) ;
#9237 = CARTESIAN_POINT ( 'NONE',  ( 5.405949406249999534, 9.363379034771803333, -113.5937500020483810 ) ) ;
#9238 = CARTESIAN_POINT ( 'NONE',  ( -10.81189881249999907, -6.242252689847864744, -79.96875000204836681 ) ) ;
#9239 = CARTESIAN_POINT ( 'NONE',  ( -2.293366432827344421E-15, -12.48450537969573659, -82.90625000204838102 ) ) ;
#9240 = CARTESIAN_POINT ( 'NONE',  ( -10.00000000000000000, -5.773502691896251982, -172.5000000040967905 ) ) ;
#9241 = CARTESIAN_POINT ( 'NONE',  ( 7.644554776091147741E-16, 12.48450537969573659, -164.6562500020484094 ) ) ;
#9242 = CARTESIAN_POINT ( 'NONE',  ( -5.405949406250003975, -9.363379034771801557, -179.0312500020483810 ) ) ;
#9243 = CARTESIAN_POINT ( 'NONE',  ( 7.644554776091147741E-16, 12.48450537969573659, -44.46875000204836681 ) ) ;
#9244 = CARTESIAN_POINT ( 'NONE',  ( -2.121150477449813534E-15, -11.54700538379251284, -154.2500000040967620 ) ) ;
#9245 = CARTESIAN_POINT ( 'NONE',  ( -10.81189881249999729, 6.242252689847871849, -0.9062500020483681418 ) ) ;
#9246 = CARTESIAN_POINT ( 'NONE',  ( -5.405949406250003975, -9.363379034771801557, -7.843750002048343717 ) ) ;
#9247 = CARTESIAN_POINT ( 'NONE',  ( 9.999999999999998224, 0.000000000000000000, -6.499999999999977796 ) ) ;
#9248 = CARTESIAN_POINT ( 'NONE',  ( 5.405949406249992428, -9.363379034771808662, -111.0937500020483810 ) ) ;
#9249 = ADVANCED_FACE ( 'NONE', ( #24658 ), #21614, .F. ) ;
#9250 = CARTESIAN_POINT ( 'NONE',  ( 10.00000000000000000, 5.773502691896255534, -93.37499999999997158 ) ) ;
#9251 = CARTESIAN_POINT ( 'NONE',  ( 5.405949406249992428, -9.363379034771808662, -9.281250002048352599 ) ) ;
#9252 = CARTESIAN_POINT ( 'NONE',  ( 9.999999999999996447, -5.773502691896262640, -100.0000000040967763 ) ) ;
#9253 = CARTESIAN_POINT ( 'NONE',  ( 9.999999999999994671, -5.773502691896262640, -170.5000000040967905 ) ) ;
#9254 = CARTESIAN_POINT ( 'NONE',  ( -5.405949406250003975, -9.363379034771801557, -117.5312500020483952 ) ) ;
#9255 = CARTESIAN_POINT ( 'NONE',  ( -10.81189881249999729, -6.242252689847864744, -93.65625000204840944 ) ) ;
#9256 = ORIENTED_EDGE ( 'NONE', *, *, #23486, .T. ) ;
#9257 =( BOUNDED_CURVE ( )  B_SPLINE_CURVE ( 2, ( #36270, #29165, #15969, #32622, #32201, #22469, #16384 ),
 .UNSPECIFIED., .F., .F. ) 
 B_SPLINE_CURVE_WITH_KNOTS ( ( 3, 2, 2, 3 ),
 ( 0.2798507462686568026, 0.2810945273631841879, 0.2823383084577115731, 0.2835820895522389029 ),
 .UNSPECIFIED. ) 
 CURVE ( )  GEOMETRIC_REPRESENTATION_ITEM ( )  RATIONAL_B_SPLINE_CURVE ( ( 0.9999999999999880096, 0.8660254037844506980, 1.000000000000000000, 0.8660254037844387076, 1.000000000000000000, 0.8660254037844267172, 1.000000000000011990 ) ) 
 REPRESENTATION_ITEM ( '' )  );
#9258 = CARTESIAN_POINT ( 'NONE',  ( 9.999999999999998224, 0.000000000000000000, -92.37500000409677625 ) ) ;
#9259 = CARTESIAN_POINT ( 'NONE',  ( 9.999999999999998224, 0.000000000000000000, -29.37500000409676204 ) ) ;
#9260 = CARTESIAN_POINT ( 'NONE',  ( 5.405949406249999534, 9.363379034771803333, -40.09375000204837391 ) ) ;
#9261 = ORIENTED_EDGE ( 'NONE', *, *, #26728, .F. ) ;
#9262 = CARTESIAN_POINT ( 'NONE',  ( -4.999999999999996447, 8.660254037844387298, -16.49999999999995737 ) ) ;
#9263 = CARTESIAN_POINT ( 'NONE',  ( -10.81189881249999729, 1.324075727343319199E-15, -23.28125000204836326 ) ) ;
#9264 = CARTESIAN_POINT ( 'NONE',  ( 9.999999999999998224, 0.000000000000000000, -156.5000000000000000 ) ) ;
#9265 = CARTESIAN_POINT ( 'NONE',  ( 7.070501591499377789E-16, 11.54700538379251284, -21.50000000409676915 ) ) ;
#9266 = CARTESIAN_POINT ( 'NONE',  ( -5.000000000000003553, -8.660254037844383745, -119.8750000040967905 ) ) ;
#9268 = ORIENTED_EDGE ( 'NONE', *, *, #31909, .F. ) ;
#9267 = CARTESIAN_POINT ( 'NONE',  ( -5.405949406249996869, 9.363379034771805109, -127.0312500020483952 ) ) ;
#9269 = CARTESIAN_POINT ( 'NONE',  ( 5.000000000000000000, 8.660254037844385522, -117.6250000040967905 ) ) ;
#9270 = ORIENTED_EDGE ( 'NONE', *, *, #18258, .F. ) ;
#9271 = CARTESIAN_POINT ( 'NONE',  ( -10.81189881249999729, 1.324075727343319199E-15, -50.28125000204835970 ) ) ;
#9272 = MECHANICAL_CONTEXT ( 'NONE', #7703, 'mechanical' ) ;
#9273 = CARTESIAN_POINT ( 'NONE',  ( -5.405949406249996869, 9.363379034771805109, -104.3437500020483810 ) ) ;
#9275 = ORIENTED_EDGE ( 'NONE', *, *, #24028, .T. ) ;
#9274 = ORIENTED_EDGE ( 'NONE', *, *, #7790, .T. ) ;
#9276 = CARTESIAN_POINT ( 'NONE',  ( -10.00000000000012790, -5.773502691896177375, -175.5000000040967905 ) ) ;
#9277 = CARTESIAN_POINT ( 'NONE',  ( 9.999999999999998224, 0.000000000000000000, -144.8750000040967905 ) ) ;
#9278 = CARTESIAN_POINT ( 'NONE',  ( -10.81189881249999729, 1.324075727343319199E-15, -147.5937500020483810 ) ) ;
#9279 = CARTESIAN_POINT ( 'NONE',  ( -5.405949406249996869, 9.363379034771805109, -179.5312500020483810 ) ) ;
#9280 = CARTESIAN_POINT ( 'NONE',  ( -10.81189881249999907, -6.242252689847864744, -10.96875000204836859 ) ) ;
#9281 = FACE_OUTER_BOUND ( 'NONE', #28596, .T. ) ;
#9282 = CARTESIAN_POINT ( 'NONE',  ( 10.81189881249999729, 6.242252689847867408, -139.2187500020483810 ) ) ;
#9283 = CARTESIAN_POINT ( 'NONE',  ( 7.644554776091147741E-16, 12.48450537969573659, -104.4687500020483668 ) ) ;
#9284 = CARTESIAN_POINT ( 'NONE',  ( -2.121150477449813534E-15, -11.54700538379251284, -147.8750000000000000 ) ) ;
#9285 = CARTESIAN_POINT ( 'NONE',  ( -10.81189881249999907, -6.242252689847864744, -107.1562500020483952 ) ) ;
#9286 = CARTESIAN_POINT ( 'NONE',  ( -9.999999999999998224, 5.773502691896259087, -190.7500000040968189 ) ) ;
#9287 = CARTESIAN_POINT ( 'NONE',  ( 10.81189881249999729, 0.000000000000000000, -125.8437500020483952 ) ) ;
#9288 = CARTESIAN_POINT ( 'NONE',  ( -10.81189881249999729, 6.242252689847871849, -189.9062500020484379 ) ) ;
#9289 = AXIS2_PLACEMENT_3D ( 'NONE', #41625, #18328, #18543 ) ;
#9290 = CARTESIAN_POINT ( 'NONE',  ( -2.121150477449813534E-15, -11.54700538379251284, -47.37499999999996447 ) ) ;
#9291 = CARTESIAN_POINT ( 'NONE',  ( -2.121150477449813534E-15, -11.54700538379251284, -135.8750000000000000 ) ) ;
#9292 = CARTESIAN_POINT ( 'NONE',  ( 9.999999999999996447, -5.773502691896262640, -2.124999999999960476 ) ) ;
#9293 = EDGE_CURVE ( 'NONE', #8991, #38740, #24869, .T. ) ;
#9294 = CARTESIAN_POINT ( 'NONE',  ( -2.293366432827344421E-15, -12.48450537969573659, -69.21875000204838102 ) ) ;
#9295 = CARTESIAN_POINT ( 'NONE',  ( -10.81189881249999907, -6.242252689847864744, -46.96875000204835970 ) ) ;
#9296 = CARTESIAN_POINT ( 'NONE',  ( 4.999999999999992006, -8.660254037844389075, -185.6250000040967905 ) ) ;
#9297 = CARTESIAN_POINT ( 'NONE',  ( 7.644554776091147741E-16, 12.48450537969573659, -26.65625000204837747 ) ) ;
#9298 = CARTESIAN_POINT ( 'NONE',  ( -10.81189881249999729, 6.242252689847871849, -39.71875000204835970 ) ) ;
#9299 = CARTESIAN_POINT ( 'NONE',  ( 10.00000000000076916, -5.773502691895816774, -107.5000000040967620 ) ) ;
#9300 = CARTESIAN_POINT ( 'NONE',  ( 10.81189881249999729, 0.000000000000000000, -136.3437500020484094 ) ) ;
#9301 = EDGE_CURVE ( 'NONE', #13682, #12005, #6843, .T. ) ;
#9302 = CARTESIAN_POINT ( 'NONE',  ( -9.999999999999998224, 1.224646799147353059E-15, -113.7499999999999858 ) ) ;
#9303 = CARTESIAN_POINT ( 'NONE',  ( -9.999999999999998224, 1.224646799147353059E-15, -118.6250000040967905 ) ) ;
#9304 = EDGE_CURVE ( 'NONE', #33047, #29342, #15499, .T. ) ;
#9305 = CARTESIAN_POINT ( 'NONE',  ( 7.070501591499377789E-16, 11.54700538379251284, -69.12500000000000000 ) ) ;
#9306 = CARTESIAN_POINT ( 'NONE',  ( -10.81189881249999729, 1.324075727343319199E-15, -140.2812500020483810 ) ) ;
#9307 = CARTESIAN_POINT ( 'NONE',  ( -5.405949406250003975, -9.363379034771801557, -113.0312500020483952 ) ) ;
#9308 = EDGE_CURVE ( 'NONE', #32599, #21643, #15789, .T. ) ;
#9309 = ORIENTED_EDGE ( 'NONE', *, *, #5844, .T. ) ;
#9310 = CARTESIAN_POINT ( 'NONE',  ( 7.070501591499376803E-16, 11.54700538379251284, -121.6249999999999858 ) ) ;
#9311 = CARTESIAN_POINT ( 'NONE',  ( 7.070501591499377789E-16, 11.54700538379251284, -117.5000000040967905 ) ) ;
#9312 = DIRECTION ( 'NONE',  ( -0.000000000000000000, -0.000000000000000000, 1.000000000000000000 ) ) ;
#9313 = CARTESIAN_POINT ( 'NONE',  ( 10.81189881249999551, -6.242252689847874514, -73.46875000204835260 ) ) ;
#9314 = CARTESIAN_POINT ( 'NONE',  ( -9.999999999999998224, 5.773502691896259087, -41.87499999999997868 ) ) ;
#9315 = CARTESIAN_POINT ( 'NONE',  ( -5.000000000000003553, -8.660254037844383745, -26.87500000409676204 ) ) ;
#9316 = CARTESIAN_POINT ( 'NONE',  ( 5.405949406249999534, 9.363379034771803333, -41.78125000204838102 ) ) ;
#9317 = CARTESIAN_POINT ( 'NONE',  ( -9.999999999999479527, -5.773502691896549521, -142.1249999999999716 ) ) ;
#9318 = CARTESIAN_POINT ( 'NONE',  ( 5.405949406249999534, 9.363379034771803333, -35.78125000204837391 ) ) ;
#9319 = VECTOR ( 'NONE', #21876, 1000.000000000000000 ) ;
#9320 = CARTESIAN_POINT ( 'NONE',  ( -5.000000000000003553, -8.660254037844383745, -139.0000000000000000 ) ) ;
#9321 = CARTESIAN_POINT ( 'NONE',  ( 5.405949406249992428, -9.363379034771808662, -135.2812500020483810 ) ) ;
#9322 = CARTESIAN_POINT ( 'NONE',  ( 5.405949406249999534, 9.363379034771803333, -152.7812500020484094 ) ) ;
#9323 = CARTESIAN_POINT ( 'NONE',  ( 7.070501591499376803E-16, 11.54700538379251284, -60.12499999999998579 ) ) ;
#9324 = EDGE_CURVE ( 'NONE', #3757, #32390, #35932, .T. ) ;
#9325 = CARTESIAN_POINT ( 'NONE',  ( -9.999999999999742428, -5.773502691896402084, -121.1250000000000000 ) ) ;
#9326 = VERTEX_POINT ( 'NONE', #15542 ) ;
#9327 = AXIS2_PLACEMENT_3D ( 'NONE', #1300, #27625, #27192 ) ;
#9328 = EDGE_CURVE ( 'NONE', #17257, #24467, #18284, .T. ) ;
#9329 = ORIENTED_EDGE ( 'NONE', *, *, #40131, .F. ) ;
#9330 = ORIENTED_EDGE ( 'NONE', *, *, #27150, .T. ) ;
#9331 = ADVANCED_FACE ( 'NONE', ( #14691 ), #41012, .F. ) ;
#9332 = CARTESIAN_POINT ( 'NONE',  ( 5.405949406249992428, -9.363379034771808662, -174.0937500020484094 ) ) ;
#9333 = CARTESIAN_POINT ( 'NONE',  ( -10.81189881249999907, -6.242252689847864744, -34.96875000204835260 ) ) ;
#9334 = CARTESIAN_POINT ( 'NONE',  ( 4.999999999999992006, -8.660254037844389075, -128.6250000040967620 ) ) ;
#9335 = CARTESIAN_POINT ( 'NONE',  ( -2.293366432827344421E-15, -12.48450537969573659, -165.2187500020483810 ) ) ;
#9336 = CARTESIAN_POINT ( 'NONE',  ( -5.405949406250003975, -9.363379034771801557, -148.8437500020483810 ) ) ;
#9337 =( BOUNDED_CURVE ( )  B_SPLINE_CURVE ( 2, ( #36964, #24032, #30514, #7407, #37170, #20554, #40194 ),
 .UNSPECIFIED., .F., .F. ) 
 B_SPLINE_CURVE_WITH_KNOTS ( ( 3, 2, 2, 3 ),
 ( 0.6119402985074627876, 0.6131840796019901729, 0.6144278606965176692, 0.6156716417910449435 ),
 .UNSPECIFIED. ) 
 CURVE ( )  GEOMETRIC_REPRESENTATION_ITEM ( )  RATIONAL_B_SPLINE_CURVE ( ( 0.9999999999999880096, 0.8660254037844506980, 1.000000000000000000, 0.8660254037844387076, 1.000000000000000000, 0.8660254037844148378, 1.000000000000023981 ) ) 
 REPRESENTATION_ITEM ( '' )  );
#9338 = LINE ( 'NONE', #15584, #34187 ) ;
#9339 = CARTESIAN_POINT ( 'NONE',  ( -2.293366432827344421E-15, -12.48450537969573659, -136.7187500020483810 ) ) ;
#9340 = AXIS2_PLACEMENT_3D ( 'NONE', #38004, #37132, #7579 ) ;
#9341 = CARTESIAN_POINT ( 'NONE',  ( 10.81189881249999729, 0.000000000000000000, -142.5312500020483810 ) ) ;
#9342 = CARTESIAN_POINT ( 'NONE',  ( -10.81189881249999729, 6.242252689847871849, -17.21875000204836681 ) ) ;
#9343 = CARTESIAN_POINT ( 'NONE',  ( -5.405949406250003975, -9.363379034771801557, -148.8437500020483810 ) ) ;
#9344 = CARTESIAN_POINT ( 'NONE',  ( -9.999999999999998224, 1.224646799147353059E-15, -150.1250000040967905 ) ) ;
#9345 = CARTESIAN_POINT ( 'NONE',  ( 9.999999999999998224, 0.000000000000000000, -44.37500000409677625 ) ) ;
#9346 = CARTESIAN_POINT ( 'NONE',  ( 7.070501591499377789E-16, 11.54700538379251284, -166.6249999999999716 ) ) ;
#9347 = CARTESIAN_POINT ( 'NONE',  ( 10.81189881249999551, -6.242252689847874514, -73.46875000204835260 ) ) ;
#9348 = CARTESIAN_POINT ( 'NONE',  ( 7.644554776091147741E-16, 12.48450537969573659, -52.15625000204838813 ) ) ;
#9349 = CARTESIAN_POINT ( 'NONE',  ( -10.81189881249999729, 1.324075727343319199E-15, -65.09375000204836681 ) ) ;
#9350 = DIRECTION ( 'NONE',  ( -0.000000000000000000, -0.000000000000000000, -1.000000000000000000 ) ) ;
#9351 = CARTESIAN_POINT ( 'NONE',  ( -10.81189881249999907, -6.242252689847864744, -172.9687500020484094 ) ) ;
#9352 = CARTESIAN_POINT ( 'NONE',  ( 4.999999999999992006, -8.660254037844389075, -140.2500000000000000 ) ) ;
#9353 = CARTESIAN_POINT ( 'NONE',  ( 5.405949406249992428, -9.363379034771808662, -150.2812500020483810 ) ) ;
#9354 = CARTESIAN_POINT ( 'NONE',  ( 9.999999999999998224, 0.000000000000000000, -28.99999999999997158 ) ) ;
#9355 = CARTESIAN_POINT ( 'NONE',  ( 7.070501591499377789E-16, 11.54700538379251284, -125.0000000040967763 ) ) ;
#9356 = CARTESIAN_POINT ( 'NONE',  ( 9.999999999999998224, 0.000000000000000000, -93.49999999999998579 ) ) ;
#9357 = EDGE_CURVE ( 'NONE', #37654, #25583, #11643, .T. ) ;
#9358 = ORIENTED_EDGE ( 'NONE', *, *, #1245, .T. ) ;
#9359 = CARTESIAN_POINT ( 'NONE',  ( -5.405949406250003975, -9.363379034771801557, -122.0312500020483952 ) ) ;
#9360 = CARTESIAN_POINT ( 'NONE',  ( 5.000000000000000000, 8.660254037844385522, -143.1250000040967905 ) ) ;
#9361 = EDGE_CURVE ( 'NONE', #36871, #15029, #8918, .T. ) ;
#9362 = CARTESIAN_POINT ( 'NONE',  ( -5.405949406249996869, 9.363379034771805109, -169.0312500020484094 ) ) ;
#9363 = CARTESIAN_POINT ( 'NONE',  ( -5.000000000000003553, -8.660254037844383745, -49.37500000409678336 ) ) ;
#9364 = CYLINDRICAL_SURFACE ( 'NONE', #29730, 9.999999999999998224 ) ;
#9365 = CARTESIAN_POINT ( 'NONE',  ( 10.81189881249999551, -6.242252689847874514, -60.15625000204838813 ) ) ;
#9366 = CARTESIAN_POINT ( 'NONE',  ( 5.000000000000000000, 8.660254037844385522, -73.74999999999998579 ) ) ;
#9367 = CARTESIAN_POINT ( 'NONE',  ( -10.81189881249999907, -6.242252689847864744, -170.1562500020483810 ) ) ;
#9368 = CARTESIAN_POINT ( 'NONE',  ( 10.81189881249999907, 6.242252689847868297, -142.2187500020484094 ) ) ;
#9369 = FACE_OUTER_BOUND ( 'NONE', #42542, .T. ) ;
#9370 = CARTESIAN_POINT ( 'NONE',  ( 9.999999999999479527, 5.773502691896553074, -80.25000000409676204 ) ) ;
#9371 = ORIENTED_EDGE ( 'NONE', *, *, #8772, .F. ) ;
#9372 = DIRECTION ( 'NONE',  ( -0.000000000000000000, -0.000000000000000000, 1.000000000000000000 ) ) ;
#9373 = VECTOR ( 'NONE', #11714, 1000.000000000000000 ) ;
#9374 =( BOUNDED_CURVE ( )  B_SPLINE_CURVE ( 2, ( #41367, #31045, #4488, #17630, #28232, #1263, #11583 ),
 .UNSPECIFIED., .F., .F. ) 
 B_SPLINE_CURVE_WITH_KNOTS ( ( 3, 2, 2, 3 ),
 ( 0.1082089552238805485, 0.1094527363184079616, 0.1106965174129353746, 0.1119402985074627876 ),
 .UNSPECIFIED. ) 
 CURVE ( )  GEOMETRIC_REPRESENTATION_ITEM ( )  RATIONAL_B_SPLINE_CURVE ( ( 1.000000000000004441, 0.8660254037844343777, 1.000000000000000000, 0.8660254037844387076, 1.000000000000000000, 0.8660254037844282715, 1.000000000000010436 ) ) 
 REPRESENTATION_ITEM ( '' )  );
#9375 = EDGE_CURVE ( 'NONE', #8957, #37898, #6691, .T. ) ;
#9377 = ORIENTED_EDGE ( 'NONE', *, *, #11053, .T. ) ;
#9376 = CARTESIAN_POINT ( 'NONE',  ( 5.405949406249992428, -9.363379034771808662, -69.28125000204838102 ) ) ;
#9378 = SHAPE_REPRESENTATION_RELATIONSHIP ( 'NONE' , 'NONE' ,  #10057, #19190 ) ;
#9380 = ORIENTED_EDGE ( 'NONE', *, *, #28564, .T. ) ;
#9379 = CARTESIAN_POINT ( 'NONE',  ( 9.999999999999998224, 0.000000000000000000, -143.0000000000000000 ) ) ;
#9381 = VECTOR ( 'NONE', #39901, 1000.000000000000000 ) ;
#9382 = ORIENTED_EDGE ( 'NONE', *, *, #31803, .T. ) ;
#9383 = CARTESIAN_POINT ( 'NONE',  ( 7.644554776091147741E-16, 12.48450537969573659, -29.46875000204835970 ) ) ;
#9385 = CARTESIAN_POINT ( 'NONE',  ( 9.999999999999479527, 5.773502691896553074, -114.3749999999999716 ) ) ;
#9384 =( BOUNDED_CURVE ( )  B_SPLINE_CURVE ( 2, ( #10079, #27341, #40475, #24117, #33194, #37253, #7069 ),
 .UNSPECIFIED., .F., .F. ) 
 B_SPLINE_CURVE_WITH_KNOTS ( ( 3, 2, 2, 3 ),
 ( 0.9179104477611943480, 0.9191542288557217333, 0.9203980099502490075, 0.9216417910447763928 ),
 .UNSPECIFIED. ) 
 CURVE ( )  GEOMETRIC_REPRESENTATION_ITEM ( )  RATIONAL_B_SPLINE_CURVE ( ( 0.9999999999999641398, 0.8660254037844745678, 1.000000000000000000, 0.8660254037844387076, 1.000000000000000000, 0.8660254037844148378, 1.000000000000023981 ) ) 
 REPRESENTATION_ITEM ( '' )  );
#9386 = CARTESIAN_POINT ( 'NONE',  ( 5.405949406249999534, 9.363379034771803333, -5.781250002048377468 ) ) ;
#9387 = CARTESIAN_POINT ( 'NONE',  ( 10.81189881249999551, -6.242252689847874514, -58.46875000204836681 ) ) ;
#9388 = CARTESIAN_POINT ( 'NONE',  ( -5.000000000000003553, -8.660254037844383745, -109.3750000040967763 ) ) ;
#9389 = CARTESIAN_POINT ( 'NONE',  ( -10.00000000000000000, -5.773502691896251982, -25.12499999999997868 ) ) ;
#9390 = CARTESIAN_POINT ( 'NONE',  ( -5.405949406249996869, 9.363379034771805109, -185.3437500020483810 ) ) ;
#9391 = CARTESIAN_POINT ( 'NONE',  ( 7.644554776091147741E-16, 12.48450537969573659, -167.4687500020483810 ) ) ;
#9392 = CARTESIAN_POINT ( 'NONE',  ( -10.81189881249999907, -6.242252689847864744, -160.9687500020484094 ) ) ;
#9393 = CARTESIAN_POINT ( 'NONE',  ( -5.405949406249996869, 9.363379034771805109, -170.3437500020484094 ) ) ;
#9394 = CARTESIAN_POINT ( 'NONE',  ( 9.999999999999998224, 0.000000000000000000, -200.0000000000000000 ) ) ;
#9395 =( BOUNDED_CURVE ( )  B_SPLINE_CURVE ( 2, ( #31576, #5234, #28332, #41470, #11905, #25100, #38246 ),
 .UNSPECIFIED., .F., .F. ) 
 B_SPLINE_CURVE_WITH_KNOTS ( ( 3, 2, 2, 3 ),
 ( 0.2947761194029852039, 0.2960199004975125336, 0.2972636815920398634, 0.2985074626865671932 ),
 .UNSPECIFIED. ) 
 CURVE ( )  GEOMETRIC_REPRESENTATION_ITEM ( )  RATIONAL_B_SPLINE_CURVE ( ( 0.9999999999999880096, 0.8660254037844506980, 1.000000000000000000, 0.8660254037844387076, 1.000000000000000000, 0.8660254037844327124, 1.000000000000005995 ) ) 
 REPRESENTATION_ITEM ( '' )  );
#9396 = CARTESIAN_POINT ( 'NONE',  ( -9.999999999999998224, 1.224646799147353059E-15, -25.24999999999996803 ) ) ;
#9397 = CARTESIAN_POINT ( 'NONE',  ( 10.00000000000000000, 5.773502691896255534, -190.8750000000000000 ) ) ;
#9398 = CARTESIAN_POINT ( 'NONE',  ( 5.405949406249992428, -9.363379034771808662, -105.0937500020483810 ) ) ;
#9399 = DIRECTION ( 'NONE',  ( 0.000000000000000000, 0.000000000000000000, 1.000000000000000000 ) ) ;
#9400 = CARTESIAN_POINT ( 'NONE',  ( -2.293366432827344421E-15, -12.48450537969573659, -72.40625000204836681 ) ) ;
#9401 = CARTESIAN_POINT ( 'NONE',  ( 5.000000000000000000, 8.660254037844385522, -96.62500000409677625 ) ) ;
#9402 = CARTESIAN_POINT ( 'NONE',  ( -2.293366432827344421E-15, -12.48450537969573659, -87.21875000204838102 ) ) ;
#9403 = VECTOR ( 'NONE', #38328, 1000.000000000000000 ) ;
#9404 = CARTESIAN_POINT ( 'NONE',  ( 7.644554776091147741E-16, 12.48450537969573659, -64.15625000204838102 ) ) ;
#9405 = CARTESIAN_POINT ( 'NONE',  ( 4.999999999999992006, -8.660254037844389075, -143.6250000040967905 ) ) ;
#9406 = CARTESIAN_POINT ( 'NONE',  ( -9.999999999999998224, 5.773502691896259087, -112.3749999999999858 ) ) ;
#9407 = VERTEX_POINT ( 'NONE', #26337 ) ;
#9408 = CARTESIAN_POINT ( 'NONE',  ( -10.81189881249999729, -6.242252689847864744, -144.6562500020484094 ) ) ;
#9409 = CARTESIAN_POINT ( 'NONE',  ( -10.81189881249999907, -6.242252689847864744, -153.6562500020484094 ) ) ;
#9410 = CARTESIAN_POINT ( 'NONE',  ( -2.293366432827344421E-15, -12.48450537969573659, -193.9062500020484094 ) ) ;
#9411 = LINE ( 'NONE', #15653, #41265 ) ;
#9412 = CARTESIAN_POINT ( 'NONE',  ( 5.405949406249992428, -9.363379034771808662, -90.09375000204838102 ) ) ;
#9413 = ORIENTED_EDGE ( 'NONE', *, *, #10491, .T. ) ;
#9414 = CARTESIAN_POINT ( 'NONE',  ( 5.000000000000000000, 8.660254037844385522, -57.24999999999996447 ) ) ;
#9415 = CARTESIAN_POINT ( 'NONE',  ( -5.405949406250003975, -9.363379034771801557, -187.8437500020483810 ) ) ;
#9416 = CARTESIAN_POINT ( 'NONE',  ( -5.000000000000003553, -8.660254037844383745, -77.87500000409677625 ) ) ;
#9417 = CARTESIAN_POINT ( 'NONE',  ( 5.000000000000000000, 8.660254037844385522, -102.2500000000000000 ) ) ;
#9418 = CARTESIAN_POINT ( 'NONE',  ( 5.000000000000000000, 8.660254037844385522, -12.62500000409674783 ) ) ;
#9419 = CARTESIAN_POINT ( 'NONE',  ( 10.81189881249999551, -6.242252689847874514, -87.15625000204838102 ) ) ;
#9420 = CARTESIAN_POINT ( 'NONE',  ( -10.81189881249999729, 1.324075727343319199E-15, -69.78125000204838102 ) ) ;
#9421 = CARTESIAN_POINT ( 'NONE',  ( 9.999999999999996447, -5.773502691896262640, -62.50000000409677625 ) ) ;
#9422 = CARTESIAN_POINT ( 'NONE',  ( 7.644554776091147741E-16, 12.48450537969573659, -17.46875000204836681 ) ) ;
#9423 = DIRECTION ( 'NONE',  ( -0.000000000000000000, -0.000000000000000000, 1.000000000000000000 ) ) ;
#9424 = CARTESIAN_POINT ( 'NONE',  ( -2.293366432827344421E-15, -12.48450537969573659, -195.4062500020484094 ) ) ;
#9425 = EDGE_CURVE ( 'NONE', #12898, #12699, #8084, .T. ) ;
#9426 = CARTESIAN_POINT ( 'NONE',  ( 5.405949406249999534, 9.363379034771803333, -10.28125000204835260 ) ) ;
#9427 = CARTESIAN_POINT ( 'NONE',  ( -2.293366432827344421E-15, -12.48450537969573659, -9.218750002048359704 ) ) ;
#9428 = DIRECTION ( 'NONE',  ( -0.000000000000000000, -0.000000000000000000, 1.000000000000000000 ) ) ;
#9429 = CARTESIAN_POINT ( 'NONE',  ( -9.999999999999998224, 1.224646799147353059E-15, -112.6250000040967763 ) ) ;
#9430 = CYLINDRICAL_SURFACE ( 'NONE', #4544, 9.999999999999998224 ) ;
#9431 = CARTESIAN_POINT ( 'NONE',  ( 9.999999999999996447, -5.773502691896262640, -176.1250000000000000 ) ) ;
#9432 = CARTESIAN_POINT ( 'NONE',  ( 0.000000000000000000, 0.000000000000000000, -200.0000000000000000 ) ) ;
#9434 = ORIENTED_EDGE ( 'NONE', *, *, #1670, .T. ) ;
#9433 = CARTESIAN_POINT ( 'NONE',  ( -10.81189881249999729, 1.324075727343319199E-15, -101.2812500020483952 ) ) ;
#9435 = LINE ( 'NONE', #22600, #33124 ) ;
#9436 = EDGE_LOOP ( 'NONE', ( #6363, #19699, #18010, #5297 ) ) ;
#9437 = EDGE_LOOP ( 'NONE', ( #3905, #15681, #18723, #35615 ) ) ;
#9438 = ADVANCED_FACE ( 'NONE', ( #42296 ), #39279, .T. ) ;
#9439 = CARTESIAN_POINT ( 'NONE',  ( -5.405949406249996869, 9.363379034771805109, -36.84375000204836681 ) ) ;
#9440 = CARTESIAN_POINT ( 'NONE',  ( -10.81189881249999729, 1.324075727343319199E-15, -33.78125000204837391 ) ) ;
#9441 = LOCAL_TIME ( 11, 57, 6.000000000000000000, #36403 ) ;
#9442 = SECURITY_CLASSIFICATION_LEVEL ( 'unclassified' ) ;
#9443 = CARTESIAN_POINT ( 'NONE',  ( -10.81189881249999729, 6.242252689847871849, -83.21875000204838102 ) ) ;
#9444 = CARTESIAN_POINT ( 'NONE',  ( 9.999999999999998224, 0.000000000000000000, -34.99999999999997868 ) ) ;
#9445 = CLOSED_SHELL ( 'NONE', ( #21625, #42060, #16461, #24987, #10367, #10628, #28622, #33494, #17007, #36653, #30049, #38001, #11163, #37755, #1666, #33094, #14950, #17703, #6670, #4067, #21424, #36888, #42276, #33633, #35912, #11701, #18512, #10593, #35026, #10523, #12751, #4942, #21461, #18687, #34137, #28640, #17648, #30291, #34981, #16630, #14054, #8021, #8235, #5903, #11135, #34302, #36614, #34953, #34702, #16710, #28498, #15370, #12110, #19328, #7571, #33815, #40184, #22248, #16413, #29870, #7889, #26496, #15639, #20947, #37585, #10528, #9249, #36249, #24861, #16679, #25577, #12446, #25394, #5071, #25526, #20922, #11438, #22938, #4335, #20102, #36642, #2523, #20900, #3810, #29767, #23122, #36670, #415, #4586, #15674, #26474, #2213, #20778, #28027, #26638, #28140, #2685, #8363, #10902, #32793, #37257, #8018, #39413, #33607, #32168, #9331, #35436, #20768, #20188, #893, #4994, #7152, #36749, #2921, #10544, #5365, #36078, #7274, #27396, #36648, #6464, #27283 ) ) ;
#9446 = CARTESIAN_POINT ( 'NONE',  ( -10.81189881249999729, 1.324075727343319199E-15, -198.5937500020484094 ) ) ;
#9447 = LINE ( 'NONE', #31923, #1238 ) ;
#9448 = CARTESIAN_POINT ( 'NONE',  ( 9.999999999999479527, 5.773502691896553074, -49.87499999999996447 ) ) ;
#9449 = CARTESIAN_POINT ( 'NONE',  ( -5.405949406249996869, 9.363379034771805109, -155.5312500020484094 ) ) ;
#9450 = CARTESIAN_POINT ( 'NONE',  ( -9.999999999999998224, 1.224646799147353059E-15, -9.125000004096744277 ) ) ;
#9451 = CARTESIAN_POINT ( 'NONE',  ( -4.999999999999996447, 8.660254037844387298, -178.5000000000000000 ) ) ;
#9452 = CARTESIAN_POINT ( 'NONE',  ( 5.405949406249992428, -9.363379034771808662, -126.0937500020483668 ) ) ;
#9453 = CARTESIAN_POINT ( 'NONE',  ( 10.81189881249999551, -6.242252689847874514, -96.15625000204838102 ) ) ;
#9454 = CARTESIAN_POINT ( 'NONE',  ( 10.81189881249999551, -6.242252689847874514, -110.9687500020483810 ) ) ;
#9455 = CARTESIAN_POINT ( 'NONE',  ( -10.81189881249999729, 6.242252689847871849, -80.21875000204838102 ) ) ;
#9456 = CARTESIAN_POINT ( 'NONE',  ( -5.405949406249996869, 9.363379034771805109, -88.03125000204838102 ) ) ;
#9457 = CARTESIAN_POINT ( 'NONE',  ( 4.999999999999992006, -8.660254037844389075, -170.6250000040968189 ) ) ;
#9458 = DIRECTION ( 'NONE',  ( 1.000000000000000000, 0.000000000000000000, 0.000000000000000000 ) ) ;
#9459 = CARTESIAN_POINT ( 'NONE',  ( -2.293366432827344421E-15, -12.48450537969573659, -166.9062500020484379 ) ) ;
#9460 = CARTESIAN_POINT ( 'NONE',  ( -10.81189881249999729, 6.242252689847871849, -180.9062500020484094 ) ) ;
#9461 = CARTESIAN_POINT ( 'NONE',  ( 10.00000000000000000, 5.773502691896255534, -156.7500000040967905 ) ) ;
#9462 = CARTESIAN_POINT ( 'NONE',  ( 14.84614977916193190, 1.301042606982605321E-14, 52.14285714285716011 ) ) ;
#9463 = CARTESIAN_POINT ( 'NONE',  ( -10.81189881249999729, 6.242252689847871849, -9.718750002048361480 ) ) ;
#9464 = CARTESIAN_POINT ( 'NONE',  ( -2.293366432827344421E-15, -12.48450537969573659, -112.7187500020483952 ) ) ;
#9465 = CARTESIAN_POINT ( 'NONE',  ( -10.00000000000000000, -5.773502691896251982, -88.12499999999998579 ) ) ;
#9466 = CARTESIAN_POINT ( 'NONE',  ( 7.644554776091147741E-16, 12.48450537969573659, -13.15625000204836859 ) ) ;
#9467 = CARTESIAN_POINT ( 'NONE',  ( 9.999999999999996447, -5.773502691896262640, -95.50000000409677625 ) ) ;
#9468 =( BOUNDED_CURVE ( )  B_SPLINE_CURVE ( 2, ( #20274, #17023, #4094, #40121, #17236, #10552, #23737 ),
 .UNSPECIFIED., .F., .F. ) 
 B_SPLINE_CURVE_WITH_KNOTS ( ( 3, 2, 2, 3 ),
 ( 0.4664179104477613191, 0.4676616915422886489, 0.4689054726368160342, 0.4701492537313434195 ),
 .UNSPECIFIED. ) 
 CURVE ( )  GEOMETRIC_REPRESENTATION_ITEM ( )  RATIONAL_B_SPLINE_CURVE ( ( 0.9999999999999880096, 0.8660254037844506980, 1.000000000000000000, 0.8660254037844387076, 1.000000000000000000, 0.8660254037844267172, 1.000000000000011990 ) ) 
 REPRESENTATION_ITEM ( '' )  );
#9469 = FACE_OUTER_BOUND ( 'NONE', #2299, .T. ) ;
#9470 = CARTESIAN_POINT ( 'NONE',  ( 10.81189881249999907, 6.242252689847868297, -106.4062500020483952 ) ) ;
#9471 = CARTESIAN_POINT ( 'NONE',  ( 10.81189881249999729, 6.242252689847867408, -91.40625000204836681 ) ) ;
#9472 = ORIENTED_EDGE ( 'NONE', *, *, #36192, .T. ) ;
#9473 = EDGE_CURVE ( 'NONE', #41377, #3757, #30148, .T. ) ;
#9474 = CARTESIAN_POINT ( 'NONE',  ( 9.999999999999998224, 0.000000000000000000, -83.37500000409677625 ) ) ;
#9475 = CARTESIAN_POINT ( 'NONE',  ( 9.999999999999998224, 0.000000000000000000, -4.999999999999976907 ) ) ;
#9476 = CARTESIAN_POINT ( 'NONE',  ( 7.644554776091147741E-16, 12.48450537969573659, -45.96875000204836681 ) ) ;
#9477 = ORIENTED_EDGE ( 'NONE', *, *, #39350, .T. ) ;
#9478 = CARTESIAN_POINT ( 'NONE',  ( -9.999999999999998224, 1.224646799147353059E-15, -19.24999999999996092 ) ) ;
#9479 = CARTESIAN_POINT ( 'NONE',  ( -9.999999999999998224, 1.224646799147353059E-15, -154.2500000000000000 ) ) ;
#9480 = CARTESIAN_POINT ( 'NONE',  ( 9.999999999999996447, -5.773502691896262640, -13.00000000409676204 ) ) ;
#9481 = CARTESIAN_POINT ( 'NONE',  ( 0.000000000000000000, 0.000000000000000000, -169.9999999999999716 ) ) ;
#9483 = ORIENTED_EDGE ( 'NONE', *, *, #28564, .F. ) ;
#9482 = CARTESIAN_POINT ( 'NONE',  ( 10.81189881249999729, 0.000000000000000000, -126.0312500020483952 ) ) ;
#9484 = AXIS2_PLACEMENT_3D ( 'NONE', #35580, #8819, #11604 ) ;
#9485 = CARTESIAN_POINT ( 'NONE',  ( 10.00000000000154010, -5.773502691895370020, -21.62499999999993250 ) ) ;
#9486 = EDGE_CURVE ( 'NONE', #7623, #41888, #12711, .T. ) ;
#9487 = ORIENTED_EDGE ( 'NONE', *, *, #40899, .T. ) ;
#9488 = CARTESIAN_POINT ( 'NONE',  ( 10.81189881249999907, 6.242252689847868297, -56.90625000204837391 ) ) ;
#9489 = APPLICATION_PROTOCOL_DEFINITION ( 'international standard', 'config_control_design', 1994, #25362 ) ;
#9490 = CARTESIAN_POINT ( 'NONE',  ( 5.405949406249999534, 9.363379034771803333, -101.5937500020483810 ) ) ;
#9492 = ORIENTED_EDGE ( 'NONE', *, *, #21192, .T. ) ;
#9491 = ORIENTED_EDGE ( 'NONE', *, *, #2858, .T. ) ;
#9493 = CARTESIAN_POINT ( 'NONE',  ( 0.000000000000000000, 0.000000000000000000, -200.0000000000000000 ) ) ;
#9494 = CARTESIAN_POINT ( 'NONE',  ( -9.999999999999998224, 1.224646799147353059E-15, -127.6250000040967620 ) ) ;
#9495 = CARTESIAN_POINT ( 'NONE',  ( 5.405949406249999534, 9.363379034771803333, -179.7812500020484094 ) ) ;
#9496 = CARTESIAN_POINT ( 'NONE',  ( -9.999999999999998224, 1.224646799147353059E-15, -175.2500000000000284 ) ) ;
#9497 = CARTESIAN_POINT ( 'NONE',  ( 9.999999999999998224, 0.000000000000000000, -177.5000000000000000 ) ) ;
#9498 = CARTESIAN_POINT ( 'NONE',  ( -2.293366432827344421E-15, -12.48450537969573659, -129.2187500020483810 ) ) ;
#9499 = CARTESIAN_POINT ( 'NONE',  ( 5.405949406249992428, -9.363379034771808662, -99.09375000204838102 ) ) ;
#9500 = CARTESIAN_POINT ( 'NONE',  ( 10.00000000000051159, -5.773502691895965988, -147.6249999999999716 ) ) ;
#9501 = CARTESIAN_POINT ( 'NONE',  ( 5.405949406249992428, -9.363379034771808662, -109.7812500020483810 ) ) ;
#9502 = CARTESIAN_POINT ( 'NONE',  ( 7.070501591499377789E-16, 11.54700538379251284, -192.5000000040968189 ) ) ;
#9503 = CARTESIAN_POINT ( 'NONE',  ( 5.405949406249992428, -9.363379034771808662, -117.0937500020483810 ) ) ;
#9504 = CARTESIAN_POINT ( 'NONE',  ( -10.81189881249999729, 6.242252689847871849, -188.4062500020484094 ) ) ;
#9505 =( BOUNDED_CURVE ( )  B_SPLINE_CURVE ( 2, ( #28216, #1888, #4904, #14371, #21515, #34482, #31028 ),
 .UNSPECIFIED., .F., .F. ) 
 B_SPLINE_CURVE_WITH_KNOTS ( ( 3, 2, 2, 3 ),
 ( 0.1940298507462686894, 0.1952736318407960470, 0.1965174129353234322, 0.1977611940298507898 ),
 .UNSPECIFIED. ) 
 CURVE ( )  GEOMETRIC_REPRESENTATION_ITEM ( )  RATIONAL_B_SPLINE_CURVE ( ( 0.9999999999999970024, 0.8660254037844417052, 1.000000000000000000, 0.8660254037844387076, 1.000000000000000000, 0.8660254037844327124, 1.000000000000005995 ) ) 
 REPRESENTATION_ITEM ( '' )  );
#9506 = DIRECTION ( 'NONE',  ( -0.000000000000000000, -0.000000000000000000, 1.000000000000000000 ) ) ;
#9507 = CARTESIAN_POINT ( 'NONE',  ( 7.070501591499377789E-16, 11.54700538379251284, -136.6250000000000000 ) ) ;
#9508 = CARTESIAN_POINT ( 'NONE',  ( 5.000000000000000000, 8.660254037844385522, -4.749999999999976907 ) ) ;
#9509 = CARTESIAN_POINT ( 'NONE',  ( 10.81189881249999729, 6.242252689847867408, -70.21875000204839523 ) ) ;
#9510 = CARTESIAN_POINT ( 'NONE',  ( -10.81189881249999907, -6.242252689847864744, -51.46875000204837391 ) ) ;
#9511 = CARTESIAN_POINT ( 'NONE',  ( -5.000000000000003553, -8.660254037844383745, -176.8750000040967905 ) ) ;
#9512 = CARTESIAN_POINT ( 'NONE',  ( -10.81189881249999907, -6.242252689847864744, -24.65625000204838457 ) ) ;
#9513 = AXIS2_PLACEMENT_3D ( 'NONE', #16695, #32704, #26855 ) ;
#9514 = CARTESIAN_POINT ( 'NONE',  ( -10.81189881249999907, -6.242252689847864744, -30.46875000204835260 ) ) ;
#9515 = CARTESIAN_POINT ( 'NONE',  ( 4.999999999999992006, -8.660254037844389075, -8.249999999999952038 ) ) ;
#9516 = CARTESIAN_POINT ( 'NONE',  ( -10.81189881249999729, 6.242252689847871849, -138.7187500020483810 ) ) ;
#9517 = CARTESIAN_POINT ( 'NONE',  ( -10.00000000000000000, -5.773502691896251982, -110.6249999999999858 ) ) ;
#9518 = VECTOR ( 'NONE', #35365, 1000.000000000000000 ) ;
#9519 = CARTESIAN_POINT ( 'NONE',  ( -4.999999999999996447, 8.660254037844387298, -65.99999999999997158 ) ) ;
#9520 = CARTESIAN_POINT ( 'NONE',  ( -10.81189881249999729, 1.324075727343319199E-15, -129.7812500020483810 ) ) ;
#9521 = CARTESIAN_POINT ( 'NONE',  ( -5.405949406250003975, -9.363379034771801557, -116.0312500020483952 ) ) ;
#9522 = ORIENTED_EDGE ( 'NONE', *, *, #7513, .T. ) ;
#9523 = DIRECTION ( 'NONE',  ( -0.000000000000000000, -1.000000000000000000, -0.000000000000000000 ) ) ;
#9524 = CARTESIAN_POINT ( 'NONE',  ( 9.999999999999998224, 0.000000000000000000, -111.8750000040967763 ) ) ;
#9525 = CARTESIAN_POINT ( 'NONE',  ( 9.999999999999998224, 0.000000000000000000, -183.8750000040967905 ) ) ;
#9526 = CARTESIAN_POINT ( 'NONE',  ( -5.405949406249996869, 9.363379034771805109, -66.84375000204836681 ) ) ;
#9527 = EDGE_LOOP ( 'NONE', ( #33700, #9745, #25892, #31406 ) ) ;
#9528 = CARTESIAN_POINT ( 'NONE',  ( 10.00000000000000000, 5.773502691896255534, -42.37499999999997158 ) ) ;
#9529 = CARTESIAN_POINT ( 'NONE',  ( 5.000000000000000000, 8.660254037844385522, -20.12500000409675494 ) ) ;
#9530 = CARTESIAN_POINT ( 'NONE',  ( 10.81189881249999729, 6.242252689847867408, -41.90625000204836681 ) ) ;
#9531 = DIRECTION ( 'NONE',  ( 0.000000000000000000, 0.000000000000000000, 1.000000000000000000 ) ) ;
#9532 = CARTESIAN_POINT ( 'NONE',  ( -4.999999999999996447, 8.660254037844387298, -45.37500000409677625 ) ) ;
#9533 = CARTESIAN_POINT ( 'NONE',  ( 10.81189881249999729, 0.000000000000000000, -37.53125000204838102 ) ) ;
#9534 = CARTESIAN_POINT ( 'NONE',  ( 10.81189881249999907, 6.242252689847868297, -134.9062500020483810 ) ) ;
#9535 = CARTESIAN_POINT ( 'NONE',  ( -10.81189881249999907, -6.242252689847864744, -149.1562500020483810 ) ) ;
#9536 = EDGE_LOOP ( 'NONE', ( #16580, #30089, #2343, #8308 ) ) ;
#9537 = ORIENTED_EDGE ( 'NONE', *, *, #35621, .T. ) ;
#9538 = EDGE_CURVE ( 'NONE', #41318, #21756, #34561, .T. ) ;
#9539 = VERTEX_POINT ( 'NONE', #38862 ) ;
#9540 = ADVANCED_FACE ( 'NONE', ( #28950 ), #6278, .F. ) ;
#9541 = DIRECTION ( 'NONE',  ( -0.000000000000000000, -0.000000000000000000, 1.000000000000000000 ) ) ;
#9542 = CARTESIAN_POINT ( 'NONE',  ( 10.81189881249999729, 0.000000000000000000, -173.8437500020484094 ) ) ;
#9543 = CARTESIAN_POINT ( 'NONE',  ( -5.405949406250003975, -9.363379034771801557, -22.84375000204835615 ) ) ;
#9544 = CARTESIAN_POINT ( 'NONE',  ( -9.999999999999998224, 1.224646799147353059E-15, -126.1250000040967620 ) ) ;
#9545 = CARTESIAN_POINT ( 'NONE',  ( 10.81189881249999551, -6.242252689847874514, -164.9687500020483810 ) ) ;
#9546 = CARTESIAN_POINT ( 'NONE',  ( -2.293366432827344421E-15, -12.48450537969573659, -142.7187500020484094 ) ) ;
#9547 = DIRECTION ( 'NONE',  ( -0.000000000000000000, -0.000000000000000000, 1.000000000000000000 ) ) ;
#9548 = CARTESIAN_POINT ( 'NONE',  ( 5.405949406249999534, 9.363379034771803333, -124.0937500020483952 ) ) ;
#9549 = CARTESIAN_POINT ( 'NONE',  ( -10.81189881249999907, -6.242252689847864744, -129.6562500020483810 ) ) ;
#9550 = CARTESIAN_POINT ( 'NONE',  ( -2.293366432827344421E-15, -12.48450537969573659, -15.21875000204835615 ) ) ;
#9551 = CARTESIAN_POINT ( 'NONE',  ( -10.81189881249999729, 6.242252689847871849, -149.2187500020484379 ) ) ;
#9552 = CARTESIAN_POINT ( 'NONE',  ( 0.000000000000000000, 0.000000000000000000, -200.0000000000000000 ) ) ;
#9553 = CARTESIAN_POINT ( 'NONE',  ( 9.999999999998456346, 5.773502691897149042, -25.87499999999993960 ) ) ;
#9554 = CARTESIAN_POINT ( 'NONE',  ( -2.121150477449813534E-15, -11.54700538379251284, -165.8750000000000000 ) ) ;
#9555 = CARTESIAN_POINT ( 'NONE',  ( -9.999999999999998224, 1.224646799147353059E-15, -70.24999999999998579 ) ) ;
#9556 = CARTESIAN_POINT ( 'NONE',  ( 10.81189881249999729, 0.000000000000000000, -76.34375000204838102 ) ) ;
#9557 = CARTESIAN_POINT ( 'NONE',  ( -10.81189881249999907, -6.242252689847864744, -47.15625000204836681 ) ) ;
#9558 = CARTESIAN_POINT ( 'NONE',  ( 7.644554776091147741E-16, 12.48450537969573659, -50.46875000204836681 ) ) ;
#9559 = CYLINDRICAL_SURFACE ( 'NONE', #2017, 9.999999999999998224 ) ;
#9560 = CARTESIAN_POINT ( 'NONE',  ( 10.81189881249999551, -6.242252689847874514, -160.4687500020484094 ) ) ;
#9561 = CARTESIAN_POINT ( 'NONE',  ( -2.121150477449813534E-15, -11.54700538379251284, -138.8750000000000000 ) ) ;
#9562 = CARTESIAN_POINT ( 'NONE',  ( -10.81189881249999729, -6.242252689847864744, -137.1562500020484094 ) ) ;
#9563 = CARTESIAN_POINT ( 'NONE',  ( 4.999999999999992006, -8.660254037844389075, -23.62500000409675849 ) ) ;
#9564 = CARTESIAN_POINT ( 'NONE',  ( 7.070501591499377789E-16, 11.54700538379251284, -116.0000000040967763 ) ) ;
#9565 = CARTESIAN_POINT ( 'NONE',  ( 7.070501591499377789E-16, 11.54700538379251284, -91.62500000000000000 ) ) ;
#9566 = EDGE_LOOP ( 'NONE', ( #12030, #20591, #32015 ) ) ;
#9567 = CARTESIAN_POINT ( 'NONE',  ( 5.405949406249999534, 9.363379034771803333, -118.2812500020483952 ) ) ;
#9568 = CARTESIAN_POINT ( 'NONE',  ( -5.000000000000003553, -8.660254037844383745, -142.3750000040967905 ) ) ;
#9569 = DIRECTION ( 'NONE',  ( 1.000000000000000000, 0.000000000000000000, 0.000000000000000000 ) ) ;
#9570 = CARTESIAN_POINT ( 'NONE',  ( 5.405949406249992428, -9.363379034771808662, -174.2812500020484094 ) ) ;
#9571 = CARTESIAN_POINT ( 'NONE',  ( -2.121150477449813534E-15, -11.54700538379251284, -49.25000000409676915 ) ) ;
#9572 = CARTESIAN_POINT ( 'NONE',  ( 9.999999999999479527, 5.773502691896553074, -48.75000000409676204 ) ) ;
#9573 = CARTESIAN_POINT ( 'NONE',  ( 10.81189881249999551, -6.242252689847874514, -57.15625000204837391 ) ) ;
#9574 = CARTESIAN_POINT ( 'NONE',  ( 9.999999999999998224, 0.000000000000000000, -101.3750000040967905 ) ) ;
#9575 = CARTESIAN_POINT ( 'NONE',  ( 10.81189881249999551, -6.242252689847874514, -157.6562500020484094 ) ) ;
#9576 = VECTOR ( 'NONE', #27352, 1000.000000000000000 ) ;
#9577 = CARTESIAN_POINT ( 'NONE',  ( 5.405949406249999534, 9.363379034771803333, -146.5937500020483810 ) ) ;
#9578 = CARTESIAN_POINT ( 'NONE',  ( 9.999999999999998224, 0.000000000000000000, -167.3750000040967905 ) ) ;
#9579 = CARTESIAN_POINT ( 'NONE',  ( -9.999999999999998224, 1.224646799147353059E-15, -74.74999999999998579 ) ) ;
#9580 = ORIENTED_EDGE ( 'NONE', *, *, #5930, .F. ) ;
#9581 = CARTESIAN_POINT ( 'NONE',  ( 9.999999999999998224, 0.000000000000000000, -78.49999999999998579 ) ) ;
#9583 = ORIENTED_EDGE ( 'NONE', *, *, #16948, .F. ) ;
#9582 = CARTESIAN_POINT ( 'NONE',  ( -10.81189881249999907, -6.242252689847864744, -71.15625000204839523 ) ) ;
#9584 = EDGE_CURVE ( 'NONE', #24932, #27948, #39067, .T. ) ;
#9586 = EDGE_LOOP ( 'NONE', ( #5144, #34825, #5497, #32629 ) ) ;
#9585 = CARTESIAN_POINT ( 'NONE',  ( 10.81189881249999729, 0.000000000000000000, -121.3437500020483952 ) ) ;
#9587 = ORIENTED_EDGE ( 'NONE', *, *, #9018, .F. ) ;
#9588 = EDGE_CURVE ( 'NONE', #4873, #3545, #41717, .T. ) ;
#9589 = CARTESIAN_POINT ( 'NONE',  ( 10.81189881249999729, 6.242252689847867408, -31.21875000204835260 ) ) ;
#9590 = CARTESIAN_POINT ( 'NONE',  ( -10.81189881249999729, 1.324075727343319199E-15, -194.0937500020484094 ) ) ;
#9592 = ADVANCED_FACE ( 'NONE', ( #26124 ), #22894, .T. ) ;
#9591 = CARTESIAN_POINT ( 'NONE',  ( -5.405949406250003975, -9.363379034771801557, -51.34375000204835260 ) ) ;
#9593 = LINE ( 'NONE', #39787, #30966 ) ;
#9594 = CARTESIAN_POINT ( 'NONE',  ( 7.070501591499377789E-16, 11.54700538379251284, -28.62499999999998224 ) ) ;
#9595 = CARTESIAN_POINT ( 'NONE',  ( -10.81189881249999729, -6.242252689847864744, -189.4687500020484094 ) ) ;
#9596 = CARTESIAN_POINT ( 'NONE',  ( 10.81189881249999551, -6.242252689847874514, -167.9687500020483810 ) ) ;
#9597 = CC_DESIGN_PERSON_AND_ORGANIZATION_ASSIGNMENT ( #19613, #39262, ( #24948 ) ) ;
#9598 = CARTESIAN_POINT ( 'NONE',  ( 5.405949406249992428, -9.363379034771808662, -153.0937500020483810 ) ) ;
#9599 = CARTESIAN_POINT ( 'NONE',  ( -2.293366432827344421E-15, -12.48450537969573659, -171.2187500020483810 ) ) ;
#9600 = CARTESIAN_POINT ( 'NONE',  ( 9.999999999999998224, 0.000000000000000000, -107.3750000040967763 ) ) ;
#9601 = CARTESIAN_POINT ( 'NONE',  ( 7.070501591499376803E-16, 11.54700538379251284, -188.0000000040968189 ) ) ;
#9602 = CARTESIAN_POINT ( 'NONE',  ( 7.070501591499377789E-16, 11.54700538379251284, -187.6250000000000284 ) ) ;
#9603 = VECTOR ( 'NONE', #11321, 1000.000000000000000 ) ;
#9604 = CARTESIAN_POINT ( 'NONE',  ( 5.405949406249999534, 9.363379034771803333, -94.09375000204838102 ) ) ;
#9605 = CARTESIAN_POINT ( 'NONE',  ( 9.999999999999479527, 5.773502691896553074, -108.7500000040967620 ) ) ;
#9606 = CARTESIAN_POINT ( 'NONE',  ( -10.81189881249999907, -6.242252689847864744, -74.15625000204835260 ) ) ;
#9607 = CARTESIAN_POINT ( 'NONE',  ( -9.999999999999998224, 1.224646799147353059E-15, -142.6250000040967905 ) ) ;
#9608 = CARTESIAN_POINT ( 'NONE',  ( -5.405949406250003975, -9.363379034771801557, -187.8437500020483810 ) ) ;
#9609 = CARTESIAN_POINT ( 'NONE',  ( 7.644554776091147741E-16, 12.48450537969573659, -81.96875000204838102 ) ) ;
#9610 = CARTESIAN_POINT ( 'NONE',  ( -10.81189881249999729, 1.324075727343319199E-15, -57.78125000204836681 ) ) ;
#9611 = CARTESIAN_POINT ( 'NONE',  ( 10.00000000000000000, 5.773502691896255534, -135.7500000040967905 ) ) ;
#9612 = CARTESIAN_POINT ( 'NONE',  ( 9.999999999999998224, 0.000000000000000000, -119.0000000000000000 ) ) ;
#9613 = VERTEX_POINT ( 'NONE', #30641 ) ;
#9614 = VECTOR ( 'NONE', #20125, 1000.000000000000000 ) ;
#9615 = CARTESIAN_POINT ( 'NONE',  ( 5.405949406249992428, -9.363379034771808662, -144.2812500020483810 ) ) ;
#9616 = CARTESIAN_POINT ( 'NONE',  ( -10.81189881249999907, -6.242252689847864744, -159.6562500020484094 ) ) ;
#9617 = ADVANCED_FACE ( 'NONE', ( #3678 ), #37319, .T. ) ;
#9618 = CARTESIAN_POINT ( 'NONE',  ( -10.81189881249999907, -6.242252689847864744, -197.1562500020484379 ) ) ;
#9619 = LINE ( 'NONE', #22791, #4070 ) ;
#9620 = CARTESIAN_POINT ( 'NONE',  ( 5.405949406249992428, -9.363379034771808662, -91.59375000204838102 ) ) ;
#9621 = ORIENTED_EDGE ( 'NONE', *, *, #17219, .T. ) ;
#9622 = CARTESIAN_POINT ( 'NONE',  ( 7.070501591499377789E-16, 11.54700538379251284, -60.12499999999997868 ) ) ;
#9623 = CARTESIAN_POINT ( 'NONE',  ( -5.405949406249996869, 9.363379034771805109, -188.3437500020483810 ) ) ;
#9624 = CARTESIAN_POINT ( 'NONE',  ( -10.00000000000000000, -5.773502691896251982, -70.50000000409677625 ) ) ;
#9625 = CARTESIAN_POINT ( 'NONE',  ( 23.09401076758504345, 1.040834085586084257E-14, 49.99999999999998579 ) ) ;
#9626 = CARTESIAN_POINT ( 'NONE',  ( -9.999999999999998224, 1.224646799147353059E-15, -139.6250000040967905 ) ) ;
#9627 = CARTESIAN_POINT ( 'NONE',  ( -10.81189881249999729, 6.242252689847871849, -83.40625000204836681 ) ) ;
#9628 = CARTESIAN_POINT ( 'NONE',  ( -10.81189881249999729, -6.242252689847864744, -65.15625000204838102 ) ) ;
#9629 =( BOUNDED_CURVE ( )  B_SPLINE_CURVE ( 2, ( #24953, #28400, #14984, #21477, #8539, #5295, #20832 ),
 .UNSPECIFIED., .F., .F. ) 
 B_SPLINE_CURVE_WITH_KNOTS ( ( 3, 2, 2, 3 ),
 ( 0.01492537313432837180, 0.01616915422885573453, 0.01741293532338310246, 0.01865671641791046345 ),
 .UNSPECIFIED. ) 
 CURVE ( )  GEOMETRIC_REPRESENTATION_ITEM ( )  RATIONAL_B_SPLINE_CURVE ( ( 0.9999999999999984457, 0.8660254037844402619, 1.000000000000000000, 0.8660254037844387076, 1.000000000000000000, 0.8660254037844368202, 1.000000000000001776 ) ) 
 REPRESENTATION_ITEM ( '' )  );
#9630 = CARTESIAN_POINT ( 'NONE',  ( -9.999999999999998224, 1.224646799147353059E-15, -63.12500000409676204 ) ) ;
#9631 = CARTESIAN_POINT ( 'NONE',  ( 5.405949406249999534, 9.363379034771803333, -20.59375000204835615 ) ) ;
#9632 = CARTESIAN_POINT ( 'NONE',  ( -9.999999999999998224, 1.224646799147353059E-15, -151.6250000040967905 ) ) ;
#9633 = CARTESIAN_POINT ( 'NONE',  ( 5.405949406249999534, 9.363379034771803333, -181.2812500020483810 ) ) ;
#9634 = CARTESIAN_POINT ( 'NONE',  ( -5.405949406250003975, -9.363379034771801557, -9.531250002048352599 ) ) ;
#9635 = CYLINDRICAL_SURFACE ( 'NONE', #7000, 5.000000000000002665 ) ;
#9636 = CYLINDRICAL_SURFACE ( 'NONE', #24889, 9.999999999999998224 ) ;
#9637 = CYLINDRICAL_SURFACE ( 'NONE', #9748, 20.00000000000000355 ) ;
#9638 = DIRECTION ( 'NONE',  ( 0.000000000000000000, 1.000000000000000000, 0.000000000000000000 ) ) ;
#9639 =( BOUNDED_CURVE ( )  B_SPLINE_CURVE ( 2, ( #32707, #9605, #19523, #2932, #22778, #6380, #36148 ),
 .UNSPECIFIED., .F., .F. ) 
 B_SPLINE_CURVE_WITH_KNOTS ( ( 3, 2, 2, 3 ),
 ( 0.4477611940298508730, 0.4490049751243782028, 0.4502487562189055881, 0.4514925373134329734 ),
 .UNSPECIFIED. ) 
 CURVE ( )  GEOMETRIC_REPRESENTATION_ITEM ( )  RATIONAL_B_SPLINE_CURVE ( ( 0.9999999999999880096, 0.8660254037844506980, 1.000000000000000000, 0.8660254037844387076, 1.000000000000000000, 0.8660254037844267172, 1.000000000000011990 ) ) 
 REPRESENTATION_ITEM ( '' )  );
#9640 = CARTESIAN_POINT ( 'NONE',  ( 5.000000000000000000, 8.660254037844385522, -166.7500000000000000 ) ) ;
#9641 = CARTESIAN_POINT ( 'NONE',  ( 9.999999999999998224, 0.000000000000000000, -200.0000000000000000 ) ) ;
#9642 = AXIS2_PLACEMENT_3D ( 'NONE', #17157, #26681, #13283 ) ;
#9644 = EDGE_LOOP ( 'NONE', ( #21891, #30300, #22496, #15785 ) ) ;
#9643 = CARTESIAN_POINT ( 'NONE',  ( 5.405949406249992428, -9.363379034771808662, -93.28125000204838102 ) ) ;
#9645 = CARTESIAN_POINT ( 'NONE',  ( 9.999999999999998224, 0.000000000000000000, -159.8750000040967905 ) ) ;
#9647 = VERTEX_POINT ( 'NONE', #13983 ) ;
#9646 = CARTESIAN_POINT ( 'NONE',  ( -9.999999999999998224, 1.224646799147353059E-15, -154.2500000000000000 ) ) ;
#9648 = EDGE_LOOP ( 'NONE', ( #7148, #1482, #5785, #24717 ) ) ;
#9649 = CARTESIAN_POINT ( 'NONE',  ( -10.81189881249999907, -6.242252689847864744, -34.96875000204835260 ) ) ;
#9650 = CARTESIAN_POINT ( 'NONE',  ( -10.81189881249999729, 1.324075727343319199E-15, -23.28125000204836326 ) ) ;
#9651 = COORDINATED_UNIVERSAL_TIME_OFFSET ( 6, 0, .AHEAD. ) ;
#9652 = CARTESIAN_POINT ( 'NONE',  ( -5.405949406250003975, -9.363379034771801557, -81.34375000204838102 ) ) ;
#9653 = CARTESIAN_POINT ( 'NONE',  ( -2.121150477449813534E-15, -11.54700538379251284, -173.7500000040968189 ) ) ;
#9654 = APPLICATION_CONTEXT ( 'configuration controlled 3d designs of mechanical parts and assemblies' ) ;
#9655 = CARTESIAN_POINT ( 'NONE',  ( -5.405949406249996869, 9.363379034771805109, -191.3437500020484094 ) ) ;
#9656 = DIRECTION ( 'NONE',  ( -0.000000000000000000, -0.000000000000000000, 1.000000000000000000 ) ) ;
#9657 = CARTESIAN_POINT ( 'NONE',  ( 9.999999999999998224, 0.000000000000000000, -173.0000000000000284 ) ) ;
#9658 = CARTESIAN_POINT ( 'NONE',  ( -10.81189881249999729, 1.324075727343319199E-15, -156.7812500020484094 ) ) ;
#9659 = CARTESIAN_POINT ( 'NONE',  ( 5.000000000000000000, 8.660254037844385522, -3.625000004096767814 ) ) ;
#9660 = CARTESIAN_POINT ( 'NONE',  ( 9.999999999999998224, 0.000000000000000000, -102.8750000040967763 ) ) ;
#9661 = EDGE_CURVE ( 'NONE', #1760, #6518, #7838, .T. ) ;
#9662 = CARTESIAN_POINT ( 'NONE',  ( 10.81189881249999907, 6.242252689847868297, -119.7187500020483810 ) ) ;
#9663 = CARTESIAN_POINT ( 'NONE',  ( -5.405949406250003975, -9.363379034771801557, -101.0312500020483952 ) ) ;
#9664 = CARTESIAN_POINT ( 'NONE',  ( -5.405949406250003975, -9.363379034771801557, -105.3437500020483810 ) ) ;
#9665 = CARTESIAN_POINT ( 'NONE',  ( 5.405949406249992428, -9.363379034771808662, -76.59375000204838102 ) ) ;
#9666 = CARTESIAN_POINT ( 'NONE',  ( -2.293366432827344421E-15, -12.48450537969573659, -85.90625000204839523 ) ) ;
#9667 = CARTESIAN_POINT ( 'NONE',  ( -4.999999999999996447, 8.660254037844387298, -169.8750000040967905 ) ) ;
#9668 = DIRECTION ( 'NONE',  ( -0.000000000000000000, -0.000000000000000000, 1.000000000000000000 ) ) ;
#9669 = CARTESIAN_POINT ( 'NONE',  ( -10.81189881249999729, 1.324075727343319199E-15, -170.2812500020484094 ) ) ;
#9670 = CARTESIAN_POINT ( 'NONE',  ( -2.293366432827344421E-15, -12.48450537969573659, -177.4062500020483810 ) ) ;
#9671 = CARTESIAN_POINT ( 'NONE',  ( -9.999999999999998224, 1.224646799147353059E-15, -157.6250000040967905 ) ) ;
#9672 = CYLINDRICAL_SURFACE ( 'NONE', #33939, 9.999999999999998224 ) ;
#9673 = CARTESIAN_POINT ( 'NONE',  ( 5.405949406249999534, 9.363379034771803333, -5.593750002048370362 ) ) ;
#9674 = CARTESIAN_POINT ( 'NONE',  ( -9.999999999999998224, 1.224646799147353059E-15, -60.12500000409676204 ) ) ;
#9675 = CARTESIAN_POINT ( 'NONE',  ( -5.405949406250003975, -9.363379034771801557, -115.8437500020483810 ) ) ;
#9676 = CARTESIAN_POINT ( 'NONE',  ( -2.121150477449813534E-15, -11.54700538379251284, -81.87500000000000000 ) ) ;
#9677 = CARTESIAN_POINT ( 'NONE',  ( 10.81189881249999729, 0.000000000000000000, -15.03125000204835793 ) ) ;
#9678 = CARTESIAN_POINT ( 'NONE',  ( 7.070501591499377789E-16, 11.54700538379251284, -99.50000000409677625 ) ) ;
#9679 = CARTESIAN_POINT ( 'NONE',  ( 9.999999999999998224, 0.000000000000000000, -170.3750000040968189 ) ) ;
#9680 = CARTESIAN_POINT ( 'NONE',  ( -5.405949406250003975, -9.363379034771801557, -110.0312500020483810 ) ) ;
#9681 = CARTESIAN_POINT ( 'NONE',  ( -5.405949406250003975, -9.363379034771801557, -92.03125000204838102 ) ) ;
#9682 = ORIENTED_EDGE ( 'NONE', *, *, #37564, .T. ) ;
#9683 = CARTESIAN_POINT ( 'NONE',  ( -5.000000000000003553, -8.660254037844383745, -86.87500000409677625 ) ) ;
#9684 = CARTESIAN_POINT ( 'NONE',  ( -5.405949406249996869, 9.363379034771805109, -38.34375000204837391 ) ) ;
#9685 = EDGE_LOOP ( 'NONE', ( #34773, #25054, #14933, #23337 ) ) ;
#9686 = CARTESIAN_POINT ( 'NONE',  ( 9.999999999999998224, 0.000000000000000000, -19.99999999999996092 ) ) ;
#9687 = CARTESIAN_POINT ( 'NONE',  ( 7.070501591499377789E-16, 11.54700538379251284, -147.1250000000000000 ) ) ;
#9688 = CARTESIAN_POINT ( 'NONE',  ( -9.999999999999998224, 5.773502691896259087, -9.250000004096760264 ) ) ;
#9689 = CARTESIAN_POINT ( 'NONE',  ( 9.999999999999998224, 0.000000000000000000, -197.0000000000000000 ) ) ;
#9691 = ORIENTED_EDGE ( 'NONE', *, *, #24327, .T. ) ;
#9690 = CARTESIAN_POINT ( 'NONE',  ( 5.405949406249999534, 9.363379034771803333, -118.2812500020483952 ) ) ;
#9692 = CARTESIAN_POINT ( 'NONE',  ( -9.999999999999998224, 1.224646799147353059E-15, -64.62500000409676204 ) ) ;
#9693 = ORIENTED_EDGE ( 'NONE', *, *, #34252, .T. ) ;
#9694 = CARTESIAN_POINT ( 'NONE',  ( 7.644554776091147741E-16, 12.48450537969573659, -52.15625000204838813 ) ) ;
#9695 = APPROVAL_DATE_TIME ( #15732, #19346 ) ;
#9696 = CARTESIAN_POINT ( 'NONE',  ( 5.405949406249992428, -9.363379034771808662, -106.5937500020483810 ) ) ;
#9697 = CARTESIAN_POINT ( 'NONE',  ( -10.81189881249999729, 6.242252689847871849, -122.4062500020483952 ) ) ;
#9698 = ORIENTED_EDGE ( 'NONE', *, *, #11181, .T. ) ;
#9699 = CIRCLE ( 'NONE', #5582, 25.00000000000000000 ) ;
#9700 = CARTESIAN_POINT ( 'NONE',  ( 0.000000000000000000, 0.000000000000000000, -99.99999999999998579 ) ) ;
#9701 = CARTESIAN_POINT ( 'NONE',  ( 7.070501591499376803E-16, 11.54700538379251284, -78.12500000000000000 ) ) ;
#9702 = CARTESIAN_POINT ( 'NONE',  ( -5.405949406250003975, -9.363379034771801557, -182.0312500020483810 ) ) ;
#9703 = CARTESIAN_POINT ( 'NONE',  ( -10.81189881249999729, 1.324075727343319199E-15, -2.093750002048366810 ) ) ;
#9704 = CARTESIAN_POINT ( 'NONE',  ( 7.070501591499376803E-16, 11.54700538379251284, -0.5000000040967461645 ) ) ;
#9705 = CARTESIAN_POINT ( 'NONE',  ( 5.405949406249992428, -9.363379034771808662, -133.5937500020483810 ) ) ;
#9706 =( BOUNDED_CURVE ( )  B_SPLINE_CURVE ( 2, ( #8767, #8976, #21923, #22143, #35317, #5746, #18899 ),
 .UNSPECIFIED., .F., .F. ) 
 B_SPLINE_CURVE_WITH_KNOTS ( ( 3, 2, 2, 3 ),
 ( 0.3358208955223880854, 0.3370646766169154707, 0.3383084577114429670, 0.3395522388059703522 ),
 .UNSPECIFIED. ) 
 CURVE ( )  GEOMETRIC_REPRESENTATION_ITEM ( )  RATIONAL_B_SPLINE_CURVE ( ( 1.000000000000000000, 0.8660254037844387076, 1.000000000000000000, 0.8660254037844387076, 1.000000000000000000, 0.8660254037844148378, 1.000000000000023981 ) ) 
 REPRESENTATION_ITEM ( '' )  );
#9707 = CARTESIAN_POINT ( 'NONE',  ( 5.405949406249999534, 9.363379034771803333, -101.5937500020483810 ) ) ;
#9708 = CARTESIAN_POINT ( 'NONE',  ( -2.293366432827344421E-15, -12.48450537969573659, -105.4062500020483810 ) ) ;
#9709 = CARTESIAN_POINT ( 'NONE',  ( 9.999999999999996447, -5.773502691896262640, -197.5000000040968189 ) ) ;
#9710 = CARTESIAN_POINT ( 'NONE',  ( 7.644554776091147741E-16, 12.48450537969573659, -111.9687500020483668 ) ) ;
#9711 = CARTESIAN_POINT ( 'NONE',  ( 10.81189881249999551, -6.242252689847874514, -186.1562500020484094 ) ) ;
#9712 = CARTESIAN_POINT ( 'NONE',  ( 9.999999999999998224, 0.000000000000000000, -6.875000004096742501 ) ) ;
#9713 = CARTESIAN_POINT ( 'NONE',  ( -5.000000000000003553, -8.660254037844383745, -142.0000000000000000 ) ) ;
#9714 = CARTESIAN_POINT ( 'NONE',  ( 7.070501591499377789E-16, 11.54700538379251284, -4.624999999999963585 ) ) ;
#9715 = CARTESIAN_POINT ( 'NONE',  ( -5.405949406250003975, -9.363379034771801557, -60.34375000204835970 ) ) ;
#9716 = CARTESIAN_POINT ( 'NONE',  ( -10.81189881249999907, -6.242252689847864744, -48.46875000204837391 ) ) ;
#9717 = CARTESIAN_POINT ( 'NONE',  ( -4.999999999999996447, 8.660254037844387298, -180.3750000040967905 ) ) ;
#9718 = CARTESIAN_POINT ( 'NONE',  ( -10.81189881249999729, 1.324075727343319199E-15, -17.28125000204835970 ) ) ;
#9719 = CARTESIAN_POINT ( 'NONE',  ( -2.293366432827344421E-15, -12.48450537969573659, -33.21875000204835260 ) ) ;
#9720 = CARTESIAN_POINT ( 'NONE',  ( 9.999999999999998224, 0.000000000000000000, -27.87500000409676204 ) ) ;
#9721 = CARTESIAN_POINT ( 'NONE',  ( 10.81189881249999551, -6.242252689847874514, -139.4687500020483810 ) ) ;
#9722 = CARTESIAN_POINT ( 'NONE',  ( -4.999999999999996447, 8.660254037844387298, -102.0000000000000000 ) ) ;
#9723 = CARTESIAN_POINT ( 'NONE',  ( -9.999999999998456346, -5.773502691897145489, -28.12499999999995026 ) ) ;
#9724 = CARTESIAN_POINT ( 'NONE',  ( -2.121150477449813534E-15, -11.54700538379251284, -71.37500000000000000 ) ) ;
#9725 = CARTESIAN_POINT ( 'NONE',  ( 5.405949406249992428, -9.363379034771808662, -135.2812500020483810 ) ) ;
#9726 = CARTESIAN_POINT ( 'NONE',  ( 5.405949406249992428, -9.363379034771808662, -114.2812500020483952 ) ) ;
#9727 = EDGE_CURVE ( 'NONE', #31328, #15306, #31806, .T. ) ;
#9728 = ORIENTED_EDGE ( 'NONE', *, *, #16959, .F. ) ;
#9729 = AXIS2_PLACEMENT_3D ( 'NONE', #8740, #31199, #27952 ) ;
#9730 = DIRECTION ( 'NONE',  ( 1.000000000000000000, 0.000000000000000000, 0.000000000000000000 ) ) ;
#9731 = CARTESIAN_POINT ( 'NONE',  ( 7.070501591499377789E-16, 11.54700538379251284, -108.5000000040967763 ) ) ;
#9732 = CARTESIAN_POINT ( 'NONE',  ( -4.999999999999996447, 8.660254037844387298, -162.0000000000000000 ) ) ;
#9733 = CARTESIAN_POINT ( 'NONE',  ( 10.81189881249999729, 0.000000000000000000, -65.84375000204836681 ) ) ;
#9734 = ORIENTED_EDGE ( 'NONE', *, *, #14872, .T. ) ;
#9735 = CARTESIAN_POINT ( 'NONE',  ( 4.999999999999992006, -8.660254037844389075, -39.74999999999997868 ) ) ;
#9736 = APPROVAL_PERSON_ORGANIZATION ( #14830, #40954, #11177 ) ;
#9737 = CARTESIAN_POINT ( 'NONE',  ( -10.00000000000000000, -5.773502691896251982, -19.50000000409677270 ) ) ;
#9738 = CARTESIAN_POINT ( 'NONE',  ( -5.405949406249996869, 9.363379034771805109, -43.03125000204838102 ) ) ;
#9739 = CARTESIAN_POINT ( 'NONE',  ( -10.00000000000102496, 5.773502691895664007, -16.37499999999995381 ) ) ;
#9740 = CARTESIAN_POINT ( 'NONE',  ( 10.00000000000000000, 5.773502691896255534, -33.75000000409675494 ) ) ;
#9741 = CYLINDRICAL_SURFACE ( 'NONE', #36240, 9.999999999999998224 ) ;
#9742 = CARTESIAN_POINT ( 'NONE',  ( -10.81189881249999729, 6.242252689847871849, -134.4062500020484094 ) ) ;
#9743 = CARTESIAN_POINT ( 'NONE',  ( -10.81189881249999729, 6.242252689847871849, -146.4062500020484094 ) ) ;
#9744 = CARTESIAN_POINT ( 'NONE',  ( -1.040834085586084257E-14, 145.0000000000000000, 22.49999999999999289 ) ) ;
#9745 = ORIENTED_EDGE ( 'NONE', *, *, #14315, .T. ) ;
#9746 = ORIENTED_EDGE ( 'NONE', *, *, #36492, .T. ) ;
#9747 = ORIENTED_EDGE ( 'NONE', *, *, #23044, .T. ) ;
#9748 = AXIS2_PLACEMENT_3D ( 'NONE', #35973, #19551, #3599 ) ;
#9749 = DIRECTION ( 'NONE',  ( -0.000000000000000000, -0.000000000000000000, -1.000000000000000000 ) ) ;
#9750 =( BOUNDED_CURVE ( )  B_SPLINE_CURVE ( 2, ( #32078, #2928, #5745, #16057, #2306, #38115, #21709 ),
 .UNSPECIFIED., .F., .F. ) 
 B_SPLINE_CURVE_WITH_KNOTS ( ( 3, 2, 2, 3 ),
 ( 0.6156716417910449435, 0.6169154228855723288, 0.6181592039800996030, 0.6194029850746269883 ),
 .UNSPECIFIED. ) 
 CURVE ( )  GEOMETRIC_REPRESENTATION_ITEM ( )  RATIONAL_B_SPLINE_CURVE ( ( 0.9999999999999761302, 0.8660254037844625774, 1.000000000000000000, 0.8660254037844387076, 1.000000000000000000, 0.8660254037844267172, 1.000000000000011990 ) ) 
 REPRESENTATION_ITEM ( '' )  );
#9751 = CARTESIAN_POINT ( 'NONE',  ( -10.81189881249999729, 6.242252689847871849, -174.7187500020483810 ) ) ;
#9752 = APPROVAL_PERSON_ORGANIZATION ( #40105, #7210, #33655 ) ;
#9753 = CARTESIAN_POINT ( 'NONE',  ( -5.405949406250003975, -9.363379034771801557, -25.84375000204835970 ) ) ;
#9754 = CARTESIAN_POINT ( 'NONE',  ( 4.999999999999992006, -8.660254037844389075, -61.12500000409676204 ) ) ;
#9755 = CARTESIAN_POINT ( 'NONE',  ( -2.293366432827344421E-15, -12.48450537969573659, -159.2187500020483526 ) ) ;
#9756 = CARTESIAN_POINT ( 'NONE',  ( 5.405949406249999534, 9.363379034771803333, -143.5937500020483810 ) ) ;
#9757 = CARTESIAN_POINT ( 'NONE',  ( -9.999999999998456346, -5.773502691897145489, -9.000000004096717632 ) ) ;
#9758 = CARTESIAN_POINT ( 'NONE',  ( 5.405949406249999534, 9.363379034771803333, -125.5937500020483668 ) ) ;
#9759 = CARTESIAN_POINT ( 'NONE',  ( 5.405949406249999534, 9.363379034771803333, -131.7812500020483810 ) ) ;
#9760 = CARTESIAN_POINT ( 'NONE',  ( -10.81189881249999729, 6.242252689847871849, -18.71875000204837391 ) ) ;
#9761 = CARTESIAN_POINT ( 'NONE',  ( 10.81189881249999729, 6.242252689847867408, -134.7187500020483810 ) ) ;
#9762 = FACE_OUTER_BOUND ( 'NONE', #1107, .T. ) ;
#9763 = CARTESIAN_POINT ( 'NONE',  ( 5.000000000000000000, 8.660254037844385522, -44.12500000409677625 ) ) ;
#9764 = CARTESIAN_POINT ( 'NONE',  ( 7.070501591499377789E-16, 11.54700538379251284, -162.1250000000000284 ) ) ;
#9765 = CARTESIAN_POINT ( 'NONE',  ( 7.644554776091147741E-16, 12.48450537969573659, -1.156250002048359038 ) ) ;
#9766 = VECTOR ( 'NONE', #28351, 1000.000000000000000 ) ;
#9767 = CARTESIAN_POINT ( 'NONE',  ( -10.81189881249999907, -6.242252689847864744, -70.96875000204840944 ) ) ;
#9768 = CARTESIAN_POINT ( 'NONE',  ( -5.405949406249996869, 9.363379034771805109, -38.53125000204838102 ) ) ;
#9769 = CARTESIAN_POINT ( 'NONE',  ( 7.644554776091147741E-16, 12.48450537969573659, -53.46875000204836681 ) ) ;
#9770 = CARTESIAN_POINT ( 'NONE',  ( 7.070501591499376803E-16, 11.54700538379251284, -90.50000000409677625 ) ) ;
#9771 = CARTESIAN_POINT ( 'NONE',  ( -5.405949406249996869, 9.363379034771805109, -158.3437500020483810 ) ) ;
#9772 = CARTESIAN_POINT ( 'NONE',  ( 7.070501591499377789E-16, 11.54700538379251284, -136.6250000000000000 ) ) ;
#9773 = CARTESIAN_POINT ( 'NONE',  ( 5.405949406249992428, -9.363379034771808662, -141.2812500020483810 ) ) ;
#9774 = CARTESIAN_POINT ( 'NONE',  ( 0.000000000000000000, 0.000000000000000000, -200.0000000000000000 ) ) ;
#9775 = CARTESIAN_POINT ( 'NONE',  ( 5.000000000000000000, 8.660254037844385522, -113.1250000040967763 ) ) ;
#9776 = CARTESIAN_POINT ( 'NONE',  ( -5.000000000000003553, -8.660254037844383745, -87.99999999999998579 ) ) ;
#9777 = ORIENTED_EDGE ( 'NONE', *, *, #11801, .T. ) ;
#9778 = CARTESIAN_POINT ( 'NONE',  ( 5.405949406249992428, -9.363379034771808662, -117.2812500020483952 ) ) ;
#9779 = CARTESIAN_POINT ( 'NONE',  ( -10.00000000000000000, -5.773502691896251982, -133.5000000040967905 ) ) ;
#9780 = CARTESIAN_POINT ( 'NONE',  ( -9.999999999999479527, -5.773502691896549521, -141.0000000040967620 ) ) ;
#9781 = CARTESIAN_POINT ( 'NONE',  ( -10.81189881249999729, 1.324075727343319199E-15, -173.2812500020484094 ) ) ;
#9782 = CARTESIAN_POINT ( 'NONE',  ( 9.999999999999998224, 0.000000000000000000, -42.87500000409677625 ) ) ;
#9783 = EDGE_CURVE ( 'NONE', #1402, #32484, #17657, .T. ) ;
#9784 = DIRECTION ( 'NONE',  ( 1.000000000000000000, 0.000000000000000000, 0.000000000000000000 ) ) ;
#9785 = CARTESIAN_POINT ( 'NONE',  ( -10.81189881249999907, -6.242252689847864744, -57.65625000204838102 ) ) ;
#9786 = AXIS2_PLACEMENT_3D ( 'NONE', #40377, #24012, #1347 ) ;
#9787 = CARTESIAN_POINT ( 'NONE',  ( 9.999999999999479527, 5.773502691896553074, -101.2500000040967763 ) ) ;
#9788 = CARTESIAN_POINT ( 'NONE',  ( 10.81189881249999907, 6.242252689847868297, -160.4062500020484094 ) ) ;
#9789 = CARTESIAN_POINT ( 'NONE',  ( -10.81189881249999907, -6.242252689847864744, -145.9687500020484094 ) ) ;
#9790 = CYLINDRICAL_SURFACE ( 'NONE', #15982, 9.999999999999998224 ) ;
#9791 = CARTESIAN_POINT ( 'NONE',  ( 7.070501591499376803E-16, 11.54700538379251284, -174.1250000000000000 ) ) ;
#9792 = ORIENTED_EDGE ( 'NONE', *, *, #17580, .F. ) ;
#9793 = CARTESIAN_POINT ( 'NONE',  ( 9.999999999999998224, 0.000000000000000000, -189.8750000040967905 ) ) ;
#9794 = CIRCLE ( 'NONE', #20826, 20.00000000000000355 ) ;
#9796 = ORIENTED_EDGE ( 'NONE', *, *, #39140, .F. ) ;
#9795 = CARTESIAN_POINT ( 'NONE',  ( 10.81189881249999729, 0.000000000000000000, -69.03125000204838102 ) ) ;
#9798 = ORIENTED_EDGE ( 'NONE', *, *, #15572, .T. ) ;
#9797 = CARTESIAN_POINT ( 'NONE',  ( -10.81189881249999729, 1.324075727343319199E-15, -117.5937500020483810 ) ) ;
#9799 = ORIENTED_EDGE ( 'NONE', *, *, #23824, .F. ) ;
#9800 = CARTESIAN_POINT ( 'NONE',  ( -5.405949406250003975, -9.363379034771801557, -21.34375000204835615 ) ) ;
#9801 = CARTESIAN_POINT ( 'NONE',  ( 7.644554776091147741E-16, 12.48450537969573659, -198.9687500020484094 ) ) ;
#9802 = CARTESIAN_POINT ( 'NONE',  ( 10.81189881249999907, 6.242252689847868297, -47.71875000204835970 ) ) ;
#9803 = CARTESIAN_POINT ( 'NONE',  ( -9.999999999999998224, 1.224646799147353059E-15, -72.12500000409677625 ) ) ;
#9804 = CARTESIAN_POINT ( 'NONE',  ( -9.999999999999998224, 1.224646799147353059E-15, -29.74999999999997158 ) ) ;
#9805 = CARTESIAN_POINT ( 'NONE',  ( 5.405949406249999534, 9.363379034771803333, -181.0937500020483810 ) ) ;
#9806 = CARTESIAN_POINT ( 'NONE',  ( -5.405949406249996869, 9.363379034771805109, -171.8437500020484094 ) ) ;
#9807 = CARTESIAN_POINT ( 'NONE',  ( -10.81189881249999729, 1.324075727343319199E-15, -150.5937500020483810 ) ) ;
#9808 = VECTOR ( 'NONE', #7453, 1000.000000000000000 ) ;
#9809 = CARTESIAN_POINT ( 'NONE',  ( -5.405949406249996869, 9.363379034771805109, -161.3437500020484094 ) ) ;
#9810 = CARTESIAN_POINT ( 'NONE',  ( -5.000000000000003553, -8.660254037844383745, -161.8750000040967905 ) ) ;
#9811 = CARTESIAN_POINT ( 'NONE',  ( 5.000000000000000000, 8.660254037844385522, -184.7500000000000000 ) ) ;
#9812 = CARTESIAN_POINT ( 'NONE',  ( 10.81189881249999907, 6.242252689847868297, -94.21875000204838102 ) ) ;
#9813 = CARTESIAN_POINT ( 'NONE',  ( 9.999999999999998224, 0.000000000000000000, -200.0000000000000000 ) ) ;
#9814 = CARTESIAN_POINT ( 'NONE',  ( 5.405949406249992428, -9.363379034771808662, -73.78125000204838102 ) ) ;
#9815 = CARTESIAN_POINT ( 'NONE',  ( 10.81189881249999729, 0.000000000000000000, -185.8437500020483810 ) ) ;
#9816 = CARTESIAN_POINT ( 'NONE',  ( 10.81189881249999729, 6.242252689847867408, -163.4062500020483810 ) ) ;
#9817 = CARTESIAN_POINT ( 'NONE',  ( 5.405949406249992428, -9.363379034771808662, -63.28125000204837391 ) ) ;
#9818 = CARTESIAN_POINT ( 'NONE',  ( 9.999999999999996447, -5.773502691896262640, -142.0000000040967905 ) ) ;
#9819 = CARTESIAN_POINT ( 'NONE',  ( -5.000000000000003553, -8.660254037844383745, -118.0000000000000000 ) ) ;
#9820 = ORIENTED_EDGE ( 'NONE', *, *, #385, .F. ) ;
#9821 = CARTESIAN_POINT ( 'NONE',  ( 5.405949406249992428, -9.363379034771808662, -145.7812500020483810 ) ) ;
#9822 = CARTESIAN_POINT ( 'NONE',  ( -2.293366432827344421E-15, -12.48450537969573659, -154.9062500020483810 ) ) ;
#9823 = VECTOR ( 'NONE', #25142, 1000.000000000000000 ) ;
#9824 = DIRECTION ( 'NONE',  ( -0.000000000000000000, -0.000000000000000000, 1.000000000000000000 ) ) ;
#9825 = CARTESIAN_POINT ( 'NONE',  ( 10.81189881249999907, 6.242252689847868297, -88.21875000204838102 ) ) ;
#9826 = VERTEX_POINT ( 'NONE', #23529 ) ;
#9827 = CARTESIAN_POINT ( 'NONE',  ( -2.121150477449813534E-15, -11.54700538379251284, -57.87499999999998579 ) ) ;
#9828 = CARTESIAN_POINT ( 'NONE',  ( 10.81189881249999729, 0.000000000000000000, -185.8437500020483810 ) ) ;
#9829 = CARTESIAN_POINT ( 'NONE',  ( 5.000000000000000000, 8.660254037844385522, -62.12500000409676204 ) ) ;
#9830 = EDGE_CURVE ( 'NONE', #21964, #414, #5058, .T. ) ;
#9831 = EDGE_CURVE ( 'NONE', #35094, #6, #40752, .T. ) ;
#9832 = CARTESIAN_POINT ( 'NONE',  ( -9.999999999999998224, 1.224646799147353059E-15, -118.6250000040967905 ) ) ;
#9833 = CARTESIAN_POINT ( 'NONE',  ( 4.999999999999992006, -8.660254037844389075, -144.7500000000000000 ) ) ;
#9834 = EDGE_CURVE ( 'NONE', #8492, #5685, #20607, .T. ) ;
#9835 = CARTESIAN_POINT ( 'NONE',  ( 10.81189881249999551, -6.242252689847874514, -84.15625000204838102 ) ) ;
#9836 = CARTESIAN_POINT ( 'NONE',  ( 5.405949406249999534, 9.363379034771803333, -68.78125000204838102 ) ) ;
#9837 = EDGE_CURVE ( 'NONE', #35669, #36871, #20483, .T. ) ;
#9838 = CARTESIAN_POINT ( 'NONE',  ( -2.121150477449813534E-15, -11.54700538379251284, -62.75000000409677625 ) ) ;
#9839 = CARTESIAN_POINT ( 'NONE',  ( 10.81189881249999551, -6.242252689847874514, -16.46875000204836681 ) ) ;
#9840 = CARTESIAN_POINT ( 'NONE',  ( -10.00000000000051337, 5.773502691895962435, -37.75000000409675494 ) ) ;
#9841 = CARTESIAN_POINT ( 'NONE',  ( 5.405949406249999534, 9.363379034771803333, -188.7812500020484094 ) ) ;
#9842 = CARTESIAN_POINT ( 'NONE',  ( -5.405949406249996869, 9.363379034771805109, -10.03125000204835260 ) ) ;
#9843 = CARTESIAN_POINT ( 'NONE',  ( -10.81189881249999729, 6.242252689847871849, -0.7187500020483512664 ) ) ;
#9844 = CARTESIAN_POINT ( 'NONE',  ( -9.999999999999998224, 1.224646799147353059E-15, -118.2500000000000000 ) ) ;
#9845 = CARTESIAN_POINT ( 'NONE',  ( -5.000000000000003553, -8.660254037844383745, -45.99999999999998579 ) ) ;
#9846 = APPROVAL ( #40943, 'UNSPECIFIED' ) ;
#9847 = CARTESIAN_POINT ( 'NONE',  ( -9.999999999999998224, 1.836970198721029589E-15, 0.000000000000000000 ) ) ;
#9848 = CARTESIAN_POINT ( 'NONE',  ( -4.999999999999996447, 8.660254037844387298, -166.5000000000000000 ) ) ;
#9849 = CARTESIAN_POINT ( 'NONE',  ( -5.000000000000003553, -8.660254037844383745, -36.99999999999997868 ) ) ;
#9851 = VERTEX_POINT ( 'NONE', #33251 ) ;
#9850 = CARTESIAN_POINT ( 'NONE',  ( 5.405949406249992428, -9.363379034771808662, -94.78125000204838102 ) ) ;
#9852 = DIRECTION ( 'NONE',  ( 1.000000000000000000, 0.000000000000000000, 0.000000000000000000 ) ) ;
#9853 = EDGE_CURVE ( 'NONE', #4202, #35880, #9468, .T. ) ;
#9855 = ORIENTED_EDGE ( 'NONE', *, *, #13702, .F. ) ;
#9854 = CARTESIAN_POINT ( 'NONE',  ( -5.405949406249996869, 9.363379034771805109, -101.3437500020483810 ) ) ;
#9856 = ORIENTED_EDGE ( 'NONE', *, *, #38885, .T. ) ;
#9857 = CARTESIAN_POINT ( 'NONE',  ( -2.293366432827344421E-15, -12.48450537969573659, -33.21875000204834549 ) ) ;
#9858 = CARTESIAN_POINT ( 'NONE',  ( -10.81189881249999729, 1.324075727343319199E-15, -24.78125000204836681 ) ) ;
#9859 = DATE_TIME_ROLE ( 'classification_date' ) ;
#9860 = EDGE_CURVE ( 'NONE', #29087, #29783, #19915, .T. ) ;
#9861 = CARTESIAN_POINT ( 'NONE',  ( 10.81189881249999907, 6.242252689847868297, -73.21875000204836681 ) ) ;
#9862 = LINE ( 'NONE', #3821, #5683 ) ;
#9863 = EDGE_CURVE ( 'NONE', #8912, #28824, #31543, .T. ) ;
#9864 = CARTESIAN_POINT ( 'NONE',  ( 10.81189881249999729, 0.000000000000000000, -190.3437500020484094 ) ) ;
#9865 = DIRECTION ( 'NONE',  ( -0.000000000000000000, -0.000000000000000000, -1.000000000000000000 ) ) ;
#9866 = CARTESIAN_POINT ( 'NONE',  ( -2.293366432827344421E-15, -12.48450537969573659, -154.9062500020483810 ) ) ;
#9867 = CARTESIAN_POINT ( 'NONE',  ( -4.999999999999996447, 8.660254037844387298, -6.375000004096770034 ) ) ;
#9868 = FACE_OUTER_BOUND ( 'NONE', #26266, .T. ) ;
#9869 = CARTESIAN_POINT ( 'NONE',  ( -5.405949406249996869, 9.363379034771805109, -120.8437500020483952 ) ) ;
#9870 = CARTESIAN_POINT ( 'NONE',  ( -10.81189881249999729, 6.242252689847871849, -98.40625000204838102 ) ) ;
#9871 = CARTESIAN_POINT ( 'NONE',  ( 10.81189881249999551, -6.242252689847874514, -109.4687500020483952 ) ) ;
#9872 = EDGE_CURVE ( 'NONE', #15363, #18023, #40316, .T. ) ;
#9873 = CARTESIAN_POINT ( 'NONE',  ( 10.81189881249999907, 6.242252689847868297, -74.71875000204838102 ) ) ;
#9874 = CARTESIAN_POINT ( 'NONE',  ( -10.81189881249999907, -6.242252689847864744, -84.65625000204836681 ) ) ;
#9875 = CARTESIAN_POINT ( 'NONE',  ( -10.00000000000000000, -5.773502691896251982, -165.0000000040967905 ) ) ;
#9876 =( BOUNDED_CURVE ( )  B_SPLINE_CURVE ( 2, ( #25369, #15412, #28608, #35297, #38734, #5727, #18880 ),
 .UNSPECIFIED., .F., .F. ) 
 B_SPLINE_CURVE_WITH_KNOTS ( ( 3, 2, 2, 3 ),
 ( 0.8582089552238808539, 0.8594527363184081281, 0.8606965174129356244, 0.8619402985074630097 ),
 .UNSPECIFIED. ) 
 CURVE ( )  GEOMETRIC_REPRESENTATION_ITEM ( )  RATIONAL_B_SPLINE_CURVE ( ( 0.9999999999999761302, 0.8660254037844625774, 1.000000000000000000, 0.8660254037844387076, 1.000000000000000000, 0.8660254037844028474, 1.000000000000035971 ) ) 
 REPRESENTATION_ITEM ( '' )  );
#9877 = CARTESIAN_POINT ( 'NONE',  ( -9.999999999999998224, 1.224646799147353059E-15, -67.24999999999997158 ) ) ;
#9878 = CARTESIAN_POINT ( 'NONE',  ( -5.405949406249996869, 9.363379034771805109, -169.0312500020484094 ) ) ;
#9879 = CARTESIAN_POINT ( 'NONE',  ( 10.81189881249999907, 6.242252689847868297, -179.9062500020484094 ) ) ;
#9880 = CARTESIAN_POINT ( 'NONE',  ( 7.070501591499377789E-16, 11.54700538379251284, -156.5000000040968189 ) ) ;
#9881 = CARTESIAN_POINT ( 'NONE',  ( -9.999999999999998224, 0.000000000000000000, -99.99999999999998579 ) ) ;
#9882 = CARTESIAN_POINT ( 'NONE',  ( 5.405949406249992428, -9.363379034771808662, -3.093750002048367698 ) ) ;
#9883 = CARTESIAN_POINT ( 'NONE',  ( 10.00000000000154010, -5.773502691895370020, -53.50000000409673362 ) ) ;
#9884 = CARTESIAN_POINT ( 'NONE',  ( 5.405949406249999534, 9.363379034771803333, -116.5937500020483810 ) ) ;
#9885 = CARTESIAN_POINT ( 'NONE',  ( 9.999999999999998224, 0.000000000000000000, -78.49999999999998579 ) ) ;
#9886 = CARTESIAN_POINT ( 'NONE',  ( 10.81189881249999907, 6.242252689847868297, -10.40625000204836859 ) ) ;
#9887 = CARTESIAN_POINT ( 'NONE',  ( 9.999999999999996447, -5.773502691896262640, -98.50000000409677625 ) ) ;
#9888 = CARTESIAN_POINT ( 'NONE',  ( -10.00000000000000000, -5.773502691896252870, -171.0000000040967905 ) ) ;
#9889 = CARTESIAN_POINT ( 'NONE',  ( 5.405949406249992428, -9.363379034771808662, -106.7812500020483810 ) ) ;
#9890 = CARTESIAN_POINT ( 'NONE',  ( -2.293366432827344421E-15, -12.48450537969573659, -88.90625000204838102 ) ) ;
#9891 = ORIENTED_EDGE ( 'NONE', *, *, #30774, .T. ) ;
#9892 = CARTESIAN_POINT ( 'NONE',  ( -2.121150477449813534E-15, -11.54700538379251284, -86.75000000409677625 ) ) ;
#9893 = CARTESIAN_POINT ( 'NONE',  ( -9.999999999999998224, 1.224646799147353059E-15, -73.62500000409677625 ) ) ;
#9894 = CARTESIAN_POINT ( 'NONE',  ( 10.81189881249999907, 6.242252689847868297, -44.71875000204835970 ) ) ;
#9895 = VERTEX_POINT ( 'NONE', #38175 ) ;
#9896 = CARTESIAN_POINT ( 'NONE',  ( -10.00000000000000000, -5.773502691896251982, -7.124999999999969802 ) ) ;
#9897 = CARTESIAN_POINT ( 'NONE',  ( 9.999999999999996447, -5.773502691896262640, -149.1250000000000000 ) ) ;
#9898 = CARTESIAN_POINT ( 'NONE',  ( 5.000000000000000000, 8.660254037844385522, -139.7499999999999716 ) ) ;
#9899 = CARTESIAN_POINT ( 'NONE',  ( -9.999999999999998224, 1.224646799147353059E-15, -12.12500000409674783 ) ) ;
#9900 = CARTESIAN_POINT ( 'NONE',  ( -5.000000000000003553, -8.660254037844383745, -193.0000000000000000 ) ) ;
#9902 = VERTEX_POINT ( 'NONE', #21123 ) ;
#9901 = CARTESIAN_POINT ( 'NONE',  ( 5.405949406249992428, -9.363379034771808662, -121.7812500020483952 ) ) ;
#9903 = CYLINDRICAL_SURFACE ( 'NONE', #16548, 9.999999999999998224 ) ;
#9904 = ORIENTED_EDGE ( 'NONE', *, *, #4319, .T. ) ;
#9905 = CARTESIAN_POINT ( 'NONE',  ( 10.81189881249999729, 0.000000000000000000, -42.03125000204838102 ) ) ;
#9906 = APPROVAL_STATUS ( 'not_yet_approved' ) ;
#9907 = CARTESIAN_POINT ( 'NONE',  ( -10.81189881249999729, 6.242252689847871849, -107.2187500020483810 ) ) ;
#9908 = CARTESIAN_POINT ( 'NONE',  ( -5.405949406249996869, 9.363379034771805109, -122.5312500020483952 ) ) ;
#9909 = VERTEX_POINT ( 'NONE', #11612 ) ;
#9910 = CARTESIAN_POINT ( 'NONE',  ( -9.999999999999227285, -5.773502691896698735, -133.1249999999999716 ) ) ;
#9911 = CARTESIAN_POINT ( 'NONE',  ( 9.999999999999479527, 5.773502691896553074, -78.37499999999995737 ) ) ;
#9912 = CARTESIAN_POINT ( 'NONE',  ( -5.405949406250003975, -9.363379034771801557, -179.0312500020483810 ) ) ;
#9913 = CARTESIAN_POINT ( 'NONE',  ( -9.999999999999998224, 1.224646799147353059E-15, -26.74999999999996803 ) ) ;
#9914 = CARTESIAN_POINT ( 'NONE',  ( 9.999999999998969713, 5.773502691896851502, -0.7500000040967217396 ) ) ;
#9915 = CARTESIAN_POINT ( 'NONE',  ( -10.81189881249999729, -6.242252689847864744, -129.4687500020483810 ) ) ;
#9916 = CARTESIAN_POINT ( 'NONE',  ( 5.405949406249992428, -9.363379034771808662, -100.5937500020483810 ) ) ;
#9917 = CARTESIAN_POINT ( 'NONE',  ( -9.999999999999479527, -5.773502691896549521, -143.6250000000000000 ) ) ;
#9918 = CARTESIAN_POINT ( 'NONE',  ( -5.405949406249996869, 9.363379034771805109, -107.5312500020483810 ) ) ;
#9919 = CARTESIAN_POINT ( 'NONE',  ( 4.999999999999992006, -8.660254037844389075, -184.1250000040967905 ) ) ;
#9920 = CARTESIAN_POINT ( 'NONE',  ( -10.81189881249999729, 1.324075727343319199E-15, -114.5937500020483810 ) ) ;
#9921 = CARTESIAN_POINT ( 'NONE',  ( 5.405949406249992428, -9.363379034771808662, -183.2812500020484094 ) ) ;
#9922 = CARTESIAN_POINT ( 'NONE',  ( 9.999999999999998224, 0.000000000000000000, -141.5000000000000000 ) ) ;
#9923 = CARTESIAN_POINT ( 'NONE',  ( -2.121150477449813534E-15, -11.54700538379251284, -6.874999999999964473 ) ) ;
#9924 = CARTESIAN_POINT ( 'NONE',  ( 7.644554776091147741E-16, 12.48450537969573659, -57.96875000204836681 ) ) ;
#9925 = CARTESIAN_POINT ( 'NONE',  ( -5.405949406250003975, -9.363379034771801557, -46.84375000204838102 ) ) ;
#9926 = CARTESIAN_POINT ( 'NONE',  ( -9.999999999999998224, 1.224646799147353059E-15, -178.6250000040968189 ) ) ;
#9927 = CARTESIAN_POINT ( 'NONE',  ( 5.405949406249999534, 9.363379034771803333, -14.78125000204835793 ) ) ;
#9928 = CARTESIAN_POINT ( 'NONE',  ( -10.81189881249999907, -6.242252689847864744, -33.46875000204835260 ) ) ;
#9929 = CARTESIAN_POINT ( 'NONE',  ( 9.999999999999998224, 0.000000000000000000, -107.3750000040967763 ) ) ;
#9930 = CARTESIAN_POINT ( 'NONE',  ( -10.81189881249999907, -6.242252689847864744, -138.4687500020484094 ) ) ;
#9931 = CARTESIAN_POINT ( 'NONE',  ( -5.000000000000003553, -8.660254037844383745, -104.4999999999999858 ) ) ;
#9932 = CARTESIAN_POINT ( 'NONE',  ( -5.405949406250003975, -9.363379034771801557, -39.53125000204838102 ) ) ;
#9933 = CARTESIAN_POINT ( 'NONE',  ( 5.000000000000000000, 8.660254037844385522, -119.1250000040967905 ) ) ;
#9934 = CARTESIAN_POINT ( 'NONE',  ( -5.000000000000003553, -8.660254037844383745, -69.99999999999998579 ) ) ;
#9935 = CARTESIAN_POINT ( 'NONE',  ( 7.644554776091147741E-16, 12.48450537969573659, -130.1562500020483810 ) ) ;
#9936 = CARTESIAN_POINT ( 'NONE',  ( 7.644554776091147741E-16, 12.48450537969573659, -119.6562500020484094 ) ) ;
#9937 = ORIENTED_EDGE ( 'NONE', *, *, #252, .T. ) ;
#9938 = CARTESIAN_POINT ( 'NONE',  ( 9.999999999999998224, 0.000000000000000000, -6.499999999999977796 ) ) ;
#9939 = CARTESIAN_POINT ( 'NONE',  ( 4.999999999999992006, -8.660254037844389075, -109.1250000040967763 ) ) ;
#9940 = CARTESIAN_POINT ( 'NONE',  ( 5.405949406249992428, -9.363379034771808662, -67.59375000204836681 ) ) ;
#9941 = ORIENTED_EDGE ( 'NONE', *, *, #36841, .T. ) ;
#9942 = CARTESIAN_POINT ( 'NONE',  ( 9.999999999999998224, 0.000000000000000000, -30.49999999999997158 ) ) ;
#9943 = CARTESIAN_POINT ( 'NONE',  ( 7.070501591499377789E-16, 11.54700538379251284, -20.00000000409677625 ) ) ;
#9944 = CARTESIAN_POINT ( 'NONE',  ( -10.81189881249999729, 1.324075727343319199E-15, -44.28125000204838102 ) ) ;
#9945 = CARTESIAN_POINT ( 'NONE',  ( -9.999999999999998224, 1.224646799147353059E-15, -200.0000000000000000 ) ) ;
#9946 = CARTESIAN_POINT ( 'NONE',  ( -9.999999999999998224, 1.224646799147353059E-15, -37.62500000409676915 ) ) ;
#9947 = DIRECTION ( 'NONE',  ( 0.000000000000000000, 0.000000000000000000, -1.000000000000000000 ) ) ;
#9948 = CARTESIAN_POINT ( 'NONE',  ( -2.293366432827344421E-15, -12.48450537969573659, -136.9062500020484094 ) ) ;
#9949 = EDGE_CURVE ( 'NONE', #9613, #23672, #10834, .T. ) ;
#9950 = CARTESIAN_POINT ( 'NONE',  ( 5.405949406249992428, -9.363379034771808662, -138.2812500020483810 ) ) ;
#9951 = DIRECTION ( 'NONE',  ( 1.000000000000000000, 0.000000000000000000, 0.000000000000000000 ) ) ;
#9952 = ORIENTED_EDGE ( 'NONE', *, *, #10185, .F. ) ;
#9953 = VERTEX_POINT ( 'NONE', #37533 ) ;
#9954 = VERTEX_POINT ( 'NONE', #11832 ) ;
#9955 =( BOUNDED_CURVE ( )  B_SPLINE_CURVE ( 2, ( #23684, #34468, #4247, #11347, #10705, #23901, #21282 ),
 .UNSPECIFIED., .F., .F. ) 
 B_SPLINE_CURVE_WITH_KNOTS ( ( 3, 2, 2, 3 ),
 ( 0.6865671641791046831, 0.6878109452736320684, 0.6890547263681594536, 0.6902985074626868389 ),
 .UNSPECIFIED. ) 
 CURVE ( )  GEOMETRIC_REPRESENTATION_ITEM ( )  RATIONAL_B_SPLINE_CURVE ( ( 0.9999999999999761302, 0.8660254037844625774, 1.000000000000000000, 0.8660254037844387076, 1.000000000000000000, 0.8660254037844148378, 1.000000000000023981 ) ) 
 REPRESENTATION_ITEM ( '' )  );
#9956 = EDGE_CURVE ( 'NONE', #34592, #1591, #25490, .T. ) ;
#9957 = CARTESIAN_POINT ( 'NONE',  ( 9.999999999999998224, 0.000000000000000000, -200.0000000000000000 ) ) ;
#9958 = CARTESIAN_POINT ( 'NONE',  ( -5.405949406249996869, 9.363379034771805109, -173.3437500020484094 ) ) ;
#9959 = CARTESIAN_POINT ( 'NONE',  ( 10.81189881249999729, 0.000000000000000000, -22.34375000204835615 ) ) ;
#9960 = CARTESIAN_POINT ( 'NONE',  ( -9.999999999999998224, 1.224646799147353059E-15, -129.1250000040967620 ) ) ;
#9961 = CARTESIAN_POINT ( 'NONE',  ( -10.81189881249999729, 1.324075727343319199E-15, -156.5937500020483810 ) ) ;
#9962 = CARTESIAN_POINT ( 'NONE',  ( 10.81189881249999907, 6.242252689847868297, -148.2187500020484094 ) ) ;
#9963 = CARTESIAN_POINT ( 'NONE',  ( -2.121150477449813534E-15, -11.54700538379251284, -9.874999999999982236 ) ) ;
#9964 = CARTESIAN_POINT ( 'NONE',  ( -10.81189881249999729, 6.242252689847871849, -128.2187500020483810 ) ) ;
#9965 = CARTESIAN_POINT ( 'NONE',  ( -2.293366432827344421E-15, -12.48450537969573659, -130.9062500020483810 ) ) ;
#9966 = CARTESIAN_POINT ( 'NONE',  ( 7.644554776091147741E-16, 12.48450537969573659, -18.96875000204837391 ) ) ;
#9967 = CARTESIAN_POINT ( 'NONE',  ( -10.81189881249999729, -6.242252689847864744, -141.4687500020483810 ) ) ;
#9968 = DIRECTION ( 'NONE',  ( -0.000000000000000000, -0.000000000000000000, 1.000000000000000000 ) ) ;
#9969 = DIRECTION ( 'NONE',  ( 0.000000000000000000, 0.000000000000000000, -1.000000000000000000 ) ) ;
#9970 = CARTESIAN_POINT ( 'NONE',  ( 4.999999999999992006, -8.660254037844389075, -162.7500000000000000 ) ) ;
#9971 = CARTESIAN_POINT ( 'NONE',  ( 4.999999999999992006, -8.660254037844389075, -167.6250000040967905 ) ) ;
#9972 = CARTESIAN_POINT ( 'NONE',  ( -10.81189881249999729, 6.242252689847871849, -72.71875000204835260 ) ) ;
#9973 = CARTESIAN_POINT ( 'NONE',  ( 5.405949406249999534, 9.363379034771803333, -44.78125000204838102 ) ) ;
#9974 = CARTESIAN_POINT ( 'NONE',  ( -5.405949406249996869, 9.363379034771805109, -53.34375000204835970 ) ) ;
#9975 = DIRECTION ( 'NONE',  ( -0.000000000000000000, -0.000000000000000000, -1.000000000000000000 ) ) ;
#9976 = CARTESIAN_POINT ( 'NONE',  ( -5.405949406250003975, -9.363379034771801557, -165.3437500020484094 ) ) ;
#9977 = CARTESIAN_POINT ( 'NONE',  ( 10.00000000000000000, 5.773502691896255534, -129.3750000000000000 ) ) ;
#9978 = CARTESIAN_POINT ( 'NONE',  ( 10.81189881249999551, -6.242252689847874514, -136.6562500020484094 ) ) ;
#9979 = CARTESIAN_POINT ( 'NONE',  ( 9.999999999999998224, 0.000000000000000000, -98.37500000409677625 ) ) ;
#9980 = CARTESIAN_POINT ( 'NONE',  ( -5.000000000000003553, -8.660254037844383745, -110.8750000040967763 ) ) ;
#9981 = CARTESIAN_POINT ( 'NONE',  ( 7.070501591499377789E-16, 11.54700538379251284, -94.62499999999997158 ) ) ;
#9982 = EDGE_LOOP ( 'NONE', ( #11520, #19248, #9120, #27863 ) ) ;
#9983 = CARTESIAN_POINT ( 'NONE',  ( 5.405949406249992428, -9.363379034771808662, -114.2812500020483952 ) ) ;
#9984 = CARTESIAN_POINT ( 'NONE',  ( -5.000000000000003553, -8.660254037844383745, -128.8750000040967905 ) ) ;
#9985 = CARTESIAN_POINT ( 'NONE',  ( -9.999999999999998224, 1.224646799147353059E-15, -200.0000000000000000 ) ) ;
#9986 = CARTESIAN_POINT ( 'NONE',  ( -2.293366432827344421E-15, -12.48450537969573659, -160.9062500020483810 ) ) ;
#9987 = CARTESIAN_POINT ( 'NONE',  ( -9.999999999999998224, 5.773502691896259087, -45.25000000409676915 ) ) ;
#9988 = CYLINDRICAL_SURFACE ( 'NONE', #27662, 9.999999999999998224 ) ;
#9989 = CARTESIAN_POINT ( 'NONE',  ( 5.405949406249999534, 9.363379034771803333, -59.78125000204836681 ) ) ;
#9990 = EDGE_CURVE ( 'NONE', #10829, #24501, #37311, .T. ) ;
#9991 = CARTESIAN_POINT ( 'NONE',  ( 10.81189881249999907, 6.242252689847868297, -163.4062500020484094 ) ) ;
#9992 = CARTESIAN_POINT ( 'NONE',  ( 10.81189881249999729, 0.000000000000000000, -137.8437500020484094 ) ) ;
#9993 = CARTESIAN_POINT ( 'NONE',  ( -9.999999999999998224, 1.224646799147353059E-15, -200.0000000000000000 ) ) ;
#9994 = CARTESIAN_POINT ( 'NONE',  ( 7.070501591499376803E-16, 11.54700538379251284, -171.5000000040967905 ) ) ;
#9995 = ORIENTED_EDGE ( 'NONE', *, *, #41316, .T. ) ;
#9996 = CARTESIAN_POINT ( 'NONE',  ( -12.99038105676666888, -7.500000000000057732, 49.99999999999998579 ) ) ;
#9997 =( BOUNDED_CURVE ( )  B_SPLINE_CURVE ( 2, ( #12138, #31379, #41273, #24695, #5253, #22082, #38263 ),
 .UNSPECIFIED., .F., .F. ) 
 B_SPLINE_CURVE_WITH_KNOTS ( ( 3, 2, 2, 3 ),
 ( 0.4402985074626867279, 0.4415422885572141132, 0.4427860696517414429, 0.4440298507462688282 ),
 .UNSPECIFIED. ) 
 CURVE ( )  GEOMETRIC_REPRESENTATION_ITEM ( )  RATIONAL_B_SPLINE_CURVE ( ( 0.9999999999999820144, 0.8660254037844566932, 1.000000000000000000, 0.8660254037844387076, 1.000000000000000000, 0.8660254037844207220, 1.000000000000017986 ) ) 
 REPRESENTATION_ITEM ( '' )  );
#9999 = ORIENTED_EDGE ( 'NONE', *, *, #20684, .T. ) ;
#9998 = CARTESIAN_POINT ( 'NONE',  ( 10.81189881249999729, 0.000000000000000000, -73.53125000204838102 ) ) ;
#10000 = PERSON_AND_ORGANIZATION_ROLE ( 'creator' ) ;
#10002 = ORIENTED_EDGE ( 'NONE', *, *, #16038, .T. ) ;
#10001 = CARTESIAN_POINT ( 'NONE',  ( -5.405949406250003975, -9.363379034771801557, -117.3437500020483810 ) ) ;
#10003 = ORIENTED_EDGE ( 'NONE', *, *, #2805, .T. ) ;
#10004 = VECTOR ( 'NONE', #10783, 1000.000000000000000 ) ;
#10005 = CARTESIAN_POINT ( 'NONE',  ( -2.293366432827344421E-15, -12.48450537969573659, -22.71875000204837391 ) ) ;
#10006 = CARTESIAN_POINT ( 'NONE',  ( 5.405949406249992428, -9.363379034771808662, -196.5937500020484094 ) ) ;
#10007 =( BOUNDED_CURVE ( )  B_SPLINE_CURVE ( 2, ( #33287, #15834, #29034, #3712, #30040, #39944, #14678 ),
 .UNSPECIFIED., .F., .F. ) 
 B_SPLINE_CURVE_WITH_KNOTS ( ( 3, 2, 2, 3 ),
 ( 0.3582089552238806873, 0.3594527363184080726, 0.3606965174129355134, 0.3619402985074628432 ),
 .UNSPECIFIED. ) 
 CURVE ( )  GEOMETRIC_REPRESENTATION_ITEM ( )  RATIONAL_B_SPLINE_CURVE ( ( 0.9999999999999880096, 0.8660254037844506980, 1.000000000000000000, 0.8660254037844387076, 1.000000000000000000, 0.8660254037844207220, 1.000000000000017986 ) ) 
 REPRESENTATION_ITEM ( '' )  );
#10008 = CARTESIAN_POINT ( 'NONE',  ( -5.405949406249996869, 9.363379034771805109, -44.34375000204837391 ) ) ;
#10009 = CARTESIAN_POINT ( 'NONE',  ( -5.000000000000003553, -8.660254037844383745, -134.5000000000000000 ) ) ;
#10010 = EDGE_CURVE ( 'NONE', #27538, #36032, #19665, .T. ) ;
#10011 = CARTESIAN_POINT ( 'NONE',  ( 5.000000000000000000, 8.660254037844385522, -27.24999999999996803 ) ) ;
#10012 = CARTESIAN_POINT ( 'NONE',  ( -10.81189881249999729, 1.324075727343319199E-15, -179.0937500020484094 ) ) ;
#10013 = VECTOR ( 'NONE', #10164, 1000.000000000000000 ) ;
#10014 = CARTESIAN_POINT ( 'NONE',  ( -5.405949406249996869, 9.363379034771805109, -167.3437500020484094 ) ) ;
#10015 = CARTESIAN_POINT ( 'NONE',  ( 10.81189881249999729, 0.000000000000000000, -149.8437500020483810 ) ) ;
#10016 = CARTESIAN_POINT ( 'NONE',  ( 5.405949406249992428, -9.363379034771808662, -165.0937500020484094 ) ) ;
#10017 = LINE ( 'NONE', #33132, #6768 ) ;
#10018 = CARTESIAN_POINT ( 'NONE',  ( 9.999999999999998224, 0.000000000000000000, -102.8750000040967763 ) ) ;
#10019 = CARTESIAN_POINT ( 'NONE',  ( -9.999999999999998224, 1.224646799147353059E-15, -187.2500000000000000 ) ) ;
#10020 = CARTESIAN_POINT ( 'NONE',  ( 10.81189881249999729, 0.000000000000000000, -100.3437500020483810 ) ) ;
#10021 = CARTESIAN_POINT ( 'NONE',  ( 9.999999999999998224, 0.000000000000000000, -152.0000000000000000 ) ) ;
#10022 = CARTESIAN_POINT ( 'NONE',  ( -10.81189881249999907, -6.242252689847864744, -65.15625000204838102 ) ) ;
#10023 = CARTESIAN_POINT ( 'NONE',  ( 10.81189881249999729, 0.000000000000000000, -188.8437500020483810 ) ) ;
#10024 = CARTESIAN_POINT ( 'NONE',  ( -5.405949406250003975, -9.363379034771801557, -120.5312500020483952 ) ) ;
#10025 = CARTESIAN_POINT ( 'NONE',  ( -5.405949406250003975, -9.363379034771801557, -164.0312500020484094 ) ) ;
#10026 = CARTESIAN_POINT ( 'NONE',  ( -5.405949406250003975, -9.363379034771801557, -53.03125000204836681 ) ) ;
#10027 = CARTESIAN_POINT ( 'NONE',  ( -9.999999999999998224, 5.773502691896259087, -141.2500000040967905 ) ) ;
#10028 = CARTESIAN_POINT ( 'NONE',  ( -4.999999999999996447, 8.660254037844387298, -117.0000000000000000 ) ) ;
#10029 = ORIENTED_EDGE ( 'NONE', *, *, #25344, .F. ) ;
#10030 = CARTESIAN_POINT ( 'NONE',  ( 10.81189881249999729, 6.242252689847867408, -133.4062500020483810 ) ) ;
#10031 = CARTESIAN_POINT ( 'NONE',  ( -5.405949406250003975, -9.363379034771801557, -146.0312500020483810 ) ) ;
#10032 = CARTESIAN_POINT ( 'NONE',  ( 10.81189881249999907, 6.242252689847868297, -193.4062500020484094 ) ) ;
#10033 = CARTESIAN_POINT ( 'NONE',  ( 10.00000000000000000, 5.773502691896255534, -131.2500000040967905 ) ) ;
#10034 = CARTESIAN_POINT ( 'NONE',  ( -10.81189881249999729, 1.324075727343319199E-15, -86.09375000204836681 ) ) ;
#10035 = ORIENTED_EDGE ( 'NONE', *, *, #7513, .F. ) ;
#10036 = CARTESIAN_POINT ( 'NONE',  ( 9.999999999999998224, 0.000000000000000000, -54.49999999999996447 ) ) ;
#10037 = CARTESIAN_POINT ( 'NONE',  ( -5.405949406249996869, 9.363379034771805109, -185.3437500020483810 ) ) ;
#10038 = CARTESIAN_POINT ( 'NONE',  ( 7.070501591499377789E-16, 11.54700538379251284, -69.50000000409679046 ) ) ;
#10039 = CYLINDRICAL_SURFACE ( 'NONE', #343, 9.999999999999998224 ) ;
#10040 = FACE_OUTER_BOUND ( 'NONE', #14721, .T. ) ;
#10041 = CARTESIAN_POINT ( 'NONE',  ( -10.81189881249999729, 6.242252689847871849, -87.90625000204838102 ) ) ;
#10042 = VECTOR ( 'NONE', #17756, 1000.000000000000000 ) ;
#10043 = CARTESIAN_POINT ( 'NONE',  ( 10.81189881249999551, -6.242252689847874514, -60.15625000204838813 ) ) ;
#10044 = VECTOR ( 'NONE', #15879, 1000.000000000000000 ) ;
#10045 = CARTESIAN_POINT ( 'NONE',  ( -2.121150477449813534E-15, -11.54700538379251284, -61.25000000409677625 ) ) ;
#10046 = CARTESIAN_POINT ( 'NONE',  ( -2.293366432827344421E-15, -12.48450537969573659, -19.71875000204837036 ) ) ;
#10047 = LINE ( 'NONE', #22803, #23490 ) ;
#10048 = CARTESIAN_POINT ( 'NONE',  ( 10.81189881249999729, 0.000000000000000000, -186.0312500020484094 ) ) ;
#10049 = CARTESIAN_POINT ( 'NONE',  ( 5.405949406249992428, -9.363379034771808662, -10.78125000204835438 ) ) ;
#10050 = LINE ( 'NONE', #39200, #2185 ) ;
#10051 = CARTESIAN_POINT ( 'NONE',  ( -4.999999999999996447, 8.660254037844387298, -175.8750000040967905 ) ) ;
#10052 = AXIS2_PLACEMENT_3D ( 'NONE', #7855, #10434, #324 ) ;
#10053 = CARTESIAN_POINT ( 'NONE',  ( 60.00000000000000711, 0.000000000000000000, -240.0000000000000000 ) ) ;
#10054 = CARTESIAN_POINT ( 'NONE',  ( -9.999999999999227285, -5.773502691896698735, -135.0000000040967620 ) ) ;
#10055 = CARTESIAN_POINT ( 'NONE',  ( 4.999999999999992006, -8.660254037844389075, -167.2500000000000000 ) ) ;
#10056 = CARTESIAN_POINT ( 'NONE',  ( 9.999999999999998224, 0.000000000000000000, -168.8750000040967905 ) ) ;
#10057 = SHAPE_REPRESENTATION ( 'retaining plate', ( #39998 ), #28334 ) ;
#10059 = ORIENTED_EDGE ( 'NONE', *, *, #24680, .F. ) ;
#10058 = CARTESIAN_POINT ( 'NONE',  ( -5.405949406250003975, -9.363379034771801557, -95.03125000204838102 ) ) ;
#10060 = CARTESIAN_POINT ( 'NONE',  ( 9.999999999999998224, 0.000000000000000000, -180.8750000040967905 ) ) ;
#10062 = EDGE_LOOP ( 'NONE', ( #35120, #639, #26318, #20504 ) ) ;
#10061 = CARTESIAN_POINT ( 'NONE',  ( -10.81189881249999729, -6.242252689847864744, -102.4687500020483810 ) ) ;
#10063 = ORIENTED_EDGE ( 'NONE', *, *, #26217, .T. ) ;
#10064 = CARTESIAN_POINT ( 'NONE',  ( -5.405949406250003975, -9.363379034771801557, -34.84375000204836681 ) ) ;
#10065 = CARTESIAN_POINT ( 'NONE',  ( 10.81189881249999551, -6.242252689847874514, -19.65625000204837747 ) ) ;
#10066 = PERSON_AND_ORGANIZATION_ROLE ( 'classification_officer' ) ;
#10067 = CARTESIAN_POINT ( 'NONE',  ( 10.81189881249999907, 6.242252689847868297, -70.21875000204840944 ) ) ;
#10068 = CARTESIAN_POINT ( 'NONE',  ( 9.999999999999998224, 0.000000000000000000, -173.3750000040968189 ) ) ;
#10069 = EDGE_CURVE ( 'NONE', #38354, #41544, #1723, .T. ) ;
#10070 = CARTESIAN_POINT ( 'NONE',  ( -5.405949406249996869, 9.363379034771805109, -195.8437500020484094 ) ) ;
#10071 = CARTESIAN_POINT ( 'NONE',  ( 10.81189881249999551, -6.242252689847874514, -152.9687500020484094 ) ) ;
#10072 = EDGE_CURVE ( 'NONE', #10798, #22060, #28519, .T. ) ;
#10073 = CIRCLE ( 'NONE', #6631, 5.500000000000003553 ) ;
#10074 = DIRECTION ( 'NONE',  ( -0.000000000000000000, -0.000000000000000000, 1.000000000000000000 ) ) ;
#10075 = CARTESIAN_POINT ( 'NONE',  ( 7.070501591499376803E-16, 11.54700538379251284, -172.6249999999999716 ) ) ;
#10076 = CARTESIAN_POINT ( 'NONE',  ( -10.81189881249999729, 1.324075727343319199E-15, -152.2812500020484094 ) ) ;
#10077 = CARTESIAN_POINT ( 'NONE',  ( 4.999999999999992006, -8.660254037844389075, -7.125000004096743389 ) ) ;
#10078 = CARTESIAN_POINT ( 'NONE',  ( 10.81189881249999907, 6.242252689847868297, -122.7187500020483810 ) ) ;
#10079 = CARTESIAN_POINT ( 'NONE',  ( 9.999999999999998224, 0.000000000000000000, -15.49999999999995737 ) ) ;
#10080 = CARTESIAN_POINT ( 'NONE',  ( -2.293366432827344421E-15, -12.48450537969573659, -87.40625000204838102 ) ) ;
#10081 = CARTESIAN_POINT ( 'NONE',  ( -5.405949406250003975, -9.363379034771801557, -109.8437500020483810 ) ) ;
#10082 = CARTESIAN_POINT ( 'NONE',  ( -5.405949406250003975, -9.363379034771801557, -81.34375000204838102 ) ) ;
#10083 = CARTESIAN_POINT ( 'NONE',  ( 5.405949406249999534, 9.363379034771803333, -80.78125000204838102 ) ) ;
#10084 = CARTESIAN_POINT ( 'NONE',  ( 10.00000000000000000, 5.773502691896255534, -164.2500000040967905 ) ) ;
#10085 = CARTESIAN_POINT ( 'NONE',  ( -2.121150477449813534E-15, -11.54700538379251284, -11.37499999999995737 ) ) ;
#10086 = CARTESIAN_POINT ( 'NONE',  ( -10.81189881249999729, 1.324075727343319199E-15, -167.2812500020484094 ) ) ;
#10087 = CARTESIAN_POINT ( 'NONE',  ( -2.293366432827344421E-15, -12.48450537969573659, -181.9062500020483810 ) ) ;
#10088 = CARTESIAN_POINT ( 'NONE',  ( 9.999999999999998224, 1.224646799147353059E-15, -99.99999999999998579 ) ) ;
#10089 = CARTESIAN_POINT ( 'NONE',  ( -10.81189881249999729, 1.324075727343319199E-15, -6.593750002048370362 ) ) ;
#10090 = CARTESIAN_POINT ( 'NONE',  ( 10.81189881249999729, 0.000000000000000000, -115.3437500020483810 ) ) ;
#10091 = CARTESIAN_POINT ( 'NONE',  ( 5.000000000000000000, 8.660254037844385522, -81.24999999999998579 ) ) ;
#10092 = CARTESIAN_POINT ( 'NONE',  ( 10.81189881249999729, 0.000000000000000000, -10.53125000204835260 ) ) ;
#10093 = CARTESIAN_POINT ( 'NONE',  ( 4.999999999999992006, -8.660254037844389075, -92.62500000409677625 ) ) ;
#10094 = ADVANCED_FACE ( 'NONE', ( #26293 ), #9037, .T. ) ;
#10095 = DIRECTION ( 'NONE',  ( -1.000000000000000000, 0.000000000000000000, 0.000000000000000000 ) ) ;
#10096 = CARTESIAN_POINT ( 'NONE',  ( 10.81189881249999907, 6.242252689847868297, -109.4062500020483952 ) ) ;
#10097 = CARTESIAN_POINT ( 'NONE',  ( -10.81189881249999729, -6.242252689847864744, -84.65625000204836681 ) ) ;
#10098 = VERTEX_POINT ( 'NONE', #22202 ) ;
#10099 = CARTESIAN_POINT ( 'NONE',  ( 7.070501591499377789E-16, 11.54700538379251284, -84.50000000409677625 ) ) ;
#10100 = CARTESIAN_POINT ( 'NONE',  ( 7.070501591499376803E-16, 11.54700538379251284, -48.12499999999997158 ) ) ;
#10101 = CARTESIAN_POINT ( 'NONE',  ( -5.405949406249996869, 9.363379034771805109, -44.34375000204837391 ) ) ;
#10102 = VERTEX_POINT ( 'NONE', #26079 ) ;
#10103 = CARTESIAN_POINT ( 'NONE',  ( -4.999999999999996447, 8.660254037844387298, -10.49999999999995381 ) ) ;
#10104 = CARTESIAN_POINT ( 'NONE',  ( 5.000000000000000000, 8.660254037844385522, -147.2500000000000000 ) ) ;
#10105 = CARTESIAN_POINT ( 'NONE',  ( -9.999999999999998224, 1.224646799147353059E-15, -15.12500000409674961 ) ) ;
#10106 = EDGE_CURVE ( 'NONE', #6565, #22119, #32911, .T. ) ;
#10107 = CARTESIAN_POINT ( 'NONE',  ( -4.999999999999996447, 8.660254037844387298, -15.37500000409675138 ) ) ;
#10108 = CARTESIAN_POINT ( 'NONE',  ( 10.00000000000000000, 5.773502691896255534, -193.8750000000000284 ) ) ;
#10109 = PLANE ( 'NONE',  #22036 ) ;
#10111 = ORIENTED_EDGE ( 'NONE', *, *, #1444, .T. ) ;
#10110 = CARTESIAN_POINT ( 'NONE',  ( 10.81189881249999729, 0.000000000000000000, -115.5312500020483952 ) ) ;
#10112 = LINE ( 'NONE', #19821, #6933 ) ;
#10113 = EDGE_LOOP ( 'NONE', ( #33426, #3365, #17108, #36037 ) ) ;
#10114 = CARTESIAN_POINT ( 'NONE',  ( -2.293366432827344421E-15, -12.48450537969573659, -49.90625000204838102 ) ) ;
#10115 = DATE_TIME_ROLE ( 'creation_date' ) ;
#10116 = CARTESIAN_POINT ( 'NONE',  ( 5.405949406249999534, 9.363379034771803333, -97.09375000204838102 ) ) ;
#10117 = CARTESIAN_POINT ( 'NONE',  ( -10.81189881249999729, 6.242252689847871849, -123.9062500020483810 ) ) ;
#10119 = ORIENTED_EDGE ( 'NONE', *, *, #7351, .F. ) ;
#10118 = ADVANCED_FACE ( 'NONE', ( #6643 ), #19793, .T. ) ;
#10120 = CARTESIAN_POINT ( 'NONE',  ( 9.999999999999998224, 0.000000000000000000, -84.87500000409677625 ) ) ;
#10121 = DIRECTION ( 'NONE',  ( -0.000000000000000000, -0.000000000000000000, 1.000000000000000000 ) ) ;
#10122 =( BOUNDED_CURVE ( )  B_SPLINE_CURVE ( 2, ( #33149, #10033, #3579, #26447, #13049, #16713, #29478 ),
 .UNSPECIFIED., .F., .F. ) 
 B_SPLINE_CURVE_WITH_KNOTS ( ( 3, 2, 2, 3 ),
 ( 0.3358208955223880854, 0.3370646766169154707, 0.3383084577114429670, 0.3395522388059703522 ),
 .UNSPECIFIED. ) 
 CURVE ( )  GEOMETRIC_REPRESENTATION_ITEM ( )  RATIONAL_B_SPLINE_CURVE ( ( 1.000000000000000000, 0.8660254037844387076, 1.000000000000000000, 0.8660254037844387076, 1.000000000000000000, 0.8660254037844148378, 1.000000000000023981 ) ) 
 REPRESENTATION_ITEM ( '' )  );
#10123 = EDGE_CURVE ( 'NONE', #33268, #33809, #3920, .T. ) ;
#10124 = CARTESIAN_POINT ( 'NONE',  ( 5.405949406249999534, 9.363379034771803333, -170.7812500020484094 ) ) ;
#10125 = CARTESIAN_POINT ( 'NONE',  ( -10.00000000000102496, 5.773502691895664007, -13.75000000409673184 ) ) ;
#10126 = ADVANCED_FACE ( 'NONE', ( #35588 ), #39022, .T. ) ;
#10127 = CARTESIAN_POINT ( 'NONE',  ( -10.81189881249999729, 1.324075727343319199E-15, -132.5937500020483810 ) ) ;
#10128 = CARTESIAN_POINT ( 'NONE',  ( 5.405949406249999534, 9.363379034771803333, -98.59375000204838102 ) ) ;
#10129 = CARTESIAN_POINT ( 'NONE',  ( -5.405949406250003975, -9.363379034771801557, -107.0312500020483810 ) ) ;
#10130 = CARTESIAN_POINT ( 'NONE',  ( 10.00000000000000000, 5.773502691896255534, -186.7500000040967905 ) ) ;
#10131 = CARTESIAN_POINT ( 'NONE',  ( 10.81189881249999551, -6.242252689847874514, -110.9687500020483810 ) ) ;
#10132 = CARTESIAN_POINT ( 'NONE',  ( -5.405949406250003975, -9.363379034771801557, -183.5312500020484094 ) ) ;
#10133 = CARTESIAN_POINT ( 'NONE',  ( 9.999999999999998224, 0.000000000000000000, -149.3750000040967905 ) ) ;
#10134 = DIRECTION ( 'NONE',  ( -0.4999999999999998890, -0.8660254037844387076, 0.000000000000000000 ) ) ;
#10135 = CARTESIAN_POINT ( 'NONE',  ( 7.070501591499377789E-16, 11.54700538379251284, -132.1250000000000000 ) ) ;
#10136 = CARTESIAN_POINT ( 'NONE',  ( -9.999999999999998224, 5.773502691896259087, -4.374999999999961808 ) ) ;
#10137 = CARTESIAN_POINT ( 'NONE',  ( 10.81189881249999729, 6.242252689847867408, -61.21875000204838813 ) ) ;
#10138 = CARTESIAN_POINT ( 'NONE',  ( -2.293366432827344421E-15, -12.48450537969573659, -49.71875000204835970 ) ) ;
#10139 = CARTESIAN_POINT ( 'NONE',  ( 9.999999999999996447, -5.773502691896262640, -178.0000000040967905 ) ) ;
#10140 = CARTESIAN_POINT ( 'NONE',  ( 7.644554776091147741E-16, 12.48450537969573659, -17.65625000204836681 ) ) ;
#10141 = CARTESIAN_POINT ( 'NONE',  ( -5.405949406250003975, -9.363379034771801557, -28.84375000204836326 ) ) ;
#10142 = CARTESIAN_POINT ( 'NONE',  ( -9.999999999999998224, 1.224646799147353059E-15, -124.6250000040967763 ) ) ;
#10143 = CARTESIAN_POINT ( 'NONE',  ( -10.81189881249999907, -6.242252689847864744, -136.9687500020483810 ) ) ;
#10144 = CARTESIAN_POINT ( 'NONE',  ( -9.999999999999998224, 1.224646799147353059E-15, -106.2499999999999858 ) ) ;
#10145 = CARTESIAN_POINT ( 'NONE',  ( -10.81189881249999907, -6.242252689847864744, -36.65625000204835970 ) ) ;
#10146 = CARTESIAN_POINT ( 'NONE',  ( 9.999999999999998224, 0.000000000000000000, -27.49999999999996803 ) ) ;
#10147 = CARTESIAN_POINT ( 'NONE',  ( -4.999999999999996447, 8.660254037844387298, -58.49999999999997158 ) ) ;
#10148 = CARTESIAN_POINT ( 'NONE',  ( 5.405949406249999534, 9.363379034771803333, -133.2812500020483810 ) ) ;
#10149 = CARTESIAN_POINT ( 'NONE',  ( -10.81189881249999729, 1.324075727343319199E-15, -111.7812500020483810 ) ) ;
#10150 = EDGE_CURVE ( 'NONE', #29288, #26359, #17130, .T. ) ;
#10151 = ORIENTED_EDGE ( 'NONE', *, *, #23826, .T. ) ;
#10152 = FACE_OUTER_BOUND ( 'NONE', #39088, .T. ) ;
#10153 = CARTESIAN_POINT ( 'NONE',  ( 10.00000000000000000, 5.773502691896255534, -110.2500000040967905 ) ) ;
#10154 = CARTESIAN_POINT ( 'NONE',  ( -10.00000000000025580, 5.773502691896109873, -100.7500000040968047 ) ) ;
#10155 = CARTESIAN_POINT ( 'NONE',  ( -10.81189881249999729, 1.324075727343319199E-15, -66.59375000204836681 ) ) ;
#10156 = VERTEX_POINT ( 'NONE', #2991 ) ;
#10157 = CARTESIAN_POINT ( 'NONE',  ( 10.00000000000000000, 5.773502691896255534, -33.37499999999996447 ) ) ;
#10158 = CARTESIAN_POINT ( 'NONE',  ( 9.999999999999996447, -5.773502691896262640, -19.00000000409676915 ) ) ;
#10159 = CARTESIAN_POINT ( 'NONE',  ( -5.405949406249996869, 9.363379034771805109, -46.03125000204838813 ) ) ;
#10160 = DIRECTION ( 'NONE',  ( -0.000000000000000000, -0.000000000000000000, 1.000000000000000000 ) ) ;
#10161 = CARTESIAN_POINT ( 'NONE',  ( -10.00000000000000000, -5.773502691896251982, -34.50000000409675494 ) ) ;
#10162 = CARTESIAN_POINT ( 'NONE',  ( -9.999999999999998224, 1.224646799147353059E-15, -107.7499999999999858 ) ) ;
#10163 = CARTESIAN_POINT ( 'NONE',  ( -10.81189881249999907, -6.242252689847864744, -143.1562500020484094 ) ) ;
#10164 = DIRECTION ( 'NONE',  ( -0.000000000000000000, -0.000000000000000000, 1.000000000000000000 ) ) ;
#10165 = ORIENTED_EDGE ( 'NONE', *, *, #26456, .F. ) ;
#10166 = ORIENTED_EDGE ( 'NONE', *, *, #38108, .T. ) ;
#10167 = VERTEX_POINT ( 'NONE', #42457 ) ;
#10168 = DIRECTION ( 'NONE',  ( -0.000000000000000000, -0.000000000000000000, 1.000000000000000000 ) ) ;
#10169 = CARTESIAN_POINT ( 'NONE',  ( 0.000000000000000000, 0.000000000000000000, -200.0000000000000000 ) ) ;
#10170 = CARTESIAN_POINT ( 'NONE',  ( -5.405949406250003975, -9.363379034771801557, -174.3437500020484094 ) ) ;
#10171 = CARTESIAN_POINT ( 'NONE',  ( -5.405949406249996869, 9.363379034771805109, -24.84375000204835970 ) ) ;
#10172 = FACE_OUTER_BOUND ( 'NONE', #36876, .T. ) ;
#10173 = VECTOR ( 'NONE', #24333, 1000.000000000000000 ) ;
#10174 = CARTESIAN_POINT ( 'NONE',  ( 10.81189881249999729, 6.242252689847867408, -158.7187500020484094 ) ) ;
#10175 = CARTESIAN_POINT ( 'NONE',  ( 10.81189881249999907, 6.242252689847868297, -142.2187500020484094 ) ) ;
#10176 = CARTESIAN_POINT ( 'NONE',  ( 10.00000000000102318, -5.773502691895667560, -88.00000000409673362 ) ) ;
#10177 = CARTESIAN_POINT ( 'NONE',  ( 10.81189881249999729, 0.000000000000000000, -127.3437500020483952 ) ) ;
#10178 = CARTESIAN_POINT ( 'NONE',  ( 10.81189881249999907, 6.242252689847868297, -134.9062500020483810 ) ) ;
#10179 = CARTESIAN_POINT ( 'NONE',  ( 5.405949406249992428, -9.363379034771808662, -13.59375000204834905 ) ) ;
#10180 = CARTESIAN_POINT ( 'NONE',  ( 7.644554776091147741E-16, 12.48450537969573659, -141.9687500020483810 ) ) ;
#10181 = CARTESIAN_POINT ( 'NONE',  ( -5.000000000000003553, -8.660254037844383745, -130.0000000000000000 ) ) ;
#10182 = CARTESIAN_POINT ( 'NONE',  ( -99.99999999999994316, -40.00000000000000711, -170.0000000000000000 ) ) ;
#10183 = CARTESIAN_POINT ( 'NONE',  ( 9.999999999999996447, -5.773502691896262640, -158.1250000000000284 ) ) ;
#10184 = CARTESIAN_POINT ( 'NONE',  ( 4.999999999999992006, -8.660254037844389075, -17.24999999999996092 ) ) ;
#10185 = EDGE_CURVE ( 'NONE', #2553, #1094, #22410, .T. ) ;
#10186 = CARTESIAN_POINT ( 'NONE',  ( 10.81189881249999729, 0.000000000000000000, -71.84375000204836681 ) ) ;
#10187 = CARTESIAN_POINT ( 'NONE',  ( 5.405949406249999534, 9.363379034771803333, -41.78125000204838102 ) ) ;
#10188 = CARTESIAN_POINT ( 'NONE',  ( 10.81189881249999729, 0.000000000000000000, -56.84375000204835970 ) ) ;
#10189 = CARTESIAN_POINT ( 'NONE',  ( -5.000000000000003553, -8.660254037844383745, -113.8750000040967763 ) ) ;
#10190 = CARTESIAN_POINT ( 'NONE',  ( -10.81189881249999907, -6.242252689847864744, -162.4687500020483526 ) ) ;
#10191 = CARTESIAN_POINT ( 'NONE',  ( 5.000000000000000000, 8.660254037844385522, -127.7499999999999716 ) ) ;
#10192 = CARTESIAN_POINT ( 'NONE',  ( -2.293366432827344421E-15, -12.48450537969573659, -141.4062500020484094 ) ) ;
#10193 = DIRECTION ( 'NONE',  ( -1.000000000000000000, 0.000000000000000000, 0.000000000000000000 ) ) ;
#10194 = CARTESIAN_POINT ( 'NONE',  ( -2.121150477449813534E-15, -11.54700538379251284, -113.7500000040967905 ) ) ;
#10195 = CARTESIAN_POINT ( 'NONE',  ( -9.999999999999998224, 1.224646799147353059E-15, -89.74999999999998579 ) ) ;
#10196 = VERTEX_POINT ( 'NONE', #15701 ) ;
#10197 = CARTESIAN_POINT ( 'NONE',  ( -10.81189881249999729, 6.242252689847871849, -108.9062500020483810 ) ) ;
#10198 = CARTESIAN_POINT ( 'NONE',  ( -10.00000000000000000, -5.773502691896251982, -130.5000000040967905 ) ) ;
#10199 = DIRECTION ( 'NONE',  ( -0.000000000000000000, -0.000000000000000000, 1.000000000000000000 ) ) ;
#10200 = CARTESIAN_POINT ( 'NONE',  ( 10.81189881249999551, -6.242252689847874514, -166.6562500020484094 ) ) ;
#10201 = CARTESIAN_POINT ( 'NONE',  ( -10.00000000000000000, -5.773502691896251982, -39.00000000409676915 ) ) ;
#10202 = CARTESIAN_POINT ( 'NONE',  ( 9.999999999999998224, 0.000000000000000000, -90.87500000409677625 ) ) ;
#10203 = CARTESIAN_POINT ( 'NONE',  ( 10.81189881249999907, 6.242252689847868297, -49.40625000204837391 ) ) ;
#10204 = CARTESIAN_POINT ( 'NONE',  ( 9.999999999999998224, 0.000000000000000000, -63.49999999999997158 ) ) ;
#10205 = CARTESIAN_POINT ( 'NONE',  ( 5.405949406249992428, -9.363379034771808662, -160.7812500020484094 ) ) ;
#10206 = CARTESIAN_POINT ( 'NONE',  ( -5.405949406249996869, 9.363379034771805109, -134.3437500020484094 ) ) ;
#10207 = CARTESIAN_POINT ( 'NONE',  ( -9.999999999999998224, 1.224646799147353059E-15, -51.12500000409675494 ) ) ;
#10208 = CARTESIAN_POINT ( 'NONE',  ( -9.999999999999918288, -5.773502691896298167, -196.1250000000000284 ) ) ;
#10209 = ORIENTED_EDGE ( 'NONE', *, *, #38350, .T. ) ;
#10210 =( BOUNDED_CURVE ( )  B_SPLINE_CURVE ( 2, ( #8148, #14594, #1249, #21296, #11148, #30391, #20867 ),
 .UNSPECIFIED., .F., .F. ) 
 B_SPLINE_CURVE_WITH_KNOTS ( ( 3, 2, 2, 3 ),
 ( 0.3880597014925373789, 0.3893034825870647087, 0.3905472636815920939, 0.3917910447761194792 ),
 .UNSPECIFIED. ) 
 CURVE ( )  GEOMETRIC_REPRESENTATION_ITEM ( )  RATIONAL_B_SPLINE_CURVE ( ( 0.9999999999999940048, 0.8660254037844447028, 1.000000000000000000, 0.8660254037844387076, 1.000000000000000000, 0.8660254037844327124, 1.000000000000005995 ) ) 
 REPRESENTATION_ITEM ( '' )  );
#10211 = DIRECTION ( 'NONE',  ( 0.000000000000000000, 0.000000000000000000, -1.000000000000000000 ) ) ;
#10213 = ORIENTED_EDGE ( 'NONE', *, *, #4358, .T. ) ;
#10212 = CARTESIAN_POINT ( 'NONE',  ( -5.405949406250003975, -9.363379034771801557, -68.03125000204838102 ) ) ;
#10214 = CALENDAR_DATE ( 2026, 28, 9 ) ;
#10216 = ORIENTED_EDGE ( 'NONE', *, *, #6673, .F. ) ;
#10215 = CARTESIAN_POINT ( 'NONE',  ( 10.81189881249999551, -6.242252689847874514, -116.9687500020483952 ) ) ;
#10217 = CARTESIAN_POINT ( 'NONE',  ( 5.405949406249992428, -9.363379034771808662, -22.59375000204835615 ) ) ;
#10218 = CARTESIAN_POINT ( 'NONE',  ( 7.644554776091147741E-16, 12.48450537969573659, -1.156250002048369474 ) ) ;
#10219 = CARTESIAN_POINT ( 'NONE',  ( 10.81189881249999907, 6.242252689847868297, -46.21875000204837391 ) ) ;
#10220 = LINE ( 'NONE', #19726, #33020 ) ;
#10221 = CARTESIAN_POINT ( 'NONE',  ( 9.999999999999998224, 0.000000000000000000, -0.4999999999999726885 ) ) ;
#10222 = CARTESIAN_POINT ( 'NONE',  ( 10.81189881249999551, -6.242252689847874514, -176.9687500020484094 ) ) ;
#10223 = CARTESIAN_POINT ( 'NONE',  ( -10.81189881249999729, 1.324075727343319199E-15, -171.5937500020484094 ) ) ;
#10224 = CARTESIAN_POINT ( 'NONE',  ( -5.405949406250003975, -9.363379034771801557, -145.8437500020483810 ) ) ;
#10225 = CARTESIAN_POINT ( 'NONE',  ( 10.81189881249999729, 0.000000000000000000, -164.8437500020484094 ) ) ;
#10226 = CARTESIAN_POINT ( 'NONE',  ( -9.999999999999479527, -5.773502691896549521, -105.0000000040967620 ) ) ;
#10227 = CARTESIAN_POINT ( 'NONE',  ( 9.999999999999998224, 0.000000000000000000, -194.3750000040967905 ) ) ;
#10228 = CARTESIAN_POINT ( 'NONE',  ( -5.000000000000003553, -8.660254037844383745, -190.0000000000000000 ) ) ;
#10229 = CARTESIAN_POINT ( 'NONE',  ( 5.405949406249999534, 9.363379034771803333, -98.59375000204838102 ) ) ;
#10230 = CARTESIAN_POINT ( 'NONE',  ( 9.999999999999998224, 0.000000000000000000, -72.49999999999998579 ) ) ;
#10231 = CARTESIAN_POINT ( 'NONE',  ( 7.644554776091147741E-16, 12.48450537969573659, -67.15625000204838102 ) ) ;
#10232 = CARTESIAN_POINT ( 'NONE',  ( -5.000000000000003553, -8.660254037844383745, -5.499999999999976907 ) ) ;
#10233 = CARTESIAN_POINT ( 'NONE',  ( 10.81189881249999551, -6.242252689847874514, -188.9687500020484094 ) ) ;
#10234 = CARTESIAN_POINT ( 'NONE',  ( 7.644554776091147741E-16, 12.48450537969573659, -119.6562500020484094 ) ) ;
#10235 = CARTESIAN_POINT ( 'NONE',  ( 10.81189881249999729, 6.242252689847867408, -160.4062500020483810 ) ) ;
#10236 = CARTESIAN_POINT ( 'NONE',  ( -2.293366432827344421E-15, -12.48450537969573659, -52.90625000204837391 ) ) ;
#10237 = CARTESIAN_POINT ( 'NONE',  ( -4.999999999999996447, 8.660254037844387298, -141.3750000040967905 ) ) ;
#10238 = CARTESIAN_POINT ( 'NONE',  ( -9.999999999999998224, 5.773502691896259087, -118.3750000000000000 ) ) ;
#10239 = ORIENTED_EDGE ( 'NONE', *, *, #6160, .T. ) ;
#10240 = CARTESIAN_POINT ( 'NONE',  ( -2.293366432827344421E-15, -12.48450537969573659, -135.4062500020483810 ) ) ;
#10241 = CARTESIAN_POINT ( 'NONE',  ( -5.405949406249996869, 9.363379034771805109, -145.0312500020483810 ) ) ;
#10242 = CARTESIAN_POINT ( 'NONE',  ( -5.405949406249996869, 9.363379034771805109, -191.5312500020484094 ) ) ;
#10243 = CARTESIAN_POINT ( 'NONE',  ( -9.999999999999998224, 1.224646799147353059E-15, -43.62500000409677625 ) ) ;
#10244 = CARTESIAN_POINT ( 'NONE',  ( 7.644554776091147741E-16, 12.48450537969573659, -83.46875000204838102 ) ) ;
#10245 = VERTEX_POINT ( 'NONE', #6439 ) ;
#10246 = CARTESIAN_POINT ( 'NONE',  ( -9.999999999999998224, 1.224646799147353059E-15, -56.74999999999996447 ) ) ;
#10247 = CARTESIAN_POINT ( 'NONE',  ( -10.81189881249999729, 1.324075727343319199E-15, -177.5937500020484094 ) ) ;
#10248 = CARTESIAN_POINT ( 'NONE',  ( -4.999999999999996447, 8.660254037844387298, -69.37500000409677625 ) ) ;
#10249 = ADVANCED_FACE ( 'NONE', ( #19582 ), #42668, .T. ) ;
#10250 = CARTESIAN_POINT ( 'NONE',  ( 4.999999999999992006, -8.660254037844389075, -109.1250000040967763 ) ) ;
#10251 = DIRECTION ( 'NONE',  ( -0.000000000000000000, -0.000000000000000000, -1.000000000000000000 ) ) ;
#10252 = CARTESIAN_POINT ( 'NONE',  ( -10.81189881249999907, -6.242252689847864744, -80.15625000204839523 ) ) ;
#10253 = CARTESIAN_POINT ( 'NONE',  ( -2.293366432827344421E-15, -12.48450537969573659, -55.90625000204837391 ) ) ;
#10254 =( BOUNDED_CURVE ( )  B_SPLINE_CURVE ( 2, ( #35990, #593, #30154, #9653, #13294, #13079, #10068 ),
 .UNSPECIFIED., .F., .F. ) 
 B_SPLINE_CURVE_WITH_KNOTS ( ( 3, 2, 2, 3 ),
 ( 0.1231343283582089221, 0.1243781094527362935, 0.1256218905472636649, 0.1268656716417910224 ),
 .UNSPECIFIED. ) 
 CURVE ( )  GEOMETRIC_REPRESENTATION_ITEM ( )  RATIONAL_B_SPLINE_CURVE ( ( 1.000000000000002887, 0.8660254037844355990, 1.000000000000000000, 0.8660254037844387076, 1.000000000000000000, 0.8660254037844417052, 0.9999999999999970024 ) ) 
 REPRESENTATION_ITEM ( '' )  );
#10255 = CARTESIAN_POINT ( 'NONE',  ( -9.999999999999998224, 1.224646799147353059E-15, -54.12500000409675494 ) ) ;
#10256 = CARTESIAN_POINT ( 'NONE',  ( 10.81189881249999551, -6.242252689847874514, -7.468750002048357928 ) ) ;
#10257 = CARTESIAN_POINT ( 'NONE',  ( 9.999999999999998224, 0.000000000000000000, -177.8750000040967905 ) ) ;
#10258 = CARTESIAN_POINT ( 'NONE',  ( -2.293366432827344421E-15, -12.48450537969573659, -183.4062500020483810 ) ) ;
#10259 = CARTESIAN_POINT ( 'NONE',  ( 10.81189881249999907, 6.242252689847868297, -8.906250002048366810 ) ) ;
#10260 = CARTESIAN_POINT ( 'NONE',  ( -9.999999999999998224, 1.224646799147353059E-15, -79.24999999999998579 ) ) ;
#10261 = CARTESIAN_POINT ( 'NONE',  ( 9.999999999999998224, 0.000000000000000000, -176.3750000040967905 ) ) ;
#10262 = CARTESIAN_POINT ( 'NONE',  ( 9.999999999999998224, 0.000000000000000000, -200.0000000000000000 ) ) ;
#10263 = CYLINDRICAL_SURFACE ( 'NONE', #27268, 9.999999999999998224 ) ;
#10264 =( BOUNDED_CURVE ( )  B_SPLINE_CURVE ( 2, ( #13129, #20262, #33449, #39265, #36877, #29560, #26536 ),
 .UNSPECIFIED., .F., .F. ) 
 B_SPLINE_CURVE_WITH_KNOTS ( ( 3, 2, 2, 3 ),
 ( 0.5783582089552241623, 0.5796019900497515476, 0.5808457711442788218, 0.5820895522388062071 ),
 .UNSPECIFIED. ) 
 CURVE ( )  GEOMETRIC_REPRESENTATION_ITEM ( )  RATIONAL_B_SPLINE_CURVE ( ( 0.9999999999999641398, 0.8660254037844745678, 1.000000000000000000, 0.8660254037844387076, 1.000000000000000000, 0.8660254037844148378, 1.000000000000023981 ) ) 
 REPRESENTATION_ITEM ( '' )  );
#10265 = CARTESIAN_POINT ( 'NONE',  ( 7.070501591499377789E-16, 11.54700538379251284, -166.6249999999999716 ) ) ;
#10266 = CARTESIAN_POINT ( 'NONE',  ( 4.999999999999992006, -8.660254037844389075, -62.24999999999997158 ) ) ;
#10268 = ORIENTED_EDGE ( 'NONE', *, *, #16204, .T. ) ;
#10267 = CARTESIAN_POINT ( 'NONE',  ( -10.81189881249999729, 1.324075727343319199E-15, -90.78125000204838102 ) ) ;
#10269 = CARTESIAN_POINT ( 'NONE',  ( 7.070501591499376803E-16, 11.54700538379251284, -107.0000000040967763 ) ) ;
#10271 = ORIENTED_EDGE ( 'NONE', *, *, #41214, .F. ) ;
#10270 = CARTESIAN_POINT ( 'NONE',  ( -9.999999999999998224, 1.224646799147353059E-15, -70.24999999999998579 ) ) ;
#10272 = ORIENTED_EDGE ( 'NONE', *, *, #14973, .T. ) ;
#10273 = CARTESIAN_POINT ( 'NONE',  ( -10.81189881249999907, -6.242252689847864744, -31.96875000204835970 ) ) ;
#10274 = CARTESIAN_POINT ( 'NONE',  ( 5.405949406249992428, -9.363379034771808662, -18.28125000204835970 ) ) ;
#10275 = AXIS2_PLACEMENT_3D ( 'NONE', #41128, #21294, #1459 ) ;
#10276 = CARTESIAN_POINT ( 'NONE',  ( -5.405949406250003975, -9.363379034771801557, -69.34375000204836681 ) ) ;
#10277 = CARTESIAN_POINT ( 'NONE',  ( -9.999999999999998224, 5.773502691896259087, -41.87499999999997158 ) ) ;
#10278 = CARTESIAN_POINT ( 'NONE',  ( 7.644554776091147741E-16, 12.48450537969573659, -195.9687500020484094 ) ) ;
#10279 = CARTESIAN_POINT ( 'NONE',  ( -10.81189881249999729, 6.242252689847871849, -152.2187500020483526 ) ) ;
#10280 = DIRECTION ( 'NONE',  ( 1.000000000000000000, 0.000000000000000000, 0.000000000000000000 ) ) ;
#10281 = VECTOR ( 'NONE', #11195, 1000.000000000000000 ) ;
#10282 = CARTESIAN_POINT ( 'NONE',  ( -99.99999999999994316, -40.00000000000000711, -160.0000000000000000 ) ) ;
#10283 = CARTESIAN_POINT ( 'NONE',  ( 10.81189881249999907, 6.242252689847868297, -148.4062500020484094 ) ) ;
#10284 = CARTESIAN_POINT ( 'NONE',  ( -2.121150477449813534E-15, -11.54700538379251284, -5.750000004096770923 ) ) ;
#10285 = CARTESIAN_POINT ( 'NONE',  ( -9.999999999999479527, -5.773502691896549521, -80.62499999999997158 ) ) ;
#10286 = CARTESIAN_POINT ( 'NONE',  ( -2.293366432827344421E-15, -12.48450537969573659, -121.7187500020483952 ) ) ;
#10287 = CARTESIAN_POINT ( 'NONE',  ( 7.070501591499376803E-16, 11.54700538379251284, -141.1250000000000000 ) ) ;
#10288 = CARTESIAN_POINT ( 'NONE',  ( -2.293366432827344421E-15, -12.48450537969573659, -93.40625000204839523 ) ) ;
#10289 = CARTESIAN_POINT ( 'NONE',  ( 10.81189881249999729, 6.242252689847867408, -106.2187500020483810 ) ) ;
#10290 = CARTESIAN_POINT ( 'NONE',  ( 5.405949406249992428, -9.363379034771808662, -73.59375000204838102 ) ) ;
#10291 = CARTESIAN_POINT ( 'NONE',  ( 5.405949406249992428, -9.363379034771808662, -73.78125000204838102 ) ) ;
#10292 = CARTESIAN_POINT ( 'NONE',  ( 7.070501591499377789E-16, 11.54700538379251284, -159.5000000040967905 ) ) ;
#10293 = CARTESIAN_POINT ( 'NONE',  ( 9.999999999999479527, 5.773502691896553074, -115.8749999999999858 ) ) ;
#10294 = CARTESIAN_POINT ( 'NONE',  ( -10.81189881249999729, 6.242252689847871849, -158.4062500020483810 ) ) ;
#10295 = CARTESIAN_POINT ( 'NONE',  ( 10.81189881249999551, -6.242252689847874514, -172.6562500020484379 ) ) ;
#10296 = DIRECTION ( 'NONE',  ( -1.000000000000000000, 0.000000000000000000, 0.000000000000000000 ) ) ;
#10297 = CARTESIAN_POINT ( 'NONE',  ( 10.81189881249999551, -6.242252689847874514, 0.03124999795164895566 ) ) ;
#10298 = CARTESIAN_POINT ( 'NONE',  ( 9.999999999999998224, 0.000000000000000000, -9.875000004096746054 ) ) ;
#10299 = CARTESIAN_POINT ( 'NONE',  ( -10.81189881249999729, 1.324075727343319199E-15, -104.0937500020483810 ) ) ;
#10300 = CARTESIAN_POINT ( 'NONE',  ( 10.00000000000000000, 5.773502691896255534, -79.87499999999998579 ) ) ;
#10301 = CARTESIAN_POINT ( 'NONE',  ( -5.405949406249996869, 9.363379034771805109, -8.531250002048352599 ) ) ;
#10302 = CARTESIAN_POINT ( 'NONE',  ( -9.999999999999998224, 1.224646799147353059E-15, -88.62500000409677625 ) ) ;
#10303 = CARTESIAN_POINT ( 'NONE',  ( -10.00000000000000000, -5.773502691896252870, -172.1250000000000284 ) ) ;
#10304 = CARTESIAN_POINT ( 'NONE',  ( 10.81189881249999907, 6.242252689847868297, -100.4062500020483952 ) ) ;
#10305 = CARTESIAN_POINT ( 'NONE',  ( -10.81189881249999729, 6.242252689847871849, -86.40625000204838102 ) ) ;
#10306 = ORIENTED_EDGE ( 'NONE', *, *, #33061, .F. ) ;
#10307 = CARTESIAN_POINT ( 'NONE',  ( -9.999999999999998224, 1.224646799147353059E-15, -82.62500000409676204 ) ) ;
#10308 = CARTESIAN_POINT ( 'NONE',  ( 7.070501591499376803E-16, 11.54700538379251284, -134.0000000040967905 ) ) ;
#10309 = CARTESIAN_POINT ( 'NONE',  ( -10.81189881249999729, 6.242252689847871849, -35.21875000204835260 ) ) ;
#10310 = ORIENTED_EDGE ( 'NONE', *, *, #35327, .T. ) ;
#10311 = CARTESIAN_POINT ( 'NONE',  ( -9.999999999999998224, 1.224646799147353059E-15, -5.749999999999976907 ) ) ;
#10312 = AXIS2_PLACEMENT_3D ( 'NONE', #4442, #27969, #30783 ) ;
#10313 = CARTESIAN_POINT ( 'NONE',  ( -10.81189881249999907, -6.242252689847864744, -35.15625000204835970 ) ) ;
#10314 = EDGE_CURVE ( 'NONE', #36340, #28518, #5802, .T. ) ;
#10315 = CARTESIAN_POINT ( 'NONE',  ( -5.000000000000003553, -8.660254037844383745, -148.0000000000000000 ) ) ;
#10316 = CARTESIAN_POINT ( 'NONE',  ( 10.00000000000102318, -5.773502691895667560, -32.12499999999992895 ) ) ;
#10317 = CARTESIAN_POINT ( 'NONE',  ( -10.00000000000000000, -5.773502691896251982, -13.50000000409676204 ) ) ;
#10318 = CARTESIAN_POINT ( 'NONE',  ( 9.999999999999996447, -5.773502691896262640, -194.1250000000000284 ) ) ;
#10319 = CYLINDRICAL_SURFACE ( 'NONE', #40610, 9.999999999999998224 ) ;
#10321 = ORIENTED_EDGE ( 'NONE', *, *, #27218, .F. ) ;
#10320 = CARTESIAN_POINT ( 'NONE',  ( 5.405949406249999534, 9.363379034771803333, -119.7812500020483952 ) ) ;
#10322 = DIRECTION ( 'NONE',  ( 1.000000000000000000, 0.000000000000000000, 0.000000000000000000 ) ) ;
#10323 = ORIENTED_EDGE ( 'NONE', *, *, #6971, .T. ) ;
#10324 = CARTESIAN_POINT ( 'NONE',  ( -10.81189881249999729, 1.324075727343319199E-15, -44.28125000204838102 ) ) ;
#10325 = PERSON_AND_ORGANIZATION_ROLE ( 'creator' ) ;
#10326 = CARTESIAN_POINT ( 'NONE',  ( 10.81189881249999729, 0.000000000000000000, -94.34375000204838102 ) ) ;
#10327 = CARTESIAN_POINT ( 'NONE',  ( -5.405949406249996869, 9.363379034771805109, -125.5312500020483952 ) ) ;
#10328 = ORIENTED_EDGE ( 'NONE', *, *, #41868, .T. ) ;
#10329 =( BOUNDED_CURVE ( )  B_SPLINE_CURVE ( 2, ( #24832, #8422, #34754, #31518, #1947, #15073, #28274 ),
 .UNSPECIFIED., .F., .F. ) 
 B_SPLINE_CURVE_WITH_KNOTS ( ( 3, 2, 2, 3 ),
 ( 0.5820895522388062071, 0.5833333333333335924, 0.5845771144278607556, 0.5858208955223881409 ),
 .UNSPECIFIED. ) 
 CURVE ( )  GEOMETRIC_REPRESENTATION_ITEM ( )  RATIONAL_B_SPLINE_CURVE ( ( 0.9999999999999761302, 0.8660254037844625774, 1.000000000000000000, 0.8660254037844387076, 1.000000000000000000, 0.8660254037844267172, 1.000000000000011990 ) ) 
 REPRESENTATION_ITEM ( '' )  );
#10330 = CARTESIAN_POINT ( 'NONE',  ( -9.999999999999998224, 1.224646799147353059E-15, -5.749999999999976907 ) ) ;
#10331 = CARTESIAN_POINT ( 'NONE',  ( -5.405949406249996869, 9.363379034771805109, -172.0312500020484094 ) ) ;
#10332 = CYLINDRICAL_SURFACE ( 'NONE', #32138, 9.999999999999998224 ) ;
#10333 = AXIS2_PLACEMENT_3D ( 'NONE', #27748, #40883, #34661 ) ;
#10334 = CARTESIAN_POINT ( 'NONE',  ( 10.81189881249999551, -6.242252689847874514, -131.9687500020483810 ) ) ;
#10335 = CARTESIAN_POINT ( 'NONE',  ( 5.405949406249992428, -9.363379034771808662, -96.09375000204838102 ) ) ;
#10336 = CARTESIAN_POINT ( 'NONE',  ( 9.999999999999998224, 0.000000000000000000, -43.99999999999998579 ) ) ;
#10337 = CARTESIAN_POINT ( 'NONE',  ( -10.81189881249999729, 1.324075727343319199E-15, -102.7812500020483952 ) ) ;
#10338 = CARTESIAN_POINT ( 'NONE',  ( 5.000000000000000000, 8.660254037844385522, -183.6250000040967905 ) ) ;
#10339 = CARTESIAN_POINT ( 'NONE',  ( -5.405949406249996869, 9.363379034771805109, -111.8437500020483810 ) ) ;
#10340 = CARTESIAN_POINT ( 'NONE',  ( -5.405949406250003975, -9.363379034771801557, -182.0312500020483810 ) ) ;
#10341 = CARTESIAN_POINT ( 'NONE',  ( -4.999999999999996447, 8.660254037844387298, -2.999999999999975131 ) ) ;
#10342 = CARTESIAN_POINT ( 'NONE',  ( 7.070501591499376803E-16, 11.54700538379251284, -181.6250000000000000 ) ) ;
#10343 = CARTESIAN_POINT ( 'NONE',  ( -10.81189881249999907, -6.242252689847864744, -198.6562500020484094 ) ) ;
#10344 = CARTESIAN_POINT ( 'NONE',  ( 10.81189881249999729, 6.242252689847867408, -62.71875000204839523 ) ) ;
#10345 = CARTESIAN_POINT ( 'NONE',  ( -5.405949406249996869, 9.363379034771805109, -41.34375000204837391 ) ) ;
#10346 = CARTESIAN_POINT ( 'NONE',  ( -4.999999999999996447, 8.660254037844387298, -183.3750000040967905 ) ) ;
#10347 = CARTESIAN_POINT ( 'NONE',  ( 10.81189881249999907, 6.242252689847868297, -20.90625000204836681 ) ) ;
#10348 = CARTESIAN_POINT ( 'NONE',  ( 5.405949406249999534, 9.363379034771803333, -26.59375000204835970 ) ) ;
#10349 = FACE_OUTER_BOUND ( 'NONE', #8261, .T. ) ;
#10350 = CARTESIAN_POINT ( 'NONE',  ( -10.81189881249999729, 6.242252689847871849, -126.7187500020483952 ) ) ;
#10351 = CARTESIAN_POINT ( 'NONE',  ( -2.121150477449813534E-15, -11.54700538379251284, -108.8749999999999858 ) ) ;
#10352 = CARTESIAN_POINT ( 'NONE',  ( 5.405949406249999534, 9.363379034771803333, -34.28125000204837391 ) ) ;
#10353 = CARTESIAN_POINT ( 'NONE',  ( 10.00000000000000000, 5.773502691896255534, -61.87499999999998579 ) ) ;
#10354 = CARTESIAN_POINT ( 'NONE',  ( -10.81189881249999729, 1.324075727343319199E-15, -134.2812500020483810 ) ) ;
#10355 = CARTESIAN_POINT ( 'NONE',  ( 10.81189881249999729, 0.000000000000000000, -108.0312500020483810 ) ) ;
#10356 = ORIENTED_EDGE ( 'NONE', *, *, #41809, .T. ) ;
#10357 = CARTESIAN_POINT ( 'NONE',  ( 0.000000000000000000, 0.000000000000000000, -219.9999999999999716 ) ) ;
#10358 = CARTESIAN_POINT ( 'NONE',  ( 4.999999999999992006, -8.660254037844389075, -112.1250000040967763 ) ) ;
#10359 = CARTESIAN_POINT ( 'NONE',  ( 10.81189881249999729, 0.000000000000000000, -62.84375000204836681 ) ) ;
#10360 = ORIENTED_EDGE ( 'NONE', *, *, #4119, .F. ) ;
#10361 = CARTESIAN_POINT ( 'NONE',  ( -4.999999999999996447, 8.660254037844387298, -29.99999999999997158 ) ) ;
#10362 = ADVANCED_FACE ( 'NONE', ( #28900 ), #12885, .T. ) ;
#10363 = ADVANCED_FACE ( 'NONE', ( #32356 ), #2780, .T. ) ;
#10364 = CARTESIAN_POINT ( 'NONE',  ( 5.405949406249992428, -9.363379034771808662, -31.78125000204837391 ) ) ;
#10365 = EDGE_CURVE ( 'NONE', #39621, #4388, #1185, .T. ) ;
#10366 = CARTESIAN_POINT ( 'NONE',  ( -5.000000000000003553, -8.660254037844383745, -35.87500000409676915 ) ) ;
#10367 = ADVANCED_FACE ( 'NONE', ( #24284 ), #3631, .F. ) ;
#10368 = CARTESIAN_POINT ( 'NONE',  ( -4.999999999999996447, 8.660254037844387298, -151.8750000040967905 ) ) ;
#10369 = CARTESIAN_POINT ( 'NONE',  ( -10.81189881249999907, -6.242252689847864744, -141.6562500020483810 ) ) ;
#10370 = APPROVAL ( #12809, 'UNSPECIFIED' ) ;
#10371 = CARTESIAN_POINT ( 'NONE',  ( 9.999999999999998224, 0.000000000000000000, -167.3750000040967905 ) ) ;
#10372 = ORIENTED_EDGE ( 'NONE', *, *, #24915, .F. ) ;
#10373 =( BOUNDED_CURVE ( )  B_SPLINE_CURVE ( 2, ( #35514, #29030, #9167, #8543, #21695, #2698, #2074 ),
 .UNSPECIFIED., .F., .F. ) 
 B_SPLINE_CURVE_WITH_KNOTS ( ( 3, 2, 2, 3 ),
 ( 0.3992537313432836799, 0.4004975124378110651, 0.4017412935323383949, 0.4029850746268657802 ),
 .UNSPECIFIED. ) 
 CURVE ( )  GEOMETRIC_REPRESENTATION_ITEM ( )  RATIONAL_B_SPLINE_CURVE ( ( 0.9999999999999880096, 0.8660254037844506980, 1.000000000000000000, 0.8660254037844387076, 1.000000000000000000, 0.8660254037844267172, 1.000000000000011990 ) ) 
 REPRESENTATION_ITEM ( '' )  );
#10374 = ORIENTED_EDGE ( 'NONE', *, *, #26094, .T. ) ;
#10375 = CARTESIAN_POINT ( 'NONE',  ( 5.000000000000000000, 8.660254037844385522, -114.2499999999999858 ) ) ;
#10376 = CARTESIAN_POINT ( 'NONE',  ( 0.000000000000000000, 0.000000000000000000, -200.0000000000000000 ) ) ;
#10377 = CARTESIAN_POINT ( 'NONE',  ( 10.81189881249999907, 6.242252689847868297, -163.2187500020483810 ) ) ;
#10378 = ADVANCED_FACE ( 'NONE', ( #34632, #27507 ), #13521, .F. ) ;
#10379 = CARTESIAN_POINT ( 'NONE',  ( 5.405949406249999534, 9.363379034771803333, -199.2812500020484094 ) ) ;
#10380 = CARTESIAN_POINT ( 'NONE',  ( -10.81189881249999729, 6.242252689847871849, -20.21875000204836326 ) ) ;
#10381 = CARTESIAN_POINT ( 'NONE',  ( 9.999999999999742428, 5.773502691896404748, -156.7500000040967905 ) ) ;
#10382 = CARTESIAN_POINT ( 'NONE',  ( -10.00000000000051337, 5.773502691895962435, -149.8750000000000000 ) ) ;
#10383 = CARTESIAN_POINT ( 'NONE',  ( 7.644554776091147741E-16, 12.48450537969573659, -155.4687500020484094 ) ) ;
#10384 = CARTESIAN_POINT ( 'NONE',  ( 10.81189881249999907, 6.242252689847868297, -139.2187500020484094 ) ) ;
#10385 = CARTESIAN_POINT ( 'NONE',  ( -9.999999999999998224, 1.224646799147353059E-15, -172.6250000040968189 ) ) ;
#10386 = CARTESIAN_POINT ( 'NONE',  ( 10.81189881249999729, 0.000000000000000000, -121.3437500020483952 ) ) ;
#10387 = CARTESIAN_POINT ( 'NONE',  ( -5.000000000000003553, -8.660254037844383745, -194.8750000040967905 ) ) ;
#10388 = CARTESIAN_POINT ( 'NONE',  ( 7.644554776091147741E-16, 12.48450537969573659, -133.1562500020483810 ) ) ;
#10389 = CARTESIAN_POINT ( 'NONE',  ( -10.81189881249999729, 1.324075727343319199E-15, -8.093750002048343717 ) ) ;
#10390 = CARTESIAN_POINT ( 'NONE',  ( 7.644554776091147741E-16, 12.48450537969573659, -137.4687500020483810 ) ) ;
#10391 = CARTESIAN_POINT ( 'NONE',  ( -9.999999999999998224, 1.224646799147353059E-15, -172.6250000040968189 ) ) ;
#10392 = CARTESIAN_POINT ( 'NONE',  ( -4.999999999999996447, 8.660254037844387298, -157.5000000000000000 ) ) ;
#10393 = CARTESIAN_POINT ( 'NONE',  ( -10.81189881249999907, -6.242252689847864744, -0.6562500020483587049 ) ) ;
#10394 = SECURITY_CLASSIFICATION ( '', '', #18567 ) ;
#10395 = CARTESIAN_POINT ( 'NONE',  ( 10.81189881249999551, -6.242252689847874514, -80.96875000204838102 ) ) ;
#10396 = CARTESIAN_POINT ( 'NONE',  ( -10.81189881249999729, 6.242252689847871849, -63.71875000204838102 ) ) ;
#10397 = CARTESIAN_POINT ( 'NONE',  ( -2.293366432827344421E-15, -12.48450537969573659, -40.90625000204836681 ) ) ;
#10398 = CARTESIAN_POINT ( 'NONE',  ( 7.644554776091147741E-16, 12.48450537969573659, -54.96875000204836681 ) ) ;
#10399 = CARTESIAN_POINT ( 'NONE',  ( 10.00000000000051159, -5.773502691895965988, -113.5000000040967620 ) ) ;
#10400 = CARTESIAN_POINT ( 'NONE',  ( 7.644554776091147741E-16, 12.48450537969573659, -159.9687500020483810 ) ) ;
#10401 = CARTESIAN_POINT ( 'NONE',  ( -10.00000000000000000, -5.773502691896251982, -128.6250000000000000 ) ) ;
#10402 = CARTESIAN_POINT ( 'NONE',  ( -10.81189881249999729, -6.242252689847864744, -138.6562500020484094 ) ) ;
#10403 = EDGE_CURVE ( 'NONE', #25696, #35021, #19162, .T. ) ;
#10404 = CARTESIAN_POINT ( 'NONE',  ( 10.00000000000154010, -5.773502691895370020, -23.50000000409674072 ) ) ;
#10405 = CARTESIAN_POINT ( 'NONE',  ( 7.070501591499377789E-16, 11.54700538379251284, -82.62500000000000000 ) ) ;
#10406 = CARTESIAN_POINT ( 'NONE',  ( 10.81189881249999551, -6.242252689847874514, -19.65625000204837391 ) ) ;
#10407 = ORIENTED_EDGE ( 'NONE', *, *, #16935, .T. ) ;
#10408 = CARTESIAN_POINT ( 'NONE',  ( 7.644554776091147741E-16, 12.48450537969573659, -112.1562500020483952 ) ) ;
#10409 = CARTESIAN_POINT ( 'NONE',  ( 7.070501591499377789E-16, 11.54700538379251284, -135.5000000040967905 ) ) ;
#10410 = CARTESIAN_POINT ( 'NONE',  ( 10.00000000000044764, -5.773502691896004180, -177.6249999999999716 ) ) ;
#10411 = CARTESIAN_POINT ( 'NONE',  ( -2.121150477449813534E-15, -11.54700538379251284, -44.75000000409676204 ) ) ;
#10412 = LINE ( 'NONE', #33104, #38688 ) ;
#10413 = CARTESIAN_POINT ( 'NONE',  ( -10.81189881249999907, -6.242252689847864744, -48.65625000204836681 ) ) ;
#10414 = CARTESIAN_POINT ( 'NONE',  ( 4.999999999999992006, -8.660254037844389075, -191.2500000000000000 ) ) ;
#10415 = CARTESIAN_POINT ( 'NONE',  ( -5.405949406249996869, 9.363379034771805109, -158.5312500020484094 ) ) ;
#10416 = CARTESIAN_POINT ( 'NONE',  ( -10.81189881249999729, 1.324075727343319199E-15, -137.0937500020483810 ) ) ;
#10417 = CARTESIAN_POINT ( 'NONE',  ( 7.071067811865472841, -7.071067811865472841, -200.0000000000000000 ) ) ;
#10418 = CARTESIAN_POINT ( 'NONE',  ( 4.999999999999992006, -8.660254037844389075, -115.1250000040967905 ) ) ;
#10419 = ORIENTED_EDGE ( 'NONE', *, *, #28886, .T. ) ;
#10420 = DIRECTION ( 'NONE',  ( -0.6123724356957962467, -0.3535533905932750631, 0.7071067811865454633 ) ) ;
#10421 = CC_DESIGN_APPROVAL ( #23300, ( #18005 ) ) ;
#10422 = EDGE_CURVE ( 'NONE', #33095, #795, #20008, .T. ) ;
#10424 = ORIENTED_EDGE ( 'NONE', *, *, #29872, .F. ) ;
#10423 = CARTESIAN_POINT ( 'NONE',  ( 10.81189881249999907, 6.242252689847868297, -61.40625000204838102 ) ) ;
#10425 = PERSON_AND_ORGANIZATION_ROLE ( 'creator' ) ;
#10427 = ORIENTED_EDGE ( 'NONE', *, *, #12999, .T. ) ;
#10426 = CARTESIAN_POINT ( 'NONE',  ( 10.81189881249999551, -6.242252689847874514, -115.4687500020483810 ) ) ;
#10428 = CARTESIAN_POINT ( 'NONE',  ( 10.81189881249999551, -6.242252689847874514, -20.96875000204836681 ) ) ;
#10429 = UNCERTAINTY_MEASURE_WITH_UNIT (LENGTH_MEASURE( 1.000000000000000082E-05 ), #23882, 'distance_accuracy_value', 'NONE');
#10430 = CARTESIAN_POINT ( 'NONE',  ( 10.81189881249999729, 0.000000000000000000, -194.8437500020484094 ) ) ;
#10431 = AXIS2_PLACEMENT_3D ( 'NONE', #16513, #33166, #16728 ) ;
#10432 = CARTESIAN_POINT ( 'NONE',  ( -10.81189881249999729, 6.242252689847871849, -50.21875000204836681 ) ) ;
#10433 = CARTESIAN_POINT ( 'NONE',  ( -8.659811548901195977, -5.000849327365069819, 0.000000000000000000 ) ) ;
#10434 = DIRECTION ( 'NONE',  ( -0.000000000000000000, -0.000000000000000000, 1.000000000000000000 ) ) ;
#10435 = CARTESIAN_POINT ( 'NONE',  ( -10.81189881249999729, 6.242252689847871849, -176.2187500020483810 ) ) ;
#10436 = CARTESIAN_POINT ( 'NONE',  ( -10.81189881249999907, -6.242252689847864744, -157.9687500020484379 ) ) ;
#10437 = CARTESIAN_POINT ( 'NONE',  ( 5.405949406249999534, 9.363379034771803333, -151.0937500020483810 ) ) ;
#10438 = CARTESIAN_POINT ( 'NONE',  ( -10.81189881249999729, 1.324075727343319199E-15, -159.5937500020484094 ) ) ;
#10439 = FACE_OUTER_BOUND ( 'NONE', #25934, .T. ) ;
#10440 = CARTESIAN_POINT ( 'NONE',  ( 0.000000000000000000, 0.000000000000000000, -99.99999999999998579 ) ) ;
#10441 = CARTESIAN_POINT ( 'NONE',  ( 5.000000000000000000, 8.660254037844385522, -177.2500000000000284 ) ) ;
#10442 = CARTESIAN_POINT ( 'NONE',  ( -5.405949406250003975, -9.363379034771801557, -96.34375000204838102 ) ) ;
#10443 = CARTESIAN_POINT ( 'NONE',  ( 9.999999999999998224, 0.000000000000000000, -183.5000000000000000 ) ) ;
#10444 = CARTESIAN_POINT ( 'NONE',  ( 5.405949406249992428, -9.363379034771808662, -67.78125000204838102 ) ) ;
#10445 = CARTESIAN_POINT ( 'NONE',  ( 4.999999999999992006, -8.660254037844389075, -97.12500000409677625 ) ) ;
#10446 = CARTESIAN_POINT ( 'NONE',  ( 5.405949406249999534, 9.363379034771803333, -182.5937500020483810 ) ) ;
#10447 = CARTESIAN_POINT ( 'NONE',  ( -2.293366432827344421E-15, -12.48450537969573659, -120.4062500020483952 ) ) ;
#10448 = CARTESIAN_POINT ( 'NONE',  ( 10.81189881249999729, 0.000000000000000000, -159.0312500020484094 ) ) ;
#10449 = CARTESIAN_POINT ( 'NONE',  ( -10.81189881249999729, 1.324075727343319199E-15, -56.28125000204836681 ) ) ;
#10450 = CARTESIAN_POINT ( 'NONE',  ( -4.999999999999996447, 8.660254037844387298, -138.3750000040967905 ) ) ;
#10451 = CARTESIAN_POINT ( 'NONE',  ( -9.999999999999998224, 1.224646799147353059E-15, -109.2499999999999858 ) ) ;
#10452 = AXIS2_PLACEMENT_3D ( 'NONE', #22039, #11663, #35000 ) ;
#10453 = ORIENTED_EDGE ( 'NONE', *, *, #34124, .T. ) ;
#10454 = CARTESIAN_POINT ( 'NONE',  ( -5.405949406250003975, -9.363379034771801557, -137.0312500020484094 ) ) ;
#10455 = CARTESIAN_POINT ( 'NONE',  ( 5.405949406249992428, -9.363379034771808662, -150.2812500020483810 ) ) ;
#10456 = CARTESIAN_POINT ( 'NONE',  ( 10.81189881249999729, 0.000000000000000000, -187.5312500020484094 ) ) ;
#10457 = CARTESIAN_POINT ( 'NONE',  ( -5.405949406250003975, -9.363379034771801557, -79.84375000204838102 ) ) ;
#10458 = VERTEX_POINT ( 'NONE', #17985 ) ;
#10459 = CARTESIAN_POINT ( 'NONE',  ( 9.999999999999998224, 0.000000000000000000, -48.49999999999998579 ) ) ;
#10460 = CARTESIAN_POINT ( 'NONE',  ( -10.81189881249999907, -6.242252689847864744, -183.4687500020484379 ) ) ;
#10461 = CARTESIAN_POINT ( 'NONE',  ( -2.121150477449813534E-15, -11.54700538379251284, -65.75000000409679046 ) ) ;
#10462 = CARTESIAN_POINT ( 'NONE',  ( 9.999999999999998224, 0.000000000000000000, -109.9999999999999858 ) ) ;
#10463 =( BOUNDED_CURVE ( )  B_SPLINE_CURVE ( 2, ( #6607, #42631, #13061, #26255, #39404, #9840, #32944 ),
 .UNSPECIFIED., .F., .F. ) 
 B_SPLINE_CURVE_WITH_KNOTS ( ( 3, 2, 2, 3 ),
 ( 0.7985074626865673597, 0.7997512437810947450, 0.8009950248756220192, 0.8022388059701494045 ),
 .UNSPECIFIED. ) 
 CURVE ( )  GEOMETRIC_REPRESENTATION_ITEM ( )  RATIONAL_B_SPLINE_CURVE ( ( 0.9999999999999761302, 0.8660254037844625774, 1.000000000000000000, 0.8660254037844387076, 1.000000000000000000, 0.8660254037844267172, 1.000000000000011990 ) ) 
 REPRESENTATION_ITEM ( '' )  );
#10464 = CARTESIAN_POINT ( 'NONE',  ( -10.81189881249999907, -6.242252689847864744, -77.15625000204836681 ) ) ;
#10465 = CARTESIAN_POINT ( 'NONE',  ( -10.81189881249999729, 1.324075727343319199E-15, -62.28125000204837391 ) ) ;
#10466 = CARTESIAN_POINT ( 'NONE',  ( -9.999999999999998224, 5.773502691896259087, -54.25000000409676915 ) ) ;
#10467 = CARTESIAN_POINT ( 'NONE',  ( -5.405949406249996869, 9.363379034771805109, -6.843750002048371250 ) ) ;
#10468 = CARTESIAN_POINT ( 'NONE',  ( 25.00000000000000000, 3.061616997868383043E-15, -160.0000000000000000 ) ) ;
#10469 = CARTESIAN_POINT ( 'NONE',  ( -5.405949406249996869, 9.363379034771805109, -185.5312500020484094 ) ) ;
#10470 = AXIS2_PLACEMENT_3D ( 'NONE', #22539, #29230, #3324 ) ;
#10471 = CARTESIAN_POINT ( 'NONE',  ( 10.81189881249999907, 6.242252689847868297, -7.406250002048365033 ) ) ;
#10472 = FACE_OUTER_BOUND ( 'NONE', #1427, .T. ) ;
#10473 = CARTESIAN_POINT ( 'NONE',  ( 9.999999999999998224, 0.000000000000000000, -88.99999999999998579 ) ) ;
#10474 = CYLINDRICAL_SURFACE ( 'NONE', #13481, 9.999999999999998224 ) ;
#10475 = CARTESIAN_POINT ( 'NONE',  ( 9.999999999999998224, 0.000000000000000000, -200.0000000000000000 ) ) ;
#10477 = EDGE_LOOP ( 'NONE', ( #13499, #30624, #25365, #5091 ) ) ;
#10476 = CARTESIAN_POINT ( 'NONE',  ( 5.405949406249992428, -9.363379034771808662, -90.28125000204838102 ) ) ;
#10478 = CARTESIAN_POINT ( 'NONE',  ( -2.121150477449813534E-15, -11.54700538379251284, -162.8750000000000000 ) ) ;
#10480 = VERTEX_POINT ( 'NONE', #11511 ) ;
#10479 = DIRECTION ( 'NONE',  ( 1.000000000000000000, 0.000000000000000000, 0.000000000000000000 ) ) ;
#10481 = ORIENTED_EDGE ( 'NONE', *, *, #10010, .T. ) ;
#10482 = AXIS2_PLACEMENT_3D ( 'NONE', #15050, #5151, #7960 ) ;
#10483 = CARTESIAN_POINT ( 'NONE',  ( 10.81189881249999551, -6.242252689847874514, -22.46875000204837391 ) ) ;
#10484 = CARTESIAN_POINT ( 'NONE',  ( 10.81189881249999907, 6.242252689847868297, -22.40625000204837747 ) ) ;
#10485 = SECURITY_CLASSIFICATION_LEVEL ( 'unclassified' ) ;
#10486 = CARTESIAN_POINT ( 'NONE',  ( -10.81189881249999729, 6.242252689847871849, -68.21875000204838102 ) ) ;
#10487 = CARTESIAN_POINT ( 'NONE',  ( 0.000000000000000000, 0.000000000000000000, -200.0000000000000000 ) ) ;
#10488 = CARTESIAN_POINT ( 'NONE',  ( 9.999999999999998224, 0.000000000000000000, -48.49999999999998579 ) ) ;
#10489 = CARTESIAN_POINT ( 'NONE',  ( -10.81189881249999907, -6.242252689847864744, -195.4687500020484094 ) ) ;
#10490 = CARTESIAN_POINT ( 'NONE',  ( -5.405949406250003975, -9.363379034771801557, -150.3437500020483810 ) ) ;
#10491 = EDGE_CURVE ( 'NONE', #27538, #8850, #31396, .T. ) ;
#10492 = CARTESIAN_POINT ( 'NONE',  ( 7.070501591499376803E-16, 11.54700538379251284, -72.50000000409677625 ) ) ;
#10493 = CARTESIAN_POINT ( 'NONE',  ( 9.999999999999998224, 0.000000000000000000, -132.8750000040967905 ) ) ;
#10494 = CARTESIAN_POINT ( 'NONE',  ( -10.81189881249999907, -6.242252689847864744, -150.6562500020484094 ) ) ;
#10495 = CARTESIAN_POINT ( 'NONE',  ( -9.999999999999998224, 1.224646799147353059E-15, -4.625000004096769146 ) ) ;
#10496 = CARTESIAN_POINT ( 'NONE',  ( -9.999999999999998224, 1.224646799147353059E-15, -200.0000000000000000 ) ) ;
#10497 = CARTESIAN_POINT ( 'NONE',  ( 7.644554776091147741E-16, 12.48450537969573659, -119.4687500020483952 ) ) ;
#10498 = DIRECTION ( 'NONE',  ( 1.000000000000000000, 0.000000000000000000, 0.000000000000000000 ) ) ;
#10499 = CARTESIAN_POINT ( 'NONE',  ( 5.405949406249999534, 9.363379034771803333, -88.28125000204838102 ) ) ;
#10500 = CARTESIAN_POINT ( 'NONE',  ( -10.81189881249999729, 6.242252689847871849, -102.7187500020483810 ) ) ;
#10501 = CARTESIAN_POINT ( 'NONE',  ( -2.293366432827344421E-15, -12.48450537969573659, -73.71875000204835260 ) ) ;
#10502 = CARTESIAN_POINT ( 'NONE',  ( -10.81189881249999907, -6.242252689847864744, -74.15625000204835260 ) ) ;
#10503 = CARTESIAN_POINT ( 'NONE',  ( -4.999999999999996447, 8.660254037844387298, -160.8750000040967905 ) ) ;
#10504 =( BOUNDED_CURVE ( )  B_SPLINE_CURVE ( 2, ( #4802, #37396, #7839, #34814, #20986, #4591, #11265 ),
 .UNSPECIFIED., .F., .F. ) 
 B_SPLINE_CURVE_WITH_KNOTS ( ( 3, 2, 2, 3 ),
 ( 0.2537313432835822113, 0.2549751243781095411, 0.2562189054726369264, 0.2574626865671643117 ),
 .UNSPECIFIED. ) 
 CURVE ( )  GEOMETRIC_REPRESENTATION_ITEM ( )  RATIONAL_B_SPLINE_CURVE ( ( 0.9999999999999880096, 0.8660254037844506980, 1.000000000000000000, 0.8660254037844387076, 1.000000000000000000, 0.8660254037844267172, 1.000000000000011990 ) ) 
 REPRESENTATION_ITEM ( '' )  );
#10505 = CARTESIAN_POINT ( 'NONE',  ( -5.405949406250003975, -9.363379034771801557, -158.0312500020484094 ) ) ;
#10506 = CARTESIAN_POINT ( 'NONE',  ( 5.405949406249999534, 9.363379034771803333, -173.7812500020484094 ) ) ;
#10507 = CARTESIAN_POINT ( 'NONE',  ( -9.999999999999998224, 1.224646799147353059E-15, -136.6250000040967620 ) ) ;
#10508 = FACE_OUTER_BOUND ( 'NONE', #24152, .T. ) ;
#10509 = CARTESIAN_POINT ( 'NONE',  ( 9.999999999999998224, 0.000000000000000000, -79.99999999999998579 ) ) ;
#10510 = CARTESIAN_POINT ( 'NONE',  ( -10.81189881249999729, 6.242252689847871849, -102.7187500020483810 ) ) ;
#10511 = CARTESIAN_POINT ( 'NONE',  ( -10.00000000000000000, -5.773502691896251982, -79.12499999999998579 ) ) ;
#10512 = CARTESIAN_POINT ( 'NONE',  ( 5.405949406249999534, 9.363379034771803333, -2.781250002048374359 ) ) ;
#10513 = CARTESIAN_POINT ( 'NONE',  ( -5.000000000000003553, -8.660254037844383745, -86.87500000409677625 ) ) ;
#10514 = DIRECTION ( 'NONE',  ( -0.000000000000000000, -0.000000000000000000, 1.000000000000000000 ) ) ;
#10515 = CARTESIAN_POINT ( 'NONE',  ( -10.81189881249999729, 1.324075727343319199E-15, -102.7812500020483952 ) ) ;
#10516 = CARTESIAN_POINT ( 'NONE',  ( -5.405949406249996869, 9.363379034771805109, -80.53125000204838102 ) ) ;
#10517 =( BOUNDED_CURVE ( )  B_SPLINE_CURVE ( 2, ( #647, #9910, #33659, #39686, #22878, #30425, #26745 ),
 .UNSPECIFIED., .F., .F. ) 
 B_SPLINE_CURVE_WITH_KNOTS ( ( 3, 2, 2, 3 ),
 ( 0.3320895522388061516, 0.3333333333333334259, 0.3345771144278607556, 0.3358208955223880854 ),
 .UNSPECIFIED. ) 
 CURVE ( )  GEOMETRIC_REPRESENTATION_ITEM ( )  RATIONAL_B_SPLINE_CURVE ( ( 0.9999999999999820144, 0.8660254037844566932, 1.000000000000000000, 0.8660254037844387076, 1.000000000000000000, 0.8660254037844387076, 1.000000000000000000 ) ) 
 REPRESENTATION_ITEM ( '' )  );
#10518 = CARTESIAN_POINT ( 'NONE',  ( -10.00000000000000000, -5.773502691896251982, -73.50000000409674783 ) ) ;
#10519 = DIRECTION ( 'NONE',  ( 0.000000000000000000, -0.000000000000000000, -1.000000000000000000 ) ) ;
#10520 = CARTESIAN_POINT ( 'NONE',  ( 5.405949406249992428, -9.363379034771808662, -31.59375000204836681 ) ) ;
#10521 = ORIENTED_EDGE ( 'NONE', *, *, #2444, .T. ) ;
#10522 = CARTESIAN_POINT ( 'NONE',  ( 5.000000000000000000, 8.660254037844385522, -12.24999999999995559 ) ) ;
#10523 = ADVANCED_FACE ( 'NONE', ( #39646 ), #30968, .F. ) ;
#10524 = CARTESIAN_POINT ( 'NONE',  ( 10.81189881249999729, 0.000000000000000000, -27.03125000204836681 ) ) ;
#10525 = CARTESIAN_POINT ( 'NONE',  ( -9.999999999999998224, 5.773502691896259087, -145.3750000000000000 ) ) ;
#10526 = DIRECTION ( 'NONE',  ( -0.000000000000000000, -0.000000000000000000, 1.000000000000000000 ) ) ;
#10527 = CARTESIAN_POINT ( 'NONE',  ( -4.999999999999996447, 8.660254037844387298, -3.375000004096767370 ) ) ;
#10528 = ADVANCED_FACE ( 'NONE', ( #29959 ), #11083, .F. ) ;
#10529 = CARTESIAN_POINT ( 'NONE',  ( 4.999999999999992006, -8.660254037844389075, -192.7500000000000000 ) ) ;
#10530 = CARTESIAN_POINT ( 'NONE',  ( 4.999999999999992006, -8.660254037844389075, -155.6250000040967905 ) ) ;
#10532 = ORIENTED_EDGE ( 'NONE', *, *, #33338, .F. ) ;
#10531 = CARTESIAN_POINT ( 'NONE',  ( -10.81189881249999729, 6.242252689847871849, -114.9062500020483952 ) ) ;
#10533 = ORIENTED_EDGE ( 'NONE', *, *, #32563, .F. ) ;
#10534 = VERTEX_POINT ( 'NONE', #14307 ) ;
#10535 = CARTESIAN_POINT ( 'NONE',  ( 10.81189881249999907, 6.242252689847868297, -47.90625000204836681 ) ) ;
#10536 = PERSON_AND_ORGANIZATION ( #11915, #17965 ) ;
#10537 = CARTESIAN_POINT ( 'NONE',  ( -10.81189881249999729, 1.324075727343319199E-15, -95.09375000204838102 ) ) ;
#10538 = CARTESIAN_POINT ( 'NONE',  ( 10.81189881249999729, 0.000000000000000000, -121.5312500020483952 ) ) ;
#10539 = VERTEX_POINT ( 'NONE', #24713 ) ;
#10540 = CARTESIAN_POINT ( 'NONE',  ( 5.000000000000002665, 20.00000000000000000, -219.9999999999999716 ) ) ;
#10541 = CARTESIAN_POINT ( 'NONE',  ( 5.405949406249992428, -9.363379034771808662, -198.0937500020484094 ) ) ;
#10542 = CARTESIAN_POINT ( 'NONE',  ( -10.81189881249999729, 6.242252689847871849, -168.9062500020483810 ) ) ;
#10543 = LINE ( 'NONE', #23521, #9381 ) ;
#10544 = ADVANCED_FACE ( 'NONE', ( #7872 ), #40641, .F. ) ;
#10545 = CARTESIAN_POINT ( 'NONE',  ( -10.81189881249999729, 6.242252689847871849, -120.7187500020483952 ) ) ;
#10546 = CARTESIAN_POINT ( 'NONE',  ( -10.81189881249999729, 1.324075727343319199E-15, -93.59375000204838102 ) ) ;
#10547 = CARTESIAN_POINT ( 'NONE',  ( 10.81189881249999907, 6.242252689847868297, -199.2187500020484094 ) ) ;
#10548 = CARTESIAN_POINT ( 'NONE',  ( 10.81189881249999907, 6.242252689847868297, -97.40625000204839523 ) ) ;
#10549 = CARTESIAN_POINT ( 'NONE',  ( 4.999999999999992006, -8.660254037844389075, -182.6250000040967905 ) ) ;
#10550 = CARTESIAN_POINT ( 'NONE',  ( 5.405949406249999534, 9.363379034771803333, -106.0937500020483810 ) ) ;
#10551 = CARTESIAN_POINT ( 'NONE',  ( 5.405949406249999534, 9.363379034771803333, -179.7812500020484094 ) ) ;
#10552 = CARTESIAN_POINT ( 'NONE',  ( 10.00000000000051159, -5.773502691895965988, -104.5000000040967620 ) ) ;
#10553 = CARTESIAN_POINT ( 'NONE',  ( 7.644554776091147741E-16, 12.48450537969573659, -199.1562500020484094 ) ) ;
#10554 = CARTESIAN_POINT ( 'NONE',  ( 5.405949406249992428, -9.363379034771808662, -58.59375000204835970 ) ) ;
#10555 = CARTESIAN_POINT ( 'NONE',  ( 5.405949406249999534, 9.363379034771803333, -40.09375000204837391 ) ) ;
#10556 = CARTESIAN_POINT ( 'NONE',  ( -10.00000000000000000, -5.773502691896251982, -174.0000000040967905 ) ) ;
#10557 = CARTESIAN_POINT ( 'NONE',  ( 5.405949406249992428, -9.363379034771808662, -15.28125000204835793 ) ) ;
#10558 = CARTESIAN_POINT ( 'NONE',  ( -2.293366432827344421E-15, -12.48450537969573659, -21.21875000204837036 ) ) ;
#10559 = DIRECTION ( 'NONE',  ( -0.000000000000000000, -0.000000000000000000, 1.000000000000000000 ) ) ;
#10560 = CARTESIAN_POINT ( 'NONE',  ( 7.644554776091147741E-16, 12.48450537969573659, -132.9687500020483810 ) ) ;
#10561 = CARTESIAN_POINT ( 'NONE',  ( 4.999999999999992006, -8.660254037844389075, -104.2499999999999858 ) ) ;
#10562 = CARTESIAN_POINT ( 'NONE',  ( 5.405949406249992428, -9.363379034771808662, -30.28125000204837036 ) ) ;
#10563 = LINE ( 'NONE', #7779, #33461 ) ;
#10564 = CARTESIAN_POINT ( 'NONE',  ( 4.999999999999992006, -8.660254037844389075, -57.74999999999997158 ) ) ;
#10565 = CARTESIAN_POINT ( 'NONE',  ( 10.81189881249999729, 0.000000000000000000, -126.0312500020483952 ) ) ;
#10566 = CARTESIAN_POINT ( 'NONE',  ( -10.81189881249999729, 1.324075727343319199E-15, -108.7812500020483810 ) ) ;
#10567 = ORIENTED_EDGE ( 'NONE', *, *, #17511, .T. ) ;
#10568 = CARTESIAN_POINT ( 'NONE',  ( -9.999999999999998224, 1.224646799147353059E-15, -7.249999999999978684 ) ) ;
#10569 = CARTESIAN_POINT ( 'NONE',  ( 5.000000000000000000, 8.660254037844385522, -99.62500000409679046 ) ) ;
#10570 = CARTESIAN_POINT ( 'NONE',  ( 9.999999999999994671, -5.773502691896262640, -136.0000000040967905 ) ) ;
#10571 = CARTESIAN_POINT ( 'NONE',  ( 10.81189881249999551, -6.242252689847874514, -55.46875000204837391 ) ) ;
#10572 = ORIENTED_EDGE ( 'NONE', *, *, #35256, .F. ) ;
#10573 = CARTESIAN_POINT ( 'NONE',  ( -9.999999999999998224, 1.224646799147353059E-15, -35.74999999999997868 ) ) ;
#10574 = CARTESIAN_POINT ( 'NONE',  ( -10.81189881249999729, 6.242252689847871849, -38.40625000204835260 ) ) ;
#10575 = CARTESIAN_POINT ( 'NONE',  ( 0.000000000000000000, 0.000000000000000000, -99.99999999999998579 ) ) ;
#10576 = CARTESIAN_POINT ( 'NONE',  ( -9.999999999999998224, 1.224646799147353059E-15, -39.12500000409676915 ) ) ;
#10577 = PLANE ( 'NONE',  #12775 ) ;
#10578 = CARTESIAN_POINT ( 'NONE',  ( -10.81189881249999729, 1.324075727343319199E-15, -144.7812500020483810 ) ) ;
#10579 =( BOUNDED_CURVE ( )  B_SPLINE_CURVE ( 2, ( #37013, #20602, #986, #26667, #27305, #20387, #20818 ),
 .UNSPECIFIED., .F., .F. ) 
 B_SPLINE_CURVE_WITH_KNOTS ( ( 3, 2, 2, 3 ),
 ( 0.1007462686567163757, 0.1019900497512437887, 0.1032338308457712017, 0.1044776119402986148 ),
 .UNSPECIFIED. ) 
 CURVE ( )  GEOMETRIC_REPRESENTATION_ITEM ( )  RATIONAL_B_SPLINE_CURVE ( ( 1.000000000000004441, 0.8660254037844342667, 1.000000000000000000, 0.8660254037844387076, 1.000000000000000000, 0.8660254037844267172, 1.000000000000011990 ) ) 
 REPRESENTATION_ITEM ( '' )  );
#10580 = CARTESIAN_POINT ( 'NONE',  ( -10.00000000000012434, 5.773502691896184480, -166.7500000040967905 ) ) ;
#10581 = ORIENTED_EDGE ( 'NONE', *, *, #33908, .T. ) ;
#10582 = ORIENTED_EDGE ( 'NONE', *, *, #38051, .T. ) ;
#10583 = CARTESIAN_POINT ( 'NONE',  ( -10.00000000000012434, 5.773502691896184480, -158.8750000000000000 ) ) ;
#10584 = LINE ( 'NONE', #36926, #22172 ) ;
#10585 = CARTESIAN_POINT ( 'NONE',  ( 10.81189881249999551, -6.242252689847874514, -169.4687500020483810 ) ) ;
#10586 = CARTESIAN_POINT ( 'NONE',  ( 5.405949406249999534, 9.363379034771803333, -197.7812500020484094 ) ) ;
#10587 = EDGE_CURVE ( 'NONE', #41907, #28187, #2914, .T. ) ;
#10588 = CARTESIAN_POINT ( 'NONE',  ( 10.81189881249999551, -6.242252689847874514, -17.96875000204837036 ) ) ;
#10589 = DIRECTION ( 'NONE',  ( -1.000000000000000000, 0.000000000000000000, 0.000000000000000000 ) ) ;
#10590 = ADVANCED_FACE ( 'NONE', ( #4412 ), #22716, .T. ) ;
#10591 = CARTESIAN_POINT ( 'NONE',  ( -5.405949406250003975, -9.363379034771801557, -157.8437500020483810 ) ) ;
#10592 = CARTESIAN_POINT ( 'NONE',  ( 10.81189881249999729, 0.000000000000000000, -136.3437500020484094 ) ) ;
#10593 = ADVANCED_FACE ( 'NONE', ( #17772 ), #1398, .F. ) ;
#10594 = CARTESIAN_POINT ( 'NONE',  ( -9.999999999999479527, -5.773502691896549521, -119.6249999999999858 ) ) ;
#10595 = CARTESIAN_POINT ( 'NONE',  ( 10.81189881249999729, 0.000000000000000000, -113.8437500020483810 ) ) ;
#10596 = CARTESIAN_POINT ( 'NONE',  ( 10.00000000000000000, 5.773502691896255534, -197.2500000040968189 ) ) ;
#10597 = CARTESIAN_POINT ( 'NONE',  ( 10.81189881249999907, 6.242252689847868297, -125.9062500020483810 ) ) ;
#10598 = CARTESIAN_POINT ( 'NONE',  ( -2.293366432827344421E-15, -12.48450537969573659, -9.218750002048359704 ) ) ;
#10599 = CARTESIAN_POINT ( 'NONE',  ( 5.405949406249992428, -9.363379034771808662, -139.5937500020483810 ) ) ;
#10600 = CARTESIAN_POINT ( 'NONE',  ( 0.000000000000000000, 0.000000000000000000, -200.0000000000000000 ) ) ;
#10601 = CARTESIAN_POINT ( 'NONE',  ( 10.00000000000000000, 5.773502691896255534, -156.3749999999999716 ) ) ;
#10602 = CARTESIAN_POINT ( 'NONE',  ( -5.000000000000003553, -8.660254037844383745, -18.99999999999996092 ) ) ;
#10603 = CARTESIAN_POINT ( 'NONE',  ( -10.81189881249999729, 6.242252689847871849, -84.71875000204836681 ) ) ;
#10604 = CARTESIAN_POINT ( 'NONE',  ( 7.644554776091147741E-16, 12.48450537969573659, -65.46875000204836681 ) ) ;
#10605 = CARTESIAN_POINT ( 'NONE',  ( -9.999999999999998224, 1.224646799147353059E-15, -118.6250000040967905 ) ) ;
#10606 = CARTESIAN_POINT ( 'NONE',  ( -5.405949406250003975, -9.363379034771801557, -44.03125000204838102 ) ) ;
#10607 = CARTESIAN_POINT ( 'NONE',  ( -5.405949406250003975, -9.363379034771801557, -46.84375000204838102 ) ) ;
#10608 = LINE ( 'NONE', #13838, #28881 ) ;
#10609 = CARTESIAN_POINT ( 'NONE',  ( -5.405949406249996869, 9.363379034771805109, -150.8437500020483810 ) ) ;
#10610 = CARTESIAN_POINT ( 'NONE',  ( -9.999999999999998224, 1.224646799147353059E-15, -133.2499999999999716 ) ) ;
#10611 = CARTESIAN_POINT ( 'NONE',  ( -10.81189881249999729, -6.242252689847864744, -131.1562500020483810 ) ) ;
#10612 = CARTESIAN_POINT ( 'NONE',  ( 10.70731569305653252, 1.500182182591227154, -180.0000000000000284 ) ) ;
#10613 = CARTESIAN_POINT ( 'NONE',  ( 9.999999999999998224, 0.000000000000000000, -81.49999999999998579 ) ) ;
#10614 = CARTESIAN_POINT ( 'NONE',  ( 10.81189881249999729, 6.242252689847867408, -20.90625000204836681 ) ) ;
#10615 = VERTEX_POINT ( 'NONE', #15599 ) ;
#10616 = CARTESIAN_POINT ( 'NONE',  ( -5.405949406249996869, 9.363379034771805109, -113.5312500020483952 ) ) ;
#10617 = CARTESIAN_POINT ( 'NONE',  ( -9.999999999999998224, 5.773502691896259087, -129.2500000040967905 ) ) ;
#10618 = DIRECTION ( 'NONE',  ( -0.000000000000000000, -0.000000000000000000, 1.000000000000000000 ) ) ;
#10619 = CARTESIAN_POINT ( 'NONE',  ( -9.999999999999998224, 5.773502691896259087, -43.75000000409676204 ) ) ;
#10620 = EDGE_CURVE ( 'NONE', #5685, #8492, #31701, .T. ) ;
#10621 = CARTESIAN_POINT ( 'NONE',  ( -9.999999999999998224, 1.224646799147353059E-15, -43.62500000409677625 ) ) ;
#10622 = CARTESIAN_POINT ( 'NONE',  ( -2.293366432827344421E-15, -12.48450537969573659, -48.40625000204838102 ) ) ;
#10623 =( BOUNDED_CURVE ( )  B_SPLINE_CURVE ( 2, ( #37586, #1559, #17710, #14032, #14690, #30905, #27879 ),
 .UNSPECIFIED., .F., .F. ) 
 B_SPLINE_CURVE_WITH_KNOTS ( ( 3, 2, 2, 3 ),
 ( 0.7201492537313435305, 0.7213930348258709158, 0.7226368159203983010, 0.7238805970149256863 ),
 .UNSPECIFIED. ) 
 CURVE ( )  GEOMETRIC_REPRESENTATION_ITEM ( )  RATIONAL_B_SPLINE_CURVE ( ( 0.9999999999999761302, 0.8660254037844625774, 1.000000000000000000, 0.8660254037844387076, 1.000000000000000000, 0.8660254037844028474, 1.000000000000035971 ) ) 
 REPRESENTATION_ITEM ( '' )  );
#10624 = DIRECTION ( 'NONE',  ( -0.000000000000000000, -0.000000000000000000, -1.000000000000000000 ) ) ;
#10625 = CARTESIAN_POINT ( 'NONE',  ( 5.405949406249999534, 9.363379034771803333, -149.7812500020483810 ) ) ;
#10626 = CARTESIAN_POINT ( 'NONE',  ( -2.293366432827344421E-15, -12.48450537969573659, -133.7187500020483810 ) ) ;
#10627 = CARTESIAN_POINT ( 'NONE',  ( 0.000000000000000000, 0.000000000000000000, -223.0000000000000000 ) ) ;
#10628 = ADVANCED_FACE ( 'NONE', ( #31832 ), #38072, .F. ) ;
#10629 = VERTEX_POINT ( 'NONE', #25348 ) ;
#10630 = DIRECTION ( 'NONE',  ( -0.8660254037844439257, 0.000000000000000000, 0.4999999999999907296 ) ) ;
#10631 = EDGE_LOOP ( 'NONE', ( #10119, #3876, #2758, #8867 ) ) ;
#10633 = VERTEX_POINT ( 'NONE', #2676 ) ;
#10632 = CARTESIAN_POINT ( 'NONE',  ( -5.405949406250003975, -9.363379034771801557, -60.53125000204836681 ) ) ;
#10634 = APPROVAL_STATUS ( 'not_yet_approved' ) ;
#10636 = ORIENTED_EDGE ( 'NONE', *, *, #22174, .F. ) ;
#10635 = CARTESIAN_POINT ( 'NONE',  ( 5.405949406249992428, -9.363379034771808662, -111.0937500020483810 ) ) ;
#10637 = CARTESIAN_POINT ( 'NONE',  ( -10.81189881249999729, 1.324075727343319199E-15, -18.59375000204835260 ) ) ;
#10638 = CARTESIAN_POINT ( 'NONE',  ( 10.81189881249999551, -6.242252689847874514, -191.9687500020484379 ) ) ;
#10639 = CARTESIAN_POINT ( 'NONE',  ( 10.81189881249999729, 0.000000000000000000, -50.84375000204835260 ) ) ;
#10640 = DIRECTION ( 'NONE',  ( -0.000000000000000000, -0.000000000000000000, -1.000000000000000000 ) ) ;
#10641 = CARTESIAN_POINT ( 'NONE',  ( -5.000000000000003553, -8.660254037844383745, -31.37500000409676559 ) ) ;
#10642 = CARTESIAN_POINT ( 'NONE',  ( -10.81189881249999729, 6.242252689847871849, -179.2187500020484379 ) ) ;
#10643 = CARTESIAN_POINT ( 'NONE',  ( 10.81189881249999729, 0.000000000000000000, -163.3437500020484094 ) ) ;
#10644 = CARTESIAN_POINT ( 'NONE',  ( 5.405949406249999534, 9.363379034771803333, -139.0937500020483810 ) ) ;
#10646 = EDGE_CURVE ( 'NONE', #37675, #3284, #18021, .T. ) ;
#10645 = CARTESIAN_POINT ( 'NONE',  ( 10.81189881249999729, 0.000000000000000000, -158.8437500020483810 ) ) ;
#10647 = CARTESIAN_POINT ( 'NONE',  ( 10.00000000000051159, -5.773502691895965988, -93.62499999999997158 ) ) ;
#10648 = CYLINDRICAL_SURFACE ( 'NONE', #10880, 9.999999999999998224 ) ;
#10649 = CARTESIAN_POINT ( 'NONE',  ( 10.00000000000000000, 5.773502691896255534, -177.3750000000000000 ) ) ;
#10650 = EDGE_CURVE ( 'NONE', #3605, #41097, #29887, .T. ) ;
#10651 = CARTESIAN_POINT ( 'NONE',  ( -5.405949406249996869, 9.363379034771805109, -92.34375000204838102 ) ) ;
#10652 = CARTESIAN_POINT ( 'NONE',  ( 9.999999999999998224, 0.000000000000000000, -100.9999999999999858 ) ) ;
#10653 = CARTESIAN_POINT ( 'NONE',  ( 10.81189881249999551, -6.242252689847874514, -69.15625000204839523 ) ) ;
#10654 = CARTESIAN_POINT ( 'NONE',  ( 0.000000000000000000, 0.000000000000000000, -200.0000000000000000 ) ) ;
#10655 = CARTESIAN_POINT ( 'NONE',  ( 10.81189881249999907, 6.242252689847868297, -178.2187500020483810 ) ) ;
#10656 = CARTESIAN_POINT ( 'NONE',  ( 5.405949406249992428, -9.363379034771808662, -126.2812500020483668 ) ) ;
#10657 = CARTESIAN_POINT ( 'NONE',  ( 5.405949406249999534, 9.363379034771803333, -163.2812500020484094 ) ) ;
#10658 = CARTESIAN_POINT ( 'NONE',  ( 5.405949406249999534, 9.363379034771803333, -49.28125000204838813 ) ) ;
#10659 = CARTESIAN_POINT ( 'NONE',  ( 10.00000000000000000, 5.773502691896255534, -132.7500000040967905 ) ) ;
#10660 = CARTESIAN_POINT ( 'NONE',  ( 10.00000000000000000, 5.773502691896255534, -105.3749999999999858 ) ) ;
#10661 = VERTEX_POINT ( 'NONE', #38281 ) ;
#10662 = CARTESIAN_POINT ( 'NONE',  ( -10.81189881249999729, -6.242252689847864744, -137.1562500020484094 ) ) ;
#10663 = CARTESIAN_POINT ( 'NONE',  ( -2.121150477449813534E-15, -11.54700538379251284, -157.2500000040967620 ) ) ;
#10664 = CARTESIAN_POINT ( 'NONE',  ( -5.405949406250003975, -9.363379034771801557, -149.0312500020483810 ) ) ;
#10665 = CARTESIAN_POINT ( 'NONE',  ( 10.81189881249999729, 0.000000000000000000, -192.0312500020484094 ) ) ;
#10666 = CARTESIAN_POINT ( 'NONE',  ( 5.405949406249992428, -9.363379034771808662, -79.59375000204838102 ) ) ;
#10667 = ORIENTED_EDGE ( 'NONE', *, *, #20133, .F. ) ;
#10668 = CARTESIAN_POINT ( 'NONE',  ( -9.999999999999998224, 1.224646799147353059E-15, -49.24999999999998579 ) ) ;
#10669 = CARTESIAN_POINT ( 'NONE',  ( 10.81189881249999907, 6.242252689847868297, -184.2187500020483810 ) ) ;
#10670 = CARTESIAN_POINT ( 'NONE',  ( -5.000000000000003553, -8.660254037844383745, -65.87500000409676204 ) ) ;
#10671 = CARTESIAN_POINT ( 'NONE',  ( 9.999999999999998224, 0.000000000000000000, -21.87500000409675494 ) ) ;
#10672 = CARTESIAN_POINT ( 'NONE',  ( -2.121150477449813534E-15, -11.54700538379251284, -165.8750000000000000 ) ) ;
#10673 = CARTESIAN_POINT ( 'NONE',  ( -2.293366432827344421E-15, -12.48450537969573659, -73.90625000204836681 ) ) ;
#10674 = CARTESIAN_POINT ( 'NONE',  ( -2.293366432827344421E-15, -12.48450537969573659, -63.40625000204837391 ) ) ;
#10675 = ADVANCED_FACE ( 'NONE', ( #24928 ), #18422, .T. ) ;
#10676 = CARTESIAN_POINT ( 'NONE',  ( -4.999999999999996447, 8.660254037844387298, -52.87500000409675494 ) ) ;
#10677 = CARTESIAN_POINT ( 'NONE',  ( -10.81189881249999907, -6.242252689847864744, -13.96875000204836326 ) ) ;
#10678 = CARTESIAN_POINT ( 'NONE',  ( -9.999999999998969713, -5.773502691896847949, -30.00000000409673717 ) ) ;
#10679 = CARTESIAN_POINT ( 'NONE',  ( 10.81189881249999551, -6.242252689847874514, -174.1562500020484094 ) ) ;
#10680 = CARTESIAN_POINT ( 'NONE',  ( -10.81189881249999729, 6.242252689847871849, -2.406250002048360592 ) ) ;
#10681 = CARTESIAN_POINT ( 'NONE',  ( 0.000000000000000000, 0.000000000000000000, -180.0000000000000000 ) ) ;
#10682 = CARTESIAN_POINT ( 'NONE',  ( -2.121150477449813534E-15, -11.54700538379251284, -161.3750000000000000 ) ) ;
#10683 = CARTESIAN_POINT ( 'NONE',  ( 9.999999999999998224, 0.000000000000000000, -155.0000000000000000 ) ) ;
#10684 = CARTESIAN_POINT ( 'NONE',  ( 10.00000000000038369, -5.773502691896038819, -153.6250000000000284 ) ) ;
#10685 = VECTOR ( 'NONE', #10134, 1000.000000000000000 ) ;
#10686 = FACE_OUTER_BOUND ( 'NONE', #30821, .T. ) ;
#10688 = ORIENTED_EDGE ( 'NONE', *, *, #34402, .T. ) ;
#10687 = CARTESIAN_POINT ( 'NONE',  ( 5.405949406249992428, -9.363379034771808662, -88.78125000204838102 ) ) ;
#10690 = ORIENTED_EDGE ( 'NONE', *, *, #15931, .T. ) ;
#10689 = CARTESIAN_POINT ( 'NONE',  ( -5.000000000000003553, -8.660254037844383745, -122.8750000040967905 ) ) ;
#10691 = ORIENTED_EDGE ( 'NONE', *, *, #18172, .T. ) ;
#10692 = CARTESIAN_POINT ( 'NONE',  ( 10.81189881249999729, 0.000000000000000000, -25.34375000204835970 ) ) ;
#10693 = AXIS2_PLACEMENT_3D ( 'NONE', #35903, #2889, #39973 ) ;
#10694 = CARTESIAN_POINT ( 'NONE',  ( 5.405949406249999534, 9.363379034771803333, -17.78125000204835970 ) ) ;
#10695 = DATE_AND_TIME ( #30152, #9441 ) ;
#10696 = CARTESIAN_POINT ( 'NONE',  ( -5.405949406249996869, 9.363379034771805109, -74.34375000204838102 ) ) ;
#10697 = CARTESIAN_POINT ( 'NONE',  ( 9.999999999999872102, 5.773502691896329253, -164.2500000040968189 ) ) ;
#10698 = CARTESIAN_POINT ( 'NONE',  ( -5.000000000000003553, -8.660254037844383745, -47.49999999999998579 ) ) ;
#10699 = CARTESIAN_POINT ( 'NONE',  ( 10.81189881249999551, -6.242252689847874514, -187.4687500020484094 ) ) ;
#10700 = CARTESIAN_POINT ( 'NONE',  ( -2.293366432827344421E-15, -12.48450537969573659, -163.7187500020483810 ) ) ;
#10701 = CARTESIAN_POINT ( 'NONE',  ( 7.644554776091147741E-16, 12.48450537969573659, -2.468750002048359704 ) ) ;
#10702 = CARTESIAN_POINT ( 'NONE',  ( -9.999999999999742428, -5.773502691896402084, -121.5000000040967905 ) ) ;
#10703 = CARTESIAN_POINT ( 'NONE',  ( 5.000000000000000000, 8.660254037844385522, -147.2500000000000000 ) ) ;
#10704 = CARTESIAN_POINT ( 'NONE',  ( -10.00000000000051337, 5.773502691895962435, -143.8750000000000000 ) ) ;
#10705 = CARTESIAN_POINT ( 'NONE',  ( -4.999999999999996447, 8.660254037844387298, -60.37500000409676204 ) ) ;
#10706 = CARTESIAN_POINT ( 'NONE',  ( 10.81189881249999551, -6.242252689847874514, -109.4687500020483810 ) ) ;
#10707 = CARTESIAN_POINT ( 'NONE',  ( 9.999999999999998224, 0.000000000000000000, -200.0000000000000000 ) ) ;
#10708 = CARTESIAN_POINT ( 'NONE',  ( 7.644554776091147741E-16, 12.48450537969573659, -94.15625000204839523 ) ) ;
#10709 = CARTESIAN_POINT ( 'NONE',  ( -10.81189881249999729, 6.242252689847871849, -96.71875000204836681 ) ) ;
#10710 =( BOUNDED_CURVE ( )  B_SPLINE_CURVE ( 2, ( #34659, #11534, #27533, #37230, #24738, #24517, #27963 ),
 .UNSPECIFIED., .F., .F. ) 
 B_SPLINE_CURVE_WITH_KNOTS ( ( 3, 2, 2, 3 ),
 ( 0.6902985074626868389, 0.6915422885572141132, 0.6927860696517414985, 0.6940298507462688837 ),
 .UNSPECIFIED. ) 
 CURVE ( )  GEOMETRIC_REPRESENTATION_ITEM ( )  RATIONAL_B_SPLINE_CURVE ( ( 0.9999999999999761302, 0.8660254037844625774, 1.000000000000000000, 0.8660254037844387076, 1.000000000000000000, 0.8660254037844148378, 1.000000000000023981 ) ) 
 REPRESENTATION_ITEM ( '' )  );
#10711 = CARTESIAN_POINT ( 'NONE',  ( -10.81189881249999907, -6.242252689847864744, -66.46875000204838102 ) ) ;
#10712 = AXIS2_PLACEMENT_3D ( 'NONE', #2030, #11929, #15794 ) ;
#10713 = CARTESIAN_POINT ( 'NONE',  ( 7.644554776091147741E-16, 12.48450537969573659, -79.15625000204838102 ) ) ;
#10714 = CARTESIAN_POINT ( 'NONE',  ( 9.999999999999996447, -5.773502691896262640, -166.0000000040967905 ) ) ;
#10715 = VECTOR ( 'NONE', #23764, 1000.000000000000000 ) ;
#10716 = CARTESIAN_POINT ( 'NONE',  ( -10.81189881249999729, -6.242252689847864744, -161.1562500020484094 ) ) ;
#10717 = CARTESIAN_POINT ( 'NONE',  ( -10.81189881249999729, 1.324075727343319199E-15, -174.7812500020484094 ) ) ;
#10718 = ADVANCED_FACE ( 'NONE', ( #32249 ), #38714, .T. ) ;
#10719 = CARTESIAN_POINT ( 'NONE',  ( -2.293366432827344421E-15, -12.48450537969573659, -1.718750002048352377 ) ) ;
#10720 = CARTESIAN_POINT ( 'NONE',  ( -9.999999999999998224, 1.224646799147353059E-15, -108.1250000040967763 ) ) ;
#10721 = CARTESIAN_POINT ( 'NONE',  ( 7.644554776091147741E-16, 12.48450537969573659, -102.9687500020483952 ) ) ;
#10722 = CYLINDRICAL_SURFACE ( 'NONE', #21768, 9.999999999999998224 ) ;
#10723 = CARTESIAN_POINT ( 'NONE',  ( -4.999999999999996447, 8.660254037844387298, -71.99999999999998579 ) ) ;
#10724 = CARTESIAN_POINT ( 'NONE',  ( -10.81189881249999729, 6.242252689847871849, -5.406250002048363257 ) ) ;
#10725 = CARTESIAN_POINT ( 'NONE',  ( -5.000000000000003553, -8.660254037844383745, -92.87500000409677625 ) ) ;
#10726 = VECTOR ( 'NONE', #5463, 1000.000000000000000 ) ;
#10727 = CARTESIAN_POINT ( 'NONE',  ( -9.999999999999998224, 1.224646799147353059E-15, -168.1250000040967905 ) ) ;
#10728 = CARTESIAN_POINT ( 'NONE',  ( 5.405949406249999534, 9.363379034771803333, -101.7812500020483952 ) ) ;
#10729 = CARTESIAN_POINT ( 'NONE',  ( 10.81189881249999551, -6.242252689847874514, -87.15625000204838102 ) ) ;
#10730 = CARTESIAN_POINT ( 'NONE',  ( -10.00000000000000000, -5.773502691896251982, -76.50000000409677625 ) ) ;
#10731 = CARTESIAN_POINT ( 'NONE',  ( -10.00000000000076916, 5.773502691895813221, -134.8750000000000000 ) ) ;
#10732 = CARTESIAN_POINT ( 'NONE',  ( -2.293366432827344421E-15, -12.48450537969573659, -36.21875000204835970 ) ) ;
#10733 = EDGE_LOOP ( 'NONE', ( #19249, #40144, #1869, #14383 ) ) ;
#10734 = CARTESIAN_POINT ( 'NONE',  ( -9.999999999999998224, 1.224646799147353059E-15, -4.249999999999976019 ) ) ;
#10735 = CARTESIAN_POINT ( 'NONE',  ( 5.405949406249999534, 9.363379034771803333, -25.28125000204836681 ) ) ;
#10736 = CARTESIAN_POINT ( 'NONE',  ( 10.81189881249999729, 0.000000000000000000, -14.84375000204835082 ) ) ;
#10737 = CARTESIAN_POINT ( 'NONE',  ( -5.000000000000003553, -8.660254037844383745, -32.49999999999997158 ) ) ;
#10738 = CARTESIAN_POINT ( 'NONE',  ( 5.000000000000000000, 8.660254037844385522, -3.625000004096767814 ) ) ;
#10739 = CARTESIAN_POINT ( 'NONE',  ( 10.81189881249999551, -6.242252689847874514, -139.6562500020484094 ) ) ;
#10740 = ADVANCED_FACE ( 'NONE', ( #41933 ), #38494, .T. ) ;
#10741 = CARTESIAN_POINT ( 'NONE',  ( -4.999999999999996447, 8.660254037844387298, -187.5000000000000000 ) ) ;
#10742 = CARTESIAN_POINT ( 'NONE',  ( 6.760415694317262479E-15, -15.00000000000010303, 49.99999999999998579 ) ) ;
#10744 = VERTEX_POINT ( 'NONE', #8728 ) ;
#10743 = CARTESIAN_POINT ( 'NONE',  ( 5.405949406249992428, -9.363379034771808662, -108.2812500020483810 ) ) ;
#10745 = CARTESIAN_POINT ( 'NONE',  ( -9.999999999999998224, 1.224646799147353059E-15, -75.12500000409677625 ) ) ;
#10746 = EDGE_LOOP ( 'NONE', ( #10035, #31673, #39351, #18511 ) ) ;
#10747 = ORIENTED_EDGE ( 'NONE', *, *, #19331, .T. ) ;
#10748 = CARTESIAN_POINT ( 'NONE',  ( 10.81189881249999907, 6.242252689847868297, -44.90625000204836681 ) ) ;
#10749 = DATE_TIME_ROLE ( 'classification_date' ) ;
#10750 = CARTESIAN_POINT ( 'NONE',  ( -2.293366432827344421E-15, -12.48450537969573659, -99.21875000204839523 ) ) ;
#10751 = DIRECTION ( 'NONE',  ( -1.000000000000000000, 0.000000000000000000, 0.000000000000000000 ) ) ;
#10752 = CARTESIAN_POINT ( 'NONE',  ( -5.405949406249996869, 9.363379034771805109, -192.8437500020484094 ) ) ;
#10753 =( BOUNDED_CURVE ( )  B_SPLINE_CURVE ( 2, ( #10021, #20369, #20164, #4192, #30540, #16908, #39798 ),
 .UNSPECIFIED., .F., .F. ) 
 B_SPLINE_CURVE_WITH_KNOTS ( ( 3, 2, 2, 3 ),
 ( 0.2388059701492538378, 0.2400497512437811953, 0.2412935323383085806, 0.2425373134328359381 ),
 .UNSPECIFIED. ) 
 CURVE ( )  GEOMETRIC_REPRESENTATION_ITEM ( )  RATIONAL_B_SPLINE_CURVE ( ( 0.9999999999999880096, 0.8660254037844506980, 1.000000000000000000, 0.8660254037844387076, 1.000000000000000000, 0.8660254037844267172, 1.000000000000011990 ) ) 
 REPRESENTATION_ITEM ( '' )  );
#10754 = CARTESIAN_POINT ( 'NONE',  ( -2.293366432827344421E-15, -12.48450537969573659, -171.4062500020484379 ) ) ;
#10755 = CARTESIAN_POINT ( 'NONE',  ( 0.000000000000000000, 0.000000000000000000, -200.0000000000000000 ) ) ;
#10756 = CARTESIAN_POINT ( 'NONE',  ( 10.81189881249999551, -6.242252689847874514, -124.4687500020483952 ) ) ;
#10757 = PRODUCT ( 'T-handle', 'T-handle', '', ( #851 ) ) ;
#10758 = CARTESIAN_POINT ( 'NONE',  ( 10.81189881249999551, -6.242252689847874514, -94.46875000204838102 ) ) ;
#10759 = CARTESIAN_POINT ( 'NONE',  ( -4.999999999999996447, 8.660254037844387298, -112.8750000040967763 ) ) ;
#10760 = CARTESIAN_POINT ( 'NONE',  ( -10.81189881249999729, 6.242252689847871849, -99.90625000204838102 ) ) ;
#10761 = CARTESIAN_POINT ( 'NONE',  ( -2.121150477449813534E-15, -11.54700538379251284, -187.2500000040967905 ) ) ;
#10762 = CARTESIAN_POINT ( 'NONE',  ( -2.293366432827344421E-15, -12.48450537969573659, -108.2187500020483668 ) ) ;
#10763 = CARTESIAN_POINT ( 'NONE',  ( 5.405949406249992428, -9.363379034771808662, -177.2812500020484094 ) ) ;
#10764 = EDGE_CURVE ( 'NONE', #11999, #33637, #7320, .T. ) ;
#10765 =( BOUNDED_CURVE ( )  B_SPLINE_CURVE ( 2, ( #8898, #22063, #25523, #6087, #18818, #32002, #22275 ),
 .UNSPECIFIED., .F., .F. ) 
 B_SPLINE_CURVE_WITH_KNOTS ( ( 3, 2, 2, 3 ),
 ( 0.7947761194029852039, 0.7960199004975125892, 0.7972636815920399744, 0.7985074626865673597 ),
 .UNSPECIFIED. ) 
 CURVE ( )  GEOMETRIC_REPRESENTATION_ITEM ( )  RATIONAL_B_SPLINE_CURVE ( ( 0.9999999999999880096, 0.8660254037844506980, 1.000000000000000000, 0.8660254037844387076, 1.000000000000000000, 0.8660254037844148378, 1.000000000000023981 ) ) 
 REPRESENTATION_ITEM ( '' )  );
#10766 = CARTESIAN_POINT ( 'NONE',  ( 5.000000000000000000, 8.660254037844385522, -180.2500000000000284 ) ) ;
#10767 = CARTESIAN_POINT ( 'NONE',  ( -9.999999999999740652, 5.773502691896409189, -181.3749999999999716 ) ) ;
#10768 = CARTESIAN_POINT ( 'NONE',  ( 5.405949406249999534, 9.363379034771803333, -197.7812500020484094 ) ) ;
#10769 = CARTESIAN_POINT ( 'NONE',  ( -5.405949406250003975, -9.363379034771801557, -54.34375000204835970 ) ) ;
#10770 = CARTESIAN_POINT ( 'NONE',  ( -10.81189881249999729, 6.242252689847871849, -39.71875000204835970 ) ) ;
#10771 = CARTESIAN_POINT ( 'NONE',  ( -2.121150477449813534E-15, -11.54700538379251284, -169.2500000040967620 ) ) ;
#10772 = CARTESIAN_POINT ( 'NONE',  ( 10.81189881249999907, 6.242252689847868297, -11.90625000204835615 ) ) ;
#10773 = CARTESIAN_POINT ( 'NONE',  ( -10.81189881249999907, -6.242252689847864744, -21.46875000204836681 ) ) ;
#10774 = CARTESIAN_POINT ( 'NONE',  ( 0.000000000000000000, 0.000000000000000000, -99.99999999999998579 ) ) ;
#10775 = CARTESIAN_POINT ( 'NONE',  ( 5.405949406249999534, 9.363379034771803333, -130.0937500020483810 ) ) ;
#10776 = CARTESIAN_POINT ( 'NONE',  ( 7.070501591499377789E-16, 11.54700538379251284, -94.62499999999997158 ) ) ;
#10777 = CARTESIAN_POINT ( 'NONE',  ( 10.81189881249999907, 6.242252689847868297, -31.40625000204835615 ) ) ;
#10778 = CARTESIAN_POINT ( 'NONE',  ( -9.999999999998456346, -5.773502691897145489, -27.00000000409673717 ) ) ;
#10779 = CARTESIAN_POINT ( 'NONE',  ( -9.999999999999998224, 1.224646799147353059E-15, -56.74999999999996447 ) ) ;
#10780 = CARTESIAN_POINT ( 'NONE',  ( -10.81189881249999729, 1.324075727343319199E-15, -126.7812500020483668 ) ) ;
#10781 = CARTESIAN_POINT ( 'NONE',  ( 10.81189881249999729, 6.242252689847867408, -104.9062500020483952 ) ) ;
#10782 = ORIENTED_EDGE ( 'NONE', *, *, #35792, .T. ) ;
#10783 = DIRECTION ( 'NONE',  ( -0.000000000000000000, -0.000000000000000000, 1.000000000000000000 ) ) ;
#10784 = CARTESIAN_POINT ( 'NONE',  ( 5.000000000000000000, 8.660254037844385522, -101.1250000040967905 ) ) ;
#10785 = CARTESIAN_POINT ( 'NONE',  ( -4.999999999999996447, 8.660254037844387298, -91.49999999999998579 ) ) ;
#10786 = ORGANIZATION ( 'NAUO-ORG4', 'UNSPECIFIED', 'UNSPECIFIED' ) ;
#10787 = CARTESIAN_POINT ( 'NONE',  ( 5.405949406249999534, 9.363379034771803333, -56.59375000204835970 ) ) ;
#10788 = EDGE_LOOP ( 'NONE', ( #40676, #7955, #23350, #2541 ) ) ;
#10789 = CARTESIAN_POINT ( 'NONE',  ( -4.999999999999996447, 8.660254037844387298, -31.49999999999997158 ) ) ;
#10790 = CARTESIAN_POINT ( 'NONE',  ( -5.405949406250003975, -9.363379034771801557, -33.53125000204837391 ) ) ;
#10791 = EDGE_CURVE ( 'NONE', #14676, #4387, #29006, .T. ) ;
#10792 = CARTESIAN_POINT ( 'NONE',  ( -4.999999999999996447, 8.660254037844387298, -111.3750000040967763 ) ) ;
#10793 = CARTESIAN_POINT ( 'NONE',  ( -5.000000000000003553, -8.660254037844383745, -26.87500000409676204 ) ) ;
#10794 = LINE ( 'NONE', #26997, #41741 ) ;
#10795 = CARTESIAN_POINT ( 'NONE',  ( -10.81189881249999907, -6.242252689847864744, -144.6562500020484094 ) ) ;
#10796 = DIRECTION ( 'NONE',  ( 1.000000000000000000, 0.000000000000000000, 0.000000000000000000 ) ) ;
#10797 = ORIENTED_EDGE ( 'NONE', *, *, #32796, .T. ) ;
#10799 = ORIENTED_EDGE ( 'NONE', *, *, #40243, .T. ) ;
#10798 = VERTEX_POINT ( 'NONE', #11729 ) ;
#10800 = CARTESIAN_POINT ( 'NONE',  ( -4.999999999999996447, 8.660254037844387298, -174.3750000040968189 ) ) ;
#10801 = CARTESIAN_POINT ( 'NONE',  ( -5.405949406249996869, 9.363379034771805109, -167.3437500020484094 ) ) ;
#10802 = CARTESIAN_POINT ( 'NONE',  ( -5.405949406250003975, -9.363379034771801557, -197.0312500020484094 ) ) ;
#10803 = CARTESIAN_POINT ( 'NONE',  ( 7.644554776091147741E-16, 12.48450537969573659, -12.96875000204836148 ) ) ;
#10804 = DIRECTION ( 'NONE',  ( -0.000000000000000000, -0.000000000000000000, 1.000000000000000000 ) ) ;
#10805 = CARTESIAN_POINT ( 'NONE',  ( 7.644554776091147741E-16, 12.48450537969573659, -146.4687500020484094 ) ) ;
#10806 = CARTESIAN_POINT ( 'NONE',  ( -10.81189881249999729, 1.324075727343319199E-15, -140.0937500020483810 ) ) ;
#10807 = CARTESIAN_POINT ( 'NONE',  ( 10.81189881249999551, -6.242252689847874514, -105.1562500020483810 ) ) ;
#10808 = CARTESIAN_POINT ( 'NONE',  ( -5.405949406249996869, 9.363379034771805109, -117.8437500020483810 ) ) ;
#10809 = CARTESIAN_POINT ( 'NONE',  ( -4.999999999999996447, 8.660254037844387298, -192.3750000040967905 ) ) ;
#10810 = CARTESIAN_POINT ( 'NONE',  ( 5.405949406249999534, 9.363379034771803333, -122.7812500020483952 ) ) ;
#10811 = CARTESIAN_POINT ( 'NONE',  ( 10.81189881249999729, 0.000000000000000000, -13.34375000204834905 ) ) ;
#10812 = CARTESIAN_POINT ( 'NONE',  ( -2.293366432827344421E-15, -12.48450537969573659, -132.2187500020483810 ) ) ;
#10813 = CARTESIAN_POINT ( 'NONE',  ( 5.000000000000000000, 8.660254037844385522, -63.62500000409676204 ) ) ;
#10814 = CARTESIAN_POINT ( 'NONE',  ( 9.999999999999998224, 0.000000000000000000, -179.3750000040967905 ) ) ;
#10815 = CARTESIAN_POINT ( 'NONE',  ( -10.00000000000000000, -5.773502691896251982, -158.6250000000000284 ) ) ;
#10816 = CARTESIAN_POINT ( 'NONE',  ( 5.000000000000000000, 8.660254037844385522, -18.24999999999996092 ) ) ;
#10817 = CARTESIAN_POINT ( 'NONE',  ( 10.81189881249999729, 0.000000000000000000, -79.34375000204838102 ) ) ;
#10818 = CARTESIAN_POINT ( 'NONE',  ( -5.405949406249996869, 9.363379034771805109, -63.84375000204836681 ) ) ;
#10819 = CYLINDRICAL_SURFACE ( 'NONE', #9786, 9.999999999999998224 ) ;
#10820 = CARTESIAN_POINT ( 'NONE',  ( -5.405949406250003975, -9.363379034771801557, -30.53125000204837036 ) ) ;
#10821 = CARTESIAN_POINT ( 'NONE',  ( 5.405949406249999534, 9.363379034771803333, -43.09375000204837391 ) ) ;
#10822 = CARTESIAN_POINT ( 'NONE',  ( 9.999999999999998224, 0.000000000000000000, -9.499999999999953815 ) ) ;
#10823 = CARTESIAN_POINT ( 'NONE',  ( -10.81189881249999729, 6.242252689847871849, -155.2187500020483810 ) ) ;
#10824 = CARTESIAN_POINT ( 'NONE',  ( 9.999999999999996447, -5.773502691896262640, -128.1249999999999716 ) ) ;
#10825 = CARTESIAN_POINT ( 'NONE',  ( 5.405949406249999534, 9.363379034771803333, -133.2812500020483810 ) ) ;
#10826 = CARTESIAN_POINT ( 'NONE',  ( -9.999999999999776179, -5.773502691896382544, -187.5000000040967905 ) ) ;
#10827 = CARTESIAN_POINT ( 'NONE',  ( -2.121150477449813534E-15, -11.54700538379251284, -81.87500000000000000 ) ) ;
#10828 = CARTESIAN_POINT ( 'NONE',  ( -2.293366432827344421E-15, -12.48450537969573659, -16.90625000204838102 ) ) ;
#10829 = VERTEX_POINT ( 'NONE', #15390 ) ;
#10830 = CARTESIAN_POINT ( 'NONE',  ( 10.81189881249999729, 0.000000000000000000, -106.5312500020483810 ) ) ;
#10831 = CARTESIAN_POINT ( 'NONE',  ( -9.999999999999998224, 1.224646799147353059E-15, -126.1250000040967620 ) ) ;
#10832 = CARTESIAN_POINT ( 'NONE',  ( -9.999999999999998224, 1.224646799147353059E-15, -38.74999999999997868 ) ) ;
#10833 = CARTESIAN_POINT ( 'NONE',  ( -9.999999999999998224, 5.773502691896259087, -36.25000000409675494 ) ) ;
#10834 =( BOUNDED_CURVE ( )  B_SPLINE_CURVE ( 2, ( #24598, #2149, #37747, #18097, #28260, #31073, #41398 ),
 .UNSPECIFIED., .F., .F. ) 
 B_SPLINE_CURVE_WITH_KNOTS ( ( 3, 2, 2, 3 ),
 ( 0.9813432835820897759, 0.9825870646766171612, 0.9838308457711445465, 0.9850746268656718208 ),
 .UNSPECIFIED. ) 
 CURVE ( )  GEOMETRIC_REPRESENTATION_ITEM ( )  RATIONAL_B_SPLINE_CURVE ( ( 0.9999999999999761302, 0.8660254037844625774, 1.000000000000000000, 0.8660254037844387076, 1.000000000000000000, 0.8660254037844148378, 1.000000000000023981 ) ) 
 REPRESENTATION_ITEM ( '' )  );
#10835 = CARTESIAN_POINT ( 'NONE',  ( 0.000000000000000000, 0.000000000000000000, -200.0000000000000000 ) ) ;
#10836 = CARTESIAN_POINT ( 'NONE',  ( 5.405949406249999534, 9.363379034771803333, -53.78125000204836681 ) ) ;
#10837 = CARTESIAN_POINT ( 'NONE',  ( -5.000000000000003553, -8.660254037844383745, -136.0000000000000000 ) ) ;
#10838 = CARTESIAN_POINT ( 'NONE',  ( -5.405949406250003975, -9.363379034771801557, -150.5312500020483810 ) ) ;
#10839 = CARTESIAN_POINT ( 'NONE',  ( 7.644554776091147741E-16, 12.48450537969573659, -138.9687500020484094 ) ) ;
#10841 = EDGE_CURVE ( 'NONE', #5330, #848, #16112, .T. ) ;
#10840 = LINE ( 'NONE', #31369, #39250 ) ;
#10842 = VERTEX_POINT ( 'NONE', #29215 ) ;
#10843 = ADVANCED_FACE ( 'NONE', ( #36740 ), #33091, .T. ) ;
#10844 = CARTESIAN_POINT ( 'NONE',  ( -4.999999999999996447, 8.660254037844387298, -163.8750000040967905 ) ) ;
#10845 = ORIENTED_EDGE ( 'NONE', *, *, #11941, .F. ) ;
#10846 = EDGE_LOOP ( 'NONE', ( #11332, #5663, #16276, #15558 ) ) ;
#10847 = PERSON_AND_ORGANIZATION_ROLE ( 'creator' ) ;
#10848 = AXIS2_PLACEMENT_3D ( 'NONE', #6947, #1331, #10589 ) ;
#10850 = ORIENTED_EDGE ( 'NONE', *, *, #28324, .F. ) ;
#10849 = CARTESIAN_POINT ( 'NONE',  ( 5.405949406249992428, -9.363379034771808662, -109.5937500020483810 ) ) ;
#10851 = CARTESIAN_POINT ( 'NONE',  ( 5.000000000000000000, 8.660254037844385522, -103.7500000000000000 ) ) ;
#10852 = CARTESIAN_POINT ( 'NONE',  ( -10.81189881249999729, 1.324075727343319199E-15, -192.5937500020484094 ) ) ;
#10853 = CARTESIAN_POINT ( 'NONE',  ( -2.293366432827344421E-15, -12.48450537969573659, -39.21875000204835970 ) ) ;
#10854 = CARTESIAN_POINT ( 'NONE',  ( -4.519005929163725455, -9.200975322961610914, 1.142019215729700943E-14 ) ) ;
#10855 = CARTESIAN_POINT ( 'NONE',  ( 7.070501591499376803E-16, 11.54700538379251284, -0.1249999999999685391 ) ) ;
#10856 = CARTESIAN_POINT ( 'NONE',  ( 10.81189881249999729, 0.000000000000000000, -172.3437500020484094 ) ) ;
#10857 = CARTESIAN_POINT ( 'NONE',  ( -5.405949406249996869, 9.363379034771805109, -161.3437500020484094 ) ) ;
#10858 = LINE ( 'NONE', #41276, #9373 ) ;
#10859 = CARTESIAN_POINT ( 'NONE',  ( -10.81189881249999907, -6.242252689847864744, -139.9687500020483810 ) ) ;
#10860 = CARTESIAN_POINT ( 'NONE',  ( -10.81189881249999729, 1.324075727343319199E-15, -156.5937500020483810 ) ) ;
#10861 = CARTESIAN_POINT ( 'NONE',  ( -2.121150477449813534E-15, -11.54700538379251284, -93.87500000000000000 ) ) ;
#10862 = CARTESIAN_POINT ( 'NONE',  ( 5.000000000000000000, 8.660254037844385522, -66.62500000409676204 ) ) ;
#10863 = CARTESIAN_POINT ( 'NONE',  ( -9.999999999999998224, 1.224646799147353059E-15, -176.7500000000000284 ) ) ;
#10864 = CARTESIAN_POINT ( 'NONE',  ( 5.405949406249992428, -9.363379034771808662, -87.09375000204836681 ) ) ;
#10865 = DIRECTION ( 'NONE',  ( -0.000000000000000000, -0.000000000000000000, 1.000000000000000000 ) ) ;
#10866 = CARTESIAN_POINT ( 'NONE',  ( -10.81189881249999907, -6.242252689847864744, -63.65625000204836681 ) ) ;
#10867 = CARTESIAN_POINT ( 'NONE',  ( -5.000000000000003553, -8.660254037844383745, -124.3750000040967763 ) ) ;
#10868 = CARTESIAN_POINT ( 'NONE',  ( 10.81189881249999551, -6.242252689847874514, -179.9687500020484094 ) ) ;
#10869 = CARTESIAN_POINT ( 'NONE',  ( -10.81189881249999729, 1.324075727343319199E-15, -120.7812500020483952 ) ) ;
#10870 = CARTESIAN_POINT ( 'NONE',  ( -10.81189881249999729, 1.324075727343319199E-15, -153.7812500020484094 ) ) ;
#10871 = CARTESIAN_POINT ( 'NONE',  ( 10.81189881249999551, -6.242252689847874514, -55.65625000204837391 ) ) ;
#10872 = CARTESIAN_POINT ( 'NONE',  ( 7.070501591499377789E-16, 11.54700538379251284, -132.5000000040967620 ) ) ;
#10873 = CARTESIAN_POINT ( 'NONE',  ( -10.00000000000000000, -5.773502691896251982, -104.6249999999999858 ) ) ;
#10874 =( BOUNDED_CURVE ( )  B_SPLINE_CURVE ( 2, ( #5016, #11252, #18377, #34586, #22052, #2418, #41460 ),
 .UNSPECIFIED., .F., .F. ) 
 B_SPLINE_CURVE_WITH_KNOTS ( ( 3, 2, 2, 3 ),
 ( 0.7238805970149256863, 0.7251243781094530716, 0.7263681592039803459, 0.7276119402985077311 ),
 .UNSPECIFIED. ) 
 CURVE ( )  GEOMETRIC_REPRESENTATION_ITEM ( )  RATIONAL_B_SPLINE_CURVE ( ( 0.9999999999999641398, 0.8660254037844745678, 1.000000000000000000, 0.8660254037844387076, 1.000000000000000000, 0.8660254037844148378, 1.000000000000023981 ) ) 
 REPRESENTATION_ITEM ( '' )  );
#10875 = ORIENTED_EDGE ( 'NONE', *, *, #1993, .T. ) ;
#10876 = CARTESIAN_POINT ( 'NONE',  ( -10.81189881249999729, 1.324075727343319199E-15, -132.7812500020483810 ) ) ;
#10877 = CARTESIAN_POINT ( 'NONE',  ( -2.121150477449813534E-15, -11.54700538379251284, -151.2500000040967620 ) ) ;
#10878 = CARTESIAN_POINT ( 'NONE',  ( -2.293366432827344421E-15, -12.48450537969573659, -145.9062500020484094 ) ) ;
#10879 = CARTESIAN_POINT ( 'NONE',  ( -10.81189881249999729, 1.324075727343319199E-15, -185.2812500020484094 ) ) ;
#10880 = AXIS2_PLACEMENT_3D ( 'NONE', #40215, #17334, #23841 ) ;
#10881 = ORIENTED_EDGE ( 'NONE', *, *, #17901, .T. ) ;
#10882 = CARTESIAN_POINT ( 'NONE',  ( 5.000000000000000000, 8.660254037844385522, -46.74999999999998579 ) ) ;
#10883 = CARTESIAN_POINT ( 'NONE',  ( -10.81189881249999729, 1.324075727343319199E-15, -183.5937500020483810 ) ) ;
#10884 = CARTESIAN_POINT ( 'NONE',  ( 9.999999999999996447, -5.773502691896262640, -61.00000000409677625 ) ) ;
#10885 = AXIS2_PLACEMENT_3D ( 'NONE', #4395, #10640, #11065 ) ;
#10886 = CARTESIAN_POINT ( 'NONE',  ( 4.999999999999992006, -8.660254037844389075, -110.2499999999999858 ) ) ;
#10887 = CARTESIAN_POINT ( 'NONE',  ( 9.999999999999998224, 0.000000000000000000, -119.3750000040967905 ) ) ;
#10888 = CARTESIAN_POINT ( 'NONE',  ( -5.405949406250003975, -9.363379034771801557, -80.03125000204838102 ) ) ;
#10889 = CARTESIAN_POINT ( 'NONE',  ( -5.405949406250003975, -9.363379034771801557, -62.03125000204837391 ) ) ;
#10890 = CARTESIAN_POINT ( 'NONE',  ( 9.999999999999996447, -5.773502691896262640, -52.00000000409676915 ) ) ;
#10891 = CARTESIAN_POINT ( 'NONE',  ( 5.405949406249992428, -9.363379034771808662, -13.59375000204834905 ) ) ;
#10892 = CARTESIAN_POINT ( 'NONE',  ( 5.000000000000000000, 8.660254037844385522, -88.74999999999998579 ) ) ;
#10893 = CARTESIAN_POINT ( 'NONE',  ( -10.81189881249999907, -6.242252689847864744, -177.6562500020484094 ) ) ;
#10894 = CARTESIAN_POINT ( 'NONE',  ( 5.405949406249999534, 9.363379034771803333, -2.781250002048374359 ) ) ;
#10895 = CARTESIAN_POINT ( 'NONE',  ( 10.00000000000102318, -5.773502691895667560, -87.62499999999995737 ) ) ;
#10897 = EDGE_CURVE ( 'NONE', #12865, #12739, #29637, .T. ) ;
#10896 = CARTESIAN_POINT ( 'NONE',  ( 9.999999999999998224, 0.000000000000000000, -138.8750000040968189 ) ) ;
#10898 = CARTESIAN_POINT ( 'NONE',  ( 9.999999999999742428, 5.773502691896404748, -117.3749999999999716 ) ) ;
#10899 = CARTESIAN_POINT ( 'NONE',  ( 9.999999999999548805, 5.773502691896514882, -177.3749999999999716 ) ) ;
#10900 = EDGE_CURVE ( 'NONE', #37654, #25373, #3738, .T. ) ;
#10901 = DIRECTION ( 'NONE',  ( -1.000000000000000000, -1.502314598737160017E-16, 0.000000000000000000 ) ) ;
#10902 = ADVANCED_FACE ( 'NONE', ( #30071 ), #25978, .F. ) ;
#10904 = VERTEX_POINT ( 'NONE', #16227 ) ;
#10903 = CARTESIAN_POINT ( 'NONE',  ( 10.81189881249999551, -6.242252689847874514, -84.15625000204838102 ) ) ;
#10906 = ORIENTED_EDGE ( 'NONE', *, *, #3109, .F. ) ;
#10905 = CARTESIAN_POINT ( 'NONE',  ( 9.999999999999998224, 0.000000000000000000, -122.3750000040967905 ) ) ;
#10907 = CC_DESIGN_PERSON_AND_ORGANIZATION_ASSIGNMENT ( #39681, #1056, ( #26987 ) ) ;
#10908 = ORIENTED_EDGE ( 'NONE', *, *, #17752, .T. ) ;
#10909 = CARTESIAN_POINT ( 'NONE',  ( -5.405949406249996869, 9.363379034771805109, -33.84375000204836681 ) ) ;
#10910 = CARTESIAN_POINT ( 'NONE',  ( -5.405949406249996869, 9.363379034771805109, -29.34375000204836326 ) ) ;
#10911 = CARTESIAN_POINT ( 'NONE',  ( -10.81189881249999729, 1.324075727343319199E-15, -14.28125000204835615 ) ) ;
#10912 = CARTESIAN_POINT ( 'NONE',  ( 10.81189881249999907, 6.242252689847868297, -67.21875000204838102 ) ) ;
#10913 = CYLINDRICAL_SURFACE ( 'NONE', #42182, 5.500000000000003553 ) ;
#10914 = CARTESIAN_POINT ( 'NONE',  ( -10.00000000000000000, -5.773502691896251982, -41.62499999999996447 ) ) ;
#10915 = CARTESIAN_POINT ( 'NONE',  ( -10.81189881249999729, 1.324075727343319199E-15, -186.5937500020483810 ) ) ;
#10916 = CARTESIAN_POINT ( 'NONE',  ( 5.405949406249999534, 9.363379034771803333, -163.0937500020484094 ) ) ;
#10917 = CARTESIAN_POINT ( 'NONE',  ( -9.999999999998456346, -5.773502691897145489, -26.62499999999994316 ) ) ;
#10918 = DIRECTION ( 'NONE',  ( -0.000000000000000000, -1.000000000000000000, -0.000000000000000000 ) ) ;
#10919 = CARTESIAN_POINT ( 'NONE',  ( -4.999999999999996447, 8.660254037844387298, -147.0000000000000000 ) ) ;
#10920 = EDGE_CURVE ( 'NONE', #41097, #39297, #13204, .T. ) ;
#10921 = DIRECTION ( 'NONE',  ( -1.000000000000000000, 0.000000000000000000, -0.000000000000000000 ) ) ;
#10922 = CARTESIAN_POINT ( 'NONE',  ( -10.81189881249999907, -6.242252689847864744, -112.9687500020483810 ) ) ;
#10923 = CARTESIAN_POINT ( 'NONE',  ( 9.999999999999998224, 0.000000000000000000, -18.49999999999996092 ) ) ;
#10924 = CARTESIAN_POINT ( 'NONE',  ( -5.405949406249996869, 9.363379034771805109, -92.53125000204838102 ) ) ;
#10925 = CARTESIAN_POINT ( 'NONE',  ( -5.405949406250003975, -9.363379034771801557, -99.34375000204838102 ) ) ;
#10926 = CARTESIAN_POINT ( 'NONE',  ( 10.81189881249999729, 0.000000000000000000, -67.34375000204836681 ) ) ;
#10927 = CARTESIAN_POINT ( 'NONE',  ( -10.81189881249999729, 1.324075727343319199E-15, -77.28125000204838102 ) ) ;
#10928 = CARTESIAN_POINT ( 'NONE',  ( 5.000000000000000000, 8.660254037844385522, -155.1250000040967905 ) ) ;
#10929 = CARTESIAN_POINT ( 'NONE',  ( -9.999999999999998224, 1.224646799147353059E-15, -131.7499999999999716 ) ) ;
#10930 = CARTESIAN_POINT ( 'NONE',  ( 10.81189881249999729, 0.000000000000000000, -160.5312500020484094 ) ) ;
#10931 = CARTESIAN_POINT ( 'NONE',  ( -10.81189881249999729, 1.324075727343319199E-15, -173.2812500020484094 ) ) ;
#10932 = CARTESIAN_POINT ( 'NONE',  ( -9.999999999999998224, 1.224646799147353059E-15, -145.6250000040967905 ) ) ;
#10933 = CARTESIAN_POINT ( 'NONE',  ( -9.999999999999998224, 1.224646799147353059E-15, -101.7500000000000000 ) ) ;
#10934 = CARTESIAN_POINT ( 'NONE',  ( 5.405949406249992428, -9.363379034771808662, -108.0937500020483810 ) ) ;
#10935 = CARTESIAN_POINT ( 'NONE',  ( -9.999999999999998224, 1.224646799147353059E-15, -62.74999999999997158 ) ) ;
#10936 = CARTESIAN_POINT ( 'NONE',  ( -10.00000000000000000, -5.773502691896251982, -71.62500000000000000 ) ) ;
#10937 = CARTESIAN_POINT ( 'NONE',  ( -10.81189881249999729, 1.324075727343319199E-15, -2.281250002048373915 ) ) ;
#10938 = CARTESIAN_POINT ( 'NONE',  ( -5.000000000000003553, -8.660254037844383745, -82.37500000409676204 ) ) ;
#10939 = CARTESIAN_POINT ( 'NONE',  ( -2.121150477449813534E-15, -11.54700538379251284, -171.8750000000000284 ) ) ;
#10940 = CARTESIAN_POINT ( 'NONE',  ( 10.81189881249999729, 0.000000000000000000, -97.53125000204839523 ) ) ;
#10941 = CARTESIAN_POINT ( 'NONE',  ( 10.81189881249999551, -6.242252689847874514, -84.15625000204838102 ) ) ;
#10942 = CARTESIAN_POINT ( 'NONE',  ( -5.000000000000003553, -8.660254037844383745, -76.37500000409677625 ) ) ;
#10943 = CARTESIAN_POINT ( 'NONE',  ( 7.070501591499376803E-16, 11.54700538379251284, -168.1250000000000000 ) ) ;
#10944 = CARTESIAN_POINT ( 'NONE',  ( -10.81189881249999729, 6.242252689847871849, -33.71875000204835260 ) ) ;
#10945 = ORIENTED_EDGE ( 'NONE', *, *, #40984, .F. ) ;
#10946 = CARTESIAN_POINT ( 'NONE',  ( 7.070501591499377789E-16, 11.54700538379251284, -1.624999999999975575 ) ) ;
#10947 = CARTESIAN_POINT ( 'NONE',  ( -10.81189881249999907, -6.242252689847864744, -29.15625000204835970 ) ) ;
#10948 = CARTESIAN_POINT ( 'NONE',  ( -2.293366432827344421E-15, -12.48450537969573659, -13.71875000204836503 ) ) ;
#10949 = CARTESIAN_POINT ( 'NONE',  ( -10.00000000000025580, 5.773502691896109873, -160.3750000000000000 ) ) ;
#10950 = AXIS2_PLACEMENT_3D ( 'NONE', #4577, #40380, #925 ) ;
#10951 = CARTESIAN_POINT ( 'NONE',  ( 7.070501591499377789E-16, 11.54700538379251284, -0.5000000040967511605 ) ) ;
#10952 = CARTESIAN_POINT ( 'NONE',  ( 10.81189881249999729, 0.000000000000000000, -132.0312500020484094 ) ) ;
#10953 = CARTESIAN_POINT ( 'NONE',  ( 9.999999999999998224, 0.000000000000000000, -180.5000000000000000 ) ) ;
#10954 = DIRECTION ( 'NONE',  ( 1.000000000000000000, 0.000000000000000000, 0.000000000000000000 ) ) ;
#10956 = ORIENTED_EDGE ( 'NONE', *, *, #39430, .F. ) ;
#10955 = CARTESIAN_POINT ( 'NONE',  ( -10.81189881249999907, -6.242252689847864744, -111.6562500020483952 ) ) ;
#10957 = ORIENTED_EDGE ( 'NONE', *, *, #36194, .T. ) ;
#10958 = ORIENTED_EDGE ( 'NONE', *, *, #38837, .F. ) ;
#10959 = CARTESIAN_POINT ( 'NONE',  ( 10.81189881249999729, 0.000000000000000000, -39.03125000204838102 ) ) ;
#10960 = SECURITY_CLASSIFICATION_LEVEL ( 'unclassified' ) ;
#10961 = EDGE_CURVE ( 'NONE', #25900, #6469, #32464, .T. ) ;
#10962 = CARTESIAN_POINT ( 'NONE',  ( -10.81189881249999907, -6.242252689847864744, -87.46875000204838102 ) ) ;
#10963 = CARTESIAN_POINT ( 'NONE',  ( 9.999999999999998224, 0.000000000000000000, -143.3750000040967905 ) ) ;
#10964 = FACE_OUTER_BOUND ( 'NONE', #9685, .T. ) ;
#10965 = CARTESIAN_POINT ( 'NONE',  ( -10.81189881249999729, -6.242252689847864744, -193.9687500020484094 ) ) ;
#10966 = CARTESIAN_POINT ( 'NONE',  ( 10.81189881249999907, 6.242252689847868297, -169.4062500020484094 ) ) ;
#10967 = CARTESIAN_POINT ( 'NONE',  ( 9.999999999998969713, 5.773502691896851502, -58.87499999999997158 ) ) ;
#10968 = CARTESIAN_POINT ( 'NONE',  ( 5.405949406249992428, -9.363379034771808662, -126.0937500020483668 ) ) ;
#10969 = CARTESIAN_POINT ( 'NONE',  ( 10.81189881249999907, 6.242252689847868297, -91.21875000204838102 ) ) ;
#10970 = CARTESIAN_POINT ( 'NONE',  ( 5.405949406249992428, -9.363379034771808662, -4.781250002048375691 ) ) ;
#10971 = CARTESIAN_POINT ( 'NONE',  ( -9.999999999999998224, 1.224646799147353059E-15, -154.2500000000000000 ) ) ;
#10972 = CARTESIAN_POINT ( 'NONE',  ( 10.81189881249999907, 6.242252689847868297, -98.90625000204839523 ) ) ;
#10973 = CARTESIAN_POINT ( 'NONE',  ( -10.00000000000000000, -5.773502691896251982, -177.0000000040967620 ) ) ;
#10974 = CARTESIAN_POINT ( 'NONE',  ( 10.81189881249999551, -6.242252689847874514, -106.4687500020483810 ) ) ;
#10975 = CARTESIAN_POINT ( 'NONE',  ( -2.293366432827344421E-15, -12.48450537969573659, -181.9062500020483810 ) ) ;
#10976 = CARTESIAN_POINT ( 'NONE',  ( 7.070501591499376803E-16, 11.54700538379251284, -108.1249999999999858 ) ) ;
#10977 = DIRECTION ( 'NONE',  ( 1.000000000000000000, 0.000000000000000000, 0.000000000000000000 ) ) ;
#10978 = CARTESIAN_POINT ( 'NONE',  ( -10.81189881249999729, 1.324075727343319199E-15, -197.2812500020484094 ) ) ;
#10979 = CARTESIAN_POINT ( 'NONE',  ( -2.293366432827344421E-15, -12.48450537969573659, -52.71875000204836681 ) ) ;
#10980 = VECTOR ( 'NONE', #7737, 1000.000000000000000 ) ;
#10981 = CARTESIAN_POINT ( 'NONE',  ( -2.293366432827344421E-15, -12.48450537969573659, -43.71875000204835970 ) ) ;
#10982 = CARTESIAN_POINT ( 'NONE',  ( -10.00000000000000000, -5.773502691896251982, -175.5000000040967905 ) ) ;
#10983 = CARTESIAN_POINT ( 'NONE',  ( -5.405949406249996869, 9.363379034771805109, -7.031250002048378356 ) ) ;
#10984 = CARTESIAN_POINT ( 'NONE',  ( -5.405949406250003975, -9.363379034771801557, -24.34375000204835970 ) ) ;
#10985 = CARTESIAN_POINT ( 'NONE',  ( 10.00000000000025402, -5.773502691896113426, -124.0000000040967620 ) ) ;
#10986 = CARTESIAN_POINT ( 'NONE',  ( -5.405949406249996869, 9.363379034771805109, -131.3437500020484094 ) ) ;
#10987 = CARTESIAN_POINT ( 'NONE',  ( -9.999999999999998224, 5.773502691896259087, -100.3750000000000000 ) ) ;
#10988 = CARTESIAN_POINT ( 'NONE',  ( -5.405949406249996869, 9.363379034771805109, -26.53125000204836681 ) ) ;
#10989 = CARTESIAN_POINT ( 'NONE',  ( -2.121150477449813534E-15, -11.54700538379251284, -110.7500000040967763 ) ) ;
#10990 = CARTESIAN_POINT ( 'NONE',  ( -10.00000000000000000, -5.773502691896252870, -169.1249999999999716 ) ) ;
#10991 = CARTESIAN_POINT ( 'NONE',  ( -4.999999999999996447, 8.660254037844387298, -61.49999999999997158 ) ) ;
#10992 = CARTESIAN_POINT ( 'NONE',  ( -10.81189881249999907, -6.242252689847864744, -128.1562500020483810 ) ) ;
#10993 = CARTESIAN_POINT ( 'NONE',  ( 5.405949406249992428, -9.363379034771808662, -103.7812500020483810 ) ) ;
#10994 = EDGE_LOOP ( 'NONE', ( #25069, #1890, #26001, #15680 ) ) ;
#10995 = AXIS2_PLACEMENT_3D ( 'NONE', #22315, #41718, #15810 ) ;
#10996 = CARTESIAN_POINT ( 'NONE',  ( -9.999999999999998224, 1.224646799147353059E-15, -68.74999999999997158 ) ) ;
#10997 = CARTESIAN_POINT ( 'NONE',  ( -9.999999999999998224, 1.224646799147353059E-15, -100.6250000040967905 ) ) ;
#10998 = CARTESIAN_POINT ( 'NONE',  ( -5.000000000000003553, -8.660254037844383745, -151.3750000040967905 ) ) ;
#10999 = CARTESIAN_POINT ( 'NONE',  ( 5.405949406249999534, 9.363379034771803333, -164.7812500020484094 ) ) ;
#11000 = CARTESIAN_POINT ( 'NONE',  ( -5.405949406249996869, 9.363379034771805109, -57.84375000204835970 ) ) ;
#11001 = ORIENTED_EDGE ( 'NONE', *, *, #39889, .T. ) ;
#11002 = CARTESIAN_POINT ( 'NONE',  ( -9.999999999999998224, 1.224646799147353059E-15, -26.74999999999996803 ) ) ;
#11003 = CARTESIAN_POINT ( 'NONE',  ( 5.405949406249992428, -9.363379034771808662, -39.28125000204838102 ) ) ;
#11004 = CARTESIAN_POINT ( 'NONE',  ( 5.000000000000000000, 8.660254037844385522, -163.7500000000000000 ) ) ;
#11005 = CARTESIAN_POINT ( 'NONE',  ( 0.000000000000000000, 0.000000000000000000, -99.99999999999998579 ) ) ;
#11006 = CARTESIAN_POINT ( 'NONE',  ( -4.999999999999996447, 8.660254037844387298, -30.37500000409676204 ) ) ;
#11007 =( BOUNDED_CURVE ( )  B_SPLINE_CURVE ( 2, ( #15470, #21962, #15262, #28671, #32540, #5353, #38156 ),
 .UNSPECIFIED., .F., .F. ) 
 B_SPLINE_CURVE_WITH_KNOTS ( ( 3, 2, 2, 3 ),
 ( 0.1828358208955224162, 0.1840796019900497738, 0.1853233830845771313, 0.1865671641791045166 ),
 .UNSPECIFIED. ) 
 CURVE ( )  GEOMETRIC_REPRESENTATION_ITEM ( )  RATIONAL_B_SPLINE_CURVE ( ( 0.9999999999999970024, 0.8660254037844417052, 1.000000000000000000, 0.8660254037844387076, 1.000000000000000000, 0.8660254037844357100, 1.000000000000002887 ) ) 
 REPRESENTATION_ITEM ( '' )  );
#11008 = CARTESIAN_POINT ( 'NONE',  ( 7.644554776091147741E-16, 12.48450537969573659, -131.6562500020483810 ) ) ;
#11009 = CARTESIAN_POINT ( 'NONE',  ( -9.999999999999998224, 1.224646799147353059E-15, -75.12500000409677625 ) ) ;
#11010 = EDGE_LOOP ( 'NONE', ( #25015, #6558, #20255, #41155 ) ) ;
#11011 =( BOUNDED_CURVE ( )  B_SPLINE_CURVE ( 2, ( #19438, #23548, #16395, #6711, #680, #14002, #20290 ),
 .UNSPECIFIED., .F., .F. ) 
 B_SPLINE_CURVE_WITH_KNOTS ( ( 3, 2, 2, 3 ),
 ( 0.1940298507462686894, 0.1952736318407960470, 0.1965174129353234322, 0.1977611940298507898 ),
 .UNSPECIFIED. ) 
 CURVE ( )  GEOMETRIC_REPRESENTATION_ITEM ( )  RATIONAL_B_SPLINE_CURVE ( ( 0.9999999999999970024, 0.8660254037844417052, 1.000000000000000000, 0.8660254037844387076, 1.000000000000000000, 0.8660254037844327124, 1.000000000000005995 ) ) 
 REPRESENTATION_ITEM ( '' )  );
#11013 = EDGE_LOOP ( 'NONE', ( #11087, #37618, #18353, #1593 ) ) ;
#11012 = ORIENTED_EDGE ( 'NONE', *, *, #27480, .T. ) ;
#11014 = CARTESIAN_POINT ( 'NONE',  ( 5.000000000000000000, 8.660254037844385522, -182.1250000040967905 ) ) ;
#11015 = CARTESIAN_POINT ( 'NONE',  ( -5.000000000000003553, -8.660254037844383745, -134.5000000000000000 ) ) ;
#11016 = CARTESIAN_POINT ( 'NONE',  ( 7.644554776091147741E-16, 12.48450537969573659, -162.9687500020483810 ) ) ;
#11017 =( BOUNDED_CURVE ( )  B_SPLINE_CURVE ( 2, ( #32857, #36505, #6728, #39312, #3286, #33497, #33067 ),
 .UNSPECIFIED., .F., .F. ) 
 B_SPLINE_CURVE_WITH_KNOTS ( ( 3, 2, 2, 3 ),
 ( 0.3470149253731344974, 0.3482587064676618271, 0.3495024875621891569, 0.3507462686567164867 ),
 .UNSPECIFIED. ) 
 CURVE ( )  GEOMETRIC_REPRESENTATION_ITEM ( )  RATIONAL_B_SPLINE_CURVE ( ( 0.9999999999999820144, 0.8660254037844566932, 1.000000000000000000, 0.8660254037844387076, 1.000000000000000000, 0.8660254037844327124, 1.000000000000005995 ) ) 
 REPRESENTATION_ITEM ( '' )  );
#11018 = FACE_OUTER_BOUND ( 'NONE', #15503, .T. ) ;
#11019 = CARTESIAN_POINT ( 'NONE',  ( -10.81189881249999729, 6.242252689847871849, -17.21875000204836681 ) ) ;
#11020 = CARTESIAN_POINT ( 'NONE',  ( -10.81189881249999729, -6.242252689847864744, -145.9687500020484094 ) ) ;
#11021 = CARTESIAN_POINT ( 'NONE',  ( 10.81189881249999551, -6.242252689847874514, -140.9687500020483810 ) ) ;
#11022 = CARTESIAN_POINT ( 'NONE',  ( 7.644554776091147741E-16, 12.48450537969573659, -106.1562500020483952 ) ) ;
#11023 = CARTESIAN_POINT ( 'NONE',  ( -10.81189881249999729, 6.242252689847871849, -116.2187500020483810 ) ) ;
#11024 = CARTESIAN_POINT ( 'NONE',  ( -5.405949406249996869, 9.363379034771805109, 0.6562499979516356330 ) ) ;
#11025 = CARTESIAN_POINT ( 'NONE',  ( 7.644554776091147741E-16, 12.48450537969573659, -125.6562500020483810 ) ) ;
#11026 = CARTESIAN_POINT ( 'NONE',  ( -5.405949406249996869, 9.363379034771805109, -11.34375000204834727 ) ) ;
#11028 = EDGE_CURVE ( 'NONE', #10480, #21964, #26397, .T. ) ;
#11027 = CARTESIAN_POINT ( 'NONE',  ( -10.81189881249999729, -6.242252689847864744, -129.4687500020483810 ) ) ;
#11029 = CARTESIAN_POINT ( 'NONE',  ( -10.81189881249999729, -6.242252689847864744, -198.6562500020484094 ) ) ;
#11030 = CARTESIAN_POINT ( 'NONE',  ( 4.999999999999992006, -8.660254037844389075, -196.1250000040967905 ) ) ;
#11031 = CARTESIAN_POINT ( 'NONE',  ( -9.999999999999998224, 5.773502691896259087, -154.3749999999999716 ) ) ;
#11032 = CARTESIAN_POINT ( 'NONE',  ( 4.999999999999992006, -8.660254037844389075, -17.24999999999996092 ) ) ;
#11033 = CARTESIAN_POINT ( 'NONE',  ( -10.81189881249999729, -6.242252689847864744, -79.96875000204838102 ) ) ;
#11034 = CARTESIAN_POINT ( 'NONE',  ( 10.81189881249999907, 6.242252689847868297, -61.21875000204838102 ) ) ;
#11035 = FACE_OUTER_BOUND ( 'NONE', #40829, .T. ) ;
#11036 = CARTESIAN_POINT ( 'NONE',  ( 10.81189881249999551, -6.242252689847874514, -37.65625000204836681 ) ) ;
#11037 = CARTESIAN_POINT ( 'NONE',  ( 10.81189881249999551, -6.242252689847874514, -49.46875000204836681 ) ) ;
#11038 = CARTESIAN_POINT ( 'NONE',  ( -4.999999999999996447, 8.660254037844387298, -186.0000000000000000 ) ) ;
#11039 = CARTESIAN_POINT ( 'NONE',  ( 10.81189881249999551, -6.242252689847874514, -151.4687500020483810 ) ) ;
#11040 = CARTESIAN_POINT ( 'NONE',  ( -5.000000000000003553, -8.660254037844383745, -121.0000000000000000 ) ) ;
#11041 = CARTESIAN_POINT ( 'NONE',  ( -10.81189881249999729, 1.324075727343319199E-15, -128.2812500020483810 ) ) ;
#11042 = CARTESIAN_POINT ( 'NONE',  ( 9.999999999999998224, 0.000000000000000000, -186.8750000040967905 ) ) ;
#11043 = CARTESIAN_POINT ( 'NONE',  ( 7.070501591499377789E-16, 11.54700538379251284, -85.62499999999997158 ) ) ;
#11044 = CARTESIAN_POINT ( 'NONE',  ( 10.81189881249999729, 0.000000000000000000, -15.03125000204835793 ) ) ;
#11045 = ORIENTED_EDGE ( 'NONE', *, *, #19567, .T. ) ;
#11046 = CARTESIAN_POINT ( 'NONE',  ( 10.81189881249999551, -6.242252689847874514, -102.1562500020483952 ) ) ;
#11047 = CARTESIAN_POINT ( 'NONE',  ( -4.999999999999996447, 8.660254037844387298, -121.8750000040967905 ) ) ;
#11048 = CARTESIAN_POINT ( 'NONE',  ( -4.999999999999996447, 8.660254037844387298, -8.999999999999952038 ) ) ;
#11049 = CARTESIAN_POINT ( 'NONE',  ( 5.000000000000000000, 8.660254037844385522, -33.62500000409676915 ) ) ;
#11050 = CARTESIAN_POINT ( 'NONE',  ( -10.00000000000051337, 5.773502691895962435, -74.87499999999997158 ) ) ;
#11051 = CARTESIAN_POINT ( 'NONE',  ( 10.81189881249999729, 0.000000000000000000, -40.53125000204838102 ) ) ;
#11052 = CARTESIAN_POINT ( 'NONE',  ( 10.81189881249999551, -6.242252689847874514, -151.6562500020484094 ) ) ;
#11053 = EDGE_CURVE ( 'NONE', #26894, #39570, #13628, .T. ) ;
#11054 = CARTESIAN_POINT ( 'NONE',  ( -5.405949406249996869, 9.363379034771805109, -126.8437500020483952 ) ) ;
#11055 = ORIENTED_EDGE ( 'NONE', *, *, #13238, .F. ) ;
#11056 = CARTESIAN_POINT ( 'NONE',  ( 0.000000000000000000, 0.000000000000000000, -200.0000000000000000 ) ) ;
#11057 = ORIENTED_EDGE ( 'NONE', *, *, #26285, .T. ) ;
#11058 = ORIENTED_EDGE ( 'NONE', *, *, #23349, .F. ) ;
#11060 = VERTEX_POINT ( 'NONE', #12991 ) ;
#11059 = CARTESIAN_POINT ( 'NONE',  ( -5.405949406249996869, 9.363379034771805109, -113.3437500020483810 ) ) ;
#11061 = CARTESIAN_POINT ( 'NONE',  ( -5.000000000000003553, -8.660254037844383745, -41.87500000409677625 ) ) ;
#11062 = CARTESIAN_POINT ( 'NONE',  ( -5.405949406250003975, -9.363379034771801557, -186.3437500020483810 ) ) ;
#11063 = AXIS2_PLACEMENT_3D ( 'NONE', #35718, #24957, #18883 ) ;
#11064 = CARTESIAN_POINT ( 'NONE',  ( 5.405949406249999534, 9.363379034771803333, -41.59375000204837391 ) ) ;
#11065 = DIRECTION ( 'NONE',  ( -1.000000000000000000, 0.000000000000000000, 0.000000000000000000 ) ) ;
#11066 = CARTESIAN_POINT ( 'NONE',  ( 9.999999999999612754, 5.773502691896477579, -152.2500000040967336 ) ) ;
#11067 = CARTESIAN_POINT ( 'NONE',  ( 10.81189881249999551, -6.242252689847874514, -173.9687500020483810 ) ) ;
#11068 = CARTESIAN_POINT ( 'NONE',  ( 5.405949406249999534, 9.363379034771803333, -163.0937500020484094 ) ) ;
#11069 = CARTESIAN_POINT ( 'NONE',  ( -2.121150477449813534E-15, -11.54700538379251284, -76.25000000409676204 ) ) ;
#11070 = CARTESIAN_POINT ( 'NONE',  ( -5.405949406250003975, -9.363379034771801557, -144.3437500020483810 ) ) ;
#11071 = CARTESIAN_POINT ( 'NONE',  ( -5.405949406249996869, 9.363379034771805109, -153.8437500020483810 ) ) ;
#11072 = CYLINDRICAL_SURFACE ( 'NONE', #29511, 9.999999999999998224 ) ;
#11073 = CARTESIAN_POINT ( 'NONE',  ( 4.999999999999992006, -8.660254037844389075, -182.2500000000000000 ) ) ;
#11074 = CARTESIAN_POINT ( 'NONE',  ( -10.81189881249999907, -6.242252689847864744, -88.96875000204836681 ) ) ;
#11075 = DIRECTION ( 'NONE',  ( -0.000000000000000000, -0.000000000000000000, 1.000000000000000000 ) ) ;
#11076 = CARTESIAN_POINT ( 'NONE',  ( 10.81189881249999907, 6.242252689847868297, -58.40625000204838102 ) ) ;
#11077 = CARTESIAN_POINT ( 'NONE',  ( -9.999999999999479527, -5.773502691896549521, -97.50000000409676204 ) ) ;
#11078 = EDGE_CURVE ( 'NONE', #23210, #37997, #16019, .T. ) ;
#11079 = CARTESIAN_POINT ( 'NONE',  ( 10.81189881249999551, -6.242252689847874514, -176.9687500020483810 ) ) ;
#11080 = CARTESIAN_POINT ( 'NONE',  ( 10.81189881249999907, 6.242252689847868297, -118.4062500020484094 ) ) ;
#11081 = CARTESIAN_POINT ( 'NONE',  ( -5.405949406250003975, -9.363379034771801557, -150.5312500020483810 ) ) ;
#11082 =( BOUNDED_CURVE ( )  B_SPLINE_CURVE ( 2, ( #40169, #23787, #20531, #4143, #30490, #918, #4360 ),
 .UNSPECIFIED., .F., .F. ) 
 B_SPLINE_CURVE_WITH_KNOTS ( ( 3, 2, 2, 3 ),
 ( 0.5111940298507463565, 0.5124378109452737418, 0.5136815920398011270, 0.5149253731343285123 ),
 .UNSPECIFIED. ) 
 CURVE ( )  GEOMETRIC_REPRESENTATION_ITEM ( )  RATIONAL_B_SPLINE_CURVE ( ( 0.9999999999999880096, 0.8660254037844506980, 1.000000000000000000, 0.8660254037844387076, 1.000000000000000000, 0.8660254037844267172, 1.000000000000011990 ) ) 
 REPRESENTATION_ITEM ( '' )  );
#11083 = CYLINDRICAL_SURFACE ( 'NONE', #19959, 9.999999999999998224 ) ;
#11084 = CARTESIAN_POINT ( 'NONE',  ( -10.81189881249999729, 6.242252689847871849, -44.40625000204836681 ) ) ;
#11085 = CARTESIAN_POINT ( 'NONE',  ( -9.999999999999998224, 1.224646799147353059E-15, -130.6250000040967620 ) ) ;
#11086 = CARTESIAN_POINT ( 'NONE',  ( -5.000000000000003553, -8.660254037844383745, -107.4999999999999858 ) ) ;
#11087 = ORIENTED_EDGE ( 'NONE', *, *, #23326, .F. ) ;
#11088 = CARTESIAN_POINT ( 'NONE',  ( -5.405949406250003975, -9.363379034771801557, -125.0312500020483952 ) ) ;
#11089 = CARTESIAN_POINT ( 'NONE',  ( 9.999999999999998224, 0.000000000000000000, -146.3750000040967905 ) ) ;
#11090 = CARTESIAN_POINT ( 'NONE',  ( 10.81189881249999551, -6.242252689847874514, -187.6562500020484379 ) ) ;
#11091 = ORIENTED_EDGE ( 'NONE', *, *, #1313, .T. ) ;
#11092 = CARTESIAN_POINT ( 'NONE',  ( -5.000000000000003553, -8.660254037844383745, -53.49999999999996447 ) ) ;
#11093 = CARTESIAN_POINT ( 'NONE',  ( -10.81189881249999729, 6.242252689847871849, -177.7187500020483810 ) ) ;
#11094 = CARTESIAN_POINT ( 'NONE',  ( 7.070501591499377789E-16, 11.54700538379251284, -59.00000000409676915 ) ) ;
#11095 = CYLINDRICAL_SURFACE ( 'NONE', #30680, 20.00000000000000355 ) ;
#11096 = CARTESIAN_POINT ( 'NONE',  ( -9.999999999999998224, 0.000000000000000000, -99.99999999999998579 ) ) ;
#11097 = CARTESIAN_POINT ( 'NONE',  ( 5.405949406249992428, -9.363379034771808662, -73.78125000204838102 ) ) ;
#11098 = CARTESIAN_POINT ( 'NONE',  ( -10.81189881249999729, 6.242252689847871849, -54.90625000204836681 ) ) ;
#11099 = CARTESIAN_POINT ( 'NONE',  ( -2.121150477449813534E-15, -11.54700538379251284, -49.25000000409676915 ) ) ;
#11100 = CARTESIAN_POINT ( 'NONE',  ( 10.81189881249999729, 0.000000000000000000, -10.34375000204834549 ) ) ;
#11101 = CARTESIAN_POINT ( 'NONE',  ( -9.999999999999998224, 1.224646799147353059E-15, -135.1250000040967620 ) ) ;
#11102 = CARTESIAN_POINT ( 'NONE',  ( -10.81189881249999729, 1.324075727343319199E-15, -176.2812500020484094 ) ) ;
#11103 = LOCAL_TIME ( 11, 57, 6.000000000000000000, #6471 ) ;
#11104 = CARTESIAN_POINT ( 'NONE',  ( -2.293366432827344421E-15, -12.48450537969573659, -1.906250002048359704 ) ) ;
#11105 = CARTESIAN_POINT ( 'NONE',  ( -4.999999999999996447, 8.660254037844387298, -148.5000000000000000 ) ) ;
#11106 = DIRECTION ( 'NONE',  ( -0.000000000000000000, -0.000000000000000000, -1.000000000000000000 ) ) ;
#11107 = CARTESIAN_POINT ( 'NONE',  ( 7.070501591499376803E-16, 11.54700538379251284, -177.1250000000000000 ) ) ;
#11108 = LINE ( 'NONE', #24091, #6895 ) ;
#11109 = VECTOR ( 'NONE', #1761, 1000.000000000000000 ) ;
#11111 = ORIENTED_EDGE ( 'NONE', *, *, #2221, .T. ) ;
#11110 = CARTESIAN_POINT ( 'NONE',  ( 10.81189881249999729, 0.000000000000000000, -88.53125000204838102 ) ) ;
#11112 = DIRECTION ( 'NONE',  ( 0.000000000000000000, 0.000000000000000000, 1.000000000000000000 ) ) ;
#11114 = ORIENTED_EDGE ( 'NONE', *, *, #33743, .T. ) ;
#11113 = CARTESIAN_POINT ( 'NONE',  ( -2.121150477449813534E-15, -11.54700538379251284, -122.7500000040967905 ) ) ;
#11115 = EDGE_LOOP ( 'NONE', ( #30612, #22075, #23671, #29032 ) ) ;
#11116 = CARTESIAN_POINT ( 'NONE',  ( 10.81189881249999729, 6.242252689847867408, -40.21875000204835970 ) ) ;
#11117 = CARTESIAN_POINT ( 'NONE',  ( -10.81189881249999729, 1.324075727343319199E-15, -24.59375000204835970 ) ) ;
#11118 = CARTESIAN_POINT ( 'NONE',  ( -10.81189881249999729, 1.324075727343319199E-15, -12.78125000204835615 ) ) ;
#11119 = CARTESIAN_POINT ( 'NONE',  ( 5.405949406249999534, 9.363379034771803333, -61.09375000204836681 ) ) ;
#11120 = LINE ( 'NONE', #41104, #22218 ) ;
#11121 = CARTESIAN_POINT ( 'NONE',  ( -5.000000000000003553, -8.660254037844383745, -45.99999999999998579 ) ) ;
#11122 = CARTESIAN_POINT ( 'NONE',  ( 10.81189881249999907, 6.242252689847868297, -181.2187500020484094 ) ) ;
#11123 = CARTESIAN_POINT ( 'NONE',  ( 5.405949406249992428, -9.363379034771808662, -168.0937500020484094 ) ) ;
#11124 = AXIS2_PLACEMENT_3D ( 'NONE', #14446, #27638, #21367 ) ;
#11125 =( BOUNDED_CURVE ( )  B_SPLINE_CURVE ( 2, ( #30841, #8609, #37521, #21763, #7964, #17865, #21328 ),
 .UNSPECIFIED., .F., .F. ) 
 B_SPLINE_CURVE_WITH_KNOTS ( ( 3, 2, 2, 3 ),
 ( 0.4626865671641792743, 0.4639303482587066596, 0.4651741293532339339, 0.4664179104477613191 ),
 .UNSPECIFIED. ) 
 CURVE ( )  GEOMETRIC_REPRESENTATION_ITEM ( )  RATIONAL_B_SPLINE_CURVE ( ( 0.9999999999999820144, 0.8660254037844566932, 1.000000000000000000, 0.8660254037844387076, 1.000000000000000000, 0.8660254037844267172, 1.000000000000011990 ) ) 
 REPRESENTATION_ITEM ( '' )  );
#11126 = CARTESIAN_POINT ( 'NONE',  ( -2.293366432827344421E-15, -12.48450537969573659, -177.2187500020484094 ) ) ;
#11127 = CYLINDRICAL_SURFACE ( 'NONE', #14284, 9.999999999999998224 ) ;
#11128 = FACE_OUTER_BOUND ( 'NONE', #34239, .T. ) ;
#11129 = CARTESIAN_POINT ( 'NONE',  ( -9.999999999999998224, 1.224646799147353059E-15, -140.7500000000000000 ) ) ;
#11130 = LINE ( 'NONE', #37691, #10173 ) ;
#11131 = LOCAL_TIME ( 11, 57, 6.000000000000000000, #9651 ) ;
#11132 = CARTESIAN_POINT ( 'NONE',  ( -10.81189881249999729, 1.324075727343319199E-15, -116.0937500020483810 ) ) ;
#11133 = LINE ( 'NONE', #18253, #42479 ) ;
#11134 = CARTESIAN_POINT ( 'NONE',  ( 10.81189881249999907, 6.242252689847868297, -82.40625000204836681 ) ) ;
#11135 = ADVANCED_FACE ( 'NONE', ( #39130 ), #26187, .F. ) ;
#11136 = CARTESIAN_POINT ( 'NONE',  ( -5.405949406250003975, -9.363379034771801557, -103.8437500020483810 ) ) ;
#11137 = CARTESIAN_POINT ( 'NONE',  ( 7.644554776091147741E-16, 12.48450537969573659, -65.46875000204838102 ) ) ;
#11138 = ADVANCED_FACE ( 'NONE', ( #19906 ), #39548, .T. ) ;
#11139 = CARTESIAN_POINT ( 'NONE',  ( -10.81189881249999729, 1.324075727343319199E-15, -80.28125000204838102 ) ) ;
#11140 = CARTESIAN_POINT ( 'NONE',  ( 9.999999999999996447, -5.773502691896262640, -151.0000000040967905 ) ) ;
#11141 = CARTESIAN_POINT ( 'NONE',  ( 5.000000000000000000, 8.660254037844385522, -127.7499999999999716 ) ) ;
#11142 = EDGE_CURVE ( 'NONE', #8957, #25614, #28004, .T. ) ;
#11143 = CARTESIAN_POINT ( 'NONE',  ( 5.405949406249992428, -9.363379034771808662, -154.7812500020484094 ) ) ;
#11144 = CARTESIAN_POINT ( 'NONE',  ( 10.81189881249999551, -6.242252689847874514, -169.6562500020484094 ) ) ;
#11145 = VECTOR ( 'NONE', #6142, 1000.000000000000000 ) ;
#11146 = DIRECTION ( 'NONE',  ( -0.000000000000000000, -0.000000000000000000, -1.000000000000000000 ) ) ;
#11147 = CARTESIAN_POINT ( 'NONE',  ( 7.644554776091147741E-16, 12.48450537969573659, -104.4687500020483668 ) ) ;
#11148 = CARTESIAN_POINT ( 'NONE',  ( -4.999999999999996447, 8.660254037844387298, -120.3750000040967905 ) ) ;
#11149 = CARTESIAN_POINT ( 'NONE',  ( -2.121150477449813534E-15, -11.54700538379251284, -71.37499999999997158 ) ) ;
#11150 = CARTESIAN_POINT ( 'NONE',  ( -5.405949406249996869, 9.363379034771805109, -1.031250002048372805 ) ) ;
#11151 = CARTESIAN_POINT ( 'NONE',  ( 5.000000000000000000, 8.660254037844385522, -84.62500000409677625 ) ) ;
#11152 = CARTESIAN_POINT ( 'NONE',  ( -9.999999999999998224, 1.224646799147353059E-15, -141.1250000040967905 ) ) ;
#11153 = CARTESIAN_POINT ( 'NONE',  ( -2.293366432827344421E-15, -12.48450537969573659, -100.9062500020483952 ) ) ;
#11154 = CARTESIAN_POINT ( 'NONE',  ( -2.293366432827344421E-15, -12.48450537969573659, -73.90625000204836681 ) ) ;
#11155 = CARTESIAN_POINT ( 'NONE',  ( 7.070501591499377789E-16, 11.54700538379251284, -77.00000000409677625 ) ) ;
#11156 = CARTESIAN_POINT ( 'NONE',  ( 9.999999999999998224, 0.000000000000000000, -97.99999999999998579 ) ) ;
#11157 = CARTESIAN_POINT ( 'NONE',  ( -10.81189881249999729, 1.324075727343319199E-15, -36.59375000204836681 ) ) ;
#11158 = ORIENTED_EDGE ( 'NONE', *, *, #19624, .T. ) ;
#11159 = CARTESIAN_POINT ( 'NONE',  ( -10.81189881249999907, -6.242252689847864744, -198.6562500020484094 ) ) ;
#11160 = CARTESIAN_POINT ( 'NONE',  ( -5.405949406249996869, 9.363379034771805109, -28.03125000204837036 ) ) ;
#11161 = CARTESIAN_POINT ( 'NONE',  ( 10.81189881249999551, -6.242252689847874514, -16.46875000204836326 ) ) ;
#11162 = LINE ( 'NONE', #15034, #36535 ) ;
#11163 = ADVANCED_FACE ( 'NONE', ( #19696 ), #32879, .F. ) ;
#11164 = CARTESIAN_POINT ( 'NONE',  ( -5.000000000000003553, -8.660254037844383745, -5.875000004096770034 ) ) ;
#11165 = CARTESIAN_POINT ( 'NONE',  ( 5.405949406249992428, -9.363379034771808662, -127.7812500020483810 ) ) ;
#11166 = VECTOR ( 'NONE', #34156, 1000.000000000000000 ) ;
#11167 = EDGE_CURVE ( 'NONE', #38243, #36297, #4294, .T. ) ;
#11168 = CARTESIAN_POINT ( 'NONE',  ( 9.999999999999996447, -5.773502691896262640, -185.1250000000000284 ) ) ;
#11169 = CARTESIAN_POINT ( 'NONE',  ( -10.00000000000051337, 5.773502691895962435, -106.3749999999999716 ) ) ;
#11171 = ORIENTED_EDGE ( 'NONE', *, *, #34958, .F. ) ;
#11170 = CARTESIAN_POINT ( 'NONE',  ( -5.405949406250003975, -9.363379034771801557, -111.5312500020483810 ) ) ;
#11172 = CARTESIAN_POINT ( 'NONE',  ( 0.000000000000000000, 0.000000000000000000, -99.99999999999998579 ) ) ;
#11173 = EDGE_CURVE ( 'NONE', #41888, #12272, #11713, .T. ) ;
#11174 = EDGE_LOOP ( 'NONE', ( #9019, #26158, #30473, #8061 ) ) ;
#11175 = ORIENTED_EDGE ( 'NONE', *, *, #42683, .F. ) ;
#11176 = CARTESIAN_POINT ( 'NONE',  ( 5.405949406249999534, 9.363379034771803333, -38.78125000204838102 ) ) ;
#11177 = APPROVAL_ROLE ( '' ) ;
#11178 = AXIS2_PLACEMENT_3D ( 'NONE', #29644, #88, #29862 ) ;
#11179 = CARTESIAN_POINT ( 'NONE',  ( 7.644554776091147741E-16, 12.48450537969573659, -87.96875000204838102 ) ) ;
#11180 = FACE_OUTER_BOUND ( 'NONE', #15179, .T. ) ;
#11181 = EDGE_CURVE ( 'NONE', #33599, #36083, #27119, .T. ) ;
#11182 = CARTESIAN_POINT ( 'NONE',  ( 3.425473324849547030, 10.17518912463928338, -99.99999999999998579 ) ) ;
#11183 = DIRECTION ( 'NONE',  ( -0.000000000000000000, -0.000000000000000000, 1.000000000000000000 ) ) ;
#11184 = CARTESIAN_POINT ( 'NONE',  ( 5.405949406249999534, 9.363379034771803333, -161.7812500020484094 ) ) ;
#11185 = DIRECTION ( 'NONE',  ( 1.000000000000000000, 0.000000000000000000, 0.000000000000000000 ) ) ;
#11186 = CARTESIAN_POINT ( 'NONE',  ( 5.405949406249992428, -9.363379034771808662, -121.5937500020483952 ) ) ;
#11187 = CARTESIAN_POINT ( 'NONE',  ( -10.81189881249999729, 6.242252689847871849, -90.71875000204838102 ) ) ;
#11188 = CARTESIAN_POINT ( 'NONE',  ( 10.81189881249999729, 6.242252689847867408, -2.906250002048345493 ) ) ;
#11189 = CARTESIAN_POINT ( 'NONE',  ( 5.000000000000000000, 8.660254037844385522, -106.7499999999999858 ) ) ;
#11190 = CARTESIAN_POINT ( 'NONE',  ( -5.405949406249996869, 9.363379034771805109, -97.03125000204839523 ) ) ;
#11191 = CARTESIAN_POINT ( 'NONE',  ( 7.070501591499377789E-16, 11.54700538379251284, -174.5000000040967905 ) ) ;
#11192 = CARTESIAN_POINT ( 'NONE',  ( -2.293366432827344421E-15, -12.48450537969573659, -105.2187500020483952 ) ) ;
#11193 = CARTESIAN_POINT ( 'NONE',  ( 5.405949406249999534, 9.363379034771803333, -181.2812500020483810 ) ) ;
#11194 = ADVANCED_FACE ( 'NONE', ( #37387 ), #1573, .F. ) ;
#11195 = DIRECTION ( 'NONE',  ( -0.000000000000000000, -0.000000000000000000, 1.000000000000000000 ) ) ;
#11196 = CARTESIAN_POINT ( 'NONE',  ( -10.81189881249999729, 1.324075727343319199E-15, -194.2812500020484094 ) ) ;
#11197 = CARTESIAN_POINT ( 'NONE',  ( -10.81189881249999729, 6.242252689847871849, -51.71875000204836681 ) ) ;
#11198 = CARTESIAN_POINT ( 'NONE',  ( 4.999999999999992006, -8.660254037844389075, -169.1250000040967905 ) ) ;
#11199 = CARTESIAN_POINT ( 'NONE',  ( -10.81189881249999729, 6.242252689847871849, -6.906250002048365033 ) ) ;
#11200 = CARTESIAN_POINT ( 'NONE',  ( 10.81189881249999907, 6.242252689847868297, -20.71875000204837036 ) ) ;
#11201 = CARTESIAN_POINT ( 'NONE',  ( -5.000000000000003553, -8.660254037844383745, -193.3750000040967905 ) ) ;
#11202 = CARTESIAN_POINT ( 'NONE',  ( -10.81189881249999907, -6.242252689847864744, -132.4687500020483810 ) ) ;
#11203 = CARTESIAN_POINT ( 'NONE',  ( -10.00000000000000000, -5.773502691896251982, -97.12500000000000000 ) ) ;
#11204 = CARTESIAN_POINT ( 'NONE',  ( -5.405949406250003975, -9.363379034771801557, -32.03125000204837391 ) ) ;
#11205 = CARTESIAN_POINT ( 'NONE',  ( 7.070501591499377789E-16, 11.54700538379251284, -107.0000000040967763 ) ) ;
#11206 = CARTESIAN_POINT ( 'NONE',  ( 7.070501591499376803E-16, 11.54700538379251284, -102.1250000000000000 ) ) ;
#11207 = CARTESIAN_POINT ( 'NONE',  ( -9.999999999999998224, 5.773502691896259087, -53.87499999999997868 ) ) ;
#11208 = CARTESIAN_POINT ( 'NONE',  ( 10.81189881249999551, -6.242252689847874514, -121.6562500020483952 ) ) ;
#11209 = CARTESIAN_POINT ( 'NONE',  ( 5.405949406249999534, 9.363379034771803333, -110.7812500020483810 ) ) ;
#11210 = ORIENTED_EDGE ( 'NONE', *, *, #25689, .T. ) ;
#11211 = CARTESIAN_POINT ( 'NONE',  ( -9.999999999999998224, 5.773502691896259087, -100.7500000040967905 ) ) ;
#11212 = CARTESIAN_POINT ( 'NONE',  ( 10.81189881249999907, 6.242252689847868297, -164.9062500020484094 ) ) ;
#11213 = CARTESIAN_POINT ( 'NONE',  ( 5.405949406249992428, -9.363379034771808662, -58.59375000204835970 ) ) ;
#11214 = ORIENTED_EDGE ( 'NONE', *, *, #36754, .F. ) ;
#11215 = CARTESIAN_POINT ( 'NONE',  ( -2.121150477449813534E-15, -11.54700538379251284, -29.37499999999994671 ) ) ;
#11216 = AXIS2_PLACEMENT_3D ( 'NONE', #6458, #13326, #20448 ) ;
#11217 = CARTESIAN_POINT ( 'NONE',  ( 10.81189881249999729, 0.000000000000000000, -33.03125000204837391 ) ) ;
#11218 = CARTESIAN_POINT ( 'NONE',  ( -9.999999999999998224, 5.773502691896259087, -164.8749999999999716 ) ) ;
#11219 = CYLINDRICAL_SURFACE ( 'NONE', #18688, 9.999999999999998224 ) ;
#11220 = CARTESIAN_POINT ( 'NONE',  ( -9.999999999999998224, 5.773502691896259087, -30.25000000409675138 ) ) ;
#11221 = EDGE_CURVE ( 'NONE', #8276, #40345, #41475, .T. ) ;
#11222 = CARTESIAN_POINT ( 'NONE',  ( -9.999999999999998224, 1.224646799147353059E-15, -27.12500000409676204 ) ) ;
#11223 = CARTESIAN_POINT ( 'NONE',  ( 10.81189881249999729, 0.000000000000000000, -130.5312500020484094 ) ) ;
#11224 = CARTESIAN_POINT ( 'NONE',  ( -9.999999999999998224, 1.224646799147353059E-15, -46.24999999999998579 ) ) ;
#11225 = CARTESIAN_POINT ( 'NONE',  ( 10.00000000000051159, -5.773502691895965988, -119.5000000040967905 ) ) ;
#11226 = ORIENTED_EDGE ( 'NONE', *, *, #8320, .T. ) ;
#11228 = ORIENTED_EDGE ( 'NONE', *, *, #31748, .F. ) ;
#11227 = ORIENTED_EDGE ( 'NONE', *, *, #37760, .F. ) ;
#11229 = LINE ( 'NONE', #37571, #4543 ) ;
#11230 = CARTESIAN_POINT ( 'NONE',  ( 9.999999999999998224, 0.000000000000000000, -134.0000000000000000 ) ) ;
#11231 = CARTESIAN_POINT ( 'NONE',  ( -2.293366432827344421E-15, -12.48450537969573659, -166.7187500020484094 ) ) ;
#11232 = DIRECTION ( 'NONE',  ( -0.000000000000000000, -0.000000000000000000, -1.000000000000000000 ) ) ;
#11233 = CARTESIAN_POINT ( 'NONE',  ( -2.293366432827344421E-15, -12.48450537969573659, -12.21875000204837391 ) ) ;
#11234 = CARTESIAN_POINT ( 'NONE',  ( 9.999999999999998224, 0.000000000000000000, -129.5000000000000000 ) ) ;
#11235 = CARTESIAN_POINT ( 'NONE',  ( -5.405949406249996869, 9.363379034771805109, -147.8437500020483810 ) ) ;
#11236 = CARTESIAN_POINT ( 'NONE',  ( 5.405949406249992428, -9.363379034771808662, -133.5937500020483810 ) ) ;
#11237 = CARTESIAN_POINT ( 'NONE',  ( -10.81189881249999729, 1.324075727343319199E-15, -107.2812500020483810 ) ) ;
#11238 = CARTESIAN_POINT ( 'NONE',  ( 5.405949406249992428, -9.363379034771808662, -118.5937500020483810 ) ) ;
#11239 = CARTESIAN_POINT ( 'NONE',  ( -4.999999999999996447, 8.660254037844387298, -198.3750000040967905 ) ) ;
#11240 = CARTESIAN_POINT ( 'NONE',  ( 10.81189881249999551, -6.242252689847874514, -121.6562500020483952 ) ) ;
#11241 = CARTESIAN_POINT ( 'NONE',  ( 10.81189881249999729, 0.000000000000000000, -2.843750002048367698 ) ) ;
#11242 = CARTESIAN_POINT ( 'NONE',  ( 7.644554776091147741E-16, 12.48450537969573659, -129.9687500020483810 ) ) ;
#11243 = FACE_OUTER_BOUND ( 'NONE', #2022, .T. ) ;
#11244 = CARTESIAN_POINT ( 'NONE',  ( -5.000000000000003553, -8.660254037844383745, -196.3750000040967905 ) ) ;
#11245 = CARTESIAN_POINT ( 'NONE',  ( 4.999999999999992006, -8.660254037844389075, -150.7500000000000000 ) ) ;
#11246 = CARTESIAN_POINT ( 'NONE',  ( 5.000000000000000000, 8.660254037844385522, -21.24999999999996447 ) ) ;
#11247 = CARTESIAN_POINT ( 'NONE',  ( -10.81189881249999729, 1.324075727343319199E-15, -74.09375000204838102 ) ) ;
#11248 = CARTESIAN_POINT ( 'NONE',  ( -10.81189881249999907, -6.242252689847864744, -66.46875000204838102 ) ) ;
#11249 = CARTESIAN_POINT ( 'NONE',  ( 80.00000000000002842, 39.99999999999999289, -160.0000000000000000 ) ) ;
#11250 = CARTESIAN_POINT ( 'NONE',  ( -10.81189881249999729, 1.324075727343319199E-15, -38.28125000204838102 ) ) ;
#11251 = CARTESIAN_POINT ( 'NONE',  ( 5.405949406249999534, 9.363379034771803333, -49.09375000204838102 ) ) ;
#11252 = CARTESIAN_POINT ( 'NONE',  ( 9.999999999998456346, 5.773502691897149042, -53.25000000409673362 ) ) ;
#11253 = CARTESIAN_POINT ( 'NONE',  ( -2.293366432827344421E-15, -12.48450537969573659, -157.7187500020484094 ) ) ;
#11254 = CARTESIAN_POINT ( 'NONE',  ( -2.121150477449813534E-15, -11.54700538379251284, -117.8749999999999858 ) ) ;
#11255 = CARTESIAN_POINT ( 'NONE',  ( -10.81189881249999729, -6.242252689847864744, -128.1562500020483810 ) ) ;
#11256 = CARTESIAN_POINT ( 'NONE',  ( -2.121150477449813534E-15, -11.54700538379251284, -67.25000000409676204 ) ) ;
#11257 = CARTESIAN_POINT ( 'NONE',  ( 5.000000000000000000, 8.660254037844385522, -79.74999999999998579 ) ) ;
#11258 = CARTESIAN_POINT ( 'NONE',  ( -10.81189881249999729, -6.242252689847864744, -18.65625000204837036 ) ) ;
#11259 = ORIENTED_EDGE ( 'NONE', *, *, #27279, .T. ) ;
#11260 = CARTESIAN_POINT ( 'NONE',  ( 5.405949406249999534, 9.363379034771803333, -106.2812500020483810 ) ) ;
#11261 = CARTESIAN_POINT ( 'NONE',  ( 9.999999999999996447, -5.773502691896262640, -125.5000000040967763 ) ) ;
#11262 = CYLINDRICAL_SURFACE ( 'NONE', #16675, 9.999999999999998224 ) ;
#11263 = ADVANCED_FACE ( 'NONE', ( #723 ), #7830, .T. ) ;
#11264 = CARTESIAN_POINT ( 'NONE',  ( -5.000000000000003553, -8.660254037844383745, -37.37500000409676915 ) ) ;
#11265 = CARTESIAN_POINT ( 'NONE',  ( -9.999999999999998224, 1.224646799147353059E-15, -148.2500000000000000 ) ) ;
#11266 = CARTESIAN_POINT ( 'NONE',  ( 10.81189881249999551, -6.242252689847874514, -43.65625000204836681 ) ) ;
#11267 = LINE ( 'NONE', #24463, #4183 ) ;
#11268 = CARTESIAN_POINT ( 'NONE',  ( -5.405949406249996869, 9.363379034771805109, -154.0312500020484094 ) ) ;
#11269 = CARTESIAN_POINT ( 'NONE',  ( 5.405949406249999534, 9.363379034771803333, -130.0937500020483810 ) ) ;
#11270 = CARTESIAN_POINT ( 'NONE',  ( -9.999999999999998224, 1.224646799147353059E-15, -151.2500000000000000 ) ) ;
#11271 = ORIENTED_EDGE ( 'NONE', *, *, #19605, .T. ) ;
#11272 = DIRECTION ( 'NONE',  ( -0.000000000000000000, -0.000000000000000000, 1.000000000000000000 ) ) ;
#11274 = EDGE_CURVE ( 'NONE', #31274, #41628, #34304, .T. ) ;
#11273 = ORIENTED_EDGE ( 'NONE', *, *, #26456, .T. ) ;
#11275 = ORIENTED_EDGE ( 'NONE', *, *, #10422, .T. ) ;
#11276 = ORIENTED_EDGE ( 'NONE', *, *, #4580, .T. ) ;
#11277 = FACE_OUTER_BOUND ( 'NONE', #27644, .T. ) ;
#11278 = CARTESIAN_POINT ( 'NONE',  ( 5.405949406249999534, 9.363379034771803333, -190.0937500020483810 ) ) ;
#11279 = CARTESIAN_POINT ( 'NONE',  ( 5.405949406249992428, -9.363379034771808662, -37.59375000204837391 ) ) ;
#11280 = CARTESIAN_POINT ( 'NONE',  ( -2.121150477449813534E-15, -11.54700538379251284, -155.7500000040968189 ) ) ;
#11281 = CARTESIAN_POINT ( 'NONE',  ( -9.999999999999998224, 1.224646799147353059E-15, -34.24999999999997158 ) ) ;
#11282 = CARTESIAN_POINT ( 'NONE',  ( 10.81189881249999551, -6.242252689847874514, -172.4687500020483810 ) ) ;
#11283 = CARTESIAN_POINT ( 'NONE',  ( 5.405949406249992428, -9.363379034771808662, -159.0937500020484094 ) ) ;
#11284 = CARTESIAN_POINT ( 'NONE',  ( 9.999999999999998224, 0.000000000000000000, -200.0000000000000000 ) ) ;
#11285 = CARTESIAN_POINT ( 'NONE',  ( 5.405949406249992428, -9.363379034771808662, -145.5937500020483810 ) ) ;
#11286 = CARTESIAN_POINT ( 'NONE',  ( -5.405949406250003975, -9.363379034771801557, -146.0312500020483810 ) ) ;
#11287 = CARTESIAN_POINT ( 'NONE',  ( -2.293366432827344421E-15, -12.48450537969573659, -156.2187500020483810 ) ) ;
#11288 = CARTESIAN_POINT ( 'NONE',  ( 9.999999999999742428, 5.773502691896404748, -134.2500000040967905 ) ) ;
#11289 = LINE ( 'NONE', #33555, #23996 ) ;
#11290 = CARTESIAN_POINT ( 'NONE',  ( -9.999999999999998224, 1.224646799147353059E-15, -178.2500000000000284 ) ) ;
#11291 = CARTESIAN_POINT ( 'NONE',  ( -2.293366432827344421E-15, -12.48450537969573659, -91.71875000204838102 ) ) ;
#11292 = DIRECTION ( 'NONE',  ( -0.000000000000000000, -0.000000000000000000, -1.000000000000000000 ) ) ;
#11293 = CARTESIAN_POINT ( 'NONE',  ( 5.405949406249999534, 9.363379034771803333, -55.28125000204836681 ) ) ;
#11294 = CARTESIAN_POINT ( 'NONE',  ( -9.999999999999998224, 1.224646799147353059E-15, -168.1250000040967905 ) ) ;
#11295 = CARTESIAN_POINT ( 'NONE',  ( -5.405949406250003975, -9.363379034771801557, -178.8437500020483810 ) ) ;
#11296 = CARTESIAN_POINT ( 'NONE',  ( 5.405949406249999534, 9.363379034771803333, -113.7812500020483952 ) ) ;
#11297 = CARTESIAN_POINT ( 'NONE',  ( 10.81189881249999729, 6.242252689847867408, -155.9062500020483810 ) ) ;
#11298 = CARTESIAN_POINT ( 'NONE',  ( 0.000000000000000000, 0.000000000000000000, -99.99999999999998579 ) ) ;
#11299 = CARTESIAN_POINT ( 'NONE',  ( 7.644554776091147741E-16, 12.48450537969573659, -46.15625000204837391 ) ) ;
#11300 = CARTESIAN_POINT ( 'NONE',  ( 7.070501591499377789E-16, 11.54700538379251284, -128.0000000040967620 ) ) ;
#11301 = CARTESIAN_POINT ( 'NONE',  ( 7.070501591499377789E-16, 11.54700538379251284, -108.1249999999999716 ) ) ;
#11302 = EDGE_CURVE ( 'NONE', #10534, #21693, #13345, .T. ) ;
#11303 = ORIENTED_EDGE ( 'NONE', *, *, #29515, .F. ) ;
#11304 = CARTESIAN_POINT ( 'NONE',  ( -10.81189881249999729, 1.324075727343319199E-15, -125.2812500020483668 ) ) ;
#11305 = CARTESIAN_POINT ( 'NONE',  ( 5.000000000000000000, 8.660254037844385522, -146.1250000040967905 ) ) ;
#11306 = CARTESIAN_POINT ( 'NONE',  ( 9.999999999999998224, 0.000000000000000000, -6.499999999999977796 ) ) ;
#11307 = CARTESIAN_POINT ( 'NONE',  ( -5.405949406249996869, 9.363379034771805109, -178.0312500020483810 ) ) ;
#11308 = ORIENTED_EDGE ( 'NONE', *, *, #13750, .F. ) ;
#11309 = CARTESIAN_POINT ( 'NONE',  ( 5.000000000000000000, 8.660254037844385522, -49.74999999999998579 ) ) ;
#11310 = CARTESIAN_POINT ( 'NONE',  ( -2.293366432827344421E-15, -12.48450537969573659, -174.2187500020484094 ) ) ;
#11311 = CARTESIAN_POINT ( 'NONE',  ( -4.999999999999996447, 8.660254037844387298, -60.37500000409676204 ) ) ;
#11312 = LINE ( 'NONE', #37657, #5853 ) ;
#11313 = CARTESIAN_POINT ( 'NONE',  ( -9.999999999999998224, 1.224646799147353059E-15, -130.2499999999999716 ) ) ;
#11314 = CARTESIAN_POINT ( 'NONE',  ( 10.81189881249999551, -6.242252689847874514, -64.65625000204839523 ) ) ;
#11315 = CARTESIAN_POINT ( 'NONE',  ( 10.81189881249999551, -6.242252689847874514, -55.65625000204837391 ) ) ;
#11316 = CARTESIAN_POINT ( 'NONE',  ( 9.999999999999996447, -5.773502691896262640, -46.00000000409675494 ) ) ;
#11317 = CARTESIAN_POINT ( 'NONE',  ( -10.81189881249999907, -6.242252689847864744, -4.968750002048355263 ) ) ;
#11318 = CARTESIAN_POINT ( 'NONE',  ( -4.999999999999996447, 8.660254037844387298, -157.8750000040967905 ) ) ;
#11319 = CARTESIAN_POINT ( 'NONE',  ( 10.81189881249999907, 6.242252689847868297, -179.9062500020484094 ) ) ;
#11320 = CARTESIAN_POINT ( 'NONE',  ( 4.999999999999992006, -8.660254037844389075, -87.74999999999998579 ) ) ;
#11321 = DIRECTION ( 'NONE',  ( -1.000000000000000000, 0.000000000000000000, 0.000000000000000000 ) ) ;
#11322 = ORIENTED_EDGE ( 'NONE', *, *, #35080, .T. ) ;
#11323 = CARTESIAN_POINT ( 'NONE',  ( 9.999999999999998224, 0.000000000000000000, -58.99999999999997158 ) ) ;
#11324 = DIRECTION ( 'NONE',  ( -0.000000000000000000, -0.000000000000000000, 1.000000000000000000 ) ) ;
#11325 = DIRECTION ( 'NONE',  ( 1.000000000000000000, 0.000000000000000000, 0.000000000000000000 ) ) ;
#11327 = ORIENTED_EDGE ( 'NONE', *, *, #353, .F. ) ;
#11326 = CARTESIAN_POINT ( 'NONE',  ( -2.293366432827344421E-15, -12.48450537969573659, -88.90625000204838102 ) ) ;
#11328 = DIRECTION ( 'NONE',  ( 1.000000000000000000, 0.000000000000000000, 0.000000000000000000 ) ) ;
#11329 = EDGE_CURVE ( 'NONE', #17679, #5036, #15553, .T. ) ;
#11331 = ORIENTED_EDGE ( 'NONE', *, *, #20682, .F. ) ;
#11330 = CARTESIAN_POINT ( 'NONE',  ( 9.999999999999479527, 5.773502691896553074, -92.25000000409676204 ) ) ;
#11332 = ORIENTED_EDGE ( 'NONE', *, *, #15911, .F. ) ;
#11333 = CARTESIAN_POINT ( 'NONE',  ( 5.405949406249992428, -9.363379034771808662, -37.59375000204837391 ) ) ;
#11334 = CARTESIAN_POINT ( 'NONE',  ( -10.81189881249999729, 6.242252689847871849, -27.71875000204838102 ) ) ;
#11335 = CARTESIAN_POINT ( 'NONE',  ( -5.405949406250003975, -9.363379034771801557, -12.53125000204835615 ) ) ;
#11337 = VERTEX_POINT ( 'NONE', #8683 ) ;
#11336 = CARTESIAN_POINT ( 'NONE',  ( -5.405949406249996869, 9.363379034771805109, -60.84375000204836681 ) ) ;
#11338 = CARTESIAN_POINT ( 'NONE',  ( -10.00000000000051337, 5.773502691895962435, -92.87499999999998579 ) ) ;
#11339 = CARTESIAN_POINT ( 'NONE',  ( -9.999999999999998224, 5.773502691896259087, -37.37499999999995737 ) ) ;
#11340 = CARTESIAN_POINT ( 'NONE',  ( 10.81189881249999729, 0.000000000000000000, -187.3437500020483810 ) ) ;
#11341 =( BOUNDED_SURFACE ( )  B_SPLINE_SURFACE ( 1, 2, ( 
 ( #1018, #24115, #27339, #37251, #20853, #28632, #12197, #37907, #38757, #15434, #12406, #41764, #28840, #21924, #5530, #41557, #31657, #8977, #1877, #11990, #8351, #27985, #41114, #28203, #18470, #25186, #31877, #15640, #28421, #22354, #41973, #41337, #31234, #38535, #25599, #38326, #18679, #8768, #18250, #18038, #34684, #11553, #25387, #15222, #35104, #22144, #24976, #2092, #24762, #2308, #38117, #5317, #21502, #35318, #8562, #9183, #5747, #35530, #18900, #32081, #2515, #1657, #15005, #14790, #5104, #11774, #31442, #21712, #34893, #6578, #22989, #2930, #5959, #9397, #26017, #26432, #42395, #36146, #29892, #42186, #10228, #39169, #39583, #32500, #6167, #19735, #3348, #32915, #29680, #22561, #124, #3138, #332, #16480, #36357, #16059, #35739, #13245, #19307, #9602, #13033, #16265, #10019, #2715, #29251, #19521, #23197, #6790, #12826, #22776, #19945, #25806, #35937, #6378, #32705, #15847, #33134, #29464, #42606, #26227, #23415, #39375, #9811, #13451, #3562, #19109, #26646, #16696, #39795, #32292, #29047, #12613, #38963, #20795, #30322, #40011, #546, #37195, #40216, #34202, #756, #4618, #11073, #3772, #33983, #24276, #4190, #14298, #965, #40851, #17763, #13877, #30107, #30745, #40632, #20367, #27498, #36992, #21012, #37421, #27713, #33556, #7864, #4404, #30958, #27073, #1389, #33767, #36564, #3980, #7010, #33352, #17543, #14520, #11290, #1176, #16906, #20162, #13663, #26856, #17121, #10649, #10441, #23633, #17335, #36778, #10863, #7215, #20578, #30538, #14083, #23842, #7427, #27282, #40419, #24054, #7644, #4831, #21874, #38063, #38273, #18414, #24705, #25127, #2036, #8719, #35267, #35052, #25339, #12147, #22092, #41282, #1823, #41923, #17977, #21657, #34838, #31177, #38486, #5479, #41059, #1606, #5262, #8930, #11503, #37851, #11935, #15380, #18629, #24918, #31824, #8294, #32032, #2260, #5051, #28579, #21440, #14736, #34624, #8504, #28148, #18197, #31603, #31388, #41709, #2460, #8076, #11720, #5701, #18852, #15166, #27929, #14949, #24485, #28364, #15591, #41502, #28792, #21227, #37637, #34412, #22945, #38915, #19897, #6533, #35688, #3301, #9346, #32240, #22515, #39120, #16010, #6117, #9554, #19262, #36099, #33081, #38703, #42345, #71, #19685, #29205, #5906, #32454, #29847, #28997, #32870, #19059, #3089, #9138, #22306, #12568, #39324, #2880, #15801, #2667, #12981, #12777, #9970, #25969, #23150, #29628, #35479, #9764, #13195, #22728, #16429, #19474, #16645, #36311, #35893, #42137, #26388, #39540, #6330, #6744, #32660, #3508, #12355, #25552, #16217, #25762, #29417, #42557, #26178, #24224, #40170, #285, #26811, #13406, #39749, #10815, #30695, #1127, #24008, #10183, #4570, #7818, #20966, #39963, #10392, #14250, #37150, #23788, #27453, #17286, #23369, #27024, #36943, #10601, #37375, #16858, #40589, #36519, #13830, #27230, #6957, #40373, #7385, #14034, #20532, #504, #919, #33721, #7596, #11031, #20750, #34152, #17712, #26599, #17075, #20320, #20114, #33303, #4144, #30491, #3728, #30061, #33937, #13619, #23582, #4361, #36730, #7168, #33514, #17500, #3937, #30273, #711, #18587, #28533, #5008, #8247, #5648, #11245, #28104, #41232, #24442, #31774, #28312, #4782, #37588, #11670, #2203, #17930, #1561, #18370, #21827, #1991, #31345, #41452, #14692, #38438, #25083, #11458, #35006, #27881, #8032, #41013, #14904, #34578, #24659, #24870, #37801, #11887, #8882, #14472, #18150, #15336, #38228, #1775, #21176, #21394, #30907, #31128, #8673, #34366, #21615, #27666, #40804, #38019, #15117, #8463, #34794, #5214, #31558, #5435, #41665, #12100, #25295, #22045, #35217, #1343, #6487, #29158, #39280, #25916, #23101, #21, #38863, #12308, #12930, #22895, #2621, #9713, #19216, #3249, #36051, #9922, #15753, #19635, #16167, #32818, #12521, #13144, #15962, #18796, #28951, #31985, #15543, #29363, #16376, #29576, #42502, #28745, #36263, #26339, #39491, #42088, #25713, #2411, #26125, #42297, #41871, #35846, #25506, #2828, #12719, #39068, #38654, #35427, #9089, #22257, #32406, #3040, #5855, #19009, #9507, #32615, #22676, #32194, #19425, #6279, #9291, #22462, #35639, #6067, #20861, #16594, #4466, #14147, #37262, #237, #27777, #40482, #27994, #37700, #24771, #31023, #27564, #11355, #24549, #33253, #19845, #11563, #1026, #33029, #17608, #29797, #7926, #24341, #4256, #6693, #10135, #27347, #40913, #10929, #37482, #31242, #13359, #3459, #24123, #8142, #17398, #6904, #21075, #4680, #34264, #1453, #23314, #14588, #30804, #1669, #17828, #21290, #30596, #36469, #34476, #20058, #7712, #14366, #1242, #4898, #26551, #34045, #40698, #18046, #14798, #11141, #41123, #39699, #15013, #5324, #38124, #18478, #5112, #28848, #38334, #31665, #15441, #12621, #8569, #15229, #2724, #35112, #8359, #32303, #2099, #41345, #38764, #11997, #28210, #21933, #5754, #32088, #11781, #15857, #35326, #29055, #18907, #5966, #41772, #25397, #18686, #8777, #41983, #21719, #31884, #24983, #18261, #31450, #28428, #5537, #2314, #8984, #35537, #28639, #42194, #19117, #41564, #21510, #15648, #37915, #12204, #38543, #22151, #34902, #34692, #25193, #1884, #2522, #12413, #25606, #9190, #22361, #30118, #33362, #3782, #9612, #22786, #39806, #19956, #6588, #10238, #132, #35748, #9819, #19744, #23000, #7020, #42404, #26656, #22569, #39386, #10028, #6176, #23209, #36155, #39594, #32924, #26026, #26442, #3358, #36367, #36574, #6802, #23425, #13463, #20173, #42615, #3147, #555, #19316, #16490, #29689, #32510, #16916, #33144, #12836, #2939, #13255, #25814, #39179, #35946, #3572, #16706, #29903, #26237, #341, #6389, #38970, #9406, #19530, #16068, #32714, #29261, #16274, #29473, #13042, #37002, #40430, #23853, #24287, #34424, #40021, #975, #1401, #21022, #30547, #7226, #7437, #31188, #30334, #34213, #20377, #4415, #10451, #23643, #13887, #40644, #20590, #17133, #33566, #14310, #17344, #11301, #33778, #24495, #30971, #36789, #11086, #14531, #24066, #4629, #20806, #17988, #37648, #4200, #3990, #7875, #17775, #40226, #27725, #14093, #40861, #8088, #4843, #10660, #21238, #37432, #13675, #27294, #26867, #10873, #764, #37208, #27083, #7655, #33994, #17554, #30755, #1188, #27510, #28804, #18641, #11514, #28375, #25138, #41515, #25565, #18209, #2473, #41069, #15178, #28590, #24716, #41721, #11947, #15393, #38284, #1833, #2271, #21885, #12158, #12367, #25351, #15602, #32044, #41936, #18425, #21668, #19070, #37862, #8731, #35063, #8307, #38717, #38497, #31399, #21452, #5491, #9150, #14961, #28159, #31835, #35279, #8941, #2048, #22105, #41293, #22318, #5712, #24931, #18863, #11732, #34635, #38075, #35491, #5273, #8515, #5919, #34850, #1618, #14747, #27940, #31615, #5062, #39550, #6342, #25772, #12789, #6970, #6127, #9981, #38925, #22956, #29008, #42148, #32466, #16441, #25980, #35699, #9356, #32881, #35905, #29858, #39132, #296, #6754, #12579, #29640, #19908, #42569, #23160, #39337, #36530, #13417, #9565, #22526, #26399, #36323, #16021, #33093, #32672, #16657, #3521, #23380, #29217, #26612, #83, #39760, #22739, #10195, #29428, #32251, #42356, #2678, #19271, #13206, #15812, #2891, #19485, #3100, #16229, #12993, #26189, #9776, #36110, #6544, #19698, #3312, #37601, #514, #17299, #30504, #13629, #20978, #17513, #36741, #26821, #931, #7831, #7179, #33525, #7608, #11043, #33951, #20545, #30709, #3948, #27679, #14262, #724, #24237, #17086, #39974, #30285, #4155, #23801, #13843, #14047, #27038, #1139, #40817, #3739, #7397, #34165, #27465, #36955, #10405, #40182, #20126, #20332, #40600, #23596, #10827, #16869, #30072, #10613, #4373, #33733, #27243, #40384, #20762, #24020, #17724, #37161, #30919, #37388, #4584, #1354, #14484, #11257, #24454, #33314, #12319, #31996, #28116, #1574, #2217, #12113, #34590, #28544, #8473, #35229, #41676, #41884, #5021, #8892, #5447, #25306, #1787, #2422, #5226, #8044, #18162, #21190, #4794, #18598, #38451, #22056, #31785, #17942, #25517, #15555, #28757, #31356, #14916, #5660, #15346, #31570, #18811, #25094, #31141, #34805, #2002, #18381, #34378, #24670, #14703, #27893, #21627, #35018, #41026, #11469, #15129, #21838, #28325, #8258, #8685, #41464, #37815, #21404, #41243, #11684, #24881, #38030, #11898, #38240, #9724, #39503, #26350, #36276, #12731, #15973, #13371, #19020, #35857, #6291, #32205, #9934, #36063, #12532, #2634, #19434, #23113, #25725, #9305, #26138, #29590, #22907, #39080, #6498, #22474, #3471, #32833, #19227, #34, #35650, #15764, #6081, #22689, #42309, #32417, #32626, #2839, #19647, #16606, #22269, #25931, #6707, #3262, #9519, #28961, #29169, #38665, #38874, #16391, #42098, #29375, #35440, #5866, #3052, #13156, #16178, #42517, #12943, #39290, #19859, #33044, #29809, #249, #9101, #36481, #23968, #14212, #36903, #4321, #33683, #30865, #7780, #3902, #20070, #20710, #30658, #10353, #17459, #26976, #10991, #1086, #17670, #23544, #27411, #37113, #40547, #20286, #20924, #23750, #26563, #36693, #39712, #23329, #7557, #24186, #37333, #33898, #6918, #1301, #34106, #4528, #7132, #33474, #10147, #33265, #7348, #3691, #879, #16819, #10564, #20496, #4108, #30018, #465, #13580, #26772, #40136, #10779, #39925, #17036, #17249, #40337, #30450, #30236, #27193, #13998, #675, #13794, #37761, #31733, #25046, #28494, #31519, #11627, #41411, #11845, #1519, #14432, #27626, #8205, #11207, #28060, #37547, #5175, #21575, #40974, #40765, #14653, #4962, #38188, #21353, #18329, #15297, #4742, #24405, #31305, #21788, #34538, #24612, #1948, #8632, #28275, #34968, #11418, #5392, #37978, #7986, #18544, #2163, #18110, #1737, #15074, #14863, #41186, #34755, #8423, #21138, #17888, #24833, #34324, #31086, #27842, #13712, #10488, #37245, #30155, #20418, #23677, #33606, #20209, #1225, #10698, #4025, #30581, #27760, #36824, #30371, #17812, #7476, #23464, #4662, #17170, #26901, #11121, #27120, #595, #37040, #20846, #4450, #40057, #31008, #7692, #1437, #34030, #21058, #14131, #40466, #33816, #23892, #14350, #7266, #4239, #801, #33398, #3822, #13925, #20627, #17381, #24106, #7911, #1011, #14570, #34249, #40261, #36611, #30791, #10277, #27332, #10914, #17592, #27549, #7059, #40682, #16958, #24324, #37467, #5310, #31869, #5098, #11767, #8123, #38110, #18244, #28196, #2300, #1652, #41106, #25177, #18030, #8343, #11546, #21494, #21275, #15426, #41329, #34675, #18462, #15631, #24753, #31435, #5740, #8553, #11339, #35310, #1871, #14782, #41754, #14998, #31226, #24968, #8761, #35096, #27978, #18893, #38320, #32073, #21917, #8970, #2084, #28413, #21704, #34886, #28624, #37900, #31649, #15214, #34461, #4883, #41551, #11982, #5522, #18672, #38528, #12190, #2508, #22136, #25381, #24534, #40897, #37683, #35929, #29457, #22768, #29040, #28834, #2708, #22347, #22983, #26010, #6370, #19727, #35730, #42387, #38747, #39162, #6159, #16052, #35523, #6571, #19300, #6783, #16473, #3554, #9804, #19514, #32908, #3341, #12605, #41965, #33127, #22554, #12399, #9594, #9176, #42600, #3129, #25799, #25592, #32283, #32494, #29672, #2922, #16258, #10011, #5952, #19102, #29243, #116, #38955, #42178, #13026, #26219, #39367, #36140, #15840, #13237, #32698, #23189, #26425, #39576, #9389, #12819, #36350, #19938, #30492, #30908, #41014, #3938, #7597, #8033, #27667, #27025, #20967, #24009, #17931, #27231, #31129, #37589, #30274, #17713, #21177, #30696, #40805, #27454, #24660, #1562, #40374, #13831, #14473, #24443, #4145, #11246, #20751, #4783, #34367, #11459, #17287, #14693, #1344, #27882, #14035, #37802, #17501, #20321, #920, #33515, #17076, #712, #40171, #10602, #23789, #36944, #7386, #20533, #33722, #10816, #37151, #33938, #4362, #1128, #14251, #37376, #40590, #11032, #24225, #7819, #34153, #4571, #9090, #5009, #21828, #35218, #31346, #5649, #35007, #22046, #2204, #8464, #8883, #28534, #18797, #19010, #31986, #22258, #38655, #5856, #25084, #28313, #25714, #1776, #5436, #18588, #18151, #12522, #2412, #25296, #32195, #14905, #8248, #41453, #41872, #34795, #21616, #38439, #15544, #28746, #12309, #24871, #25507, #31775, #2622, #35428, #15754, #5215, #38020, #11671, #31559, #28105, #28952, #15337, #42089, #41233, #18371, #41666, #21395, #34579, #1992, #15118, #11888, #38229, #8674, #12101, #19426, #6068, #29798, #39281, #32616, #16377, #13569, #453, #29364, #238, #22677, #39069, #13145, #36264, #9923, #19846, #12720, #33030, #36052, #20059, #23102, #26552, #35847, #25917, #42298, #3041, #2829, #26340, #6488, #13360, #35640, #9508, #9714, #39700, #10136, #6280, #16168, #6694, #15963, #42503, #12931, #26126, #19217, #23315, #22896, #19636, #29577, #38864, #32819, #3250, #3680, #22, #9292, #33254, #39492, #3460, #36470, #16595, #29159, #6905, #16808, #30007, #22463, #32407, #24174, #21125, #37321, #37535, #30643, #14199 ),
 ( #4308, #30853, #1291, #10553, #39912, #31075, #20485, #10343, #37101, #36681, #27399, #1074, #23739, #26760, #10768, #7121, #1508, #40535, #10978, #7975, #20276, #7768, #33464, #23957, #7544, #20698, #34314, #663, #27614, #23531, #40326, #20911, #3890, #34094, #33886, #4515, #17447, #26965, #17659, #14420, #40754, #4730, #11196, #24394, #17878, #17025, #869, #4096, #30224, #13782, #40123, #36892, #7336, #33671, #17238, #30438, #13985, #27182, #2363, #1725, #28049, #2151, #5591, #28483, #15063, #25245, #41175, #22204, #8831, #37967, #18744, #11614, #34528, #24822, #41400, #38599, #34744, #37749, #8412, #38390, #35379, #40963, #1937, #15490, #21988, #31507, #8193, #21563, #32144, #31294, #35165, #21340, #5380, #11406, #24600, #14852, #41615, #5165, #18099, #4952, #15286, #18317, #12259, #28262, #25454, #31936, #11834, #12049, #28695, #25035, #41822, #21777, #18957, #9039, #38177, #8621, #5804, #14642, #34956, #27831, #18531, #31721, #36209, #36423, #42248, #3411, #42670, #6645, #39024, #26501, #42459, #2574, #29112, #15703, #42037, #13094, #32982, #16547, #26295, #12466, #6858, #10087, #23264, #12673, #25869, #29745, #39444, #26081, #191, #9460, #23052, #2993, #13312, #19795, #20010, #22627, #39648, #9879, #28902, #35801, #25660, #12887, #38815, #6232, #9242, #22412, #35590, #6018, #19168, #32358, #2782, #15910, #19378, #32566, #16118, #29315, #39232, #9670, #22843, #36005, #19584, #6441, #32767, #3203, #16329, #29528, #7076, #34047, #29961, #4044, #17400, #13523, #30598, #17188, #4258, #27134, #33415, #33833, #10717, #1028, #1244, #14150, #4469, #20863, #30806, #7284, #10506, #7928, #26709, #30386, #10931, #23481, #40277, #39861, #20225, #10295, #13941, #17611, #3842, #16976, #20647, #24125, #27349, #33622, #40485, #30174, #40700, #37265, #13728, #7714, #612, #36629, #26917, #819, #14369, #23693, #40075, #36840, #27566, #11144, #16761, #20437, #24343, #37485, #23911, #37056, #7494, #33202, #3633, #401, #27780, #11784, #17830, #31026, #21292, #5326, #14800, #24552, #40915, #21721, #24773, #18691, #27996, #31887, #38337, #1456, #18481, #8779, #31452, #41567, #28214, #25400, #2317, #41126, #14590, #15233, #25196, #15444, #1886, #38546, #28643, #31244, #34266, #12001, #41774, #41347, #34904, #15015, #34479, #21078, #37702, #11357, #28431, #18263, #24985, #21936, #11566, #34694, #8144, #38128, #37917, #8361, #4901, #35116, #21513, #12207, #5540, #4682, #2103, #8571, #18048, #1672, #5114, #31669, #13258, #2728, #35330, #19319, #18910, #9616, #26030, #5969, #8987, #35752, #32092, #26445, #22789, #39182, #32928, #2526, #22155, #42197, #42618, #35540, #9194, #35950, #6392, #19533, #32717, #25609, #3150, #6180, #3361, #16279, #39389, #19121, #38767, #12416, #32306, #15651, #29476, #32513, #13046, #5757, #22364, #22572, #26240, #9822, #15860, #29059, #23004, #28851, #12624, #25818, #38973, #41987, #36158, #9409, #2942, #29264, #16071, #42408, #12839, #16494, #6591, #19748, #29692, #136, #345, #40434, #13679, #29906, #23646, #7441, #33782, #16709, #17559, #37006, #33998, #20594, #7659, #767, #27086, #20380, #10455, #30552, #23429, #33570, #13466, #6806, #19961, #7024, #40025, #3993, #10664, #4205, #4419, #17348, #20812, #13893, #40229, #17136, #36792, #979, #36577, #30338, #26659, #33147, #3576, #20176, #7229, #23857, #14097, #37212, #27299, #1192, #30759, #33365, #10031, #10878, #14314, #24070, #39597, #23213, #39809, #36370, #10241, #3786, #16920, #30121, #558, #26870, #35019, #41677, #38031, #25307, #5448, #15347, #21628, #5867, #18599, #6082, #15765, #2840, #9102, #5661, #32206, #2635, #11899, #41244, #32418, #21839, #11685, #38452, #8474, #28758, #2423, #25095, #27514, #12114, #34806, #24882, #41885, #15556, #9306, #5227, #18382, #31786, #19021, #38241, #28326, #12320, #25518, #38666, #22270, #2003, #35441, #8893, #22475, #28962, #42099, #8686, #15130, #31571, #2218, #41465, #12533, #22057, #25726, #28545, #35230, #18812, #38875, #35651, #31997, #19228, #250, #35858, #26139, #16179, #39291, #25932, #6919, #16392, #9725, #36277, #33475, #29376, #36064, #23545, #13157, #29170, #10354, #22908, #19435, #16820, #32834, #6292, #35, #26564, #10148, #32627, #36694, #42310, #7133, #6499, #3053, #30019, #3263, #42518, #26351, #39713, #23330, #12944, #20287, #13372, #15974, #36482, #26773, #19860, #3472, #39504, #29591, #20071, #19648, #9935, #23114, #39081, #9520, #6708, #33045, #16607, #29810, #13581, #33266, #12732, #39926, #3692, #22690, #466, #40975, #10992, #4529, #40548, #4109, #3903, #20497, #40137, #40766, #1087, #24187, #37548, #10780, #17460, #13795, #14213, #23969, #33899, #10565, #24406, #37114, #24613, #34325, #21354, #27627, #37334, #7987, #21139, #30451, #17037, #8206, #40338, #30237, #27412, #26977, #17671, #20925, #880, #676, #30659, #23751, #36904, #30866, #34107, #27843, #7349, #33684, #7558, #4743, #13999, #17250, #1302, #14433, #11208, #17889, #27194, #31087, #7781, #11419, #1520, #14654, #20711, #4322, #37762, #15075, #41187, #8843, #2164, #25467, #31306, #37979, #5393, #38612, #9049, #8424, #34756, #18756, #11628, #1949, #5176, #28276, #1738, #22215, #34969, #41412, #12060, #9254, #18330, #11846, #42050, #31734, #15298, #4963, #28913, #25047, #21576, #35391, #8633, #24834, #18545, #2374, #28706, #31520, #12478, #31946, #25671, #15501, #2585, #38401, #22001, #28495, #41626, #5815, #38189, #25256, #21789, #14864, #28061, #35177, #5602, #41833, #12270, #32155, #18968, #38825, #15714, #34539, #18111, #201, #16770, #29538, #23064, #16340, #22638, #22423, #39034, #15922, #16558, #19595, #42680, #13322, #29325, #36015, #32368, #32777, #42469, #9680, #29123, #26511, #12896, #412, #10096, #39870, #3421, #13106, #39660, #23273, #6243, #35601, #26718, #16128, #6029, #3213, #2792, #36220, #39454, #19387, #19179, #6454, #42258, #12683, #6655, #9889, #3643, #25880, #9470, #26091, #36432, #32578, #35811, #19805, #32993, #29756, #6868, #3004, #20019, #26305, #29970, #33212, #13532, #39242, #22853, #13737, #33631, #16985, #27359, #20656, #1254, #7085, #26927, #23920, #14378, #27575, #40085, #10515, #37276, #30184, #20445, #23702, #4054, #20235, #40711, #10728, #17196, #30607, #27790, #36851, #30397, #17839, #11153, #37064, #828, #1035, #10304, #7295, #13950, #31035, #7504, #23492, #4690, #27143, #40286, #24352, #33843, #621, #4268, #20871, #4478, #17409, #1466, #7724, #14600, #34057, #21087, #14160, #40494, #10940, #24134, #37493, #17621, #30815, #7937, #33424, #3851, #34275, #36639, #34914, #12010, #38556, #8582, #2536, #8997, #8372, #11366, #18702, #35339, #5336, #41578, #18491, #41134, #40923, #14809, #34489, #35126, #38138, #31679, #31898, #5124, #11794, #8153, #21732, #18272, #28224, #4911, #2326, #31461, #18920, #28653, #15661, #21946, #2113, #15455, #41784, #24781, #24562, #37711, #34704, #21301, #15243, #18059, #25206, #28442, #37926, #31254, #24997, #1681, #28006, #38348, #8788, #22165, #11575, #21522, #1895, #12218, #15024, #41357, #5550, #25410, #5767, #32103, #2741, #23014, #26041, #10041, #13057, #16505, #12634, #15868, #32316, #9419, #35550, #3161, #39193, #19757, #25621, #29070, #42418, #32940, #3370, #42208, #25828, #26250, #5980, #38982, #22585, #35762, #38778, #19131, #12849, #39400, #36168, #6190, #6816, #9835, #23223, #6601, #39607, #32727, #16289, #9627, #22799, #29702, #19332, #35963, #32524, #9204, #22373, #2953, #29275, #6402, #42627, #26457, #19543, #33157, #36383, #16080, #41997, #148, #19971, #29488, #13268, #3587, #28862, #12426, #33376, #10252, #10888, #13902, #23867, #7667, #23654, #30347, #26669, #27095, #36801, #4003, #23439, #37220, #7239, #37444, #4428, #34225, #40444, #37015, #20820, #34006, #568, #29916, #21035, #10464, #357, #40237, #39820, #17357, #33791, #13687, #16721, #776, #36587, #13478, #30559, #4214, #40657, #7034, #20186, #20389, #17567, #26879, #16932, #988, #14106, #27307, #24080, #3796, #30767, #10673, #11097, #1199, #14326, #40034, #30131, #33582, #17146, #7455, #27522, #20604, #24300, #7887, #8099, #18221, #8741, #38296, #21250, #4857, #31627, #24506, #14758, #17999, #27953, #14545, #21895, #5075, #41081, #24942, #22113, #31201, #24728, #12169, #1846, #17788, #41730, #11525, #34436, #5500, #21463, #1629, #37873, #18650, #41528, #28171, #31844, #21681, #27737, #31411, #41305, #14972, #28600, #8318, #2281, #1414, #11743, #2060, #40873, #15190, #38086, #18437, #8526, #34647, #5284, #34862, #28387, #15402, #11958, #25359, #35075, #38507, #25148, #8950, #4641, #11314, #30985, #37659, #25572, #29225, #41945, #9157, #15610, #16030, #22965, #22326, #5927, #22747, #26197, #6350, #35707, #3108, #19079, #92, #29438, #15821, #39344, #32259, #12377, #2688, #19281, #16452, #12587, #28814, #29018, #16237, #13214, #18872, #22534, #36119, #42579, #9365, #38725, #42156, #9989, #35501, #13002, #25780, #25991, #32053, #2482, #38933, #19494, #6137, #32475, #2899, #35914, #42364, #32889, #12797, #3319, #9785, #39142, #32680, #6552, #9573, #19706, #29650, #39558, #26409, #35287, #5720, #17309, #27251, #6980, #939, #23606, #7617, #14058, #14271, #20135, #24030, #20553, #40391, #16879, #4381, #20341, #23168, #33322, #36331, #19917, #33742, #10836, #37169, #4164, #33106, #27472, #30721, #1148, #40608, #6762, #3530, #3747, #30082, #20771, #30512, #3956, #33959, #40193, #16665, #7187, #17094, #33534, #17520, #39769, #29865, #305, #36751, #7406, #13423, #26620, #30294, #36963, #733, #23389, #23809, #13852, #10203, #36539, #522, #13637, #26829, #39983, #10413, #27047, #10622, #34174, #8267, #31580, #1362, #5031, #17733, #27687, #4593, #34600, #41477, #40824, #24462, #41253, #2012, #24892, #11478, #21636, #37609, #18608, #5238, #34386, #15140, #8052, #30927, #21200, #37826, #35029, #31151, #14494, #4803, #34815, #31799, #37397, #41035, #11909, #18392, #27902, #11266, #17951, #28555, #1582, #28339, #14712, #1799, #7840, #20987, #24679, #38041, #21415, #18171, #31365, #11696, #14926, #8697, #28125, #21850, #25104, #8483, #38250, #5458, #2231, #15357, #11051, #24246, #23500, #19034, #35242, #35871, #3067, #25530, #19449, #42112, #26152, #32640, #33432, #38679, #42532, #39094, #16193, #35455, #36649, #38888, #41687, #9113, #12126, #38463, #9533, #29391, #12957, #22703, #8904, #22068, #39303, #12546, #22282, #19241, #16995, #12331, #32217, #7093, #9318, #25317, #20243, #5879, #2433, #10313, #15776, #32008, #25738, #6304, #3859, #18824, #5673, #15568, #28769, #41897, #2645, #2854, #29183, #22488, #35663, #28972, #6094, #32430, #15987, #42323, #12746, #25945, #30614, #24144, #1261, #27798, #40502, #34497, #40930, #40293, #628, #7943, #24569, #37283, #30823, #7730, #30404, #30192, #4061, #23708, #24359, #27366, #20878, #21094, #37071, #1042, #40092, #10947, #7514, #17416, #36859, #34282, #20663, #8160, #17846, #4918, #11160, #34064, #4697, #31043, #13957, #13745, #26934, #23927, #10524, #4486, #7302, #14385, #17628, #27151, #20452, #14167, #33640, #17203, #27582, #40720, #11372, #835, #10735, #33851, #1474, #4275, #37501, #14609, #37718, #21308, #41791, #34711, #12226, #15250, #42004, #2334, #5774, #1902, #5133, #21529, #41365, #24789, #35134, #28451, #9005, #14817, #18279, #31686, #22173, #35346, #31469, #15031, #15462, #37934, #28230, #11802, #25004, #11581, #25418, #18928, #38146, #38563, #18498, #2543, #32111, #9210, #8589, #15669, #28661, #28870, #21742, #12432, #41585, #18066, #34921, #31263, #28014, #25628, #38785, #22381, #35559, #41142, #1688, #8379, #5343, #2120, #12017, #25213, #38357, #8795, #21953, #5558, #18711, #31904, #29494, #3169, #29922, #22591, #6822, #2748, #19549, #32946, #29077, #3376, #32733, #19763, #42634, #6196, #6609, #26258, #16512, #16727, #29710, #19976, #36389, #3596, #22806, #26048, #23445, #42214, #16296, #26464, #38989, #13063, #12641, #35768, #25834, #39407, #33165, #19341, #32531, #36173, #39613, #154, #6408, #13274, #2959, #13486, #10049, #29281, #23229, #16086, #9426, #42425, #9842, #364, #39199, #12855, #9634, #26675, #39826, #32322, #35971, #10259, #5986, #23020, #19137, #15875, #7894, #26885, #37226, #16940, #33797, #20193, #33382, #10471, #14113, #33588, #40040, #30137, #994, #784, #1207, #4009, #14332, #34013, #3801, #27315, #4434, #23873, #7675, #7461, #37450, #27528, #17152, #13908, #30353, #36594, #575, #37021, #20827, #13693, #20611, #23661, #36808, #7246, #4223, #17573, #20396, #27101, #40450, #30775, #10894, #40244, #24087, #10680, #24307, #40663, #17364, #11104, #30565, #7042, #42558, #16430, #13620, #9765, #12778, #12982, #286, #10393, #16011, #19686, #20115, #39750, #6534, #25970, #26179, #7169, #6331 ) ),
 .UNSPECIFIED., .F., .F., .F. ) 
 B_SPLINE_SURFACE_WITH_KNOTS ( ( 2, 2 ),
 ( 3, 2, 2, 2, 2, 2, 2, 2, 2, 2, 2, 2, 2, 2, 2, 2, 2, 2, 2, 2, 2, 2, 2, 2, 2, 2, 2, 2, 2, 2, 2, 2, 2, 2, 2, 2, 2, 2, 2, 2, 2, 2, 2, 2, 2, 2, 2, 2, 2, 2, 2, 2, 2, 2, 2, 2, 2, 2, 2, 2, 2, 2, 2, 2, 2, 2, 2, 2, 2, 2, 2, 2, 2, 2, 2, 2, 2, 2, 2, 2, 2, 2, 2, 2, 2, 2, 2, 2, 2, 2, 2, 2, 2, 2, 2, 2, 2, 2, 2, 2, 2, 2, 2, 2, 2, 2, 2, 2, 2, 2, 2, 2, 2, 2, 2, 2, 2, 2, 2, 2, 2, 2, 2, 2, 2, 2, 2, 2, 2, 2, 2, 2, 2, 2, 2, 2, 2, 2, 2, 2, 2, 2, 2, 2, 2, 2, 2, 2, 2, 2, 2, 2, 2, 2, 2, 2, 2, 2, 2, 2, 2, 2, 2, 2, 2, 2, 2, 2, 2, 2, 2, 2, 2, 2, 2, 2, 2, 2, 2, 2, 2, 2, 2, 2, 2, 2, 2, 2, 2, 2, 2, 2, 2, 2, 2, 2, 2, 2, 2, 2, 2, 2, 2, 2, 2, 2, 2, 2, 2, 2, 2, 2, 2, 2, 2, 2, 2, 2, 2, 2, 2, 2, 2, 2, 2, 2, 2, 2, 2, 2, 2, 2, 2, 2, 2, 2, 2, 2, 2, 2, 2, 2, 2, 2, 2, 2, 2, 2, 2, 2, 2, 2, 2, 2, 2, 2, 2, 2, 2, 2, 2, 2, 2, 2, 2, 2, 2, 2, 2, 2, 2, 2, 2, 2, 2, 2, 2, 2, 2, 2, 2, 2, 2, 2, 2, 2, 2, 2, 2, 2, 2, 2, 2, 2, 2, 2, 2, 2, 2, 2, 2, 2, 2, 2, 2, 2, 2, 2, 2, 2, 2, 2, 2, 2, 2, 2, 2, 2, 2, 2, 2, 2, 2, 2, 2, 2, 2, 2, 2, 2, 2, 2, 2, 2, 2, 2, 2, 2, 2, 2, 2, 2, 2, 2, 2, 2, 2, 2, 2, 2, 2, 2, 2, 2, 2, 2, 2, 2, 2, 2, 2, 2, 2, 2, 2, 2, 2, 2, 2, 2, 2, 2, 2, 2, 2, 2, 2, 2, 2, 2, 2, 2, 2, 2, 2, 2, 2, 2, 2, 2, 2, 2, 2, 2, 2, 2, 2, 2, 2, 2, 2, 2, 2, 2, 2, 2, 2, 2, 2, 2, 2, 2, 2, 2, 2, 2, 2, 2, 2, 2, 2, 2, 2, 2, 2, 2, 2, 2, 2, 2, 2, 2, 2, 2, 2, 2, 2, 2, 2, 2, 2, 2, 2, 2, 2, 2, 2, 2, 2, 2, 2, 2, 2, 2, 2, 2, 2, 2, 2, 2, 2, 2, 2, 2, 2, 2, 2, 2, 2, 2, 2, 2, 2, 2, 2, 2, 2, 2, 2, 2, 2, 2, 2, 2, 2, 2, 2, 2, 2, 2, 2, 2, 2, 2, 2, 2, 2, 2, 2, 2, 2, 2, 2, 2, 2, 2, 2, 2, 2, 2, 2, 2, 2, 2, 2, 2, 2, 2, 2, 2, 2, 2, 2, 2, 2, 2, 2, 2, 2, 2, 2, 2, 2, 2, 2, 2, 2, 2, 2, 2, 2, 2, 2, 2, 2, 2, 2, 2, 2, 2, 2, 2, 2, 2, 2, 2, 2, 2, 2, 2, 2, 2, 2, 2, 2, 2, 2, 2, 2, 2, 2, 2, 2, 2, 2, 2, 2, 2, 2, 2, 2, 2, 2, 2, 2, 2, 2, 2, 2, 2, 2, 2, 2, 2, 2, 2, 2, 2, 2, 2, 2, 2, 2, 2, 2, 2, 2, 2, 2, 2, 2, 2, 2, 2, 2, 2, 2, 2, 2, 2, 2, 2, 2, 2, 2, 2, 2, 2, 2, 2, 2, 2, 2, 2, 2, 2, 2, 2, 2, 2, 2, 2, 2, 2, 2, 2, 2, 2, 2, 2, 2, 2, 2, 2, 2, 2, 2, 2, 2, 2, 2, 2, 2, 2, 2, 2, 2, 2, 2, 2, 2, 2, 2, 2, 2, 2, 2, 2, 2, 2, 2, 2, 2, 2, 2, 2, 2, 2, 2, 2, 2, 2, 2, 2, 2, 2, 2, 2, 2, 2, 2, 2, 2, 2, 2, 2, 2, 2, 2, 2, 2, 2, 2, 2, 2, 2, 2, 2, 2, 2, 2, 2, 2, 2, 2, 2, 2, 2, 2, 2, 2, 2, 2, 2, 2, 2, 2, 2, 2, 2, 2, 2, 2, 2, 2, 2, 2, 2, 2, 2, 2, 2, 2, 2, 2, 2, 2, 2, 2, 2, 2, 2, 2, 2, 2, 2, 2, 2, 2, 2, 2, 2, 2, 2, 2, 2, 2, 2, 2, 2, 2, 2, 2, 2, 2, 2, 2, 2, 2, 2, 2, 2, 2, 2, 2, 2, 2, 2, 2, 2, 3 ),
 ( 0.000000000000000000, 1.000000000000000000 ),
 ( 0.000000000000000000, 0.001243781094527363160, 0.002487562189054726321, 0.003731343283582089481, 0.004975124378109452641, 0.006218905472636816235, 0.007462686567164178962, 0.008706467661691542556, 0.009950248756218905283, 0.01119402985074626801, 0.01243781094527363247, 0.01368159203980099520, 0.01492537313432835792, 0.01616915422885572065, 0.01741293532338308511, 0.01865671641791044610, 0.01990049751243781057, 0.02114427860696517503, 0.02238805970149253602, 0.02363184079601990048, 0.02487562189054726494, 0.02611940298507462593, 0.02736318407960199039, 0.02860696517412935486, 0.02985074626865671585, 0.03109452736318408031, 0.03233830845771144130, 0.03358208955223880576, 0.03482587064676617022, 0.03606965174129353469, 0.03731343283582089221, 0.03855721393034825667, 0.03980099502487562113, 0.04104477611940298559, 0.04228855721393035005, 0.04353233830845771452, 0.04477611940298507204, 0.04601990049751243650, 0.04726368159203980096, 0.04850746268656716542, 0.04975124378109452988, 0.05099502487562188741, 0.05223880597014925187, 0.05348258706467661633, 0.05472636815920398079, 0.05597014925373134525, 0.05721393034825870971, 0.05845771144278606724, 0.05970149253731343170, 0.06094527363184079616, 0.06218905472636816062, 0.06343283582089552508, 0.06467661691542288260, 0.06592039800995025400, 0.06716417910447761153, 0.06840796019900496905, 0.06965174129353234045, 0.07089552238805969797, 0.07213930348258706937, 0.07338308457711442689, 0.07462686567164178442, 0.07587064676616915582, 0.07711442786069651334, 0.07835820895522388474, 0.07960199004975124226, 0.08084577114427861366, 0.08208955223880597118, 0.08333333333333332871, 0.08457711442786070011, 0.08582089552238805763, 0.08706467661691542903, 0.08830845771144278655, 0.08955223880597014408, 0.09079601990049751548, 0.09203980099502487300, 0.09328358208955224440, 0.09452736318407960192, 0.09577114427860695944, 0.09701492537313433084, 0.09825870646766168837, 0.09950248756218905977, 0.1007462686567164173, 0.1019900497512437748, 0.1032338308457711462, 0.1044776119402985037, 0.1057213930348258751, 0.1069651741293532327, 0.1082089552238805902, 0.1094527363184079616, 0.1106965174129353191, 0.1119402985074626905, 0.1131840796019900480, 0.1144278606965174194, 0.1156716417910447769, 0.1169154228855721345, 0.1181592039800995059, 0.1194029850746268634, 0.1206467661691542348, 0.1218905472636815923, 0.1231343283582089498, 0.1243781094527363212, 0.1256218905472636926, 0.1268656716417910502, 0.1281094527363184077, 0.1293532338308457652, 0.1305970149253731227, 0.1318407960199005080, 0.1330845771144278655, 0.1343283582089552231, 0.1355721393034825806, 0.1368159203980099381, 0.1380597014925373234, 0.1393034825870646809, 0.1405472636815920384, 0.1417910447761193959, 0.1430348258706467535, 0.1442786069651741387, 0.1455223880597014963, 0.1467661691542288538, 0.1480099502487562113, 0.1492537313432835688, 0.1504975124378109541, 0.1517412935323383116, 0.1529850746268656692, 0.1542288557213930267, 0.1554726368159203842, 0.1567164179104477695, 0.1579601990049751270, 0.1592039800995024845, 0.1604477611940298420, 0.1616915422885572273, 0.1629353233830845848, 0.1641791044776119424, 0.1654228855721392999, 0.1666666666666666574, 0.1679104477611940427, 0.1691542288557214002, 0.1703980099502487577, 0.1716417910447761153, 0.1728855721393034728, 0.1741293532338308581, 0.1753731343283582156, 0.1766169154228855731, 0.1778606965174129306, 0.1791044776119402882, 0.1803482587064676734, 0.1815920398009950310, 0.1828358208955223885, 0.1840796019900497460, 0.1853233830845771035, 0.1865671641791044888, 0.1878109452736318463, 0.1890547263681592038, 0.1902985074626865614, 0.1915422885572139189, 0.1927860696517413042, 0.1940298507462686617, 0.1952736318407960192, 0.1965174129353233767, 0.1977611940298507343, 0.1990049751243781195, 0.2002487562189054771, 0.2014925373134328346, 0.2027363184079601921, 0.2039800995024875496, 0.2052238805970149349, 0.2064676616915422924, 0.2077114427860696499, 0.2089552238805970075, 0.2101990049751243650, 0.2114427860696517503, 0.2126865671641791078, 0.2139303482587064653, 0.2151741293532338228, 0.2164179104477611804, 0.2176616915422885656, 0.2189054726368159232, 0.2201492537313432807, 0.2213930348258706382, 0.2226368159203980235, 0.2238805970149253810, 0.2251243781094527385, 0.2263681592039800961, 0.2276119402985074536, 0.2288557213930348389, 0.2300995024875621964, 0.2313432835820895539, 0.2325870646766169114, 0.2338308457711442689, 0.2350746268656716542, 0.2363184079601990117, 0.2375621890547263693, 0.2388059701492537268, 0.2400497512437810843, 0.2412935323383084696, 0.2425373134328358271, 0.2437810945273631846, 0.2450248756218905422, 0.2462686567164178997, 0.2475124378109452850, 0.2487562189054726425, 0.2500000000000000000, 0.2512437810945273853, 0.2524875621890547150, 0.2537313432835821003, 0.2549751243781094301, 0.2562189054726368154, 0.2574626865671642006, 0.2587064676616915304, 0.2599502487562189157, 0.2611940298507462455, 0.2624378109452736307, 0.2636815920398010160, 0.2649253731343283458, 0.2661691542288557311, 0.2674129353233830608, 0.2686567164179104461, 0.2699004975124378314, 0.2711442786069651611, 0.2723880597014925464, 0.2736318407960198762, 0.2748756218905472615, 0.2761194029850746468, 0.2773631840796019765, 0.2786069651741293618, 0.2798507462686566916, 0.2810945273631840768, 0.2823383084577114621, 0.2835820895522387919, 0.2848258706467661772, 0.2860696517412935069, 0.2873134328358208922, 0.2885572139303482775, 0.2898009950248756073, 0.2910447761194029925, 0.2922885572139303223, 0.2935323383084577076, 0.2947761194029850929, 0.2960199004975124226, 0.2972636815920398079, 0.2985074626865671377, 0.2997512437810945229, 0.3009950248756219082, 0.3022388059701492380, 0.3034825870646766233, 0.3047263681592039530, 0.3059701492537313383, 0.3072139303482587236, 0.3084577114427860534, 0.3097014925373134386, 0.3109452736318407684, 0.3121890547263681537, 0.3134328358208955390, 0.3146766169154228687, 0.3159203980099502540, 0.3171641791044776393, 0.3184079601990049690, 0.3196517412935323543, 0.3208955223880596841, 0.3221393034825870694, 0.3233830845771144546, 0.3246268656716417844, 0.3258706467661691697, 0.3271144278606964995, 0.3283582089552238847, 0.3296019900497512700, 0.3308457711442785998, 0.3320895522388059851, 0.3333333333333333148, 0.3345771144278607001, 0.3358208955223880854, 0.3370646766169154152, 0.3383084577114428004, 0.3395522388059701302, 0.3407960199004975155, 0.3420398009950249008, 0.3432835820895522305, 0.3445273631840796158, 0.3457711442786069456, 0.3470149253731343308, 0.3482587064676617161, 0.3495024875621890459, 0.3507462686567164312, 0.3519900497512437609, 0.3532338308457711462, 0.3544776119402985315, 0.3557213930348258613, 0.3569651741293532465, 0.3582089552238805763, 0.3594527363184079616, 0.3606965174129353469, 0.3619402985074626766, 0.3631840796019900619, 0.3644278606965173917, 0.3656716417910447769, 0.3669154228855721622, 0.3681592039800994920, 0.3694029850746268773, 0.3706467661691542070, 0.3718905472636815923, 0.3731343283582089776, 0.3743781094527363074, 0.3756218905472636926, 0.3768656716417910224, 0.3781094527363184077, 0.3793532338308457930, 0.3805970149253731227, 0.3818407960199005080, 0.3830845771144278378, 0.3843283582089552231, 0.3855721393034826083, 0.3868159203980099381, 0.3880597014925373234, 0.3893034825870646531, 0.3905472636815920384, 0.3917910447761194237, 0.3930348258706467535, 0.3942786069651741387, 0.3955223880597014685, 0.3967661691542288538, 0.3980099502487562391, 0.3992537313432835688, 0.4004975124378109541, 0.4017412935323382839, 0.4029850746268656692, 0.4042288557213930544, 0.4054726368159203842, 0.4067164179104477695, 0.4079601990049750992, 0.4092039800995024845, 0.4104477611940298698, 0.4116915422885571996, 0.4129353233830845848, 0.4141791044776119146, 0.4154228855721392999, 0.4166666666666666852, 0.4179104477611940149, 0.4191542288557214002, 0.4203980099502487300, 0.4216417910447761153, 0.4228855721393035005, 0.4241293532338308303, 0.4253731343283582156, 0.4266169154228855454, 0.4278606965174129306, 0.4291044776119403159, 0.4303482587064676457, 0.4315920398009950310, 0.4328358208955223607, 0.4340796019900497460, 0.4353233830845771313, 0.4365671641791044610, 0.4378109452736318463, 0.4390547263681592316, 0.4402985074626865614, 0.4415422885572139466, 0.4427860696517412764, 0.4440298507462686617, 0.4452736318407960470, 0.4465174129353233767, 0.4477611940298507620, 0.4490049751243780918, 0.4502487562189054771, 0.4514925373134328623, 0.4527363184079601921, 0.4539800995024875774, 0.4552238805970149071, 0.4564676616915422924, 0.4577114427860696777, 0.4589552238805970075, 0.4601990049751243927, 0.4614427860696517225, 0.4626865671641791078, 0.4639303482587064931, 0.4651741293532338228, 0.4664179104477612081, 0.4676616915422885379, 0.4689054726368159232, 0.4701492537313433084, 0.4713930348258706382, 0.4726368159203980235, 0.4738805970149253532, 0.4751243781094527385, 0.4763681592039801238, 0.4776119402985074536, 0.4788557213930348389, 0.4800995024875621686, 0.4813432835820895539, 0.4825870646766169392, 0.4838308457711442689, 0.4850746268656716542, 0.4863184079601989840, 0.4875621890547263693, 0.4888059701492537545, 0.4900497512437810843, 0.4912935323383084696, 0.4925373134328357994, 0.4937810945273631846, 0.4950248756218905699, 0.4962686567164178997, 0.4975124378109452850, 0.4987562189054726147, 0.5000000000000000000, 0.5012437810945273853, 0.5024875621890547706, 0.5037313432835820448, 0.5049751243781094301, 0.5062189054726368154, 0.5074626865671642006, 0.5087064676616915859, 0.5099502487562188602, 0.5111940298507462455, 0.5124378109452736307, 0.5136815920398010160, 0.5149253731343284013, 0.5161691542288556755, 0.5174129353233830608, 0.5186567164179104461, 0.5199004975124378314, 0.5211442786069652167, 0.5223880597014924909, 0.5236318407960198762, 0.5248756218905472615, 0.5261194029850746468, 0.5273631840796020320, 0.5286069651741293063, 0.5298507462686566916, 0.5310945273631840768, 0.5323383084577114621, 0.5335820895522388474, 0.5348258706467661217, 0.5360696517412935069, 0.5373134328358208922, 0.5385572139303482775, 0.5398009950248756628, 0.5410447761194029370, 0.5422885572139303223, 0.5435323383084577076, 0.5447761194029850929, 0.5460199004975124781, 0.5472636815920397524, 0.5485074626865671377, 0.5497512437810945229, 0.5509950248756219082, 0.5522388059701492935, 0.5534825870646765678, 0.5547263681592039530, 0.5559701492537313383, 0.5572139303482587236, 0.5584577114427861089, 0.5597014925373133831, 0.5609452736318407684, 0.5621890547263681537, 0.5634328358208955390, 0.5646766169154229242, 0.5659203980099501985, 0.5671641791044775838, 0.5684079601990049690, 0.5696517412935323543, 0.5708955223880597396, 0.5721393034825870139, 0.5733830845771143991, 0.5746268656716417844, 0.5758706467661691697, 0.5771144278606965550, 0.5783582089552238292, 0.5796019900497512145, 0.5808457711442785998, 0.5820895522388059851, 0.5833333333333333703, 0.5845771144278606446, 0.5858208955223880299, 0.5870646766169154152, 0.5883084577114428004, 0.5895522388059701857, 0.5907960199004974600, 0.5920398009950248452, 0.5932835820895522305, 0.5945273631840796158, 0.5957711442786070011, 0.5970149253731342753, 0.5982587064676616606, 0.5995024875621890459, 0.6007462686567164312, 0.6019900497512438164, 0.6032338308457710907, 0.6044776119402984760, 0.6057213930348258613, 0.6069651741293532465, 0.6082089552238806318, 0.6094527363184079061, 0.6106965174129352913, 0.6119402985074626766, 0.6131840796019900619, 0.6144278606965174472, 0.6156716417910447214, 0.6169154228855721067, 0.6181592039800994920, 0.6194029850746268773, 0.6206467661691542625, 0.6218905472636815368, 0.6231343283582089221, 0.6243781094527363074, 0.6256218905472636926, 0.6268656716417910779, 0.6281094527363184632, 0.6293532338308457375, 0.6305970149253731227, 0.6318407960199005080, 0.6330845771144278933, 0.6343283582089552786, 0.6355721393034825528, 0.6368159203980099381, 0.6380597014925373234, 0.6393034825870647087, 0.6405472636815920939, 0.6417910447761193682, 0.6430348258706467535, 0.6442786069651741387, 0.6455223880597015240, 0.6467661691542289093, 0.6480099502487561836, 0.6492537313432835688, 0.6504975124378109541, 0.6517412935323383394, 0.6529850746268657247, 0.6542288557213929989, 0.6554726368159203842, 0.6567164179104477695, 0.6579601990049751548, 0.6592039800995025400, 0.6604477611940298143, 0.6616915422885571996, 0.6629353233830845848, 0.6641791044776119701, 0.6654228855721393554, 0.6666666666666666297, 0.6679104477611940149, 0.6691542288557214002, 0.6703980099502487855, 0.6716417910447761708, 0.6728855721393034450, 0.6741293532338308303, 0.6753731343283582156, 0.6766169154228856009, 0.6778606965174129861, 0.6791044776119402604, 0.6803482587064676457, 0.6815920398009950310, 0.6828358208955224162, 0.6840796019900498015, 0.6853233830845770758, 0.6865671641791044610, 0.6878109452736318463, 0.6890547263681592316, 0.6902985074626866169, 0.6915422885572138911, 0.6927860696517412764, 0.6940298507462686617, 0.6952736318407960470, 0.6965174129353234322, 0.6977611940298507065, 0.6990049751243780918, 0.7002487562189054771, 0.7014925373134328623, 0.7027363184079602476, 0.7039800995024875219, 0.7052238805970149071, 0.7064676616915422924, 0.7077114427860696777, 0.7089552238805970630, 0.7101990049751243372, 0.7114427860696517225, 0.7126865671641791078, 0.7139303482587064931, 0.7151741293532338783, 0.7164179104477611526, 0.7176616915422885379, 0.7189054726368159232, 0.7201492537313433084, 0.7213930348258706937, 0.7226368159203979680, 0.7238805970149253532, 0.7251243781094527385, 0.7263681592039801238, 0.7276119402985075091, 0.7288557213930347833, 0.7300995024875621686, 0.7313432835820895539, 0.7325870646766169392, 0.7338308457711443245, 0.7350746268656715987, 0.7363184079601989840, 0.7375621890547263693, 0.7388059701492537545, 0.7400497512437811398, 0.7412935323383084141, 0.7425373134328357994, 0.7437810945273631846, 0.7450248756218905699, 0.7462686567164179552, 0.7475124378109452294, 0.7487562189054726147, 0.7500000000000000000, 0.7512437810945273853, 0.7524875621890547706, 0.7537313432835820448, 0.7549751243781094301, 0.7562189054726368154, 0.7574626865671642006, 0.7587064676616915859, 0.7599502487562188602, 0.7611940298507462455, 0.7624378109452736307, 0.7636815920398010160, 0.7649253731343284013, 0.7661691542288556755, 0.7674129353233830608, 0.7686567164179104461, 0.7699004975124378314, 0.7711442786069652167, 0.7723880597014924909, 0.7736318407960198762, 0.7748756218905472615, 0.7761194029850746468, 0.7773631840796020320, 0.7786069651741293063, 0.7798507462686566916, 0.7810945273631840768, 0.7823383084577114621, 0.7835820895522388474, 0.7848258706467661217, 0.7860696517412935069, 0.7873134328358208922, 0.7885572139303482775, 0.7898009950248756628, 0.7910447761194029370, 0.7922885572139303223, 0.7935323383084577076, 0.7947761194029850929, 0.7960199004975124781, 0.7972636815920397524, 0.7985074626865671377, 0.7997512437810945229, 0.8009950248756219082, 0.8022388059701492935, 0.8034825870646765678, 0.8047263681592039530, 0.8059701492537313383, 0.8072139303482587236, 0.8084577114427861089, 0.8097014925373133831, 0.8109452736318407684, 0.8121890547263681537, 0.8134328358208955390, 0.8146766169154229242, 0.8159203980099501985, 0.8171641791044775838, 0.8184079601990049690, 0.8196517412935323543, 0.8208955223880597396, 0.8221393034825870139, 0.8233830845771143991, 0.8246268656716417844, 0.8258706467661691697, 0.8271144278606965550, 0.8283582089552238292, 0.8296019900497512145, 0.8308457711442785998, 0.8320895522388059851, 0.8333333333333333703, 0.8345771144278606446, 0.8358208955223880299, 0.8370646766169154152, 0.8383084577114428004, 0.8395522388059701857, 0.8407960199004974600, 0.8420398009950248452, 0.8432835820895522305, 0.8445273631840796158, 0.8457711442786070011, 0.8470149253731342753, 0.8482587064676616606, 0.8495024875621890459, 0.8507462686567164312, 0.8519900497512438164, 0.8532338308457710907, 0.8544776119402984760, 0.8557213930348258613, 0.8569651741293532465, 0.8582089552238806318, 0.8594527363184079061, 0.8606965174129352913, 0.8619402985074626766, 0.8631840796019900619, 0.8644278606965174472, 0.8656716417910447214, 0.8669154228855721067, 0.8681592039800994920, 0.8694029850746268773, 0.8706467661691542625, 0.8718905472636815368, 0.8731343283582089221, 0.8743781094527363074, 0.8756218905472636926, 0.8768656716417910779, 0.8781094527363184632, 0.8793532338308457375, 0.8805970149253731227, 0.8818407960199005080, 0.8830845771144278933, 0.8843283582089552786, 0.8855721393034825528, 0.8868159203980099381, 0.8880597014925373234, 0.8893034825870647087, 0.8905472636815920939, 0.8917910447761193682, 0.8930348258706467535, 0.8942786069651741387, 0.8955223880597015240, 0.8967661691542289093, 0.8980099502487561836, 0.8992537313432835688, 0.9004975124378109541, 0.9017412935323383394, 0.9029850746268657247, 0.9042288557213929989, 0.9054726368159203842, 0.9067164179104477695, 0.9079601990049751548, 0.9092039800995025400, 0.9104477611940298143, 0.9116915422885571996, 0.9129353233830845848, 0.9141791044776119701, 0.9154228855721393554, 0.9166666666666666297, 0.9179104477611940149, 0.9191542288557214002, 0.9203980099502487855, 0.9216417910447761708, 0.9228855721393034450, 0.9241293532338308303, 0.9253731343283582156, 0.9266169154228856009, 0.9278606965174129861, 0.9291044776119402604, 0.9303482587064676457, 0.9315920398009950310, 0.9328358208955224162, 0.9340796019900498015, 0.9353233830845770758, 0.9365671641791044610, 0.9378109452736318463, 0.9390547263681592316, 0.9402985074626866169, 0.9415422885572138911, 0.9427860696517412764, 0.9440298507462686617, 0.9452736318407960470, 0.9465174129353234322, 0.9477611940298507065, 0.9490049751243780918, 0.9502487562189054771, 0.9514925373134328623, 0.9527363184079602476, 0.9539800995024875219, 0.9552238805970149071, 0.9564676616915422924, 0.9577114427860696777, 0.9589552238805970630, 0.9601990049751243372, 0.9614427860696517225, 0.9626865671641791078, 0.9639303482587064931, 0.9651741293532338783, 0.9664179104477611526, 0.9676616915422885379, 0.9689054726368159232, 0.9701492537313433084, 0.9713930348258706937, 0.9726368159203979680, 0.9738805970149253532, 0.9751243781094527385, 0.9763681592039801238, 0.9776119402985075091, 0.9788557213930347833, 0.9800995024875621686, 0.9813432835820895539, 0.9825870646766169392, 0.9838308457711443245, 0.9850746268656715987, 0.9863184079601989840, 0.9875621890547263693, 0.9888059701492537545, 0.9900497512437811398, 0.9912935323383084141, 0.9925373134328357994, 0.9937810945273631846, 0.9950248756218905699 ),
 .UNSPECIFIED. ) 
 GEOMETRIC_REPRESENTATION_ITEM ( )  RATIONAL_B_SPLINE_SURFACE ( (
 ( 1.000000000000000000, 0.8660254037844387076, 1.000000000000000000, 0.8660254037844387076, 1.000000000000000000, 0.8660254037844387076, 1.000000000000000000, 0.8660254037844387076, 1.000000000000000000, 0.8660254037844387076, 1.000000000000000000, 0.8660254037844387076, 1.000000000000000000, 0.8660254037844387076, 1.000000000000000000, 0.8660254037844387076, 1.000000000000000000, 0.8660254037844387076, 1.000000000000000000, 0.8660254037844387076, 1.000000000000000000, 0.8660254037844387076, 1.000000000000000000, 0.8660254037844387076, 1.000000000000000000, 0.8660254037844387076, 1.000000000000000000, 0.8660254037844387076, 1.000000000000000000, 0.8660254037844387076, 1.000000000000000000, 0.8660254037844387076, 1.000000000000000000, 0.8660254037844387076, 1.000000000000000000, 0.8660254037844387076, 1.000000000000000000, 0.8660254037844387076, 1.000000000000000000, 0.8660254037844387076, 1.000000000000000000, 0.8660254037844387076, 1.000000000000000000, 0.8660254037844387076, 1.000000000000000000, 0.8660254037844387076, 1.000000000000000000, 0.8660254037844387076, 1.000000000000000000, 0.8660254037844387076, 1.000000000000000000, 0.8660254037844387076, 1.000000000000000000, 0.8660254037844387076, 1.000000000000000000, 0.8660254037844387076, 1.000000000000000000, 0.8660254037844387076, 1.000000000000000000, 0.8660254037844387076, 1.000000000000000000, 0.8660254037844387076, 1.000000000000000000, 0.8660254037844387076, 1.000000000000000000, 0.8660254037844387076, 1.000000000000000000, 0.8660254037844387076, 1.000000000000000000, 0.8660254037844387076, 1.000000000000000000, 0.8660254037844387076, 1.000000000000000000, 0.8660254037844387076, 1.000000000000000000, 0.8660254037844387076, 1.000000000000000000, 0.8660254037844387076, 1.000000000000000000, 0.8660254037844387076, 1.000000000000000000, 0.8660254037844387076, 1.000000000000000000, 0.8660254037844387076, 1.000000000000000000, 0.8660254037844387076, 1.000000000000000000, 0.8660254037844387076, 1.000000000000000000, 0.8660254037844387076, 1.000000000000000000, 0.8660254037844387076, 1.000000000000000000, 0.8660254037844387076, 1.000000000000000000, 0.8660254037844387076, 1.000000000000000000, 0.8660254037844387076, 1.000000000000000000, 0.8660254037844387076, 1.000000000000000000, 0.8660254037844387076, 1.000000000000000000, 0.8660254037844387076, 1.000000000000000000, 0.8660254037844387076, 1.000000000000000000, 0.8660254037844387076, 1.000000000000000000, 0.8660254037844387076, 1.000000000000000000, 0.8660254037844387076, 1.000000000000000000, 0.8660254037844387076, 1.000000000000000000, 0.8660254037844387076, 1.000000000000000000, 0.8660254037844387076, 1.000000000000000000, 0.8660254037844387076, 1.000000000000000000, 0.8660254037844387076, 1.000000000000000000, 0.8660254037844387076, 1.000000000000000000, 0.8660254037844387076, 1.000000000000000000, 0.8660254037844387076, 1.000000000000000000, 0.8660254037844387076, 1.000000000000000000, 0.8660254037844387076, 1.000000000000000000, 0.8660254037844387076, 1.000000000000000000, 0.8660254037844387076, 1.000000000000000000, 0.8660254037844387076, 1.000000000000000000, 0.8660254037844387076, 1.000000000000000000, 0.8660254037844387076, 1.000000000000000000, 0.8660254037844387076, 1.000000000000000000, 0.8660254037844387076, 1.000000000000000000, 0.8660254037844387076, 1.000000000000000000, 0.8660254037844387076, 1.000000000000000000, 0.8660254037844387076, 1.000000000000000000, 0.8660254037844387076, 1.000000000000000000, 0.8660254037844387076, 1.000000000000000000, 0.8660254037844387076, 1.000000000000000000, 0.8660254037844387076, 1.000000000000000000, 0.8660254037844387076, 1.000000000000000000, 0.8660254037844387076, 1.000000000000000000, 0.8660254037844387076, 1.000000000000000000, 0.8660254037844387076, 1.000000000000000000, 0.8660254037844387076, 1.000000000000000000, 0.8660254037844387076, 1.000000000000000000, 0.8660254037844387076, 1.000000000000000000, 0.8660254037844387076, 1.000000000000000000, 0.8660254037844387076, 1.000000000000000000, 0.8660254037844387076, 1.000000000000000000, 0.8660254037844387076, 1.000000000000000000, 0.8660254037844387076, 1.000000000000000000, 0.8660254037844387076, 1.000000000000000000, 0.8660254037844387076, 1.000000000000000000, 0.8660254037844387076, 1.000000000000000000, 0.8660254037844387076, 1.000000000000000000, 0.8660254037844387076, 1.000000000000000000, 0.8660254037844387076, 1.000000000000000000, 0.8660254037844387076, 1.000000000000000000, 0.8660254037844387076, 1.000000000000000000, 0.8660254037844387076, 1.000000000000000000, 0.8660254037844387076, 1.000000000000000000, 0.8660254037844387076, 1.000000000000000000, 0.8660254037844387076, 1.000000000000000000, 0.8660254037844387076, 1.000000000000000000, 0.8660254037844387076, 1.000000000000000000, 0.8660254037844387076, 1.000000000000000000, 0.8660254037844387076, 1.000000000000000000, 0.8660254037844387076, 1.000000000000000000, 0.8660254037844387076, 1.000000000000000000, 0.8660254037844387076, 1.000000000000000000, 0.8660254037844387076, 1.000000000000000000, 0.8660254037844387076, 1.000000000000000000, 0.8660254037844387076, 1.000000000000000000, 0.8660254037844387076, 1.000000000000000000, 0.8660254037844387076, 1.000000000000000000, 0.8660254037844387076, 1.000000000000000000, 0.8660254037844387076, 1.000000000000000000, 0.8660254037844387076, 1.000000000000000000, 0.8660254037844387076, 1.000000000000000000, 0.8660254037844387076, 1.000000000000000000, 0.8660254037844387076, 1.000000000000000000, 0.8660254037844387076, 1.000000000000000000, 0.8660254037844387076, 1.000000000000000000, 0.8660254037844387076, 1.000000000000000000, 0.8660254037844387076, 1.000000000000000000, 0.8660254037844387076, 1.000000000000000000, 0.8660254037844387076, 1.000000000000000000, 0.8660254037844387076, 1.000000000000000000, 0.8660254037844387076, 1.000000000000000000, 0.8660254037844387076, 1.000000000000000000, 0.8660254037844387076, 1.000000000000000000, 0.8660254037844387076, 1.000000000000000000, 0.8660254037844387076, 1.000000000000000000, 0.8660254037844387076, 1.000000000000000000, 0.8660254037844387076, 1.000000000000000000, 0.8660254037844387076, 1.000000000000000000, 0.8660254037844387076, 1.000000000000000000, 0.8660254037844387076, 1.000000000000000000, 0.8660254037844387076, 1.000000000000000000, 0.8660254037844387076, 1.000000000000000000, 0.8660254037844387076, 1.000000000000000000, 0.8660254037844387076, 1.000000000000000000, 0.8660254037844387076, 1.000000000000000000, 0.8660254037844387076, 1.000000000000000000, 0.8660254037844387076, 1.000000000000000000, 0.8660254037844387076, 1.000000000000000000, 0.8660254037844387076, 1.000000000000000000, 0.8660254037844387076, 1.000000000000000000, 0.8660254037844387076, 1.000000000000000000, 0.8660254037844387076, 1.000000000000000000, 0.8660254037844387076, 1.000000000000000000, 0.8660254037844387076, 1.000000000000000000, 0.8660254037844387076, 1.000000000000000000, 0.8660254037844387076, 1.000000000000000000, 0.8660254037844387076, 1.000000000000000000, 0.8660254037844387076, 1.000000000000000000, 0.8660254037844387076, 1.000000000000000000, 0.8660254037844387076, 1.000000000000000000, 0.8660254037844387076, 1.000000000000000000, 0.8660254037844387076, 1.000000000000000000, 0.8660254037844387076, 1.000000000000000000, 0.8660254037844387076, 1.000000000000000000, 0.8660254037844387076, 1.000000000000000000, 0.8660254037844387076, 1.000000000000000000, 0.8660254037844387076, 1.000000000000000000, 0.8660254037844387076, 1.000000000000000000, 0.8660254037844387076, 1.000000000000000000, 0.8660254037844387076, 1.000000000000000000, 0.8660254037844387076, 1.000000000000000000, 0.8660254037844387076, 1.000000000000000000, 0.8660254037844387076, 1.000000000000000000, 0.8660254037844387076, 1.000000000000000000, 0.8660254037844387076, 1.000000000000000000, 0.8660254037844387076, 1.000000000000000000, 0.8660254037844387076, 1.000000000000000000, 0.8660254037844387076, 1.000000000000000000, 0.8660254037844387076, 1.000000000000000000, 0.8660254037844387076, 1.000000000000000000, 0.8660254037844387076, 1.000000000000000000, 0.8660254037844387076, 1.000000000000000000, 0.8660254037844387076, 1.000000000000000000, 0.8660254037844387076, 1.000000000000000000, 0.8660254037844387076, 1.000000000000000000, 0.8660254037844387076, 1.000000000000000000, 0.8660254037844387076, 1.000000000000000000, 0.8660254037844387076, 1.000000000000000000, 0.8660254037844387076, 1.000000000000000000, 0.8660254037844387076, 1.000000000000000000, 0.8660254037844387076, 1.000000000000000000, 0.8660254037844387076, 1.000000000000000000, 0.8660254037844387076, 1.000000000000000000, 0.8660254037844387076, 1.000000000000000000, 0.8660254037844387076, 1.000000000000000000, 0.8660254037844387076, 1.000000000000000000, 0.8660254037844387076, 1.000000000000000000, 0.8660254037844387076, 1.000000000000000000, 0.8660254037844387076, 1.000000000000000000, 0.8660254037844387076, 1.000000000000000000, 0.8660254037844387076, 1.000000000000000000, 0.8660254037844387076, 1.000000000000000000, 0.8660254037844387076, 1.000000000000000000, 0.8660254037844387076, 1.000000000000000000, 0.8660254037844387076, 1.000000000000000000, 0.8660254037844387076, 1.000000000000000000, 0.8660254037844387076, 1.000000000000000000, 0.8660254037844387076, 1.000000000000000000, 0.8660254037844387076, 1.000000000000000000, 0.8660254037844387076, 1.000000000000000000, 0.8660254037844387076, 1.000000000000000000, 0.8660254037844387076, 1.000000000000000000, 0.8660254037844387076, 1.000000000000000000, 0.8660254037844387076, 1.000000000000000000, 0.8660254037844387076, 1.000000000000000000, 0.8660254037844387076, 1.000000000000000000, 0.8660254037844387076, 1.000000000000000000, 0.8660254037844387076, 1.000000000000000000, 0.8660254037844387076, 1.000000000000000000, 0.8660254037844387076, 1.000000000000000000, 0.8660254037844387076, 1.000000000000000000, 0.8660254037844387076, 1.000000000000000000, 0.8660254037844387076, 1.000000000000000000, 0.8660254037844387076, 1.000000000000000000, 0.8660254037844387076, 1.000000000000000000, 0.8660254037844387076, 1.000000000000000000, 0.8660254037844387076, 1.000000000000000000, 0.8660254037844387076, 1.000000000000000000, 0.8660254037844387076, 1.000000000000000000, 0.8660254037844387076, 1.000000000000000000, 0.8660254037844387076, 1.000000000000000000, 0.8660254037844387076, 1.000000000000000000, 0.8660254037844387076, 1.000000000000000000, 0.8660254037844387076, 1.000000000000000000, 0.8660254037844387076, 1.000000000000000000, 0.8660254037844387076, 1.000000000000000000, 0.8660254037844387076, 1.000000000000000000, 0.8660254037844387076, 1.000000000000000000, 0.8660254037844387076, 1.000000000000000000, 0.8660254037844387076, 1.000000000000000000, 0.8660254037844387076, 1.000000000000000000, 0.8660254037844387076, 1.000000000000000000, 0.8660254037844387076, 1.000000000000000000, 0.8660254037844387076, 1.000000000000000000, 0.8660254037844387076, 1.000000000000000000, 0.8660254037844387076, 1.000000000000000000, 0.8660254037844387076, 1.000000000000000000, 0.8660254037844387076, 1.000000000000000000, 0.8660254037844387076, 1.000000000000000000, 0.8660254037844387076, 1.000000000000000000, 0.8660254037844387076, 1.000000000000000000, 0.8660254037844387076, 1.000000000000000000, 0.8660254037844387076, 1.000000000000000000, 0.8660254037844387076, 1.000000000000000000, 0.8660254037844387076, 1.000000000000000000, 0.8660254037844387076, 1.000000000000000000, 0.8660254037844387076, 1.000000000000000000, 0.8660254037844387076, 1.000000000000000000, 0.8660254037844387076, 1.000000000000000000, 0.8660254037844387076, 1.000000000000000000, 0.8660254037844387076, 1.000000000000000000, 0.8660254037844387076, 1.000000000000000000, 0.8660254037844387076, 1.000000000000000000, 0.8660254037844387076, 1.000000000000000000, 0.8660254037844387076, 1.000000000000000000, 0.8660254037844387076, 1.000000000000000000, 0.8660254037844387076, 1.000000000000000000, 0.8660254037844387076, 1.000000000000000000, 0.8660254037844387076, 1.000000000000000000, 0.8660254037844387076, 1.000000000000000000, 0.8660254037844387076, 1.000000000000000000, 0.8660254037844387076, 1.000000000000000000, 0.8660254037844387076, 1.000000000000000000, 0.8660254037844387076, 1.000000000000000000, 0.8660254037844387076, 1.000000000000000000, 0.8660254037844387076, 1.000000000000000000, 0.8660254037844387076, 1.000000000000000000, 0.8660254037844387076, 1.000000000000000000, 0.8660254037844387076, 1.000000000000000000, 0.8660254037844387076, 1.000000000000000000, 0.8660254037844387076, 1.000000000000000000, 0.8660254037844387076, 1.000000000000000000, 0.8660254037844387076, 1.000000000000000000, 0.8660254037844387076, 1.000000000000000000, 0.8660254037844387076, 1.000000000000000000, 0.8660254037844387076, 1.000000000000000000, 0.8660254037844387076, 1.000000000000000000, 0.8660254037844387076, 1.000000000000000000, 0.8660254037844387076, 1.000000000000000000, 0.8660254037844387076, 1.000000000000000000, 0.8660254037844387076, 1.000000000000000000, 0.8660254037844387076, 1.000000000000000000, 0.8660254037844387076, 1.000000000000000000, 0.8660254037844387076, 1.000000000000000000, 0.8660254037844387076, 1.000000000000000000, 0.8660254037844387076, 1.000000000000000000, 0.8660254037844387076, 1.000000000000000000, 0.8660254037844387076, 1.000000000000000000, 0.8660254037844387076, 1.000000000000000000, 0.8660254037844387076, 1.000000000000000000, 0.8660254037844387076, 1.000000000000000000, 0.8660254037844387076, 1.000000000000000000, 0.8660254037844387076, 1.000000000000000000, 0.8660254037844387076, 1.000000000000000000, 0.8660254037844387076, 1.000000000000000000, 0.8660254037844387076, 1.000000000000000000, 0.8660254037844387076, 1.000000000000000000, 0.8660254037844387076, 1.000000000000000000, 0.8660254037844387076, 1.000000000000000000, 0.8660254037844387076, 1.000000000000000000, 0.8660254037844387076, 1.000000000000000000, 0.8660254037844387076, 1.000000000000000000, 0.8660254037844387076, 1.000000000000000000, 0.8660254037844387076, 1.000000000000000000, 0.8660254037844387076, 1.000000000000000000, 0.8660254037844387076, 1.000000000000000000, 0.8660254037844387076, 1.000000000000000000, 0.8660254037844387076, 1.000000000000000000, 0.8660254037844387076, 1.000000000000000000, 0.8660254037844387076, 1.000000000000000000, 0.8660254037844387076, 1.000000000000000000, 0.8660254037844387076, 1.000000000000000000, 0.8660254037844387076, 1.000000000000000000, 0.8660254037844387076, 1.000000000000000000, 0.8660254037844387076, 1.000000000000000000, 0.8660254037844387076, 1.000000000000000000, 0.8660254037844387076, 1.000000000000000000, 0.8660254037844387076, 1.000000000000000000, 0.8660254037844387076, 1.000000000000000000, 0.8660254037844387076, 1.000000000000000000, 0.8660254037844387076, 1.000000000000000000, 0.8660254037844387076, 1.000000000000000000, 0.8660254037844387076, 1.000000000000000000, 0.8660254037844387076, 1.000000000000000000, 0.8660254037844387076, 1.000000000000000000, 0.8660254037844387076, 1.000000000000000000, 0.8660254037844387076, 1.000000000000000000, 0.8660254037844387076, 1.000000000000000000, 0.8660254037844387076, 1.000000000000000000, 0.8660254037844387076, 1.000000000000000000, 0.8660254037844387076, 1.000000000000000000, 0.8660254037844387076, 1.000000000000000000, 0.8660254037844387076, 1.000000000000000000, 0.8660254037844387076, 1.000000000000000000, 0.8660254037844387076, 1.000000000000000000, 0.8660254037844387076, 1.000000000000000000, 0.8660254037844387076, 1.000000000000000000, 0.8660254037844387076, 1.000000000000000000, 0.8660254037844387076, 1.000000000000000000, 0.8660254037844387076, 1.000000000000000000, 0.8660254037844387076, 1.000000000000000000, 0.8660254037844387076, 1.000000000000000000, 0.8660254037844387076, 1.000000000000000000, 0.8660254037844387076, 1.000000000000000000, 0.8660254037844387076, 1.000000000000000000, 0.8660254037844387076, 1.000000000000000000, 0.8660254037844387076, 1.000000000000000000, 0.8660254037844387076, 1.000000000000000000, 0.8660254037844387076, 1.000000000000000000, 0.8660254037844387076, 1.000000000000000000, 0.8660254037844387076, 1.000000000000000000, 0.8660254037844387076, 1.000000000000000000, 0.8660254037844387076, 1.000000000000000000, 0.8660254037844387076, 1.000000000000000000, 0.8660254037844387076, 1.000000000000000000, 0.8660254037844387076, 1.000000000000000000, 0.8660254037844387076, 1.000000000000000000, 0.8660254037844387076, 1.000000000000000000, 0.8660254037844387076, 1.000000000000000000, 0.8660254037844387076, 1.000000000000000000, 0.8660254037844387076, 1.000000000000000000, 0.8660254037844387076, 1.000000000000000000, 0.8660254037844387076, 1.000000000000000000, 0.8660254037844387076, 1.000000000000000000, 0.8660254037844387076, 1.000000000000000000, 0.8660254037844387076, 1.000000000000000000, 0.8660254037844387076, 1.000000000000000000, 0.8660254037844387076, 1.000000000000000000, 0.8660254037844387076, 1.000000000000000000, 0.8660254037844387076, 1.000000000000000000, 0.8660254037844387076, 1.000000000000000000, 0.8660254037844387076, 1.000000000000000000, 0.8660254037844387076, 1.000000000000000000, 0.8660254037844387076, 1.000000000000000000, 0.8660254037844387076, 1.000000000000000000, 0.8660254037844387076, 1.000000000000000000, 0.8660254037844387076, 1.000000000000000000, 0.8660254037844387076, 1.000000000000000000, 0.8660254037844387076, 1.000000000000000000, 0.8660254037844387076, 1.000000000000000000, 0.8660254037844387076, 1.000000000000000000, 0.8660254037844387076, 1.000000000000000000, 0.8660254037844387076, 1.000000000000000000, 0.8660254037844387076, 1.000000000000000000, 0.8660254037844387076, 1.000000000000000000, 0.8660254037844387076, 1.000000000000000000, 0.8660254037844387076, 1.000000000000000000, 0.8660254037844387076, 1.000000000000000000, 0.8660254037844387076, 1.000000000000000000, 0.8660254037844387076, 1.000000000000000000, 0.8660254037844387076, 1.000000000000000000, 0.8660254037844387076, 1.000000000000000000, 0.8660254037844387076, 1.000000000000000000, 0.8660254037844387076, 1.000000000000000000, 0.8660254037844387076, 1.000000000000000000, 0.8660254037844387076, 1.000000000000000000, 0.8660254037844387076, 1.000000000000000000, 0.8660254037844387076, 1.000000000000000000, 0.8660254037844387076, 1.000000000000000000, 0.8660254037844387076, 1.000000000000000000, 0.8660254037844387076, 1.000000000000000000, 0.8660254037844387076, 1.000000000000000000, 0.8660254037844387076, 1.000000000000000000, 0.8660254037844387076, 1.000000000000000000, 0.8660254037844387076, 1.000000000000000000, 0.8660254037844387076, 1.000000000000000000, 0.8660254037844387076, 1.000000000000000000, 0.8660254037844387076, 1.000000000000000000, 0.8660254037844387076, 1.000000000000000000, 0.8660254037844387076, 1.000000000000000000, 0.8660254037844387076, 1.000000000000000000, 0.8660254037844387076, 1.000000000000000000, 0.8660254037844387076, 1.000000000000000000, 0.8660254037844387076, 1.000000000000000000, 0.8660254037844387076, 1.000000000000000000, 0.8660254037844387076, 1.000000000000000000, 0.8660254037844387076, 1.000000000000000000, 0.8660254037844387076, 1.000000000000000000, 0.8660254037844387076, 1.000000000000000000, 0.8660254037844387076, 1.000000000000000000, 0.8660254037844387076, 1.000000000000000000, 0.8660254037844387076, 1.000000000000000000, 0.8660254037844387076, 1.000000000000000000, 0.8660254037844387076, 1.000000000000000000, 0.8660254037844387076, 1.000000000000000000, 0.8660254037844387076, 1.000000000000000000, 0.8660254037844387076, 1.000000000000000000, 0.8660254037844387076, 1.000000000000000000, 0.8660254037844387076, 1.000000000000000000, 0.8660254037844387076, 1.000000000000000000, 0.8660254037844387076, 1.000000000000000000, 0.8660254037844387076, 1.000000000000000000, 0.8660254037844387076, 1.000000000000000000, 0.8660254037844387076, 1.000000000000000000, 0.8660254037844387076, 1.000000000000000000, 0.8660254037844387076, 1.000000000000000000, 0.8660254037844387076, 1.000000000000000000, 0.8660254037844387076, 1.000000000000000000, 0.8660254037844387076, 1.000000000000000000, 0.8660254037844387076, 1.000000000000000000, 0.8660254037844387076, 1.000000000000000000, 0.8660254037844387076, 1.000000000000000000, 0.8660254037844387076, 1.000000000000000000, 0.8660254037844387076, 1.000000000000000000, 0.8660254037844387076, 1.000000000000000000, 0.8660254037844387076, 1.000000000000000000, 0.8660254037844387076, 1.000000000000000000, 0.8660254037844387076, 1.000000000000000000, 0.8660254037844387076, 1.000000000000000000, 0.8660254037844387076, 1.000000000000000000, 0.8660254037844387076, 1.000000000000000000, 0.8660254037844387076, 1.000000000000000000, 0.8660254037844387076, 1.000000000000000000, 0.8660254037844387076, 1.000000000000000000, 0.8660254037844387076, 1.000000000000000000, 0.8660254037844387076, 1.000000000000000000, 0.8660254037844387076, 1.000000000000000000, 0.8660254037844387076, 1.000000000000000000, 0.8660254037844387076, 1.000000000000000000, 0.8660254037844387076, 1.000000000000000000, 0.8660254037844387076, 1.000000000000000000, 0.8660254037844387076, 1.000000000000000000, 0.8660254037844387076, 1.000000000000000000, 0.8660254037844387076, 1.000000000000000000, 0.8660254037844387076, 1.000000000000000000, 0.8660254037844387076, 1.000000000000000000, 0.8660254037844387076, 1.000000000000000000, 0.8660254037844387076, 1.000000000000000000, 0.8660254037844387076, 1.000000000000000000, 0.8660254037844387076, 1.000000000000000000, 0.8660254037844387076, 1.000000000000000000, 0.8660254037844387076, 1.000000000000000000, 0.8660254037844387076, 1.000000000000000000, 0.8660254037844387076, 1.000000000000000000, 0.8660254037844387076, 1.000000000000000000, 0.8660254037844387076, 1.000000000000000000, 0.8660254037844387076, 1.000000000000000000, 0.8660254037844387076, 1.000000000000000000, 0.8660254037844387076, 1.000000000000000000, 0.8660254037844387076, 1.000000000000000000, 0.8660254037844387076, 1.000000000000000000, 0.8660254037844387076, 1.000000000000000000, 0.8660254037844387076, 1.000000000000000000, 0.8660254037844387076, 1.000000000000000000, 0.8660254037844387076, 1.000000000000000000, 0.8660254037844387076, 1.000000000000000000, 0.8660254037844387076, 1.000000000000000000, 0.8660254037844387076, 1.000000000000000000, 0.8660254037844387076, 1.000000000000000000, 0.8660254037844387076, 1.000000000000000000, 0.8660254037844387076, 1.000000000000000000, 0.8660254037844387076, 1.000000000000000000, 0.8660254037844387076, 1.000000000000000000, 0.8660254037844387076, 1.000000000000000000, 0.8660254037844387076, 1.000000000000000000, 0.8660254037844387076, 1.000000000000000000, 0.8660254037844387076, 1.000000000000000000, 0.8660254037844387076, 1.000000000000000000, 0.8660254037844387076, 1.000000000000000000, 0.8660254037844387076, 1.000000000000000000, 0.8660254037844387076, 1.000000000000000000, 0.8660254037844387076, 1.000000000000000000, 0.8660254037844387076, 1.000000000000000000, 0.8660254037844387076, 1.000000000000000000, 0.8660254037844387076, 1.000000000000000000, 0.8660254037844387076, 1.000000000000000000, 0.8660254037844387076, 1.000000000000000000, 0.8660254037844387076, 1.000000000000000000, 0.8660254037844387076, 1.000000000000000000, 0.8660254037844387076, 1.000000000000000000, 0.8660254037844387076, 1.000000000000000000, 0.8660254037844387076, 1.000000000000000000, 0.8660254037844387076, 1.000000000000000000, 0.8660254037844387076, 1.000000000000000000, 0.8660254037844387076, 1.000000000000000000, 0.8660254037844387076, 1.000000000000000000, 0.8660254037844387076, 1.000000000000000000, 0.8660254037844387076, 1.000000000000000000, 0.8660254037844387076, 1.000000000000000000, 0.8660254037844387076, 1.000000000000000000, 0.8660254037844387076, 1.000000000000000000, 0.8660254037844387076, 1.000000000000000000, 0.8660254037844387076, 1.000000000000000000, 0.8660254037844387076, 1.000000000000000000, 0.8660254037844387076, 1.000000000000000000, 0.8660254037844387076, 1.000000000000000000, 0.8660254037844387076, 1.000000000000000000, 0.8660254037844387076, 1.000000000000000000, 0.8660254037844387076, 1.000000000000000000, 0.8660254037844387076, 1.000000000000000000, 0.8660254037844387076, 1.000000000000000000, 0.8660254037844387076, 1.000000000000000000, 0.8660254037844387076, 1.000000000000000000, 0.8660254037844387076, 1.000000000000000000, 0.8660254037844387076, 1.000000000000000000, 0.8660254037844387076, 1.000000000000000000, 0.8660254037844387076, 1.000000000000000000, 0.8660254037844387076, 1.000000000000000000, 0.8660254037844387076, 1.000000000000000000, 0.8660254037844387076, 1.000000000000000000, 0.8660254037844387076, 1.000000000000000000, 0.8660254037844387076, 1.000000000000000000, 0.8660254037844387076, 1.000000000000000000, 0.8660254037844387076, 1.000000000000000000, 0.8660254037844387076, 1.000000000000000000, 0.8660254037844387076, 1.000000000000000000, 0.8660254037844387076, 1.000000000000000000, 0.8660254037844387076, 1.000000000000000000, 0.8660254037844387076, 1.000000000000000000, 0.8660254037844387076, 1.000000000000000000, 0.8660254037844387076, 1.000000000000000000, 0.8660254037844387076, 1.000000000000000000, 0.8660254037844387076, 1.000000000000000000, 0.8660254037844387076, 1.000000000000000000, 0.8660254037844387076, 1.000000000000000000, 0.8660254037844387076, 1.000000000000000000, 0.8660254037844387076, 1.000000000000000000, 0.8660254037844387076, 1.000000000000000000, 0.8660254037844387076, 1.000000000000000000, 0.8660254037844387076, 1.000000000000000000, 0.8660254037844387076, 1.000000000000000000, 0.8660254037844387076, 1.000000000000000000, 0.8660254037844387076, 1.000000000000000000, 0.8660254037844387076, 1.000000000000000000, 0.8660254037844387076, 1.000000000000000000, 0.8660254037844387076, 1.000000000000000000, 0.8660254037844387076, 1.000000000000000000, 0.8660254037844387076, 1.000000000000000000, 0.8660254037844387076, 1.000000000000000000, 0.8660254037844387076, 1.000000000000000000, 0.8660254037844387076, 1.000000000000000000, 0.8660254037844387076, 1.000000000000000000, 0.8660254037844387076, 1.000000000000000000, 0.8660254037844387076, 1.000000000000000000, 0.8660254037844387076, 1.000000000000000000, 0.8660254037844387076, 1.000000000000000000, 0.8660254037844387076, 1.000000000000000000, 0.8660254037844387076, 1.000000000000000000, 0.8660254037844387076, 1.000000000000000000, 0.8660254037844387076, 1.000000000000000000, 0.8660254037844387076, 1.000000000000000000, 0.8660254037844387076, 1.000000000000000000, 0.8660254037844387076, 1.000000000000000000, 0.8660254037844387076, 1.000000000000000000, 0.8660254037844387076, 1.000000000000000000, 0.8660254037844387076, 1.000000000000000000, 0.8660254037844387076, 1.000000000000000000, 0.8660254037844387076, 1.000000000000000000, 0.8660254037844387076, 1.000000000000000000, 0.8660254037844387076, 1.000000000000000000, 0.8660254037844387076, 1.000000000000000000, 0.8660254037844387076, 1.000000000000000000, 0.8660254037844387076, 1.000000000000000000, 0.8660254037844387076, 1.000000000000000000, 0.8660254037844387076, 1.000000000000000000, 0.8660254037844387076, 1.000000000000000000, 0.8660254037844387076, 1.000000000000000000, 0.8660254037844387076, 1.000000000000000000, 0.8660254037844387076, 1.000000000000000000, 0.8660254037844387076, 1.000000000000000000, 0.8660254037844387076, 1.000000000000000000, 0.8660254037844387076, 1.000000000000000000, 0.8660254037844387076, 1.000000000000000000, 0.8660254037844387076, 1.000000000000000000, 0.8660254037844387076, 1.000000000000000000, 0.8660254037844387076, 1.000000000000000000, 0.8660254037844387076, 1.000000000000000000, 0.8660254037844387076, 1.000000000000000000, 0.8660254037844387076, 1.000000000000000000, 0.8660254037844387076, 1.000000000000000000, 0.8660254037844387076, 1.000000000000000000, 0.8660254037844387076, 1.000000000000000000, 0.8660254037844387076, 1.000000000000000000, 0.8660254037844387076, 1.000000000000000000, 0.8660254037844387076, 1.000000000000000000, 0.8660254037844387076, 1.000000000000000000, 0.8660254037844387076, 1.000000000000000000, 0.8660254037844387076, 1.000000000000000000, 0.8660254037844387076, 1.000000000000000000, 0.8660254037844387076, 1.000000000000000000, 0.8660254037844387076, 1.000000000000000000, 0.8660254037844387076, 1.000000000000000000, 0.8660254037844387076, 1.000000000000000000, 0.8660254037844387076, 1.000000000000000000, 0.8660254037844387076, 1.000000000000000000, 0.8660254037844387076, 1.000000000000000000, 0.8660254037844387076, 1.000000000000000000, 0.8660254037844387076, 1.000000000000000000, 0.8660254037844387076, 1.000000000000000000, 0.8660254037844387076, 1.000000000000000000, 0.8660254037844387076, 1.000000000000000000, 0.8660254037844387076, 1.000000000000000000, 0.8660254037844387076, 1.000000000000000000, 0.8660254037844387076, 1.000000000000000000, 0.8660254037844387076, 1.000000000000000000, 0.8660254037844387076, 1.000000000000000000, 0.8660254037844387076, 1.000000000000000000, 0.8660254037844387076, 1.000000000000000000, 0.8660254037844387076, 1.000000000000000000, 0.8660254037844387076, 1.000000000000000000, 0.8660254037844387076, 1.000000000000000000, 0.8660254037844387076, 1.000000000000000000, 0.8660254037844387076, 1.000000000000000000, 0.8660254037844387076, 1.000000000000000000, 0.8660254037844387076, 1.000000000000000000, 0.8660254037844387076, 1.000000000000000000, 0.8660254037844387076, 1.000000000000000000, 0.8660254037844387076, 1.000000000000000000, 0.8660254037844387076, 1.000000000000000000, 0.8660254037844387076, 1.000000000000000000, 0.8660254037844387076, 1.000000000000000000, 0.8660254037844387076, 1.000000000000000000, 0.8660254037844387076, 1.000000000000000000, 0.8660254037844387076, 1.000000000000000000, 0.8660254037844387076, 1.000000000000000000, 0.8660254037844387076, 1.000000000000000000, 0.8660254037844387076, 1.000000000000000000, 0.8660254037844387076, 1.000000000000000000, 0.8660254037844387076, 1.000000000000000000, 0.8660254037844387076, 1.000000000000000000, 0.8660254037844387076, 1.000000000000000000, 0.8660254037844387076, 1.000000000000000000, 0.8660254037844387076, 1.000000000000000000, 0.8660254037844387076, 1.000000000000000000, 0.8660254037844387076, 1.000000000000000000, 0.8660254037844387076, 1.000000000000000000, 0.8660254037844387076, 1.000000000000000000, 0.8660254037844387076, 1.000000000000000000, 0.8660254037844387076, 1.000000000000000000, 0.8660254037844387076, 1.000000000000000000, 0.8660254037844387076, 1.000000000000000000, 0.8660254037844387076, 1.000000000000000000, 0.8660254037844387076, 1.000000000000000000, 0.8660254037844387076, 1.000000000000000000, 0.8660254037844387076, 1.000000000000000000, 0.8660254037844387076, 1.000000000000000000, 0.8660254037844387076, 1.000000000000000000, 0.8660254037844387076, 1.000000000000000000, 0.8660254037844387076, 1.000000000000000000, 0.8660254037844387076, 1.000000000000000000, 0.8660254037844387076, 1.000000000000000000, 0.8660254037844387076, 1.000000000000000000, 0.8660254037844387076, 1.000000000000000000, 0.8660254037844387076, 1.000000000000000000, 0.8660254037844387076, 1.000000000000000000, 0.8660254037844387076, 1.000000000000000000, 0.8660254037844387076, 1.000000000000000000, 0.8660254037844387076, 1.000000000000000000, 0.8660254037844387076, 1.000000000000000000, 0.8660254037844387076, 1.000000000000000000, 0.8660254037844387076, 1.000000000000000000, 0.8660254037844387076, 1.000000000000000000, 0.8660254037844387076, 1.000000000000000000, 0.8660254037844387076, 1.000000000000000000, 0.8660254037844387076, 1.000000000000000000, 0.8660254037844387076, 1.000000000000000000, 0.8660254037844387076, 1.000000000000000000, 0.8660254037844387076, 1.000000000000000000, 0.8660254037844387076, 1.000000000000000000, 0.8660254037844387076, 1.000000000000000000, 0.8660254037844387076, 1.000000000000000000, 0.8660254037844387076, 1.000000000000000000, 0.8660254037844387076, 1.000000000000000000, 0.8660254037844387076, 1.000000000000000000, 0.8660254037844387076, 1.000000000000000000, 0.8660254037844387076, 1.000000000000000000, 0.8660254037844387076, 1.000000000000000000, 0.8660254037844387076, 1.000000000000000000, 0.8660254037844387076, 1.000000000000000000, 0.8660254037844387076, 1.000000000000000000, 0.8660254037844387076, 1.000000000000000000, 0.8660254037844387076, 1.000000000000000000, 0.8660254037844387076, 1.000000000000000000, 0.8660254037844387076, 1.000000000000000000, 0.8660254037844387076, 1.000000000000000000, 0.8660254037844387076, 1.000000000000000000, 0.8660254037844387076, 1.000000000000000000, 0.8660254037844387076, 1.000000000000000000, 0.8660254037844387076, 1.000000000000000000, 0.8660254037844387076, 1.000000000000000000, 0.8660254037844387076, 1.000000000000000000, 0.8660254037844387076, 1.000000000000000000, 0.8660254037844387076, 1.000000000000000000, 0.8660254037844387076, 1.000000000000000000, 0.8660254037844387076, 1.000000000000000000, 0.8660254037844387076, 1.000000000000000000, 0.8660254037844387076, 1.000000000000000000, 0.8660254037844387076, 1.000000000000000000, 0.8660254037844387076, 1.000000000000000000, 0.8660254037844387076, 1.000000000000000000, 0.8660254037844387076, 1.000000000000000000, 0.8660254037844387076, 1.000000000000000000, 0.8660254037844387076, 1.000000000000000000, 0.8660254037844387076, 1.000000000000000000, 0.8660254037844387076, 1.000000000000000000, 0.8660254037844387076, 1.000000000000000000, 0.8660254037844387076, 1.000000000000000000, 0.8660254037844387076, 1.000000000000000000, 0.8660254037844387076, 1.000000000000000000, 0.8660254037844387076, 1.000000000000000000, 0.8660254037844387076, 1.000000000000000000, 0.8660254037844387076, 1.000000000000000000, 0.8660254037844387076, 1.000000000000000000, 0.8660254037844387076, 1.000000000000000000, 0.8660254037844387076, 1.000000000000000000, 0.8660254037844387076, 1.000000000000000000, 0.8660254037844387076, 1.000000000000000000, 0.8660254037844387076, 1.000000000000000000, 0.8660254037844387076, 1.000000000000000000, 0.8660254037844387076, 1.000000000000000000, 0.8660254037844387076, 1.000000000000000000, 0.8660254037844387076, 1.000000000000000000, 0.8660254037844387076, 1.000000000000000000, 0.8660254037844387076, 1.000000000000000000, 0.8660254037844387076, 1.000000000000000000, 0.8660254037844387076, 1.000000000000000000, 0.8660254037844387076, 1.000000000000000000, 0.8660254037844387076, 1.000000000000000000, 0.8660254037844387076, 1.000000000000000000, 0.8660254037844387076, 1.000000000000000000, 0.8660254037844387076, 1.000000000000000000, 0.8660254037844387076, 1.000000000000000000, 0.8660254037844387076, 1.000000000000000000, 0.8660254037844387076, 1.000000000000000000, 0.8660254037844387076, 1.000000000000000000, 0.8660254037844387076, 1.000000000000000000, 0.8660254037844387076, 1.000000000000000000, 0.8660254037844387076, 1.000000000000000000, 0.8660254037844387076, 1.000000000000000000, 0.8660254037844387076, 1.000000000000000000, 0.8660254037844387076, 1.000000000000000000, 0.8660254037844387076, 1.000000000000000000, 0.8660254037844387076, 1.000000000000000000, 0.8660254037844387076, 1.000000000000000000, 0.8660254037844387076, 1.000000000000000000, 0.8660254037844387076, 1.000000000000000000, 0.8660254037844387076, 1.000000000000000000, 0.8660254037844387076, 1.000000000000000000, 0.8660254037844387076, 1.000000000000000000, 0.8660254037844387076, 1.000000000000000000, 0.8660254037844387076, 1.000000000000000000, 0.8660254037844387076, 1.000000000000000000, 0.8660254037844387076, 1.000000000000000000, 0.8660254037844387076, 1.000000000000000000, 0.8660254037844387076, 1.000000000000000000, 0.8660254037844387076, 1.000000000000000000, 0.8660254037844387076, 1.000000000000000000, 0.8660254037844387076, 1.000000000000000000, 0.8660254037844387076, 1.000000000000000000, 0.8660254037844387076, 1.000000000000000000, 0.8660254037844387076, 1.000000000000000000),
 ( 1.000000000000000000, 0.8660254037844387076, 1.000000000000000000, 0.8660254037844387076, 1.000000000000000000, 0.8660254037844387076, 1.000000000000000000, 0.8660254037844387076, 1.000000000000000000, 0.8660254037844387076, 1.000000000000000000, 0.8660254037844387076, 1.000000000000000000, 0.8660254037844387076, 1.000000000000000000, 0.8660254037844387076, 1.000000000000000000, 0.8660254037844387076, 1.000000000000000000, 0.8660254037844387076, 1.000000000000000000, 0.8660254037844387076, 1.000000000000000000, 0.8660254037844387076, 1.000000000000000000, 0.8660254037844387076, 1.000000000000000000, 0.8660254037844387076, 1.000000000000000000, 0.8660254037844387076, 1.000000000000000000, 0.8660254037844387076, 1.000000000000000000, 0.8660254037844387076, 1.000000000000000000, 0.8660254037844387076, 1.000000000000000000, 0.8660254037844387076, 1.000000000000000000, 0.8660254037844387076, 1.000000000000000000, 0.8660254037844387076, 1.000000000000000000, 0.8660254037844387076, 1.000000000000000000, 0.8660254037844387076, 1.000000000000000000, 0.8660254037844387076, 1.000000000000000000, 0.8660254037844387076, 1.000000000000000000, 0.8660254037844387076, 1.000000000000000000, 0.8660254037844387076, 1.000000000000000000, 0.8660254037844387076, 1.000000000000000000, 0.8660254037844387076, 1.000000000000000000, 0.8660254037844387076, 1.000000000000000000, 0.8660254037844387076, 1.000000000000000000, 0.8660254037844387076, 1.000000000000000000, 0.8660254037844387076, 1.000000000000000000, 0.8660254037844387076, 1.000000000000000000, 0.8660254037844387076, 1.000000000000000000, 0.8660254037844387076, 1.000000000000000000, 0.8660254037844387076, 1.000000000000000000, 0.8660254037844387076, 1.000000000000000000, 0.8660254037844387076, 1.000000000000000000, 0.8660254037844387076, 1.000000000000000000, 0.8660254037844387076, 1.000000000000000000, 0.8660254037844387076, 1.000000000000000000, 0.8660254037844387076, 1.000000000000000000, 0.8660254037844387076, 1.000000000000000000, 0.8660254037844387076, 1.000000000000000000, 0.8660254037844387076, 1.000000000000000000, 0.8660254037844387076, 1.000000000000000000, 0.8660254037844387076, 1.000000000000000000, 0.8660254037844387076, 1.000000000000000000, 0.8660254037844387076, 1.000000000000000000, 0.8660254037844387076, 1.000000000000000000, 0.8660254037844387076, 1.000000000000000000, 0.8660254037844387076, 1.000000000000000000, 0.8660254037844387076, 1.000000000000000000, 0.8660254037844387076, 1.000000000000000000, 0.8660254037844387076, 1.000000000000000000, 0.8660254037844387076, 1.000000000000000000, 0.8660254037844387076, 1.000000000000000000, 0.8660254037844387076, 1.000000000000000000, 0.8660254037844387076, 1.000000000000000000, 0.8660254037844387076, 1.000000000000000000, 0.8660254037844387076, 1.000000000000000000, 0.8660254037844387076, 1.000000000000000000, 0.8660254037844387076, 1.000000000000000000, 0.8660254037844387076, 1.000000000000000000, 0.8660254037844387076, 1.000000000000000000, 0.8660254037844387076, 1.000000000000000000, 0.8660254037844387076, 1.000000000000000000, 0.8660254037844387076, 1.000000000000000000, 0.8660254037844387076, 1.000000000000000000, 0.8660254037844387076, 1.000000000000000000, 0.8660254037844387076, 1.000000000000000000, 0.8660254037844387076, 1.000000000000000000, 0.8660254037844387076, 1.000000000000000000, 0.8660254037844387076, 1.000000000000000000, 0.8660254037844387076, 1.000000000000000000, 0.8660254037844387076, 1.000000000000000000, 0.8660254037844387076, 1.000000000000000000, 0.8660254037844387076, 1.000000000000000000, 0.8660254037844387076, 1.000000000000000000, 0.8660254037844387076, 1.000000000000000000, 0.8660254037844387076, 1.000000000000000000, 0.8660254037844387076, 1.000000000000000000, 0.8660254037844387076, 1.000000000000000000, 0.8660254037844387076, 1.000000000000000000, 0.8660254037844387076, 1.000000000000000000, 0.8660254037844387076, 1.000000000000000000, 0.8660254037844387076, 1.000000000000000000, 0.8660254037844387076, 1.000000000000000000, 0.8660254037844387076, 1.000000000000000000, 0.8660254037844387076, 1.000000000000000000, 0.8660254037844387076, 1.000000000000000000, 0.8660254037844387076, 1.000000000000000000, 0.8660254037844387076, 1.000000000000000000, 0.8660254037844387076, 1.000000000000000000, 0.8660254037844387076, 1.000000000000000000, 0.8660254037844387076, 1.000000000000000000, 0.8660254037844387076, 1.000000000000000000, 0.8660254037844387076, 1.000000000000000000, 0.8660254037844387076, 1.000000000000000000, 0.8660254037844387076, 1.000000000000000000, 0.8660254037844387076, 1.000000000000000000, 0.8660254037844387076, 1.000000000000000000, 0.8660254037844387076, 1.000000000000000000, 0.8660254037844387076, 1.000000000000000000, 0.8660254037844387076, 1.000000000000000000, 0.8660254037844387076, 1.000000000000000000, 0.8660254037844387076, 1.000000000000000000, 0.8660254037844387076, 1.000000000000000000, 0.8660254037844387076, 1.000000000000000000, 0.8660254037844387076, 1.000000000000000000, 0.8660254037844387076, 1.000000000000000000, 0.8660254037844387076, 1.000000000000000000, 0.8660254037844387076, 1.000000000000000000, 0.8660254037844387076, 1.000000000000000000, 0.8660254037844387076, 1.000000000000000000, 0.8660254037844387076, 1.000000000000000000, 0.8660254037844387076, 1.000000000000000000, 0.8660254037844387076, 1.000000000000000000, 0.8660254037844387076, 1.000000000000000000, 0.8660254037844387076, 1.000000000000000000, 0.8660254037844387076, 1.000000000000000000, 0.8660254037844387076, 1.000000000000000000, 0.8660254037844387076, 1.000000000000000000, 0.8660254037844387076, 1.000000000000000000, 0.8660254037844387076, 1.000000000000000000, 0.8660254037844387076, 1.000000000000000000, 0.8660254037844387076, 1.000000000000000000, 0.8660254037844387076, 1.000000000000000000, 0.8660254037844387076, 1.000000000000000000, 0.8660254037844387076, 1.000000000000000000, 0.8660254037844387076, 1.000000000000000000, 0.8660254037844387076, 1.000000000000000000, 0.8660254037844387076, 1.000000000000000000, 0.8660254037844387076, 1.000000000000000000, 0.8660254037844387076, 1.000000000000000000, 0.8660254037844387076, 1.000000000000000000, 0.8660254037844387076, 1.000000000000000000, 0.8660254037844387076, 1.000000000000000000, 0.8660254037844387076, 1.000000000000000000, 0.8660254037844387076, 1.000000000000000000, 0.8660254037844387076, 1.000000000000000000, 0.8660254037844387076, 1.000000000000000000, 0.8660254037844387076, 1.000000000000000000, 0.8660254037844387076, 1.000000000000000000, 0.8660254037844387076, 1.000000000000000000, 0.8660254037844387076, 1.000000000000000000, 0.8660254037844387076, 1.000000000000000000, 0.8660254037844387076, 1.000000000000000000, 0.8660254037844387076, 1.000000000000000000, 0.8660254037844387076, 1.000000000000000000, 0.8660254037844387076, 1.000000000000000000, 0.8660254037844387076, 1.000000000000000000, 0.8660254037844387076, 1.000000000000000000, 0.8660254037844387076, 1.000000000000000000, 0.8660254037844387076, 1.000000000000000000, 0.8660254037844387076, 1.000000000000000000, 0.8660254037844387076, 1.000000000000000000, 0.8660254037844387076, 1.000000000000000000, 0.8660254037844387076, 1.000000000000000000, 0.8660254037844387076, 1.000000000000000000, 0.8660254037844387076, 1.000000000000000000, 0.8660254037844387076, 1.000000000000000000, 0.8660254037844387076, 1.000000000000000000, 0.8660254037844387076, 1.000000000000000000, 0.8660254037844387076, 1.000000000000000000, 0.8660254037844387076, 1.000000000000000000, 0.8660254037844387076, 1.000000000000000000, 0.8660254037844387076, 1.000000000000000000, 0.8660254037844387076, 1.000000000000000000, 0.8660254037844387076, 1.000000000000000000, 0.8660254037844387076, 1.000000000000000000, 0.8660254037844387076, 1.000000000000000000, 0.8660254037844387076, 1.000000000000000000, 0.8660254037844387076, 1.000000000000000000, 0.8660254037844387076, 1.000000000000000000, 0.8660254037844387076, 1.000000000000000000, 0.8660254037844387076, 1.000000000000000000, 0.8660254037844387076, 1.000000000000000000, 0.8660254037844387076, 1.000000000000000000, 0.8660254037844387076, 1.000000000000000000, 0.8660254037844387076, 1.000000000000000000, 0.8660254037844387076, 1.000000000000000000, 0.8660254037844387076, 1.000000000000000000, 0.8660254037844387076, 1.000000000000000000, 0.8660254037844387076, 1.000000000000000000, 0.8660254037844387076, 1.000000000000000000, 0.8660254037844387076, 1.000000000000000000, 0.8660254037844387076, 1.000000000000000000, 0.8660254037844387076, 1.000000000000000000, 0.8660254037844387076, 1.000000000000000000, 0.8660254037844387076, 1.000000000000000000, 0.8660254037844387076, 1.000000000000000000, 0.8660254037844387076, 1.000000000000000000, 0.8660254037844387076, 1.000000000000000000, 0.8660254037844387076, 1.000000000000000000, 0.8660254037844387076, 1.000000000000000000, 0.8660254037844387076, 1.000000000000000000, 0.8660254037844387076, 1.000000000000000000, 0.8660254037844387076, 1.000000000000000000, 0.8660254037844387076, 1.000000000000000000, 0.8660254037844387076, 1.000000000000000000, 0.8660254037844387076, 1.000000000000000000, 0.8660254037844387076, 1.000000000000000000, 0.8660254037844387076, 1.000000000000000000, 0.8660254037844387076, 1.000000000000000000, 0.8660254037844387076, 1.000000000000000000, 0.8660254037844387076, 1.000000000000000000, 0.8660254037844387076, 1.000000000000000000, 0.8660254037844387076, 1.000000000000000000, 0.8660254037844387076, 1.000000000000000000, 0.8660254037844387076, 1.000000000000000000, 0.8660254037844387076, 1.000000000000000000, 0.8660254037844387076, 1.000000000000000000, 0.8660254037844387076, 1.000000000000000000, 0.8660254037844387076, 1.000000000000000000, 0.8660254037844387076, 1.000000000000000000, 0.8660254037844387076, 1.000000000000000000, 0.8660254037844387076, 1.000000000000000000, 0.8660254037844387076, 1.000000000000000000, 0.8660254037844387076, 1.000000000000000000, 0.8660254037844387076, 1.000000000000000000, 0.8660254037844387076, 1.000000000000000000, 0.8660254037844387076, 1.000000000000000000, 0.8660254037844387076, 1.000000000000000000, 0.8660254037844387076, 1.000000000000000000, 0.8660254037844387076, 1.000000000000000000, 0.8660254037844387076, 1.000000000000000000, 0.8660254037844387076, 1.000000000000000000, 0.8660254037844387076, 1.000000000000000000, 0.8660254037844387076, 1.000000000000000000, 0.8660254037844387076, 1.000000000000000000, 0.8660254037844387076, 1.000000000000000000, 0.8660254037844387076, 1.000000000000000000, 0.8660254037844387076, 1.000000000000000000, 0.8660254037844387076, 1.000000000000000000, 0.8660254037844387076, 1.000000000000000000, 0.8660254037844387076, 1.000000000000000000, 0.8660254037844387076, 1.000000000000000000, 0.8660254037844387076, 1.000000000000000000, 0.8660254037844387076, 1.000000000000000000, 0.8660254037844387076, 1.000000000000000000, 0.8660254037844387076, 1.000000000000000000, 0.8660254037844387076, 1.000000000000000000, 0.8660254037844387076, 1.000000000000000000, 0.8660254037844387076, 1.000000000000000000, 0.8660254037844387076, 1.000000000000000000, 0.8660254037844387076, 1.000000000000000000, 0.8660254037844387076, 1.000000000000000000, 0.8660254037844387076, 1.000000000000000000, 0.8660254037844387076, 1.000000000000000000, 0.8660254037844387076, 1.000000000000000000, 0.8660254037844387076, 1.000000000000000000, 0.8660254037844387076, 1.000000000000000000, 0.8660254037844387076, 1.000000000000000000, 0.8660254037844387076, 1.000000000000000000, 0.8660254037844387076, 1.000000000000000000, 0.8660254037844387076, 1.000000000000000000, 0.8660254037844387076, 1.000000000000000000, 0.8660254037844387076, 1.000000000000000000, 0.8660254037844387076, 1.000000000000000000, 0.8660254037844387076, 1.000000000000000000, 0.8660254037844387076, 1.000000000000000000, 0.8660254037844387076, 1.000000000000000000, 0.8660254037844387076, 1.000000000000000000, 0.8660254037844387076, 1.000000000000000000, 0.8660254037844387076, 1.000000000000000000, 0.8660254037844387076, 1.000000000000000000, 0.8660254037844387076, 1.000000000000000000, 0.8660254037844387076, 1.000000000000000000, 0.8660254037844387076, 1.000000000000000000, 0.8660254037844387076, 1.000000000000000000, 0.8660254037844387076, 1.000000000000000000, 0.8660254037844387076, 1.000000000000000000, 0.8660254037844387076, 1.000000000000000000, 0.8660254037844387076, 1.000000000000000000, 0.8660254037844387076, 1.000000000000000000, 0.8660254037844387076, 1.000000000000000000, 0.8660254037844387076, 1.000000000000000000, 0.8660254037844387076, 1.000000000000000000, 0.8660254037844387076, 1.000000000000000000, 0.8660254037844387076, 1.000000000000000000, 0.8660254037844387076, 1.000000000000000000, 0.8660254037844387076, 1.000000000000000000, 0.8660254037844387076, 1.000000000000000000, 0.8660254037844387076, 1.000000000000000000, 0.8660254037844387076, 1.000000000000000000, 0.8660254037844387076, 1.000000000000000000, 0.8660254037844387076, 1.000000000000000000, 0.8660254037844387076, 1.000000000000000000, 0.8660254037844387076, 1.000000000000000000, 0.8660254037844387076, 1.000000000000000000, 0.8660254037844387076, 1.000000000000000000, 0.8660254037844387076, 1.000000000000000000, 0.8660254037844387076, 1.000000000000000000, 0.8660254037844387076, 1.000000000000000000, 0.8660254037844387076, 1.000000000000000000, 0.8660254037844387076, 1.000000000000000000, 0.8660254037844387076, 1.000000000000000000, 0.8660254037844387076, 1.000000000000000000, 0.8660254037844387076, 1.000000000000000000, 0.8660254037844387076, 1.000000000000000000, 0.8660254037844387076, 1.000000000000000000, 0.8660254037844387076, 1.000000000000000000, 0.8660254037844387076, 1.000000000000000000, 0.8660254037844387076, 1.000000000000000000, 0.8660254037844387076, 1.000000000000000000, 0.8660254037844387076, 1.000000000000000000, 0.8660254037844387076, 1.000000000000000000, 0.8660254037844387076, 1.000000000000000000, 0.8660254037844387076, 1.000000000000000000, 0.8660254037844387076, 1.000000000000000000, 0.8660254037844387076, 1.000000000000000000, 0.8660254037844387076, 1.000000000000000000, 0.8660254037844387076, 1.000000000000000000, 0.8660254037844387076, 1.000000000000000000, 0.8660254037844387076, 1.000000000000000000, 0.8660254037844387076, 1.000000000000000000, 0.8660254037844387076, 1.000000000000000000, 0.8660254037844387076, 1.000000000000000000, 0.8660254037844387076, 1.000000000000000000, 0.8660254037844387076, 1.000000000000000000, 0.8660254037844387076, 1.000000000000000000, 0.8660254037844387076, 1.000000000000000000, 0.8660254037844387076, 1.000000000000000000, 0.8660254037844387076, 1.000000000000000000, 0.8660254037844387076, 1.000000000000000000, 0.8660254037844387076, 1.000000000000000000, 0.8660254037844387076, 1.000000000000000000, 0.8660254037844387076, 1.000000000000000000, 0.8660254037844387076, 1.000000000000000000, 0.8660254037844387076, 1.000000000000000000, 0.8660254037844387076, 1.000000000000000000, 0.8660254037844387076, 1.000000000000000000, 0.8660254037844387076, 1.000000000000000000, 0.8660254037844387076, 1.000000000000000000, 0.8660254037844387076, 1.000000000000000000, 0.8660254037844387076, 1.000000000000000000, 0.8660254037844387076, 1.000000000000000000, 0.8660254037844387076, 1.000000000000000000, 0.8660254037844387076, 1.000000000000000000, 0.8660254037844387076, 1.000000000000000000, 0.8660254037844387076, 1.000000000000000000, 0.8660254037844387076, 1.000000000000000000, 0.8660254037844387076, 1.000000000000000000, 0.8660254037844387076, 1.000000000000000000, 0.8660254037844387076, 1.000000000000000000, 0.8660254037844387076, 1.000000000000000000, 0.8660254037844387076, 1.000000000000000000, 0.8660254037844387076, 1.000000000000000000, 0.8660254037844387076, 1.000000000000000000, 0.8660254037844387076, 1.000000000000000000, 0.8660254037844387076, 1.000000000000000000, 0.8660254037844387076, 1.000000000000000000, 0.8660254037844387076, 1.000000000000000000, 0.8660254037844387076, 1.000000000000000000, 0.8660254037844387076, 1.000000000000000000, 0.8660254037844387076, 1.000000000000000000, 0.8660254037844387076, 1.000000000000000000, 0.8660254037844387076, 1.000000000000000000, 0.8660254037844387076, 1.000000000000000000, 0.8660254037844387076, 1.000000000000000000, 0.8660254037844387076, 1.000000000000000000, 0.8660254037844387076, 1.000000000000000000, 0.8660254037844387076, 1.000000000000000000, 0.8660254037844387076, 1.000000000000000000, 0.8660254037844387076, 1.000000000000000000, 0.8660254037844387076, 1.000000000000000000, 0.8660254037844387076, 1.000000000000000000, 0.8660254037844387076, 1.000000000000000000, 0.8660254037844387076, 1.000000000000000000, 0.8660254037844387076, 1.000000000000000000, 0.8660254037844387076, 1.000000000000000000, 0.8660254037844387076, 1.000000000000000000, 0.8660254037844387076, 1.000000000000000000, 0.8660254037844387076, 1.000000000000000000, 0.8660254037844387076, 1.000000000000000000, 0.8660254037844387076, 1.000000000000000000, 0.8660254037844387076, 1.000000000000000000, 0.8660254037844387076, 1.000000000000000000, 0.8660254037844387076, 1.000000000000000000, 0.8660254037844387076, 1.000000000000000000, 0.8660254037844387076, 1.000000000000000000, 0.8660254037844387076, 1.000000000000000000, 0.8660254037844387076, 1.000000000000000000, 0.8660254037844387076, 1.000000000000000000, 0.8660254037844387076, 1.000000000000000000, 0.8660254037844387076, 1.000000000000000000, 0.8660254037844387076, 1.000000000000000000, 0.8660254037844387076, 1.000000000000000000, 0.8660254037844387076, 1.000000000000000000, 0.8660254037844387076, 1.000000000000000000, 0.8660254037844387076, 1.000000000000000000, 0.8660254037844387076, 1.000000000000000000, 0.8660254037844387076, 1.000000000000000000, 0.8660254037844387076, 1.000000000000000000, 0.8660254037844387076, 1.000000000000000000, 0.8660254037844387076, 1.000000000000000000, 0.8660254037844387076, 1.000000000000000000, 0.8660254037844387076, 1.000000000000000000, 0.8660254037844387076, 1.000000000000000000, 0.8660254037844387076, 1.000000000000000000, 0.8660254037844387076, 1.000000000000000000, 0.8660254037844387076, 1.000000000000000000, 0.8660254037844387076, 1.000000000000000000, 0.8660254037844387076, 1.000000000000000000, 0.8660254037844387076, 1.000000000000000000, 0.8660254037844387076, 1.000000000000000000, 0.8660254037844387076, 1.000000000000000000, 0.8660254037844387076, 1.000000000000000000, 0.8660254037844387076, 1.000000000000000000, 0.8660254037844387076, 1.000000000000000000, 0.8660254037844387076, 1.000000000000000000, 0.8660254037844387076, 1.000000000000000000, 0.8660254037844387076, 1.000000000000000000, 0.8660254037844387076, 1.000000000000000000, 0.8660254037844387076, 1.000000000000000000, 0.8660254037844387076, 1.000000000000000000, 0.8660254037844387076, 1.000000000000000000, 0.8660254037844387076, 1.000000000000000000, 0.8660254037844387076, 1.000000000000000000, 0.8660254037844387076, 1.000000000000000000, 0.8660254037844387076, 1.000000000000000000, 0.8660254037844387076, 1.000000000000000000, 0.8660254037844387076, 1.000000000000000000, 0.8660254037844387076, 1.000000000000000000, 0.8660254037844387076, 1.000000000000000000, 0.8660254037844387076, 1.000000000000000000, 0.8660254037844387076, 1.000000000000000000, 0.8660254037844387076, 1.000000000000000000, 0.8660254037844387076, 1.000000000000000000, 0.8660254037844387076, 1.000000000000000000, 0.8660254037844387076, 1.000000000000000000, 0.8660254037844387076, 1.000000000000000000, 0.8660254037844387076, 1.000000000000000000, 0.8660254037844387076, 1.000000000000000000, 0.8660254037844387076, 1.000000000000000000, 0.8660254037844387076, 1.000000000000000000, 0.8660254037844387076, 1.000000000000000000, 0.8660254037844387076, 1.000000000000000000, 0.8660254037844387076, 1.000000000000000000, 0.8660254037844387076, 1.000000000000000000, 0.8660254037844387076, 1.000000000000000000, 0.8660254037844387076, 1.000000000000000000, 0.8660254037844387076, 1.000000000000000000, 0.8660254037844387076, 1.000000000000000000, 0.8660254037844387076, 1.000000000000000000, 0.8660254037844387076, 1.000000000000000000, 0.8660254037844387076, 1.000000000000000000, 0.8660254037844387076, 1.000000000000000000, 0.8660254037844387076, 1.000000000000000000, 0.8660254037844387076, 1.000000000000000000, 0.8660254037844387076, 1.000000000000000000, 0.8660254037844387076, 1.000000000000000000, 0.8660254037844387076, 1.000000000000000000, 0.8660254037844387076, 1.000000000000000000, 0.8660254037844387076, 1.000000000000000000, 0.8660254037844387076, 1.000000000000000000, 0.8660254037844387076, 1.000000000000000000, 0.8660254037844387076, 1.000000000000000000, 0.8660254037844387076, 1.000000000000000000, 0.8660254037844387076, 1.000000000000000000, 0.8660254037844387076, 1.000000000000000000, 0.8660254037844387076, 1.000000000000000000, 0.8660254037844387076, 1.000000000000000000, 0.8660254037844387076, 1.000000000000000000, 0.8660254037844387076, 1.000000000000000000, 0.8660254037844387076, 1.000000000000000000, 0.8660254037844387076, 1.000000000000000000, 0.8660254037844387076, 1.000000000000000000, 0.8660254037844387076, 1.000000000000000000, 0.8660254037844387076, 1.000000000000000000, 0.8660254037844387076, 1.000000000000000000, 0.8660254037844387076, 1.000000000000000000, 0.8660254037844387076, 1.000000000000000000, 0.8660254037844387076, 1.000000000000000000, 0.8660254037844387076, 1.000000000000000000, 0.8660254037844387076, 1.000000000000000000, 0.8660254037844387076, 1.000000000000000000, 0.8660254037844387076, 1.000000000000000000, 0.8660254037844387076, 1.000000000000000000, 0.8660254037844387076, 1.000000000000000000, 0.8660254037844387076, 1.000000000000000000, 0.8660254037844387076, 1.000000000000000000, 0.8660254037844387076, 1.000000000000000000, 0.8660254037844387076, 1.000000000000000000, 0.8660254037844387076, 1.000000000000000000, 0.8660254037844387076, 1.000000000000000000, 0.8660254037844387076, 1.000000000000000000, 0.8660254037844387076, 1.000000000000000000, 0.8660254037844387076, 1.000000000000000000, 0.8660254037844387076, 1.000000000000000000, 0.8660254037844387076, 1.000000000000000000, 0.8660254037844387076, 1.000000000000000000, 0.8660254037844387076, 1.000000000000000000, 0.8660254037844387076, 1.000000000000000000, 0.8660254037844387076, 1.000000000000000000, 0.8660254037844387076, 1.000000000000000000, 0.8660254037844387076, 1.000000000000000000, 0.8660254037844387076, 1.000000000000000000, 0.8660254037844387076, 1.000000000000000000, 0.8660254037844387076, 1.000000000000000000, 0.8660254037844387076, 1.000000000000000000, 0.8660254037844387076, 1.000000000000000000, 0.8660254037844387076, 1.000000000000000000, 0.8660254037844387076, 1.000000000000000000, 0.8660254037844387076, 1.000000000000000000, 0.8660254037844387076, 1.000000000000000000, 0.8660254037844387076, 1.000000000000000000, 0.8660254037844387076, 1.000000000000000000, 0.8660254037844387076, 1.000000000000000000, 0.8660254037844387076, 1.000000000000000000, 0.8660254037844387076, 1.000000000000000000, 0.8660254037844387076, 1.000000000000000000, 0.8660254037844387076, 1.000000000000000000, 0.8660254037844387076, 1.000000000000000000, 0.8660254037844387076, 1.000000000000000000, 0.8660254037844387076, 1.000000000000000000, 0.8660254037844387076, 1.000000000000000000, 0.8660254037844387076, 1.000000000000000000, 0.8660254037844387076, 1.000000000000000000, 0.8660254037844387076, 1.000000000000000000, 0.8660254037844387076, 1.000000000000000000, 0.8660254037844387076, 1.000000000000000000, 0.8660254037844387076, 1.000000000000000000, 0.8660254037844387076, 1.000000000000000000, 0.8660254037844387076, 1.000000000000000000, 0.8660254037844387076, 1.000000000000000000, 0.8660254037844387076, 1.000000000000000000, 0.8660254037844387076, 1.000000000000000000, 0.8660254037844387076, 1.000000000000000000, 0.8660254037844387076, 1.000000000000000000, 0.8660254037844387076, 1.000000000000000000, 0.8660254037844387076, 1.000000000000000000, 0.8660254037844387076, 1.000000000000000000, 0.8660254037844387076, 1.000000000000000000, 0.8660254037844387076, 1.000000000000000000, 0.8660254037844387076, 1.000000000000000000, 0.8660254037844387076, 1.000000000000000000, 0.8660254037844387076, 1.000000000000000000, 0.8660254037844387076, 1.000000000000000000, 0.8660254037844387076, 1.000000000000000000, 0.8660254037844387076, 1.000000000000000000, 0.8660254037844387076, 1.000000000000000000, 0.8660254037844387076, 1.000000000000000000, 0.8660254037844387076, 1.000000000000000000, 0.8660254037844387076, 1.000000000000000000, 0.8660254037844387076, 1.000000000000000000, 0.8660254037844387076, 1.000000000000000000, 0.8660254037844387076, 1.000000000000000000, 0.8660254037844387076, 1.000000000000000000, 0.8660254037844387076, 1.000000000000000000, 0.8660254037844387076, 1.000000000000000000, 0.8660254037844387076, 1.000000000000000000, 0.8660254037844387076, 1.000000000000000000, 0.8660254037844387076, 1.000000000000000000, 0.8660254037844387076, 1.000000000000000000, 0.8660254037844387076, 1.000000000000000000, 0.8660254037844387076, 1.000000000000000000, 0.8660254037844387076, 1.000000000000000000, 0.8660254037844387076, 1.000000000000000000, 0.8660254037844387076, 1.000000000000000000, 0.8660254037844387076, 1.000000000000000000, 0.8660254037844387076, 1.000000000000000000, 0.8660254037844387076, 1.000000000000000000, 0.8660254037844387076, 1.000000000000000000, 0.8660254037844387076, 1.000000000000000000, 0.8660254037844387076, 1.000000000000000000, 0.8660254037844387076, 1.000000000000000000, 0.8660254037844387076, 1.000000000000000000, 0.8660254037844387076, 1.000000000000000000, 0.8660254037844387076, 1.000000000000000000, 0.8660254037844387076, 1.000000000000000000, 0.8660254037844387076, 1.000000000000000000, 0.8660254037844387076, 1.000000000000000000, 0.8660254037844387076, 1.000000000000000000, 0.8660254037844387076, 1.000000000000000000, 0.8660254037844387076, 1.000000000000000000, 0.8660254037844387076, 1.000000000000000000, 0.8660254037844387076, 1.000000000000000000, 0.8660254037844387076, 1.000000000000000000, 0.8660254037844387076, 1.000000000000000000, 0.8660254037844387076, 1.000000000000000000, 0.8660254037844387076, 1.000000000000000000, 0.8660254037844387076, 1.000000000000000000, 0.8660254037844387076, 1.000000000000000000, 0.8660254037844387076, 1.000000000000000000, 0.8660254037844387076, 1.000000000000000000, 0.8660254037844387076, 1.000000000000000000, 0.8660254037844387076, 1.000000000000000000, 0.8660254037844387076, 1.000000000000000000, 0.8660254037844387076, 1.000000000000000000, 0.8660254037844387076, 1.000000000000000000, 0.8660254037844387076, 1.000000000000000000, 0.8660254037844387076, 1.000000000000000000, 0.8660254037844387076, 1.000000000000000000, 0.8660254037844387076, 1.000000000000000000, 0.8660254037844387076, 1.000000000000000000, 0.8660254037844387076, 1.000000000000000000, 0.8660254037844387076, 1.000000000000000000, 0.8660254037844387076, 1.000000000000000000, 0.8660254037844387076, 1.000000000000000000, 0.8660254037844387076, 1.000000000000000000, 0.8660254037844387076, 1.000000000000000000, 0.8660254037844387076, 1.000000000000000000, 0.8660254037844387076, 1.000000000000000000, 0.8660254037844387076, 1.000000000000000000, 0.8660254037844387076, 1.000000000000000000, 0.8660254037844387076, 1.000000000000000000, 0.8660254037844387076, 1.000000000000000000, 0.8660254037844387076, 1.000000000000000000, 0.8660254037844387076, 1.000000000000000000, 0.8660254037844387076, 1.000000000000000000, 0.8660254037844387076, 1.000000000000000000, 0.8660254037844387076, 1.000000000000000000, 0.8660254037844387076, 1.000000000000000000, 0.8660254037844387076, 1.000000000000000000, 0.8660254037844387076, 1.000000000000000000, 0.8660254037844387076, 1.000000000000000000, 0.8660254037844387076, 1.000000000000000000, 0.8660254037844387076, 1.000000000000000000, 0.8660254037844387076, 1.000000000000000000, 0.8660254037844387076, 1.000000000000000000, 0.8660254037844387076, 1.000000000000000000, 0.8660254037844387076, 1.000000000000000000, 0.8660254037844387076, 1.000000000000000000, 0.8660254037844387076, 1.000000000000000000, 0.8660254037844387076, 1.000000000000000000, 0.8660254037844387076, 1.000000000000000000, 0.8660254037844387076, 1.000000000000000000, 0.8660254037844387076, 1.000000000000000000, 0.8660254037844387076, 1.000000000000000000, 0.8660254037844387076, 1.000000000000000000, 0.8660254037844387076, 1.000000000000000000, 0.8660254037844387076, 1.000000000000000000, 0.8660254037844387076, 1.000000000000000000, 0.8660254037844387076, 1.000000000000000000, 0.8660254037844387076, 1.000000000000000000, 0.8660254037844387076, 1.000000000000000000, 0.8660254037844387076, 1.000000000000000000, 0.8660254037844387076, 1.000000000000000000, 0.8660254037844387076, 1.000000000000000000, 0.8660254037844387076, 1.000000000000000000, 0.8660254037844387076, 1.000000000000000000, 0.8660254037844387076, 1.000000000000000000, 0.8660254037844387076, 1.000000000000000000, 0.8660254037844387076, 1.000000000000000000, 0.8660254037844387076, 1.000000000000000000, 0.8660254037844387076, 1.000000000000000000, 0.8660254037844387076, 1.000000000000000000, 0.8660254037844387076, 1.000000000000000000, 0.8660254037844387076, 1.000000000000000000, 0.8660254037844387076, 1.000000000000000000, 0.8660254037844387076, 1.000000000000000000, 0.8660254037844387076, 1.000000000000000000, 0.8660254037844387076, 1.000000000000000000, 0.8660254037844387076, 1.000000000000000000, 0.8660254037844387076, 1.000000000000000000, 0.8660254037844387076, 1.000000000000000000, 0.8660254037844387076, 1.000000000000000000, 0.8660254037844387076, 1.000000000000000000, 0.8660254037844387076, 1.000000000000000000, 0.8660254037844387076, 1.000000000000000000, 0.8660254037844387076, 1.000000000000000000, 0.8660254037844387076, 1.000000000000000000, 0.8660254037844387076, 1.000000000000000000, 0.8660254037844387076, 1.000000000000000000, 0.8660254037844387076, 1.000000000000000000, 0.8660254037844387076, 1.000000000000000000, 0.8660254037844387076, 1.000000000000000000, 0.8660254037844387076, 1.000000000000000000, 0.8660254037844387076, 1.000000000000000000, 0.8660254037844387076, 1.000000000000000000, 0.8660254037844387076, 1.000000000000000000, 0.8660254037844387076, 1.000000000000000000, 0.8660254037844387076, 1.000000000000000000, 0.8660254037844387076, 1.000000000000000000, 0.8660254037844387076, 1.000000000000000000, 0.8660254037844387076, 1.000000000000000000, 0.8660254037844387076, 1.000000000000000000, 0.8660254037844387076, 1.000000000000000000, 0.8660254037844387076, 1.000000000000000000, 0.8660254037844387076, 1.000000000000000000, 0.8660254037844387076, 1.000000000000000000, 0.8660254037844387076, 1.000000000000000000, 0.8660254037844387076, 1.000000000000000000, 0.8660254037844387076, 1.000000000000000000, 0.8660254037844387076, 1.000000000000000000, 0.8660254037844387076, 1.000000000000000000, 0.8660254037844387076, 1.000000000000000000, 0.8660254037844387076, 1.000000000000000000, 0.8660254037844387076, 1.000000000000000000, 0.8660254037844387076, 1.000000000000000000, 0.8660254037844387076, 1.000000000000000000, 0.8660254037844387076, 1.000000000000000000, 0.8660254037844387076, 1.000000000000000000, 0.8660254037844387076, 1.000000000000000000, 0.8660254037844387076, 1.000000000000000000, 0.8660254037844387076, 1.000000000000000000, 0.8660254037844387076, 1.000000000000000000, 0.8660254037844387076, 1.000000000000000000, 0.8660254037844387076, 1.000000000000000000, 0.8660254037844387076, 1.000000000000000000, 0.8660254037844387076, 1.000000000000000000, 0.8660254037844387076, 1.000000000000000000, 0.8660254037844387076, 1.000000000000000000, 0.8660254037844387076, 1.000000000000000000, 0.8660254037844387076, 1.000000000000000000, 0.8660254037844387076, 1.000000000000000000, 0.8660254037844387076, 1.000000000000000000, 0.8660254037844387076, 1.000000000000000000, 0.8660254037844387076, 1.000000000000000000, 0.8660254037844387076, 1.000000000000000000, 0.8660254037844387076, 1.000000000000000000, 0.8660254037844387076, 1.000000000000000000, 0.8660254037844387076, 1.000000000000000000, 0.8660254037844387076, 1.000000000000000000, 0.8660254037844387076, 1.000000000000000000, 0.8660254037844387076, 1.000000000000000000, 0.8660254037844387076, 1.000000000000000000, 0.8660254037844387076, 1.000000000000000000, 0.8660254037844387076, 1.000000000000000000, 0.8660254037844387076, 1.000000000000000000, 0.8660254037844387076, 1.000000000000000000, 0.8660254037844387076, 1.000000000000000000, 0.8660254037844387076, 1.000000000000000000, 0.8660254037844387076, 1.000000000000000000, 0.8660254037844387076, 1.000000000000000000, 0.8660254037844387076, 1.000000000000000000, 0.8660254037844387076, 1.000000000000000000, 0.8660254037844387076, 1.000000000000000000, 0.8660254037844387076, 1.000000000000000000, 0.8660254037844387076, 1.000000000000000000, 0.8660254037844387076, 1.000000000000000000, 0.8660254037844387076, 1.000000000000000000, 0.8660254037844387076, 1.000000000000000000, 0.8660254037844387076, 1.000000000000000000, 0.8660254037844387076, 1.000000000000000000, 0.8660254037844387076, 1.000000000000000000, 0.8660254037844387076, 1.000000000000000000, 0.8660254037844387076, 1.000000000000000000, 0.8660254037844387076, 1.000000000000000000, 0.8660254037844387076, 1.000000000000000000, 0.8660254037844387076, 1.000000000000000000, 0.8660254037844387076, 1.000000000000000000, 0.8660254037844387076, 1.000000000000000000, 0.8660254037844387076, 1.000000000000000000, 0.8660254037844387076, 1.000000000000000000, 0.8660254037844387076, 1.000000000000000000, 0.8660254037844387076, 1.000000000000000000, 0.8660254037844387076, 1.000000000000000000, 0.8660254037844387076, 1.000000000000000000, 0.8660254037844387076, 1.000000000000000000, 0.8660254037844387076, 1.000000000000000000, 0.8660254037844387076, 1.000000000000000000, 0.8660254037844387076, 1.000000000000000000, 0.8660254037844387076, 1.000000000000000000, 0.8660254037844387076, 1.000000000000000000, 0.8660254037844387076, 1.000000000000000000, 0.8660254037844387076, 1.000000000000000000, 0.8660254037844387076, 1.000000000000000000, 0.8660254037844387076, 1.000000000000000000, 0.8660254037844387076, 1.000000000000000000, 0.8660254037844387076, 1.000000000000000000, 0.8660254037844387076, 1.000000000000000000, 0.8660254037844387076, 1.000000000000000000, 0.8660254037844387076, 1.000000000000000000, 0.8660254037844387076, 1.000000000000000000, 0.8660254037844387076, 1.000000000000000000, 0.8660254037844387076, 1.000000000000000000, 0.8660254037844387076, 1.000000000000000000, 0.8660254037844387076, 1.000000000000000000, 0.8660254037844387076, 1.000000000000000000, 0.8660254037844387076, 1.000000000000000000, 0.8660254037844387076, 1.000000000000000000, 0.8660254037844387076, 1.000000000000000000, 0.8660254037844387076, 1.000000000000000000, 0.8660254037844387076, 1.000000000000000000, 0.8660254037844387076, 1.000000000000000000, 0.8660254037844387076, 1.000000000000000000, 0.8660254037844387076, 1.000000000000000000, 0.8660254037844387076, 1.000000000000000000, 0.8660254037844387076, 1.000000000000000000, 0.8660254037844387076, 1.000000000000000000, 0.8660254037844387076, 1.000000000000000000, 0.8660254037844387076, 1.000000000000000000, 0.8660254037844387076, 1.000000000000000000, 0.8660254037844387076, 1.000000000000000000, 0.8660254037844387076, 1.000000000000000000, 0.8660254037844387076, 1.000000000000000000, 0.8660254037844387076, 1.000000000000000000, 0.8660254037844387076, 1.000000000000000000, 0.8660254037844387076, 1.000000000000000000, 0.8660254037844387076, 1.000000000000000000, 0.8660254037844387076, 1.000000000000000000, 0.8660254037844387076, 1.000000000000000000, 0.8660254037844387076, 1.000000000000000000, 0.8660254037844387076, 1.000000000000000000, 0.8660254037844387076, 1.000000000000000000, 0.8660254037844387076, 1.000000000000000000) ) ) 
 REPRESENTATION_ITEM ( '' )  SURFACE ( )  );
#11342 = CARTESIAN_POINT ( 'NONE',  ( 10.81189881249999729, 0.000000000000000000, -161.8437500020484094 ) ) ;
#11343 = CARTESIAN_POINT ( 'NONE',  ( 10.81189881249999551, -6.242252689847874514, -176.9687500020484094 ) ) ;
#11344 = CARTESIAN_POINT ( 'NONE',  ( 5.000000000000000000, 8.660254037844385522, -132.2499999999999716 ) ) ;
#11345 = DIRECTION ( 'NONE',  ( 0.000000000000000000, 0.000000000000000000, -1.000000000000000000 ) ) ;
#11346 = CARTESIAN_POINT ( 'NONE',  ( 9.999999999999998224, 0.000000000000000000, -20.37500000409675494 ) ) ;
#11347 = CARTESIAN_POINT ( 'NONE',  ( 7.070501591499376803E-16, 11.54700538379251284, -60.50000000409677625 ) ) ;
#11348 = CARTESIAN_POINT ( 'NONE',  ( -10.81189881249999907, -6.242252689847864744, -111.4687500020483810 ) ) ;
#11349 = DIRECTION ( 'NONE',  ( 1.000000000000000000, 0.000000000000000000, 0.000000000000000000 ) ) ;
#11350 = CARTESIAN_POINT ( 'NONE',  ( 10.81189881249999907, 6.242252689847868297, -83.90625000204836681 ) ) ;
#11351 = CARTESIAN_POINT ( 'NONE',  ( 10.81189881249999551, -6.242252689847874514, -98.96875000204838102 ) ) ;
#11352 = CARTESIAN_POINT ( 'NONE',  ( -10.81189881249999729, 1.324075727343319199E-15, -59.09375000204835970 ) ) ;
#11353 = CARTESIAN_POINT ( 'NONE',  ( 5.405949406249999534, 9.363379034771803333, -70.28125000204838102 ) ) ;
#11354 = CARTESIAN_POINT ( 'NONE',  ( 7.070501591499377789E-16, 11.54700538379251284, -158.0000000040968189 ) ) ;
#11355 = CARTESIAN_POINT ( 'NONE',  ( 5.000000000000000000, 8.660254037844385522, -133.7499999999999716 ) ) ;
#11356 = CARTESIAN_POINT ( 'NONE',  ( 5.405949406249999534, 9.363379034771803333, -151.2812500020484094 ) ) ;
#11357 = CARTESIAN_POINT ( 'NONE',  ( 7.644554776091147741E-16, 12.48450537969573659, -163.1562500020484094 ) ) ;
#11358 = DIRECTION ( 'NONE',  ( -0.000000000000000000, -0.000000000000000000, -1.000000000000000000 ) ) ;
#11359 = LINE ( 'NONE', #24554, #22011 ) ;
#11360 = CARTESIAN_POINT ( 'NONE',  ( -10.81189881249999729, 1.324075727343319199E-15, -98.09375000204838102 ) ) ;
#11361 = CARTESIAN_POINT ( 'NONE',  ( 5.000000000000000000, 8.660254037844385522, -42.62500000409677625 ) ) ;
#11362 = CARTESIAN_POINT ( 'NONE',  ( 9.999999999999998224, 0.000000000000000000, -76.99999999999998579 ) ) ;
#11363 = CARTESIAN_POINT ( 'NONE',  ( -10.81189881249999729, 6.242252689847871849, -192.7187500020483810 ) ) ;
#11364 = CARTESIAN_POINT ( 'NONE',  ( -9.999999999999998224, 5.773502691896259087, -79.75000000409677625 ) ) ;
#11365 = CARTESIAN_POINT ( 'NONE',  ( -9.999999999999998224, 1.224646799147353059E-15, -25.62500000409675849 ) ) ;
#11366 = CARTESIAN_POINT ( 'NONE',  ( -10.81189881249999729, 6.242252689847871849, -95.40625000204838102 ) ) ;
#11367 = CARTESIAN_POINT ( 'NONE',  ( 5.405949406249999534, 9.363379034771803333, -76.28125000204838102 ) ) ;
#11368 = CARTESIAN_POINT ( 'NONE',  ( 5.000000000000000000, 8.660254037844385522, -80.12500000409677625 ) ) ;
#11369 = CARTESIAN_POINT ( 'NONE',  ( 10.81189881249999907, 6.242252689847868297, -28.21875000204838102 ) ) ;
#11370 = ORIENTED_EDGE ( 'NONE', *, *, #37024, .T. ) ;
#11371 = CARTESIAN_POINT ( 'NONE',  ( 10.81189881249999729, 0.000000000000000000, -199.5312500020484094 ) ) ;
#11372 = CARTESIAN_POINT ( 'NONE',  ( 10.81189881249999729, 0.000000000000000000, -25.53125000204836681 ) ) ;
#11373 = CARTESIAN_POINT ( 'NONE',  ( -10.81189881249999729, 6.242252689847871849, -11.21875000204837036 ) ) ;
#11374 = CARTESIAN_POINT ( 'NONE',  ( 10.00000000000102318, -5.773502691895667560, -64.00000000409674783 ) ) ;
#11375 = CARTESIAN_POINT ( 'NONE',  ( -2.121150477449813534E-15, -11.54700538379251284, -5.750000004096755823 ) ) ;
#11376 = CARTESIAN_POINT ( 'NONE',  ( -10.81189881249999907, -6.242252689847864744, -131.1562500020483810 ) ) ;
#11377 = CIRCLE ( 'NONE', #1763, 5.000000000000002665 ) ;
#11378 = CARTESIAN_POINT ( 'NONE',  ( -9.999999999999998224, 5.773502691896259087, -185.8750000000000000 ) ) ;
#11379 = CARTESIAN_POINT ( 'NONE',  ( 9.999999999999479527, 5.773502691896553074, -120.3749999999999716 ) ) ;
#11381 = ORIENTED_EDGE ( 'NONE', *, *, #4319, .F. ) ;
#11380 = CARTESIAN_POINT ( 'NONE',  ( 10.81189881249999551, -6.242252689847874514, -106.6562500020483952 ) ) ;
#11382 = CARTESIAN_POINT ( 'NONE',  ( -2.275517850991317657E-15, -20.00000000000000000, -235.0000000000000000 ) ) ;
#11383 = ADVANCED_FACE ( 'NONE', ( #21403 ), #24880, .T. ) ;
#11384 = VERTEX_POINT ( 'NONE', #34804 ) ;
#11385 = EDGE_CURVE ( 'NONE', #3574, #33493, #11972, .T. ) ;
#11386 = EDGE_LOOP ( 'NONE', ( #31271, #42436, #9162, #26269 ) ) ;
#11387 =( BOUNDED_CURVE ( )  B_SPLINE_CURVE ( 2, ( #41964, #34885, #38954, #12604, #5951, #32072, #8760 ),
 .UNSPECIFIED., .F., .F. ) 
 B_SPLINE_CURVE_WITH_KNOTS ( ( 3, 2, 2, 3 ),
 ( 0.9738805970149255753, 0.9751243781094529606, 0.9763681592039802348, 0.9776119402985076201 ),
 .UNSPECIFIED. ) 
 CURVE ( )  GEOMETRIC_REPRESENTATION_ITEM ( )  RATIONAL_B_SPLINE_CURVE ( ( 0.9999999999999761302, 0.8660254037844625774, 1.000000000000000000, 0.8660254037844387076, 1.000000000000000000, 0.8660254037844267172, 1.000000000000011990 ) ) 
 REPRESENTATION_ITEM ( '' )  );
#11388 = CARTESIAN_POINT ( 'NONE',  ( -5.405949406249996869, 9.363379034771805109, -40.03125000204838102 ) ) ;
#11389 = PERSON_AND_ORGANIZATION_ROLE ( 'classification_officer' ) ;
#11390 = CARTESIAN_POINT ( 'NONE',  ( 10.81189881249999907, 6.242252689847868297, -85.21875000204836681 ) ) ;
#11391 = LINE ( 'NONE', #7530, #18759 ) ;
#11392 = CARTESIAN_POINT ( 'NONE',  ( -9.999999999999998224, 1.224646799147353059E-15, -113.7499999999999858 ) ) ;
#11393 = VECTOR ( 'NONE', #29049, 1000.000000000000000 ) ;
#11394 = CARTESIAN_POINT ( 'NONE',  ( -10.00000000000025580, 5.773502691896109873, -156.2500000040968189 ) ) ;
#11395 = CARTESIAN_POINT ( 'NONE',  ( -10.81189881249999729, 6.242252689847871849, -164.4062500020484094 ) ) ;
#11396 = DIRECTION ( 'NONE',  ( -1.000000000000000000, 0.000000000000000000, 0.000000000000000000 ) ) ;
#11397 = CARTESIAN_POINT ( 'NONE',  ( -10.81189881249999729, 6.242252689847871849, -122.2187500020483810 ) ) ;
#11398 = CARTESIAN_POINT ( 'NONE',  ( 10.81189881249999551, -6.242252689847874514, -85.46875000204836681 ) ) ;
#11399 = CARTESIAN_POINT ( 'NONE',  ( 10.81189881249999729, 0.000000000000000000, -3.031250002048374803 ) ) ;
#11400 = CARTESIAN_POINT ( 'NONE',  ( -10.81189881249999907, -6.242252689847864744, -195.4687500020484094 ) ) ;
#11401 = CARTESIAN_POINT ( 'NONE',  ( -10.81189881249999729, 6.242252689847871849, -90.90625000204838102 ) ) ;
#11402 = CARTESIAN_POINT ( 'NONE',  ( 5.000000000000000000, 8.660254037844385522, -176.1250000040968189 ) ) ;
#11403 = CARTESIAN_POINT ( 'NONE',  ( 5.405949406249992428, -9.363379034771808662, -172.7812500020484094 ) ) ;
#11404 = CARTESIAN_POINT ( 'NONE',  ( 10.00000000000102318, -5.773502691895667560, -70.00000000409676204 ) ) ;
#11405 = CARTESIAN_POINT ( 'NONE',  ( 7.644554776091147741E-16, 12.48450537969573659, -170.6562500020484094 ) ) ;
#11406 = CARTESIAN_POINT ( 'NONE',  ( -2.293366432827344421E-15, -12.48450537969573659, -187.9062500020484094 ) ) ;
#11407 = CARTESIAN_POINT ( 'NONE',  ( 7.644554776091147741E-16, 12.48450537969573659, -53.46875000204838102 ) ) ;
#11408 = CARTESIAN_POINT ( 'NONE',  ( 9.999999999999998224, 0.000000000000000000, -174.8750000040967905 ) ) ;
#11409 = CARTESIAN_POINT ( 'NONE',  ( -2.293366432827344421E-15, -12.48450537969573659, -12.40625000204835970 ) ) ;
#11410 = CARTESIAN_POINT ( 'NONE',  ( 5.405949406249992428, -9.363379034771808662, -21.09375000204835615 ) ) ;
#11411 = CARTESIAN_POINT ( 'NONE',  ( -9.999999999999612754, -5.773502691896474914, -153.0000000040967620 ) ) ;
#11412 = CARTESIAN_POINT ( 'NONE',  ( -10.81189881249999907, -6.242252689847864744, -124.9687500020483810 ) ) ;
#11413 = CARTESIAN_POINT ( 'NONE',  ( -2.121150477449813534E-15, -11.54700538379251284, -96.87500000000000000 ) ) ;
#11414 = CARTESIAN_POINT ( 'NONE',  ( -5.405949406249996869, 9.363379034771805109, -32.53125000204837391 ) ) ;
#11415 = CARTESIAN_POINT ( 'NONE',  ( 10.00000000000000000, 5.773502691896255534, -105.7500000040967905 ) ) ;
#11416 = EDGE_CURVE ( 'NONE', #4599, #28346, #42594, .T. ) ;
#11417 = CARTESIAN_POINT ( 'NONE',  ( 10.00000000000021672, -5.773502691896130301, -190.0000000040968189 ) ) ;
#11418 = CARTESIAN_POINT ( 'NONE',  ( -4.999999999999996447, 8.660254037844387298, -50.99999999999996447 ) ) ;
#11419 = CARTESIAN_POINT ( 'NONE',  ( -5.405949406249996869, 9.363379034771805109, -121.0312500020483952 ) ) ;
#11420 = CARTESIAN_POINT ( 'NONE',  ( -5.405949406250003975, -9.363379034771801557, -96.53125000204839523 ) ) ;
#11421 = ORIENTED_EDGE ( 'NONE', *, *, #18258, .T. ) ;
#11422 = CARTESIAN_POINT ( 'NONE',  ( -9.999999999999998224, 5.773502691896259087, -103.7500000040967620 ) ) ;
#11423 = CARTESIAN_POINT ( 'NONE',  ( -2.121150477449813534E-15, -11.54700538379251284, -166.2500000040968189 ) ) ;
#11424 = CARTESIAN_POINT ( 'NONE',  ( 7.644554776091147741E-16, 12.48450537969573659, -163.1562500020484094 ) ) ;
#11425 = CARTESIAN_POINT ( 'NONE',  ( -5.405949406250003975, -9.363379034771801557, -57.34375000204835970 ) ) ;
#11426 = ORIENTED_EDGE ( 'NONE', *, *, #17223, .T. ) ;
#11427 = CARTESIAN_POINT ( 'NONE',  ( 9.999999999999996447, -5.773502691896262640, -29.12499999999997513 ) ) ;
#11428 = CARTESIAN_POINT ( 'NONE',  ( -5.405949406250003975, -9.363379034771801557, -30.53125000204837036 ) ) ;
#11429 = CARTESIAN_POINT ( 'NONE',  ( 9.999999999999998224, 0.000000000000000000, -158.0000000000000000 ) ) ;
#11430 = DIRECTION ( 'NONE',  ( -0.000000000000000000, -0.000000000000000000, -1.000000000000000000 ) ) ;
#11431 = CARTESIAN_POINT ( 'NONE',  ( 9.999999999999996447, -5.773502691896262640, -28.00000000409677625 ) ) ;
#11432 = CIRCLE ( 'NONE', #12117, 5.000000000000002665 ) ;
#11433 = CARTESIAN_POINT ( 'NONE',  ( 4.999999999999992006, -8.660254037844389075, -23.24999999999996447 ) ) ;
#11434 = CARTESIAN_POINT ( 'NONE',  ( -5.405949406250003975, -9.363379034771801557, -131.0312500020484094 ) ) ;
#11435 = EDGE_CURVE ( 'NONE', #16951, #15509, #31569, .T. ) ;
#11436 = CARTESIAN_POINT ( 'NONE',  ( -10.00000000000051337, 5.773502691895962435, -142.7500000040967905 ) ) ;
#11437 = ORIENTED_EDGE ( 'NONE', *, *, #3272, .F. ) ;
#11438 = ADVANCED_FACE ( 'NONE', ( #2001 ), #41675, .F. ) ;
#11439 = CARTESIAN_POINT ( 'NONE',  ( 10.81189881249999729, 0.000000000000000000, -64.53125000204836681 ) ) ;
#11440 = EDGE_CURVE ( 'NONE', #35715, #34507, #25724, .T. ) ;
#11442 = ORIENTED_EDGE ( 'NONE', *, *, #9661, .T. ) ;
#11441 = ORIENTED_EDGE ( 'NONE', *, *, #18832, .T. ) ;
#11443 = CARTESIAN_POINT ( 'NONE',  ( -9.999999999999479527, -5.773502691896549521, -46.50000000409676204 ) ) ;
#11444 = CARTESIAN_POINT ( 'NONE',  ( -10.81189881249999907, -6.242252689847864744, -157.9687500020484379 ) ) ;
#11445 = CARTESIAN_POINT ( 'NONE',  ( 10.81189881249999729, 0.000000000000000000, -186.0312500020484094 ) ) ;
#11446 = CARTESIAN_POINT ( 'NONE',  ( 5.405949406249999534, 9.363379034771803333, -19.09375000204835260 ) ) ;
#11447 = CARTESIAN_POINT ( 'NONE',  ( -9.999999999999998224, 1.224646799147353059E-15, -200.0000000000000000 ) ) ;
#11448 = CARTESIAN_POINT ( 'NONE',  ( 5.405949406249999534, 9.363379034771803333, -149.5937500020483810 ) ) ;
#11449 = CARTESIAN_POINT ( 'NONE',  ( -10.81189881249999907, -6.242252689847864744, -127.9687500020483810 ) ) ;
#11450 = CARTESIAN_POINT ( 'NONE',  ( 10.81189881249999729, 0.000000000000000000, -106.5312500020483810 ) ) ;
#11451 = CARTESIAN_POINT ( 'NONE',  ( 10.81189881249999729, 0.000000000000000000, -106.3437500020483810 ) ) ;
#11452 = CARTESIAN_POINT ( 'NONE',  ( 9.999999999999998224, 0.000000000000000000, -2.375000004096766482 ) ) ;
#11453 = CARTESIAN_POINT ( 'NONE',  ( -5.405949406249996869, 9.363379034771805109, -115.0312500020483952 ) ) ;
#11454 = CARTESIAN_POINT ( 'NONE',  ( 5.405949406249992428, -9.363379034771808662, -4.593750002048368586 ) ) ;
#11456 = EDGE_CURVE ( 'NONE', #3313, #8277, #23594, .T. ) ;
#11455 = CARTESIAN_POINT ( 'NONE',  ( -2.293366432827344421E-15, -12.48450537969573659, -129.2187500020483810 ) ) ;
#11457 = CARTESIAN_POINT ( 'NONE',  ( -9.999999999999804601, 5.773502691896371886, -178.7500000040967905 ) ) ;
#11458 = CARTESIAN_POINT ( 'NONE',  ( -9.999999999999998224, 1.224646799147353059E-15, -148.2500000000000000 ) ) ;
#11459 = CARTESIAN_POINT ( 'NONE',  ( -9.999999999999998224, 1.224646799147353059E-15, -20.74999999999996447 ) ) ;
#11460 = CARTESIAN_POINT ( 'NONE',  ( -10.81189881249999729, -6.242252689847864744, -78.46875000204838102 ) ) ;
#11461 = CARTESIAN_POINT ( 'NONE',  ( 5.405949406249999534, 9.363379034771803333, -59.59375000204835970 ) ) ;
#11462 = FACE_BOUND ( 'NONE', #29875, .T. ) ;
#11463 = CARTESIAN_POINT ( 'NONE',  ( -10.81189881249999729, 1.324075727343319199E-15, -36.78125000204837391 ) ) ;
#11464 = CARTESIAN_POINT ( 'NONE',  ( 10.81189881249999551, -6.242252689847874514, -47.96875000204836681 ) ) ;
#11465 = FACE_OUTER_BOUND ( 'NONE', #267, .T. ) ;
#11466 = CARTESIAN_POINT ( 'NONE',  ( 10.81189881249999907, 6.242252689847868297, -155.7187500020483810 ) ) ;
#11467 = CARTESIAN_POINT ( 'NONE',  ( 7.070501591499377789E-16, 11.54700538379251284, -120.1249999999999858 ) ) ;
#11468 = CARTESIAN_POINT ( 'NONE',  ( 4.999999999999992006, -8.660254037844389075, -67.12500000409676204 ) ) ;
#11469 = CARTESIAN_POINT ( 'NONE',  ( -9.999999999999998224, 1.224646799147353059E-15, -73.24999999999998579 ) ) ;
#11470 = CARTESIAN_POINT ( 'NONE',  ( 7.644554776091147741E-16, 12.48450537969573659, -8.656250002048372139 ) ) ;
#11471 = ORIENTED_EDGE ( 'NONE', *, *, #36313, .T. ) ;
#11472 = CARTESIAN_POINT ( 'NONE',  ( 10.81189881249999729, 6.242252689847867408, -103.4062500020483952 ) ) ;
#11473 = CARTESIAN_POINT ( 'NONE',  ( -5.000000000000003553, -8.660254037844383745, -124.3750000040967763 ) ) ;
#11474 = CARTESIAN_POINT ( 'NONE',  ( -9.999999999999612754, -5.773502691896474914, -154.5000000040967905 ) ) ;
#11475 = CARTESIAN_POINT ( 'NONE',  ( -10.81189881249999729, 1.324075727343319199E-15, -81.59375000204838102 ) ) ;
#11476 = CARTESIAN_POINT ( 'NONE',  ( 4.999999999999992006, -8.660254037844389075, -31.12500000409676559 ) ) ;
#11477 = CARTESIAN_POINT ( 'NONE',  ( -5.000000000000003553, -8.660254037844383745, -14.49999999999995737 ) ) ;
#11478 = CARTESIAN_POINT ( 'NONE',  ( 10.81189881249999907, 6.242252689847868297, -46.40625000204836681 ) ) ;
#11479 = CARTESIAN_POINT ( 'NONE',  ( -5.000000000000003553, -8.660254037844383745, -137.5000000000000000 ) ) ;
#11480 = CARTESIAN_POINT ( 'NONE',  ( -5.405949406250003975, -9.363379034771801557, -143.0312500020483810 ) ) ;
#11481 = CARTESIAN_POINT ( 'NONE',  ( 10.81189881249999907, 6.242252689847868297, -124.2187500020483952 ) ) ;
#11482 = CARTESIAN_POINT ( 'NONE',  ( 5.000000000000000000, 8.660254037844385522, -104.1250000040967763 ) ) ;
#11483 = CARTESIAN_POINT ( 'NONE',  ( 9.999999999999998224, 0.000000000000000000, -32.37500000409676204 ) ) ;
#11484 = ORIENTED_EDGE ( 'NONE', *, *, #5611, .T. ) ;
#11485 = LOCAL_TIME ( 11, 57, 6.000000000000000000, #28885 ) ;
#11486 = ORIENTED_EDGE ( 'NONE', *, *, #1701, .F. ) ;
#11487 = ORIENTED_EDGE ( 'NONE', *, *, #13010, .F. ) ;
#11488 = CARTESIAN_POINT ( 'NONE',  ( 7.070501591499376803E-16, 11.54700538379251284, -103.6249999999999858 ) ) ;
#11489 = CARTESIAN_POINT ( 'NONE',  ( 10.81189881249999729, 0.000000000000000000, -187.3437500020483810 ) ) ;
#11491 = EDGE_CURVE ( 'NONE', #29774, #17140, #41207, .T. ) ;
#11490 = CARTESIAN_POINT ( 'NONE',  ( -2.293366432827344421E-15, -12.48450537969573659, -37.71875000204836681 ) ) ;
#11492 = DIRECTION ( 'NONE',  ( -0.08682659386424779191, -0.08682659386424779191, 0.9924325091389669673 ) ) ;
#11493 = CARTESIAN_POINT ( 'NONE',  ( 4.999999999999992006, -8.660254037844389075, -132.7499999999999716 ) ) ;
#11494 = CARTESIAN_POINT ( 'NONE',  ( -10.81189881249999729, 6.242252689847871849, -173.2187500020483810 ) ) ;
#11495 = CARTESIAN_POINT ( 'NONE',  ( 5.405949406249992428, -9.363379034771808662, -150.0937500020483810 ) ) ;
#11496 = CARTESIAN_POINT ( 'NONE',  ( -9.999999999998456346, -5.773502691897145489, -25.50000000409673007 ) ) ;
#11497 = CARTESIAN_POINT ( 'NONE',  ( 5.405949406249999534, 9.363379034771803333, -143.5937500020483810 ) ) ;
#11498 = CARTESIAN_POINT ( 'NONE',  ( 7.644554776091147741E-16, 12.48450537969573659, -148.1562500020484094 ) ) ;
#11499 =( BOUNDED_CURVE ( )  B_SPLINE_CURVE ( 2, ( #39349, #39563, #23611, #9994, #29443, #23173, #36336 ),
 .UNSPECIFIED., .F., .F. ) 
 B_SPLINE_CURVE_WITH_KNOTS ( ( 3, 2, 2, 3 ),
 ( 0.1343283582089551953, 0.1355721393034825528, 0.1368159203980099381, 0.1380597014925373234 ),
 .UNSPECIFIED. ) 
 CURVE ( )  GEOMETRIC_REPRESENTATION_ITEM ( )  RATIONAL_B_SPLINE_CURVE ( ( 1.000000000000003109, 0.8660254037844358210, 1.000000000000000000, 0.8660254037844387076, 1.000000000000000000, 0.8660254037844387076, 1.000000000000000000 ) ) 
 REPRESENTATION_ITEM ( '' )  );
#11500 = CARTESIAN_POINT ( 'NONE',  ( 7.644554776091147741E-16, 12.48450537969573659, -156.9687500020484094 ) ) ;
#11501 = CARTESIAN_POINT ( 'NONE',  ( 7.070501591499376803E-16, 11.54700538379251284, -87.12500000000000000 ) ) ;
#11502 = CARTESIAN_POINT ( 'NONE',  ( 5.000000000000000000, 8.660254037844385522, -36.24999999999997868 ) ) ;
#11503 = CARTESIAN_POINT ( 'NONE',  ( -5.000000000000003553, -8.660254037844383745, -172.0000000000000000 ) ) ;
#11504 = CARTESIAN_POINT ( 'NONE',  ( -5.405949406250003975, -9.363379034771801557, -87.34375000204836681 ) ) ;
#11505 = CARTESIAN_POINT ( 'NONE',  ( -9.999999999999740652, 5.773502691896409189, -180.2500000040967905 ) ) ;
#11506 = CARTESIAN_POINT ( 'NONE',  ( 10.81189881249999729, 0.000000000000000000, -57.03125000204836681 ) ) ;
#11507 = CARTESIAN_POINT ( 'NONE',  ( -6.774270544292668284, -7.481437397228863695, -100.0000000000000142 ) ) ;
#11508 = CARTESIAN_POINT ( 'NONE',  ( -10.81189881249999907, -6.242252689847864744, -181.9687500020484094 ) ) ;
#11509 = CARTESIAN_POINT ( 'NONE',  ( 10.81189881249999551, -6.242252689847874514, -117.1562500020483810 ) ) ;
#11510 = CARTESIAN_POINT ( 'NONE',  ( -5.405949406250003975, -9.363379034771801557, -152.0312500020484094 ) ) ;
#11511 = CARTESIAN_POINT ( 'NONE',  ( 9.999999999999998224, 0.000000000000000000, -3.875000004096768258 ) ) ;
#11512 = CARTESIAN_POINT ( 'NONE',  ( -5.405949406249996869, 9.363379034771805109, -47.53125000204838813 ) ) ;
#11513 = CARTESIAN_POINT ( 'NONE',  ( -5.000000000000003553, -8.660254037844383745, -127.3750000040967905 ) ) ;
#11514 = CARTESIAN_POINT ( 'NONE',  ( -10.00000000000000000, -5.773502691896251982, -103.1249999999999858 ) ) ;
#11515 = ORIENTED_EDGE ( 'NONE', *, *, #37809, .F. ) ;
#11516 = CARTESIAN_POINT ( 'NONE',  ( -10.81189881249999729, 1.324075727343319199E-15, -123.7812500020483952 ) ) ;
#11517 = CARTESIAN_POINT ( 'NONE',  ( -4.999999999999996447, 8.660254037844387298, -148.8750000040967905 ) ) ;
#11518 = FACE_OUTER_BOUND ( 'NONE', #9017, .T. ) ;
#11519 = CARTESIAN_POINT ( 'NONE',  ( -10.81189881249999907, -6.242252689847864744, -179.1562500020484094 ) ) ;
#11520 = ORIENTED_EDGE ( 'NONE', *, *, #33333, .F. ) ;
#11521 = CARTESIAN_POINT ( 'NONE',  ( 7.644554776091147741E-16, 12.48450537969573659, -176.4687500020483810 ) ) ;
#11522 = CARTESIAN_POINT ( 'NONE',  ( -10.00000000000000000, -5.773502691896251982, -58.50000000409676204 ) ) ;
#11523 = CARTESIAN_POINT ( 'NONE',  ( -2.121150477449813534E-15, -11.54700538379251284, -18.87499999999997868 ) ) ;
#11524 = CARTESIAN_POINT ( 'NONE',  ( 5.000000000000000000, 8.660254037844385522, -171.6250000040968189 ) ) ;
#11525 = CARTESIAN_POINT ( 'NONE',  ( -2.293366432827344421E-15, -12.48450537969573659, -69.40625000204838102 ) ) ;
#11526 = CARTESIAN_POINT ( 'NONE',  ( 10.81189881249999729, 0.000000000000000000, -54.03125000204836681 ) ) ;
#11527 = CARTESIAN_POINT ( 'NONE',  ( -9.999999999999998224, 5.773502691896259087, -43.75000000409676204 ) ) ;
#11528 = CARTESIAN_POINT ( 'NONE',  ( -5.405949406250003975, -9.363379034771801557, -1.843750002048366587 ) ) ;
#11529 = CARTESIAN_POINT ( 'NONE',  ( 4.999999999999992006, -8.660254037844389075, -29.62500000409676204 ) ) ;
#11530 = CARTESIAN_POINT ( 'NONE',  ( 10.81189881249999907, 6.242252689847868297, -176.9062500020484094 ) ) ;
#11531 = CARTESIAN_POINT ( 'NONE',  ( 9.999999999999998224, 0.000000000000000000, -200.0000000000000000 ) ) ;
#11532 = CARTESIAN_POINT ( 'NONE',  ( 9.999999999999998224, 0.000000000000000000, -173.0000000000000284 ) ) ;
#11533 = ORIENTED_EDGE ( 'NONE', *, *, #10069, .F. ) ;
#11534 = CARTESIAN_POINT ( 'NONE',  ( -9.999999999998969713, -5.773502691896847949, -61.12499999999996447 ) ) ;
#11536 = ORIENTED_EDGE ( 'NONE', *, *, #4340, .F. ) ;
#11535 = CARTESIAN_POINT ( 'NONE',  ( 10.81189881249999907, 6.242252689847868297, -85.40625000204839523 ) ) ;
#11537 =( LENGTH_UNIT ( ) NAMED_UNIT ( * ) SI_UNIT ( .MILLI., .METRE. ) );
#11539 = VERTEX_POINT ( 'NONE', #16818 ) ;
#11538 = CARTESIAN_POINT ( 'NONE',  ( 5.000000000000000000, 8.660254037844385522, -92.12500000409677625 ) ) ;
#11540 = ORIENTED_EDGE ( 'NONE', *, *, #17511, .F. ) ;
#11541 = CARTESIAN_POINT ( 'NONE',  ( -10.81189881249999729, -6.242252689847864744, -40.96875000204835260 ) ) ;
#11542 = CARTESIAN_POINT ( 'NONE',  ( -4.999999999999996447, 8.660254037844387298, -76.87500000409677625 ) ) ;
#11543 = CARTESIAN_POINT ( 'NONE',  ( 7.644554776091147741E-16, 12.48450537969573659, -11.65625000204835438 ) ) ;
#11545 = ORIENTED_EDGE ( 'NONE', *, *, #34606, .F. ) ;
#11544 = CARTESIAN_POINT ( 'NONE',  ( -5.405949406250003975, -9.363379034771801557, -66.34375000204836681 ) ) ;
#11546 = CARTESIAN_POINT ( 'NONE',  ( -9.999999999999998224, 5.773502691896259087, -38.87499999999997158 ) ) ;
#11547 = CARTESIAN_POINT ( 'NONE',  ( 5.405949406249992428, -9.363379034771808662, -187.5937500020483810 ) ) ;
#11548 = CARTESIAN_POINT ( 'NONE',  ( -10.81189881249999729, 6.242252689847871849, -168.7187500020483810 ) ) ;
#11549 = CARTESIAN_POINT ( 'NONE',  ( 10.81189881249999551, -6.242252689847874514, -178.4687500020484094 ) ) ;
#11550 = CARTESIAN_POINT ( 'NONE',  ( -2.121150477449813534E-15, -11.54700538379251284, -182.7500000040967905 ) ) ;
#11551 = CARTESIAN_POINT ( 'NONE',  ( -9.999999999999998224, 1.224646799147353059E-15, -168.1250000040967905 ) ) ;
#11552 = CARTESIAN_POINT ( 'NONE',  ( -10.00000000000076916, 5.773502691895813221, -125.8749999999999858 ) ) ;
#11553 = CARTESIAN_POINT ( 'NONE',  ( -9.999999999999998224, 5.773502691896259087, -194.8750000000000000 ) ) ;
#11554 = CARTESIAN_POINT ( 'NONE',  ( -2.293366432827344421E-15, -12.48450537969573659, -115.7187500020483952 ) ) ;
#11555 = CARTESIAN_POINT ( 'NONE',  ( 9.999999999999998224, 0.000000000000000000, -200.0000000000000000 ) ) ;
#11556 = AXIS2_PLACEMENT_3D ( 'NONE', #24433, #1766, #29099 ) ;
#11557 = CARTESIAN_POINT ( 'NONE',  ( 5.405949406249999534, 9.363379034771803333, -83.78125000204838102 ) ) ;
#11558 = CARTESIAN_POINT ( 'NONE',  ( 5.405949406249992428, -9.363379034771808662, -90.09375000204838102 ) ) ;
#11559 = AXIS2_PLACEMENT_3D ( 'NONE', #40001, #42386, #22553 ) ;
#11560 = CARTESIAN_POINT ( 'NONE',  ( -10.81189881249999907, -6.242252689847864744, -60.46875000204838102 ) ) ;
#11561 = CARTESIAN_POINT ( 'NONE',  ( 10.81189881249999907, 6.242252689847868297, -70.40625000204839523 ) ) ;
#11562 = CARTESIAN_POINT ( 'NONE',  ( 4.999999999999992006, -8.660254037844389075, -155.6250000040967905 ) ) ;
#11563 = CARTESIAN_POINT ( 'NONE',  ( -9.999999999999998224, 1.224646799147353059E-15, -133.2499999999999716 ) ) ;
#11564 = EDGE_CURVE ( 'NONE', #11901, #14343, #38713, .T. ) ;
#11565 = CARTESIAN_POINT ( 'NONE',  ( 10.81189881249999551, -6.242252689847874514, -148.6562500020484094 ) ) ;
#11566 = CARTESIAN_POINT ( 'NONE',  ( -5.405949406250003975, -9.363379034771801557, -162.5312500020484094 ) ) ;
#11567 = CARTESIAN_POINT ( 'NONE',  ( 9.999999999999866773, -5.773502691896336358, -174.6249999999999716 ) ) ;
#11568 = DIRECTION ( 'NONE',  ( -0.000000000000000000, -0.000000000000000000, 1.000000000000000000 ) ) ;
#11569 = CARTESIAN_POINT ( 'NONE',  ( -5.405949406250003975, -9.363379034771801557, -97.84375000204838102 ) ) ;
#11570 = CARTESIAN_POINT ( 'NONE',  ( -9.999999999999998224, 1.224646799147353059E-15, -42.12500000409677625 ) ) ;
#11571 = CARTESIAN_POINT ( 'NONE',  ( -4.999999999999996447, 8.660254037844387298, -74.99999999999998579 ) ) ;
#11572 = CARTESIAN_POINT ( 'NONE',  ( -2.293366432827344421E-15, -12.48450537969573659, -198.2187500020484379 ) ) ;
#11573 = CARTESIAN_POINT ( 'NONE',  ( -9.999999999999998224, 5.773502691896259087, -78.25000000409677625 ) ) ;
#11574 = CARTESIAN_POINT ( 'NONE',  ( 4.999999999999992006, -8.660254037844389075, -133.1250000040967620 ) ) ;
#11575 = CARTESIAN_POINT ( 'NONE',  ( -5.405949406249996869, 9.363379034771805109, -89.53125000204838102 ) ) ;
#11576 = CARTESIAN_POINT ( 'NONE',  ( -10.81189881249999729, 6.242252689847871849, -72.90625000204836681 ) ) ;
#11577 = CARTESIAN_POINT ( 'NONE',  ( -9.999999999999998224, 1.224646799147353059E-15, -70.62500000409677625 ) ) ;
#11578 = CARTESIAN_POINT ( 'NONE',  ( 5.405949406249999534, 9.363379034771803333, -29.59375000204836326 ) ) ;
#11579 = ORIENTED_EDGE ( 'NONE', *, *, #39797, .T. ) ;
#11580 = CARTESIAN_POINT ( 'NONE',  ( -9.999999999999998224, 1.224646799147353059E-15, -1.249999999999973355 ) ) ;
#11581 = CARTESIAN_POINT ( 'NONE',  ( 10.81189881249999907, 6.242252689847868297, -20.90625000204837747 ) ) ;
#11582 = CARTESIAN_POINT ( 'NONE',  ( 10.81189881249999729, 0.000000000000000000, -13.34375000204834905 ) ) ;
#11583 = CARTESIAN_POINT ( 'NONE',  ( 9.999999999999998224, 0.000000000000000000, -176.3750000040967905 ) ) ;
#11584 = CARTESIAN_POINT ( 'NONE',  ( -10.81189881249999729, 1.324075727343319199E-15, -143.0937500020483810 ) ) ;
#11585 = CARTESIAN_POINT ( 'NONE',  ( 9.999999999999996447, -5.773502691896262640, 0.4999999959032497276 ) ) ;
#11586 = CARTESIAN_POINT ( 'NONE',  ( 0.000000000000000000, 0.000000000000000000, -99.99999999999998579 ) ) ;
#11587 = CARTESIAN_POINT ( 'NONE',  ( 10.81189881249999729, 0.000000000000000000, -130.5312500020484094 ) ) ;
#11588 = CARTESIAN_POINT ( 'NONE',  ( 7.070501591499377789E-16, 11.54700538379251284, -181.6250000000000000 ) ) ;
#11589 = DIRECTION ( 'NONE',  ( -0.000000000000000000, -0.000000000000000000, 1.000000000000000000 ) ) ;
#11591 = ORIENTED_EDGE ( 'NONE', *, *, #13019, .T. ) ;
#11590 = CARTESIAN_POINT ( 'NONE',  ( 5.405949406249999534, 9.363379034771803333, -110.7812500020483810 ) ) ;
#11592 = CARTESIAN_POINT ( 'NONE',  ( -4.999999999999996447, 8.660254037844387298, -195.0000000000000000 ) ) ;
#11593 = VECTOR ( 'NONE', #15163, 1000.000000000000000 ) ;
#11594 = ORIENTED_EDGE ( 'NONE', *, *, #21376, .T. ) ;
#11595 =( BOUNDED_CURVE ( )  B_SPLINE_CURVE ( 2, ( #26848, #17114, #10641, #30530, #14290, #27066, #21004 ),
 .UNSPECIFIED., .F., .F. ) 
 B_SPLINE_CURVE_WITH_KNOTS ( ( 3, 2, 2, 3 ),
 ( 0.8320895522388060961, 0.8333333333333334814, 0.8345771144278608666, 0.8358208955223882519 ),
 .UNSPECIFIED. ) 
 CURVE ( )  GEOMETRIC_REPRESENTATION_ITEM ( )  RATIONAL_B_SPLINE_CURVE ( ( 0.9999999999999880096, 0.8660254037844506980, 1.000000000000000000, 0.8660254037844387076, 1.000000000000000000, 0.8660254037844148378, 1.000000000000023981 ) ) 
 REPRESENTATION_ITEM ( '' )  );
#11596 = ORIENTED_EDGE ( 'NONE', *, *, #2480, .F. ) ;
#11597 = CARTESIAN_POINT ( 'NONE',  ( -10.81189881249999907, -6.242252689847864744, -41.15625000204836681 ) ) ;
#11598 = COORDINATED_UNIVERSAL_TIME_OFFSET ( 6, 0, .AHEAD. ) ;
#11599 = CARTESIAN_POINT ( 'NONE',  ( 5.405949406249999534, 9.363379034771803333, -86.59375000204836681 ) ) ;
#11600 = CARTESIAN_POINT ( 'NONE',  ( -1.040834085586084257E-14, -145.0000000000000000, 22.49999999999999289 ) ) ;
#11601 = CARTESIAN_POINT ( 'NONE',  ( 5.000000000000000000, 8.660254037844385522, -114.2499999999999858 ) ) ;
#11602 = CARTESIAN_POINT ( 'NONE',  ( -5.000000000000003553, -8.660254037844383745, -32.87500000409676915 ) ) ;
#11603 = CARTESIAN_POINT ( 'NONE',  ( -10.81189881249999907, -6.242252689847864744, -165.6562500020483810 ) ) ;
#11604 = DIRECTION ( 'NONE',  ( 1.000000000000000000, 0.000000000000000000, 0.000000000000000000 ) ) ;
#11605 = CARTESIAN_POINT ( 'NONE',  ( 10.81189881249999729, 0.000000000000000000, -112.3437500020483810 ) ) ;
#11606 = CARTESIAN_POINT ( 'NONE',  ( 10.81189881249999729, 0.000000000000000000, -82.34375000204836681 ) ) ;
#11607 = CARTESIAN_POINT ( 'NONE',  ( 5.405949406249999534, 9.363379034771803333, -4.281250002048375691 ) ) ;
#11608 = CARTESIAN_POINT ( 'NONE',  ( -5.405949406249996869, 9.363379034771805109, -191.3437500020484094 ) ) ;
#11609 = CARTESIAN_POINT ( 'NONE',  ( 5.405949406249999534, 9.363379034771803333, -94.28125000204838102 ) ) ;
#11610 = CARTESIAN_POINT ( 'NONE',  ( -10.00000000000000000, -5.773502691896251982, -180.0000000040967905 ) ) ;
#11611 = CARTESIAN_POINT ( 'NONE',  ( 10.81189881249999551, -6.242252689847874514, -172.6562500020484094 ) ) ;
#11612 = CARTESIAN_POINT ( 'NONE',  ( -9.999999999999998224, 1.224646799147353059E-15, -144.1250000040967905 ) ) ;
#11613 = CARTESIAN_POINT ( 'NONE',  ( -5.405949406250003975, -9.363379034771801557, -176.0312500020483810 ) ) ;
#11614 = CARTESIAN_POINT ( 'NONE',  ( 10.81189881249999551, -6.242252689847874514, -190.6562500020484094 ) ) ;
#11615 = CARTESIAN_POINT ( 'NONE',  ( -10.81189881249999729, 6.242252689847871849, -50.21875000204835970 ) ) ;
#11616 = CARTESIAN_POINT ( 'NONE',  ( -10.00000000000000000, -5.773502691896251982, -163.5000000040967620 ) ) ;
#11617 = CARTESIAN_POINT ( 'NONE',  ( -5.405949406250003975, -9.363379034771801557, -8.031250002048350822 ) ) ;
#11618 = CARTESIAN_POINT ( 'NONE',  ( 10.81189881249999907, 6.242252689847868297, -10.21875000204835970 ) ) ;
#11619 = CARTESIAN_POINT ( 'NONE',  ( -9.999999999999998224, 1.224646799147353059E-15, -165.1250000040967905 ) ) ;
#11620 = CARTESIAN_POINT ( 'NONE',  ( -10.81189881249999729, 1.324075727343319199E-15, -125.0937500020483668 ) ) ;
#11621 = ADVANCED_FACE ( 'NONE', ( #3470 ), #3261, .T. ) ;
#11622 = CARTESIAN_POINT ( 'NONE',  ( -2.121150477449813534E-15, -11.54700538379251284, -93.87499999999997158 ) ) ;
#11623 = CARTESIAN_POINT ( 'NONE',  ( -5.405949406250003975, -9.363379034771801557, -21.53125000204836326 ) ) ;
#11624 = CARTESIAN_POINT ( 'NONE',  ( 5.000000000000000000, 8.660254037844385522, -107.1250000040967763 ) ) ;
#11625 = CARTESIAN_POINT ( 'NONE',  ( 9.999999999999998224, 0.000000000000000000, -197.0000000000000000 ) ) ;
#11626 = EDGE_CURVE ( 'NONE', #31885, #25488, #39502, .T. ) ;
#11627 = CARTESIAN_POINT ( 'NONE',  ( 4.999999999999992006, -8.660254037844389075, -54.74999999999996447 ) ) ;
#11628 = CARTESIAN_POINT ( 'NONE',  ( 10.81189881249999551, -6.242252689847874514, -118.6562500020483952 ) ) ;
#11629 = CARTESIAN_POINT ( 'NONE',  ( 10.81189881249999729, 0.000000000000000000, -100.5312500020483952 ) ) ;
#11630 = ORIENTED_EDGE ( 'NONE', *, *, #12241, .F. ) ;
#11631 = CARTESIAN_POINT ( 'NONE',  ( 7.070501591499377789E-16, 11.54700538379251284, -90.50000000409677625 ) ) ;
#11632 = CARTESIAN_POINT ( 'NONE',  ( -45.00000000000000711, 0.000000000000000000, -200.0000000000000000 ) ) ;
#11633 = CARTESIAN_POINT ( 'NONE',  ( 10.81189881249999907, 6.242252689847868297, -157.4062500020483810 ) ) ;
#11634 = CARTESIAN_POINT ( 'NONE',  ( 5.405949406249992428, -9.363379034771808662, -46.59375000204838102 ) ) ;
#11635 = ORIENTED_EDGE ( 'NONE', *, *, #35860, .T. ) ;
#11636 = CARTESIAN_POINT ( 'NONE',  ( -10.00000000000000000, -5.773502691896251982, -26.62499999999998224 ) ) ;
#11637 = VECTOR ( 'NONE', #40674, 1000.000000000000000 ) ;
#11638 = CARTESIAN_POINT ( 'NONE',  ( -10.81189881249999729, 6.242252689847871849, -29.40625000204835615 ) ) ;
#11639 = CARTESIAN_POINT ( 'NONE',  ( -9.999999999999998224, 5.773502691896259087, -161.8750000000000000 ) ) ;
#11640 = CARTESIAN_POINT ( 'NONE',  ( 9.999999999999998224, 0.000000000000000000, -90.49999999999998579 ) ) ;
#11641 = CARTESIAN_POINT ( 'NONE',  ( 5.000000000000000000, 8.660254037844385522, -26.12500000409675849 ) ) ;
#11642 =( BOUNDED_CURVE ( )  B_SPLINE_CURVE ( 2, ( #13562, #14413, #17231, #4509, #656, #27391, #10971 ),
 .UNSPECIFIED., .F., .F. ) 
 B_SPLINE_CURVE_WITH_KNOTS ( ( 3, 2, 2, 3 ),
 ( 0.2238805970149254365, 0.2251243781094527940, 0.2263681592039801793, 0.2276119402985075368 ),
 .UNSPECIFIED. ) 
 CURVE ( )  GEOMETRIC_REPRESENTATION_ITEM ( )  RATIONAL_B_SPLINE_CURVE ( ( 0.9999999999999940048, 0.8660254037844447028, 1.000000000000000000, 0.8660254037844387076, 1.000000000000000000, 0.8660254037844297148, 1.000000000000008882 ) ) 
 REPRESENTATION_ITEM ( '' )  );
#11643 = CIRCLE ( 'NONE', #23396, 9.750000000000001776 ) ;
#11644 = DIRECTION ( 'NONE',  ( -1.000000000000000000, 0.000000000000000000, 0.000000000000000000 ) ) ;
#11645 = CARTESIAN_POINT ( 'NONE',  ( 5.405949406249999534, 9.363379034771803333, -134.7812500020483810 ) ) ;
#11646 = CARTESIAN_POINT ( 'NONE',  ( 3.170450507625008019, 9.888387355072444151, 1.028787474604544383E-14 ) ) ;
#11647 = CARTESIAN_POINT ( 'NONE',  ( 9.999999999999998224, 0.000000000000000000, -68.37500000409677625 ) ) ;
#11648 = ORIENTED_EDGE ( 'NONE', *, *, #19041, .T. ) ;
#11649 =( BOUNDED_CURVE ( )  B_SPLINE_CURVE ( 2, ( #9475, #38616, #42262, #32159, #25051, #9053, #5606 ),
 .UNSPECIFIED., .F., .F. ) 
 B_SPLINE_CURVE_WITH_KNOTS ( ( 3, 2, 2, 3 ),
 ( 0.9701492537313435305, 0.9713930348258709158, 0.9726368159203981900, 0.9738805970149255753 ),
 .UNSPECIFIED. ) 
 CURVE ( )  GEOMETRIC_REPRESENTATION_ITEM ( )  RATIONAL_B_SPLINE_CURVE ( ( 0.9999999999999761302, 0.8660254037844625774, 1.000000000000000000, 0.8660254037844387076, 1.000000000000000000, 0.8660254037844148378, 1.000000000000023981 ) ) 
 REPRESENTATION_ITEM ( '' )  );
#11650 = CARTESIAN_POINT ( 'NONE',  ( -10.81189881249999729, 1.324075727343319199E-15, -65.28125000204838102 ) ) ;
#11651 = COORDINATED_UNIVERSAL_TIME_OFFSET ( 6, 0, .AHEAD. ) ;
#11653 = ORIENTED_EDGE ( 'NONE', *, *, #33333, .T. ) ;
#11652 = ORIENTED_EDGE ( 'NONE', *, *, #22674, .F. ) ;
#11654 = CARTESIAN_POINT ( 'NONE',  ( 10.00000000000102318, -5.773502691895667560, -46.00000000409674072 ) ) ;
#11655 = DIRECTION ( 'NONE',  ( -1.000000000000000000, 0.000000000000000000, 0.000000000000000000 ) ) ;
#11656 = CARTESIAN_POINT ( 'NONE',  ( 5.405949406249999534, 9.363379034771803333, -161.5937500020484094 ) ) ;
#11657 = CARTESIAN_POINT ( 'NONE',  ( 10.81189881249999729, 0.000000000000000000, -190.5312500020484094 ) ) ;
#11658 = CARTESIAN_POINT ( 'NONE',  ( 5.405949406249999534, 9.363379034771803333, -7.093750002048371250 ) ) ;
#11659 = VECTOR ( 'NONE', #2912, 1000.000000000000000 ) ;
#11660 = CARTESIAN_POINT ( 'NONE',  ( -10.81189881249999729, 1.324075727343319199E-15, -146.0937500020483810 ) ) ;
#11661 = CARTESIAN_POINT ( 'NONE',  ( -10.81189881249999907, -6.242252689847864744, -95.15625000204839523 ) ) ;
#11662 = CARTESIAN_POINT ( 'NONE',  ( -2.293366432827344421E-15, -12.48450537969573659, -112.7187500020483952 ) ) ;
#11663 = DIRECTION ( 'NONE',  ( 0.000000000000000000, 0.000000000000000000, 1.000000000000000000 ) ) ;
#11664 = CARTESIAN_POINT ( 'NONE',  ( -10.81189881249999907, -6.242252689847864744, -113.1562500020483952 ) ) ;
#11665 = CARTESIAN_POINT ( 'NONE',  ( -2.293366432827344421E-15, -12.48450537969573659, -4.718750002048369474 ) ) ;
#11666 = CARTESIAN_POINT ( 'NONE',  ( -5.405949406250003975, -9.363379034771801557, -127.8437500020483952 ) ) ;
#11667 = CARTESIAN_POINT ( 'NONE',  ( -10.81189881249999729, 1.324075727343319199E-15, -191.2812500020484094 ) ) ;
#11668 = AXIS2_PLACEMENT_3D ( 'NONE', #27937, #34421, #14744 ) ;
#11669 = DIRECTION ( 'NONE',  ( -0.000000000000000000, -0.000000000000000000, -1.000000000000000000 ) ) ;
#11670 = CARTESIAN_POINT ( 'NONE',  ( -9.999999999999998224, 1.224646799147353059E-15, -149.7500000000000000 ) ) ;
#11671 = CARTESIAN_POINT ( 'NONE',  ( 5.000000000000000000, 8.660254037844385522, -10.74999999999995381 ) ) ;
#11672 = CARTESIAN_POINT ( 'NONE',  ( 10.81189881249999729, 0.000000000000000000, -74.84375000204838102 ) ) ;
#11673 = CARTESIAN_POINT ( 'NONE',  ( -5.405949406250003975, -9.363379034771801557, -60.34375000204835970 ) ) ;
#11674 = CARTESIAN_POINT ( 'NONE',  ( 7.070501591499377789E-16, 11.54700538379251284, -188.0000000040967905 ) ) ;
#11675 = CARTESIAN_POINT ( 'NONE',  ( 10.81189881249999907, 6.242252689847868297, -31.40625000204834905 ) ) ;
#11676 = CARTESIAN_POINT ( 'NONE',  ( 7.644554776091147741E-16, 12.48450537969573659, -38.46875000204835260 ) ) ;
#11677 = DIRECTION ( 'NONE',  ( 1.000000000000000000, 0.000000000000000000, 0.000000000000000000 ) ) ;
#11678 = CARTESIAN_POINT ( 'NONE',  ( -5.405949406250003975, -9.363379034771801557, -145.8437500020483810 ) ) ;
#11679 = EDGE_CURVE ( 'NONE', #24959, #28547, #157, .T. ) ;
#11680 = CARTESIAN_POINT ( 'NONE',  ( -9.999999999999998224, 5.773502691896259087, -124.3750000000000000 ) ) ;
#11681 = ADVANCED_FACE ( 'NONE', ( #248 ), #15972, .T. ) ;
#11682 = CARTESIAN_POINT ( 'NONE',  ( -4.999999999999996447, 8.660254037844387298, -41.99999999999997868 ) ) ;
#11683 = EDGE_CURVE ( 'NONE', #12029, #30470, #20543, .T. ) ;
#11684 = CARTESIAN_POINT ( 'NONE',  ( -4.999999999999996447, 8.660254037844387298, -71.99999999999998579 ) ) ;
#11685 = CARTESIAN_POINT ( 'NONE',  ( -10.81189881249999729, 1.324075727343319199E-15, -141.7812500020483810 ) ) ;
#11686 = CARTESIAN_POINT ( 'NONE',  ( -5.405949406250003975, -9.363379034771801557, -9.531250002048352599 ) ) ;
#11687 = EDGE_CURVE ( 'NONE', #22477, #23032, #14990, .T. ) ;
#11688 = ORIENTED_EDGE ( 'NONE', *, *, #12166, .F. ) ;
#11689 = CARTESIAN_POINT ( 'NONE',  ( -5.000000000000003553, -8.660254037844383745, -164.5000000000000000 ) ) ;
#11690 = CARTESIAN_POINT ( 'NONE',  ( 9.999999999999998224, 0.000000000000000000, -122.3750000040967905 ) ) ;
#11691 = FACE_OUTER_BOUND ( 'NONE', #28980, .T. ) ;
#11692 = CARTESIAN_POINT ( 'NONE',  ( -10.81189881249999729, 1.324075727343319199E-15, -75.59375000204838102 ) ) ;
#11693 = CARTESIAN_POINT ( 'NONE',  ( 9.999999999999998224, 0.000000000000000000, -24.87500000409675849 ) ) ;
#11694 = LINE ( 'NONE', #41252, #24901 ) ;
#11695 = PRODUCT_RELATED_PRODUCT_CATEGORY ( 'detail', '', ( #1498 ) ) ;
#11696 = CARTESIAN_POINT ( 'NONE',  ( 10.81189881249999907, 6.242252689847868297, -41.90625000204836681 ) ) ;
#11697 = DIRECTION ( 'NONE',  ( 1.000000000000000000, 0.000000000000000000, 0.000000000000000000 ) ) ;
#11698 = CARTESIAN_POINT ( 'NONE',  ( 10.81189881249999907, 6.242252689847868297, -148.4062500020484094 ) ) ;
#11699 = CARTESIAN_POINT ( 'NONE',  ( -5.405949406249996869, 9.363379034771805109, -125.3437500020483952 ) ) ;
#11700 = CARTESIAN_POINT ( 'NONE',  ( 5.000000000000000000, 8.660254037844385522, -51.24999999999996447 ) ) ;
#11701 = ADVANCED_FACE ( 'NONE', ( #16389 ), #36274, .F. ) ;
#11702 = CARTESIAN_POINT ( 'NONE',  ( -5.000000000000003553, -8.660254037844383745, -57.99999999999997158 ) ) ;
#11703 = ORIENTED_EDGE ( 'NONE', *, *, #16335, .F. ) ;
#11704 = EDGE_CURVE ( 'NONE', #8850, #34991, #40083, .T. ) ;
#11705 = ORIENTED_EDGE ( 'NONE', *, *, #20399, .T. ) ;
#11706 = ORIENTED_EDGE ( 'NONE', *, *, #26481, .F. ) ;
#11707 = CARTESIAN_POINT ( 'NONE',  ( 4.999999999999992006, -8.660254037844389075, -145.1250000040967905 ) ) ;
#11708 = CARTESIAN_POINT ( 'NONE',  ( -10.81189881249999729, 6.242252689847871849, -180.7187500020483810 ) ) ;
#11709 = CARTESIAN_POINT ( 'NONE',  ( -10.81189881249999729, 1.324075727343319199E-15, -29.09375000204836326 ) ) ;
#11710 = CARTESIAN_POINT ( 'NONE',  ( 10.81189881249999729, 6.242252689847867408, -172.2187500020483810 ) ) ;
#11711 = CARTESIAN_POINT ( 'NONE',  ( -5.405949406250003975, -9.363379034771801557, -153.3437500020483810 ) ) ;
#11712 = ADVANCED_FACE ( 'NONE', ( #4741 ), #27410, .T. ) ;
#11713 =( BOUNDED_CURVE ( )  B_SPLINE_CURVE ( 2, ( #27037, #20977, #24019, #17941, #31140, #37160, #7396 ),
 .UNSPECIFIED., .F., .F. ) 
 B_SPLINE_CURVE_WITH_KNOTS ( ( 3, 2, 2, 3 ),
 ( 0.5223880597014926019, 0.5236318407960199872, 0.5248756218905473725, 0.5261194029850747578 ),
 .UNSPECIFIED. ) 
 CURVE ( )  GEOMETRIC_REPRESENTATION_ITEM ( )  RATIONAL_B_SPLINE_CURVE ( ( 0.9999999999999880096, 0.8660254037844506980, 1.000000000000000000, 0.8660254037844387076, 1.000000000000000000, 0.8660254037844267172, 1.000000000000011990 ) ) 
 REPRESENTATION_ITEM ( '' )  );
#11714 = DIRECTION ( 'NONE',  ( -0.000000000000000000, -0.000000000000000000, 1.000000000000000000 ) ) ;
#11715 = CARTESIAN_POINT ( 'NONE',  ( -10.81189881249999729, 6.242252689847871849, -132.7187500020483810 ) ) ;
#11716 = CARTESIAN_POINT ( 'NONE',  ( -10.81189881249999729, 1.324075727343319199E-15, -143.2812500020483810 ) ) ;
#11717 = CARTESIAN_POINT ( 'NONE',  ( -2.293366432827344421E-15, -12.48450537969573659, -157.7187500020483810 ) ) ;
#11718 = DIRECTION ( 'NONE',  ( -0.000000000000000000, -0.000000000000000000, 1.000000000000000000 ) ) ;
#11719 = CARTESIAN_POINT ( 'NONE',  ( 7.070501591499376803E-16, 11.54700538379251284, -11.00000000409676382 ) ) ;
#11720 = CARTESIAN_POINT ( 'NONE',  ( -10.00000000000000000, -5.773502691896251982, -169.1249999999999716 ) ) ;
#11721 = VECTOR ( 'NONE', #18934, 1000.000000000000114 ) ;
#11722 = CARTESIAN_POINT ( 'NONE',  ( -10.81189881249999729, 1.324075727343319199E-15, -80.09375000204838102 ) ) ;
#11723 = CARTESIAN_POINT ( 'NONE',  ( 4.999999999999992006, -8.660254037844389075, -135.7499999999999716 ) ) ;
#11724 = CARTESIAN_POINT ( 'NONE',  ( 7.644554776091147741E-16, 12.48450537969573659, -61.15625000204838102 ) ) ;
#11725 = CARTESIAN_POINT ( 'NONE',  ( 4.999999999999992006, -8.660254037844389075, -149.2500000000000000 ) ) ;
#11726 = CARTESIAN_POINT ( 'NONE',  ( -10.81189881249999907, -6.242252689847864744, -171.4687500020484094 ) ) ;
#11727 = CARTESIAN_POINT ( 'NONE',  ( -10.81189881249999729, 1.324075727343319199E-15, -117.7812500020483952 ) ) ;
#11728 = CARTESIAN_POINT ( 'NONE',  ( 7.644554776091147741E-16, 12.48450537969573659, -155.6562500020483810 ) ) ;
#11729 = CARTESIAN_POINT ( 'NONE',  ( 9.999999999999998224, 0.000000000000000000, -103.9999999999999858 ) ) ;
#11730 = CARTESIAN_POINT ( 'NONE',  ( -2.293366432827344421E-15, -12.48450537969573659, -43.90625000204837391 ) ) ;
#11731 = CARTESIAN_POINT ( 'NONE',  ( 9.999999999999996447, -5.773502691896262640, -124.0000000040967763 ) ) ;
#11732 = CARTESIAN_POINT ( 'NONE',  ( -5.000000000000003553, -8.660254037844383745, -96.99999999999998579 ) ) ;
#11733 = ORIENTED_EDGE ( 'NONE', *, *, #27221, .F. ) ;
#11734 = CARTESIAN_POINT ( 'NONE',  ( -5.405949406250003975, -9.363379034771801557, -128.0312500020484094 ) ) ;
#11735 = CARTESIAN_POINT ( 'NONE',  ( 9.999999999999996447, -5.773502691896262640, -149.5000000040968189 ) ) ;
#11736 = DIRECTION ( 'NONE',  ( -0.000000000000000000, -0.000000000000000000, 1.000000000000000000 ) ) ;
#11737 = CARTESIAN_POINT ( 'NONE',  ( 10.81189881249999729, 0.000000000000000000, -180.0312500020483810 ) ) ;
#11738 = EDGE_LOOP ( 'NONE', ( #26943, #20253, #18571, #13600 ) ) ;
#11739 = CARTESIAN_POINT ( 'NONE',  ( 5.405949406249992428, -9.363379034771808662, -171.0937500020484094 ) ) ;
#11740 = CARTESIAN_POINT ( 'NONE',  ( 10.00000000000000000, 5.773502691896255534, -57.75000000409677625 ) ) ;
#11741 = FACE_OUTER_BOUND ( 'NONE', #9536, .T. ) ;
#11742 = CARTESIAN_POINT ( 'NONE',  ( -9.999999999999998224, 1.224646799147353059E-15, -134.7499999999999716 ) ) ;
#11743 = CARTESIAN_POINT ( 'NONE',  ( -5.405949406249996869, 9.363379034771805109, -67.03125000204838102 ) ) ;
#11744 = CARTESIAN_POINT ( 'NONE',  ( 9.999999999999998224, 0.000000000000000000, -41.37500000409677625 ) ) ;
#11745 = CARTESIAN_POINT ( 'NONE',  ( 7.644554776091147741E-16, 12.48450537969573659, -5.468750002048355263 ) ) ;
#11746 = CARTESIAN_POINT ( 'NONE',  ( 5.000000000000000000, 8.660254037844385522, -9.625000004096746054 ) ) ;
#11747 = CARTESIAN_POINT ( 'NONE',  ( 10.81189881249999907, 6.242252689847868297, -172.4062500020484094 ) ) ;
#11748 = EDGE_CURVE ( 'NONE', #33393, #28805, #32427, .T. ) ;
#11749 = CARTESIAN_POINT ( 'NONE',  ( 7.071067811865472841, 7.071067811865472841, -200.0000000000000000 ) ) ;
#11750 = ORIENTED_EDGE ( 'NONE', *, *, #29145, .T. ) ;
#11751 = CARTESIAN_POINT ( 'NONE',  ( 5.000000000000000000, 8.660254037844385522, -123.6250000040967905 ) ) ;
#11752 = CARTESIAN_POINT ( 'NONE',  ( -10.00000000000051337, 5.773502691895962435, -39.25000000409674072 ) ) ;
#11753 = VECTOR ( 'NONE', #40513, 1000.000000000000000 ) ;
#11755 = ORIENTED_EDGE ( 'NONE', *, *, #23564, .T. ) ;
#11754 = CARTESIAN_POINT ( 'NONE',  ( 10.81189881249999551, -6.242252689847874514, -79.65625000204838102 ) ) ;
#11756 = AXIS2_PLACEMENT_3D ( 'NONE', #2233, #28556, #11697 ) ;
#11758 = VERTEX_POINT ( 'NONE', #20709 ) ;
#11757 = CARTESIAN_POINT ( 'NONE',  ( -5.000000000000003553, -8.660254037844383745, -140.5000000000000000 ) ) ;
#11759 = ORIENTED_EDGE ( 'NONE', *, *, #37514, .F. ) ;
#11760 =( BOUNDED_CURVE ( )  B_SPLINE_CURVE ( 2, ( #38939, #9370, #22540, #35713, #32480, #2906, #33327 ),
 .UNSPECIFIED., .F., .F. ) 
 B_SPLINE_CURVE_WITH_KNOTS ( ( 3, 2, 2, 3 ),
 ( 0.5895522388059702967, 0.5907960199004975710, 0.5920398009950249563, 0.5932835820895523415 ),
 .UNSPECIFIED. ) 
 CURVE ( )  GEOMETRIC_REPRESENTATION_ITEM ( )  RATIONAL_B_SPLINE_CURVE ( ( 0.9999999999999880096, 0.8660254037844506980, 1.000000000000000000, 0.8660254037844387076, 1.000000000000000000, 0.8660254037844267172, 1.000000000000011990 ) ) 
 REPRESENTATION_ITEM ( '' )  );
#11761 = CARTESIAN_POINT ( 'NONE',  ( 10.81189881249999729, 0.000000000000000000, -35.84375000204836681 ) ) ;
#11762 = CARTESIAN_POINT ( 'NONE',  ( 9.999999999999998224, 0.000000000000000000, -77.37500000409677625 ) ) ;
#11763 = CARTESIAN_POINT ( 'NONE',  ( 10.81189881249999907, 6.242252689847868297, -8.906250002048375691 ) ) ;
#11765 = VERTEX_POINT ( 'NONE', #17248 ) ;
#11764 = CARTESIAN_POINT ( 'NONE',  ( 5.405949406249992428, -9.363379034771808662, -66.09375000204836681 ) ) ;
#11766 = DIRECTION ( 'NONE',  ( -0.000000000000000000, -0.000000000000000000, -1.000000000000000000 ) ) ;
#11767 = CARTESIAN_POINT ( 'NONE',  ( -9.999999999999998224, 1.224646799147353059E-15, -40.24999999999997868 ) ) ;
#11768 = CARTESIAN_POINT ( 'NONE',  ( 10.81189881249999729, 6.242252689847867408, -199.2187500020484094 ) ) ;
#11769 = CARTESIAN_POINT ( 'NONE',  ( -5.405949406249996869, 9.363379034771805109, -174.8437500020484094 ) ) ;
#11770 = CARTESIAN_POINT ( 'NONE',  ( -10.81189881249999729, 1.324075727343319199E-15, -155.0937500020483810 ) ) ;
#11771 = CARTESIAN_POINT ( 'NONE',  ( 7.644554776091147741E-16, 12.48450537969573659, -177.9687500020484094 ) ) ;
#11772 = CARTESIAN_POINT ( 'NONE',  ( 7.070501591499376803E-16, 11.54700538379251284, -18.50000000409676559 ) ) ;
#11773 = DIRECTION ( 'NONE',  ( -0.000000000000000000, -0.000000000000000000, -1.000000000000000000 ) ) ;
#11774 = CARTESIAN_POINT ( 'NONE',  ( -9.999999999999998224, 5.773502691896259087, -191.8750000000000000 ) ) ;
#11775 = CARTESIAN_POINT ( 'NONE',  ( 10.81189881249999551, -6.242252689847874514, -103.4687500020483810 ) ) ;
#11776 = CARTESIAN_POINT ( 'NONE',  ( -9.999999999999998224, 1.224646799147353059E-15, -100.6250000040967905 ) ) ;
#11777 = CARTESIAN_POINT ( 'NONE',  ( 7.644554776091147741E-16, 12.48450537969573659, -80.65625000204839523 ) ) ;
#11778 = CARTESIAN_POINT ( 'NONE',  ( 10.81189881249999729, 0.000000000000000000, -91.34375000204838102 ) ) ;
#11779 = CARTESIAN_POINT ( 'NONE',  ( 7.644554776091147741E-16, 12.48450537969573659, -67.15625000204838102 ) ) ;
#11780 = CARTESIAN_POINT ( 'NONE',  ( -4.999999999999996447, 8.660254037844387298, -156.3750000040967905 ) ) ;
#11781 = CARTESIAN_POINT ( 'NONE',  ( -9.999999999999998224, 5.773502691896259087, -124.3750000000000000 ) ) ;
#11782 = AXIS2_PLACEMENT_3D ( 'NONE', #21034, #10251, #16720 ) ;
#11783 = CARTESIAN_POINT ( 'NONE',  ( 5.405949406249999534, 9.363379034771803333, -146.7812500020483810 ) ) ;
#11784 = CARTESIAN_POINT ( 'NONE',  ( 10.81189881249999551, -6.242252689847874514, -168.1562500020484094 ) ) ;
#11785 =( GEOMETRIC_REPRESENTATION_CONTEXT ( 3 ) GLOBAL_UNCERTAINTY_ASSIGNED_CONTEXT ( ( #12723 ) ) GLOBAL_UNIT_ASSIGNED_CONTEXT ( ( #35513, #38737, #42168 ) ) REPRESENTATION_CONTEXT ( 'NONE', 'WORKASPACE' ) );
#11786 = DIRECTION ( 'NONE',  ( 1.000000000000000000, 0.000000000000000000, 0.000000000000000000 ) ) ;
#11787 = CARTESIAN_POINT ( 'NONE',  ( 5.405949406249992428, -9.363379034771808662, -97.59375000204838102 ) ) ;
#11788 = ORIENTED_EDGE ( 'NONE', *, *, #14049, .T. ) ;
#11789 = CARTESIAN_POINT ( 'NONE',  ( 5.000000000000000000, 8.660254037844385522, -67.74999999999997158 ) ) ;
#11790 = CARTESIAN_POINT ( 'NONE',  ( -2.293366432827344421E-15, -12.48450537969573659, -195.2187500020484094 ) ) ;
#11791 = CARTESIAN_POINT ( 'NONE',  ( 4.999999999999992006, -8.660254037844389075, -85.12500000409677625 ) ) ;
#11792 = CARTESIAN_POINT ( 'NONE',  ( 7.099235607825172600, -8.054141481624315091, -180.0000000000000000 ) ) ;
#11793 = CARTESIAN_POINT ( 'NONE',  ( 9.999999999999998224, 0.000000000000000000, -137.3750000040967905 ) ) ;
#11794 = CARTESIAN_POINT ( 'NONE',  ( -5.405949406250003975, -9.363379034771801557, -93.53125000204838102 ) ) ;
#11795 = CARTESIAN_POINT ( 'NONE',  ( -5.405949406250003975, -9.363379034771801557, -77.03125000204838102 ) ) ;
#11796 = CARTESIAN_POINT ( 'NONE',  ( -4.999999999999996447, 8.660254037844387298, -66.37500000409676204 ) ) ;
#11797 = CARTESIAN_POINT ( 'NONE',  ( -9.999999999999998224, 1.224646799147353059E-15, -78.12500000409677625 ) ) ;
#11798 = CARTESIAN_POINT ( 'NONE',  ( -10.81189881249999729, 1.324075727343319199E-15, -24.59375000204835970 ) ) ;
#11799 = ORIENTED_EDGE ( 'NONE', *, *, #34413, .T. ) ;
#11800 = CARTESIAN_POINT ( 'NONE',  ( 5.405949406249999534, 9.363379034771803333, -190.2812500020484094 ) ) ;
#11801 = EDGE_CURVE ( 'NONE', #16199, #25687, #37063, .T. ) ;
#11802 = CARTESIAN_POINT ( 'NONE',  ( 10.81189881249999551, -6.242252689847874514, -21.15625000204837391 ) ) ;
#11803 = CARTESIAN_POINT ( 'NONE',  ( -10.81189881249999729, 1.324075727343319199E-15, -6.593750002048370362 ) ) ;
#11804 = CARTESIAN_POINT ( 'NONE',  ( -5.000000000000003553, -8.660254037844383745, -94.37500000409677625 ) ) ;
#11805 = CARTESIAN_POINT ( 'NONE',  ( -2.293366432827344421E-15, -12.48450537969573659, -145.7187500020484094 ) ) ;
#11806 = CARTESIAN_POINT ( 'NONE',  ( 9.999999999999872102, 5.773502691896329253, -161.2500000040967905 ) ) ;
#11807 = CARTESIAN_POINT ( 'NONE',  ( 10.00000000000000000, 5.773502691896255534, -180.3750000000000284 ) ) ;
#11808 = CARTESIAN_POINT ( 'NONE',  ( 9.999999999999548805, 5.773502691896514882, -176.2500000040967905 ) ) ;
#11810 = ORIENTED_EDGE ( 'NONE', *, *, #26407, .F. ) ;
#11809 = CARTESIAN_POINT ( 'NONE',  ( 10.81189881249999729, 0.000000000000000000, -100.5312500020483952 ) ) ;
#11811 = CARTESIAN_POINT ( 'NONE',  ( 9.999999999999998224, 0.000000000000000000, -200.0000000000000000 ) ) ;
#11812 = ORIENTED_EDGE ( 'NONE', *, *, #29149, .F. ) ;
#11813 = ORIENTED_EDGE ( 'NONE', *, *, #37255, .T. ) ;
#11814 = EDGE_CURVE ( 'NONE', #5330, #38561, #10563, .T. ) ;
#11815 = CARTESIAN_POINT ( 'NONE',  ( -10.81189881249999729, 1.324075727343319199E-15, -39.78125000204838102 ) ) ;
#11816 = PERSON_AND_ORGANIZATION ( #11915, #17965 ) ;
#11817 = CC_DESIGN_APPROVAL ( #40192, ( #24948 ) ) ;
#11818 = CARTESIAN_POINT ( 'NONE',  ( -10.81189881249999729, 6.242252689847871849, -84.71875000204836681 ) ) ;
#11819 = CARTESIAN_POINT ( 'NONE',  ( -9.999999999999998224, 0.000000000000000000, -99.99999999999998579 ) ) ;
#11820 = DIRECTION ( 'NONE',  ( -0.000000000000000000, -0.000000000000000000, 1.000000000000000000 ) ) ;
#11821 = CARTESIAN_POINT ( 'NONE',  ( 9.999999999999998224, 0.000000000000000000, -63.87500000409676915 ) ) ;
#11822 = CARTESIAN_POINT ( 'NONE',  ( 5.405949406249992428, -9.363379034771808662, -162.2812500020484094 ) ) ;
#11823 = AXIS2_PLACEMENT_3D ( 'NONE', #41216, #8660, #11655 ) ;
#11824 = CARTESIAN_POINT ( 'NONE',  ( -2.121150477449813534E-15, -11.54700538379251284, -86.37500000000000000 ) ) ;
#11825 = CARTESIAN_POINT ( 'NONE',  ( 10.81189881249999729, 6.242252689847867408, -119.7187500020483810 ) ) ;
#11826 = CARTESIAN_POINT ( 'NONE',  ( 10.81189881249999729, 0.000000000000000000, -83.84375000204836681 ) ) ;
#11827 = CARTESIAN_POINT ( 'NONE',  ( -5.405949406249996869, 9.363379034771805109, -2.531250002048373915 ) ) ;
#11828 = CARTESIAN_POINT ( 'NONE',  ( 10.81189881249999907, 6.242252689847868297, -190.2187500020484094 ) ) ;
#11829 = CARTESIAN_POINT ( 'NONE',  ( 10.81189881249999729, 0.000000000000000000, -93.03125000204838102 ) ) ;
#11830 = CARTESIAN_POINT ( 'NONE',  ( -9.999999999999998224, 5.773502691896259087, -177.2500000040967905 ) ) ;
#11831 = CARTESIAN_POINT ( 'NONE',  ( -2.293366432827344421E-15, -12.48450537969573659, -172.9062500020484379 ) ) ;
#11832 = CARTESIAN_POINT ( 'NONE',  ( -9.999999999999998224, 1.224646799147353059E-15, -169.6250000040967905 ) ) ;
#11833 = CARTESIAN_POINT ( 'NONE',  ( 10.81189881249999729, 0.000000000000000000, -174.0312500020484094 ) ) ;
#11834 = CARTESIAN_POINT ( 'NONE',  ( 5.405949406249992428, -9.363379034771808662, -186.2812500020484094 ) ) ;
#11835 = CARTESIAN_POINT ( 'NONE',  ( -10.81189881249999729, 1.324075727343319199E-15, -42.59375000204837391 ) ) ;
#11836 = CARTESIAN_POINT ( 'NONE',  ( -4.999999999999996447, 8.660254037844387298, -160.8750000040967905 ) ) ;
#11837 = CARTESIAN_POINT ( 'NONE',  ( -10.81189881249999729, 1.324075727343319199E-15, -2.281250002048373915 ) ) ;
#11838 = CARTESIAN_POINT ( 'NONE',  ( 5.405949406249992428, -9.363379034771808662, -15.09375000204835082 ) ) ;
#11839 = CARTESIAN_POINT ( 'NONE',  ( -10.00000000000000000, -5.773502691896252870, -165.0000000040967905 ) ) ;
#11840 = CARTESIAN_POINT ( 'NONE',  ( 10.81189881249999729, 0.000000000000000000, -119.8437500020483810 ) ) ;
#11841 = CARTESIAN_POINT ( 'NONE',  ( -9.999999999999998224, 5.773502691896259087, -86.87499999999998579 ) ) ;
#11842 = CARTESIAN_POINT ( 'NONE',  ( 5.405949406249992428, -9.363379034771808662, -21.28125000204836326 ) ) ;
#11843 = CARTESIAN_POINT ( 'NONE',  ( -5.000000000000003553, -8.660254037844383745, -103.3750000040967763 ) ) ;
#11844 = CARTESIAN_POINT ( 'NONE',  ( -2.121150477449813534E-15, -11.54700538379251284, -149.7500000040968189 ) ) ;
#11845 = CARTESIAN_POINT ( 'NONE',  ( 9.999999999999998224, 0.000000000000000000, -54.49999999999996447 ) ) ;
#11846 = CARTESIAN_POINT ( 'NONE',  ( 5.405949406249992428, -9.363379034771808662, -117.2812500020483952 ) ) ;
#11847 = CARTESIAN_POINT ( 'NONE',  ( -5.405949406249996869, 9.363379034771805109, -101.5312500020483952 ) ) ;
#11848 = ORIENTED_EDGE ( 'NONE', *, *, #25689, .F. ) ;
#11849 = AXIS2_PLACEMENT_3D ( 'NONE', #15685, #35574, #31920 ) ;
#11850 = EDGE_CURVE ( 'NONE', #13534, #38098, #39829, .T. ) ;
#11851 = CARTESIAN_POINT ( 'NONE',  ( -5.000000000000003553, -8.660254037844383745, -94.37500000409677625 ) ) ;
#11852 = CARTESIAN_POINT ( 'NONE',  ( 7.070501591499376803E-16, 11.54700538379251284, -29.00000000409674783 ) ) ;
#11853 = CARTESIAN_POINT ( 'NONE',  ( -10.81189881249999729, 1.324075727343319199E-15, -155.2812500020484094 ) ) ;
#11854 = CARTESIAN_POINT ( 'NONE',  ( 7.644554776091147741E-16, 12.48450537969573659, -48.96875000204836681 ) ) ;
#11855 = VERTEX_POINT ( 'NONE', #23542 ) ;
#11856 = CARTESIAN_POINT ( 'NONE',  ( 4.999999999999992006, -8.660254037844389075, -27.74999999999996803 ) ) ;
#11857 = APPLICATION_CONTEXT ( 'configuration controlled 3d designs of mechanical parts and assemblies' ) ;
#11858 = CARTESIAN_POINT ( 'NONE',  ( 5.405949406249999534, 9.363379034771803333, -29.78125000204837036 ) ) ;
#11859 = CARTESIAN_POINT ( 'NONE',  ( 5.000000000000000000, 8.660254037844385522, -165.2500000000000000 ) ) ;
#11860 =( BOUNDED_CURVE ( )  B_SPLINE_CURVE ( 2, ( #41530, #2689, #9158, #38298, #18440, #15822, #28816 ),
 .UNSPECIFIED., .F., .F. ) 
 B_SPLINE_CURVE_WITH_KNOTS ( ( 3, 2, 2, 3 ),
 ( 0.5746268656716420065, 0.5758706467661693917, 0.5771144278606968880, 0.5783582089552241623 ),
 .UNSPECIFIED. ) 
 CURVE ( )  GEOMETRIC_REPRESENTATION_ITEM ( )  RATIONAL_B_SPLINE_CURVE ( ( 0.9999999999999761302, 0.8660254037844625774, 1.000000000000000000, 0.8660254037844387076, 1.000000000000000000, 0.8660254037844028474, 1.000000000000035971 ) ) 
 REPRESENTATION_ITEM ( '' )  );
#11861 = CARTESIAN_POINT ( 'NONE',  ( 9.999999999999996447, -5.773502691896262640, -23.50000000409677270 ) ) ;
#11862 = CARTESIAN_POINT ( 'NONE',  ( -10.00000000000012434, 5.773502691896184480, -167.8749999999999716 ) ) ;
#11863 = CARTESIAN_POINT ( 'NONE',  ( -10.81189881249999907, -6.242252689847864744, -123.6562500020484094 ) ) ;
#11864 = CARTESIAN_POINT ( 'NONE',  ( -4.265126633838427495, 9.090591124651073329, 7.031793886498073594E-15 ) ) ;
#11865 = LINE ( 'NONE', #18563, #18308 ) ;
#11866 = ORIENTED_EDGE ( 'NONE', *, *, #7750, .T. ) ;
#11867 = CARTESIAN_POINT ( 'NONE',  ( 5.405949406249992428, -9.363379034771808662, -64.78125000204838102 ) ) ;
#11868 = APPROVAL_ROLE ( '' ) ;
#11869 = CARTESIAN_POINT ( 'NONE',  ( 10.81189881249999551, -6.242252689847874514, -107.9687500020483810 ) ) ;
#11870 = EDGE_CURVE ( 'NONE', #17989, #25211, #11377, .T. ) ;
#11872 = ORIENTED_EDGE ( 'NONE', *, *, #16038, .F. ) ;
#11871 = VERTEX_POINT ( 'NONE', #17035 ) ;
#11873 = CARTESIAN_POINT ( 'NONE',  ( -10.00000000000038547, 5.773502691896036154, -181.7500000040967905 ) ) ;
#11874 = CARTESIAN_POINT ( 'NONE',  ( -2.121150477449813534E-15, -11.54700538379251284, -183.8750000000000000 ) ) ;
#11875 = CARTESIAN_POINT ( 'NONE',  ( -5.405949406250003975, -9.363379034771801557, -157.8437500020483810 ) ) ;
#11876 = CARTESIAN_POINT ( 'NONE',  ( 7.644554776091147741E-16, 12.48450537969573659, -185.6562500020484094 ) ) ;
#11877 = CARTESIAN_POINT ( 'NONE',  ( -10.81189881249999729, 1.324075727343319199E-15, -5.093750002048369474 ) ) ;
#11878 = CARTESIAN_POINT ( 'NONE',  ( 10.81189881249999551, -6.242252689847874514, -136.4687500020483810 ) ) ;
#11879 = CARTESIAN_POINT ( 'NONE',  ( -10.81189881249999907, -6.242252689847864744, -98.15625000204839523 ) ) ;
#11880 = CARTESIAN_POINT ( 'NONE',  ( -10.81189881249999729, 1.324075727343319199E-15, -111.5937500020483810 ) ) ;
#11881 = CARTESIAN_POINT ( 'NONE',  ( -9.999999999999479527, -5.773502691896549521, -150.0000000040967905 ) ) ;
#11882 = CARTESIAN_POINT ( 'NONE',  ( 10.81189881249999551, -6.242252689847874514, -117.1562500020483810 ) ) ;
#11883 = CARTESIAN_POINT ( 'NONE',  ( -5.405949406249996869, 9.363379034771805109, 0.6562499979516356330 ) ) ;
#11884 = CARTESIAN_POINT ( 'NONE',  ( 10.81189881249999551, -6.242252689847874514, -125.9687500020483810 ) ) ;
#11885 = CARTESIAN_POINT ( 'NONE',  ( 10.81189881249999551, -6.242252689847874514, -195.1562500020484094 ) ) ;
#11886 = CARTESIAN_POINT ( 'NONE',  ( -5.000000000000003553, -8.660254037844383745, -5.875000004096770034 ) ) ;
#11887 = CARTESIAN_POINT ( 'NONE',  ( -4.999999999999996447, 8.660254037844387298, -147.0000000000000000 ) ) ;
#11888 = CARTESIAN_POINT ( 'NONE',  ( 7.070501591499377789E-16, 11.54700538379251284, -9.124999999999966249 ) ) ;
#11889 = AXIS2_PLACEMENT_3D ( 'NONE', #20130, #33318, #24459 ) ;
#11890 = CARTESIAN_POINT ( 'NONE',  ( 10.81189881249999729, 0.000000000000000000, -64.34375000204836681 ) ) ;
#11891 = CARTESIAN_POINT ( 'NONE',  ( 10.81189881249999907, 6.242252689847868297, -59.71875000204838102 ) ) ;
#11892 = CARTESIAN_POINT ( 'NONE',  ( -2.121150477449813534E-15, -11.54700538379251284, -185.7500000040967905 ) ) ;
#11893 = CARTESIAN_POINT ( 'NONE',  ( -10.81189881249999729, 6.242252689847871849, -27.90625000204838102 ) ) ;
#11894 = CARTESIAN_POINT ( 'NONE',  ( 5.405949406249999534, 9.363379034771803333, -40.09375000204837391 ) ) ;
#11895 = CARTESIAN_POINT ( 'NONE',  ( -5.000000000000003553, -8.660254037844383745, -163.3750000040967905 ) ) ;
#11896 = CARTESIAN_POINT ( 'NONE',  ( -10.81189881249999729, 6.242252689847871849, -143.2187500020484094 ) ) ;
#11897 = CARTESIAN_POINT ( 'NONE',  ( 9.999999999999996447, -5.773502691896262640, -119.1249999999999858 ) ) ;
#11898 = CARTESIAN_POINT ( 'NONE',  ( -10.00000000000000000, -5.773502691896251982, -71.62500000000000000 ) ) ;
#11899 = CARTESIAN_POINT ( 'NONE',  ( 5.405949406249999534, 9.363379034771803333, -142.2812500020483810 ) ) ;
#11900 = CARTESIAN_POINT ( 'NONE',  ( -5.405949406250003975, -9.363379034771801557, -11.03125000204835438 ) ) ;
#11901 = VERTEX_POINT ( 'NONE', #30235 ) ;
#11902 =( BOUNDED_CURVE ( )  B_SPLINE_CURVE ( 2, ( #3065, #42321, #16191, #42530, #12955, #9739, #7569 ),
 .UNSPECIFIED., .F., .F. ) 
 B_SPLINE_CURVE_WITH_KNOTS ( ( 3, 2, 2, 3 ),
 ( 0.9104477611940301474, 0.9116915422885575326, 0.9129353233830848069, 0.9141791044776121922 ),
 .UNSPECIFIED. ) 
 CURVE ( )  GEOMETRIC_REPRESENTATION_ITEM ( )  RATIONAL_B_SPLINE_CURVE ( ( 0.9999999999999641398, 0.8660254037844745678, 1.000000000000000000, 0.8660254037844387076, 1.000000000000000000, 0.8660254037844148378, 1.000000000000023981 ) ) 
 REPRESENTATION_ITEM ( '' )  );
#11903 = CARTESIAN_POINT ( 'NONE',  ( -10.81189881249999729, 1.324075727343319199E-15, -105.7812500020483810 ) ) ;
#11904 = CARTESIAN_POINT ( 'NONE',  ( 5.000000000000000000, 8.660254037844385522, -113.1250000040967763 ) ) ;
#11905 = CARTESIAN_POINT ( 'NONE',  ( 4.999999999999992006, -8.660254037844389075, -140.2500000000000000 ) ) ;
#11906 = CARTESIAN_POINT ( 'NONE',  ( 5.405949406249992428, -9.363379034771808662, -73.59375000204838102 ) ) ;
#11907 = CARTESIAN_POINT ( 'NONE',  ( -2.121150477449813534E-15, -11.54700538379251284, -23.75000000409677270 ) ) ;
#11908 = CARTESIAN_POINT ( 'NONE',  ( 9.999999999999998224, 0.000000000000000000, -93.49999999999998579 ) ) ;
#11909 = CARTESIAN_POINT ( 'NONE',  ( -5.405949406250003975, -9.363379034771801557, -44.03125000204838102 ) ) ;
#11910 =( BOUNDED_CURVE ( )  B_SPLINE_CURVE ( 2, ( #26779, #40142, #29815, #256, #13377, #19654, #26569 ),
 .UNSPECIFIED., .F., .F. ) 
 B_SPLINE_CURVE_WITH_KNOTS ( ( 3, 2, 2, 3 ),
 ( 0.2649253731343284568, 0.2661691542288558421, 0.2674129353233831718, 0.2686567164179105571 ),
 .UNSPECIFIED. ) 
 CURVE ( )  GEOMETRIC_REPRESENTATION_ITEM ( )  RATIONAL_B_SPLINE_CURVE ( ( 0.9999999999999880096, 0.8660254037844506980, 1.000000000000000000, 0.8660254037844387076, 1.000000000000000000, 0.8660254037844267172, 1.000000000000011990 ) ) 
 REPRESENTATION_ITEM ( '' )  );
#11911 = FACE_OUTER_BOUND ( 'NONE', #14278, .T. ) ;
#11912 = CARTESIAN_POINT ( 'NONE',  ( -5.405949406250003975, -9.363379034771801557, -144.5312500020483810 ) ) ;
#11913 = CARTESIAN_POINT ( 'NONE',  ( 10.81189881249999907, 6.242252689847868297, -127.2187500020483668 ) ) ;
#11914 = CARTESIAN_POINT ( 'NONE',  ( -2.275517850991317657E-15, -20.00000000000000000, -232.0000000000000000 ) ) ;
#11915 = PERSON ( 'UNSPECIFIED', 'UNSPECIFIED', 'UNSPECIFIED', ('UNSPECIFIED'), ('UNSPECIFIED'), ('UNSPECIFIED') ) ;
#11916 = LINE ( 'NONE', #18830, #1796 ) ;
#11917 = ORIENTED_EDGE ( 'NONE', *, *, #353, .T. ) ;
#11918 = EDGE_CURVE ( 'NONE', #28029, #16738, #39924, .T. ) ;
#11919 = ORIENTED_EDGE ( 'NONE', *, *, #32567, .F. ) ;
#11920 = EDGE_CURVE ( 'NONE', #11855, #31902, #26851, .T. ) ;
#11921 = ORIENTED_EDGE ( 'NONE', *, *, #38642, .T. ) ;
#11922 = EDGE_CURVE ( 'NONE', #34185, #22125, #30449, .T. ) ;
#11923 = CARTESIAN_POINT ( 'NONE',  ( -5.000000000000003553, -8.660254037844383745, -7.375000004096743389 ) ) ;
#11924 = CARTESIAN_POINT ( 'NONE',  ( -5.405949406250003975, -9.363379034771801557, -181.8437500020483810 ) ) ;
#11925 = CARTESIAN_POINT ( 'NONE',  ( -5.405949406250003975, -9.363379034771801557, -34.84375000204836681 ) ) ;
#11926 = DIRECTION ( 'NONE',  ( -0.000000000000000000, -0.000000000000000000, 1.000000000000000000 ) ) ;
#11927 = CARTESIAN_POINT ( 'NONE',  ( 10.81189881249999729, 0.000000000000000000, -166.3437500020484094 ) ) ;
#11928 = CARTESIAN_POINT ( 'NONE',  ( -10.81189881249999907, -6.242252689847864744, -151.9687500020484094 ) ) ;
#11929 = DIRECTION ( 'NONE',  ( -0.000000000000000000, -0.000000000000000000, 1.000000000000000000 ) ) ;
#11930 = CARTESIAN_POINT ( 'NONE',  ( -10.81189881249999907, -6.242252689847864744, -133.9687500020483810 ) ) ;
#11931 = CARTESIAN_POINT ( 'NONE',  ( 7.644554776091147741E-16, 12.48450537969573659, -140.6562500020484094 ) ) ;
#11932 = CARTESIAN_POINT ( 'NONE',  ( 5.405949406249992428, -9.363379034771808662, -144.0937500020483810 ) ) ;
#11933 = CARTESIAN_POINT ( 'NONE',  ( 7.070501591499376803E-16, 11.54700538379251284, -135.1250000000000000 ) ) ;
#11934 = CARTESIAN_POINT ( 'NONE',  ( 7.070501591499376803E-16, 11.54700538379251284, -169.6250000000000000 ) ) ;
#11935 = CARTESIAN_POINT ( 'NONE',  ( 4.999999999999992006, -8.660254037844389075, -171.7500000000000000 ) ) ;
#11936 = CARTESIAN_POINT ( 'NONE',  ( -5.405949406249996869, 9.363379034771805109, -78.84375000204838102 ) ) ;
#11937 = CARTESIAN_POINT ( 'NONE',  ( 9.999999999999998224, 0.000000000000000000, -128.3750000040967905 ) ) ;
#11938 = CARTESIAN_POINT ( 'NONE',  ( -10.81189881249999907, -6.242252689847864744, -59.15625000204838813 ) ) ;
#11939 = CARTESIAN_POINT ( 'NONE',  ( -8.268648510919758721, -5.984980119022559109, -100.0000000000000142 ) ) ;
#11940 = CARTESIAN_POINT ( 'NONE',  ( -2.293366432827344421E-15, -12.48450537969573659, -166.7187500020484094 ) ) ;
#11941 = EDGE_CURVE ( 'NONE', #31963, #20180, #25883, .T. ) ;
#11942 = CARTESIAN_POINT ( 'NONE',  ( 7.644554776091147741E-16, 12.48450537969573659, -113.6562500020483952 ) ) ;
#11943 = CARTESIAN_POINT ( 'NONE',  ( 10.81189881249999729, 0.000000000000000000, -148.5312500020483810 ) ) ;
#11944 = CARTESIAN_POINT ( 'NONE',  ( -10.00000000000102496, 5.773502691895664007, -15.25000000409674250 ) ) ;
#11945 = CARTESIAN_POINT ( 'NONE',  ( 10.81189881249999907, 6.242252689847868297, -46.40625000204836681 ) ) ;
#11946 = CARTESIAN_POINT ( 'NONE',  ( -9.999999999999998224, 1.224646799147353059E-15, -120.1250000040967905 ) ) ;
#11947 = CARTESIAN_POINT ( 'NONE',  ( -10.00000000000000000, -5.773502691896251982, -101.6249999999999858 ) ) ;
#11948 = VERTEX_POINT ( 'NONE', #4107 ) ;
#11949 = CARTESIAN_POINT ( 'NONE',  ( -10.81189881249999729, -6.242252689847864744, -123.6562500020484094 ) ) ;
#11950 = CARTESIAN_POINT ( 'NONE',  ( 7.070501591499377789E-16, 11.54700538379251284, -138.5000000040967905 ) ) ;
#11951 = LINE ( 'NONE', #36842, #9823 ) ;
#11952 = CARTESIAN_POINT ( 'NONE',  ( -10.81189881249999907, -6.242252689847864744, -183.6562500020483810 ) ) ;
#11953 = ORIENTED_EDGE ( 'NONE', *, *, #39430, .T. ) ;
#11954 = CARTESIAN_POINT ( 'NONE',  ( 5.405949406249992428, -9.363379034771808662, -172.5937500020484094 ) ) ;
#11955 = CARTESIAN_POINT ( 'NONE',  ( 10.00000000000000000, 5.773502691896255534, -51.75000000409676204 ) ) ;
#11956 = EDGE_CURVE ( 'NONE', #19459, #36911, #24994, .T. ) ;
#11957 = CARTESIAN_POINT ( 'NONE',  ( -9.999999999999998224, 1.224646799147353059E-15, -155.7500000000000000 ) ) ;
#11958 = CARTESIAN_POINT ( 'NONE',  ( -5.405949406249996869, 9.363379034771805109, -65.53125000204838102 ) ) ;
#11959 = CARTESIAN_POINT ( 'NONE',  ( -2.121150477449813534E-15, -11.54700538379251284, -46.25000000409676204 ) ) ;
#11960 = CARTESIAN_POINT ( 'NONE',  ( -5.000000000000003553, -8.660254037844383745, -148.3750000040967905 ) ) ;
#11961 = CARTESIAN_POINT ( 'NONE',  ( -5.405949406250003975, -9.363379034771801557, -168.5312500020484094 ) ) ;
#11962 = CARTESIAN_POINT ( 'NONE',  ( 7.070501591499376803E-16, 11.54700538379251284, -2.000000004096753159 ) ) ;
#11963 = CARTESIAN_POINT ( 'NONE',  ( 4.999999999999992006, -8.660254037844389075, -34.12500000409676915 ) ) ;
#11964 = ORIENTED_EDGE ( 'NONE', *, *, #38901, .F. ) ;
#11965 = DIRECTION ( 'NONE',  ( 0.000000000000000000, 0.000000000000000000, -1.000000000000000000 ) ) ;
#11966 = DIRECTION ( 'NONE',  ( -1.000000000000000000, 0.000000000000000000, 0.000000000000000000 ) ) ;
#11968 = ORIENTED_EDGE ( 'NONE', *, *, #15619, .T. ) ;
#11967 = CARTESIAN_POINT ( 'NONE',  ( 5.405949406249992428, -9.363379034771808662, -79.78125000204838102 ) ) ;
#11969 = EDGE_CURVE ( 'NONE', #5733, #41318, #36811, .T. ) ;
#11971 = ORIENTED_EDGE ( 'NONE', *, *, #34132, .F. ) ;
#11970 = CARTESIAN_POINT ( 'NONE',  ( 9.999999999999998224, 0.000000000000000000, -188.3750000040967905 ) ) ;
#11972 =( BOUNDED_CURVE ( )  B_SPLINE_CURVE ( 2, ( #28756, #41883, #19019, #35228, #1785, #21626, #5659 ),
 .UNSPECIFIED., .F., .F. ) 
 B_SPLINE_CURVE_WITH_KNOTS ( ( 3, 2, 2, 3 ),
 ( 0.4813432835820896649, 0.4825870646766170502, 0.4838308457711443800, 0.4850746268656717652 ),
 .UNSPECIFIED. ) 
 CURVE ( )  GEOMETRIC_REPRESENTATION_ITEM ( )  RATIONAL_B_SPLINE_CURVE ( ( 0.9999999999999880096, 0.8660254037844506980, 1.000000000000000000, 0.8660254037844387076, 1.000000000000000000, 0.8660254037844267172, 1.000000000000011990 ) ) 
 REPRESENTATION_ITEM ( '' )  );
#11973 = ORIENTED_EDGE ( 'NONE', *, *, #24630, .T. ) ;
#11974 = EDGE_CURVE ( 'NONE', #17462, #21319, #22214, .T. ) ;
#11975 = CARTESIAN_POINT ( 'NONE',  ( -5.405949406249996869, 9.363379034771805109, -30.84375000204836326 ) ) ;
#11976 = CARTESIAN_POINT ( 'NONE',  ( 9.999999999999998224, 1.224646799147353059E-15, -99.99999999999998579 ) ) ;
#11977 = CARTESIAN_POINT ( 'NONE',  ( 10.81189881249999551, -6.242252689847874514, -4.656250002048353487 ) ) ;
#11980 = EDGE_CURVE ( 'NONE', #33268, #8658, #35390, .T. ) ;
#11979 = ORIENTED_EDGE ( 'NONE', *, *, #12507, .F. ) ;
#11978 = CARTESIAN_POINT ( 'NONE',  ( -10.81189881249999729, 6.242252689847871849, -54.71875000204838102 ) ) ;
#11981 = CARTESIAN_POINT ( 'NONE',  ( 9.999999999999998224, 0.000000000000000000, -112.9999999999999858 ) ) ;
#11982 = CARTESIAN_POINT ( 'NONE',  ( -5.000000000000003553, -8.660254037844383745, -33.99999999999997158 ) ) ;
#11983 = CARTESIAN_POINT ( 'NONE',  ( -5.405949406249996869, 9.363379034771805109, -194.3437500020484094 ) ) ;
#11984 = CARTESIAN_POINT ( 'NONE',  ( 10.81189881249999729, 0.000000000000000000, -178.3437500020483810 ) ) ;
#11985 = APPROVAL ( #42375, 'UNSPECIFIED' ) ;
#11986 = CARTESIAN_POINT ( 'NONE',  ( -5.405949406250003975, -9.363379034771801557, -154.8437500020483810 ) ) ;
#11987 = CARTESIAN_POINT ( 'NONE',  ( -10.81189881249999729, -6.242252689847864744, -177.4687500020484094 ) ) ;
#11988 = LINE ( 'NONE', #12404, #19188 ) ;
#11989 = LINE ( 'NONE', #38534, #22609 ) ;
#11990 = CARTESIAN_POINT ( 'NONE',  ( -10.00000000000000000, -5.773502691896251982, -197.6250000000000284 ) ) ;
#11991 = CARTESIAN_POINT ( 'NONE',  ( -5.405949406249996869, 9.363379034771805109, -105.8437500020483810 ) ) ;
#11992 = FACE_OUTER_BOUND ( 'NONE', #35700, .T. ) ;
#11993 = CARTESIAN_POINT ( 'NONE',  ( -10.81189881249999729, 1.324075727343319199E-15, -83.28125000204838102 ) ) ;
#11994 = CARTESIAN_POINT ( 'NONE',  ( -2.293366432827344421E-15, -12.48450537969573659, -90.21875000204838102 ) ) ;
#11995 = CARTESIAN_POINT ( 'NONE',  ( 7.644554776091147741E-16, 12.48450537969573659, -65.65625000204838102 ) ) ;
#11996 = CARTESIAN_POINT ( 'NONE',  ( -9.999999999999998224, 5.773502691896259087, -145.7500000040967905 ) ) ;
#11997 = CARTESIAN_POINT ( 'NONE',  ( 9.999999999999998224, 0.000000000000000000, -125.0000000000000000 ) ) ;
#11998 = EDGE_CURVE ( 'NONE', #17213, #37997, #16361, .T. ) ;
#11999 = VERTEX_POINT ( 'NONE', #38187 ) ;
#12000 = CARTESIAN_POINT ( 'NONE',  ( -5.405949406250003975, -9.363379034771801557, -153.5312500020484094 ) ) ;
#12001 = CARTESIAN_POINT ( 'NONE',  ( -10.81189881249999907, -6.242252689847864744, -164.1562500020484094 ) ) ;
#12002 = CARTESIAN_POINT ( 'NONE',  ( 9.999999999999998224, 0.000000000000000000, -96.49999999999998579 ) ) ;
#12003 = DIRECTION ( 'NONE',  ( -0.000000000000000000, -0.000000000000000000, 1.000000000000000000 ) ) ;
#12004 = CARTESIAN_POINT ( 'NONE',  ( -5.405949406249996869, 9.363379034771805109, -101.3437500020483810 ) ) ;
#12005 = VERTEX_POINT ( 'NONE', #15500 ) ;
#12006 = CARTESIAN_POINT ( 'NONE',  ( -2.121150477449813534E-15, -11.54700538379251284, -63.87499999999999289 ) ) ;
#12007 = CARTESIAN_POINT ( 'NONE',  ( 5.405949406249992428, -9.363379034771808662, -0.2812500020483721386 ) ) ;
#12008 = CARTESIAN_POINT ( 'NONE',  ( -10.00000000000000000, -5.773502691896251982, -72.00000000409674783 ) ) ;
#12009 = CARTESIAN_POINT ( 'NONE',  ( 10.00000000000102318, -5.773502691895667560, -11.50000000409674072 ) ) ;
#12010 = CARTESIAN_POINT ( 'NONE',  ( 10.81189881249999551, -6.242252689847874514, -96.15625000204838102 ) ) ;
#12011 = CARTESIAN_POINT ( 'NONE',  ( 10.81189881249999729, 0.000000000000000000, -76.53125000204838102 ) ) ;
#12012 = CARTESIAN_POINT ( 'NONE',  ( 9.999999999999996447, -5.773502691896262640, -70.00000000409679046 ) ) ;
#12013 = LINE ( 'NONE', #22168, #35576 ) ;
#12014 = CARTESIAN_POINT ( 'NONE',  ( 7.644554776091147741E-16, 12.48450537969573659, -24.96875000204837391 ) ) ;
#12015 = ORIENTED_EDGE ( 'NONE', *, *, #3158, .T. ) ;
#12016 = CARTESIAN_POINT ( 'NONE',  ( 10.81189881249999729, 0.000000000000000000, -195.0312500020484094 ) ) ;
#12017 = CARTESIAN_POINT ( 'NONE',  ( -10.81189881249999729, 1.324075727343319199E-15, -17.28125000204835970 ) ) ;
#12018 = CARTESIAN_POINT ( 'NONE',  ( 5.405949406249999534, 9.363379034771803333, -5.593750002048370362 ) ) ;
#12019 = CARTESIAN_POINT ( 'NONE',  ( 7.070501591499376803E-16, 11.54700538379251284, -137.0000000040967905 ) ) ;
#12020 = CARTESIAN_POINT ( 'NONE',  ( -10.81189881249999907, -6.242252689847864744, -142.9687500020484094 ) ) ;
#12021 = CARTESIAN_POINT ( 'NONE',  ( 10.00000000000000000, 5.773502691896255534, 0.7499999959032500607 ) ) ;
#12022 = CARTESIAN_POINT ( 'NONE',  ( 4.999999999999992006, -8.660254037844389075, -173.2500000000000284 ) ) ;
#12023 =( BOUNDED_CURVE ( )  B_SPLINE_CURVE ( 2, ( #16651, #12986, #15805, #13411, #42562, #42142, #29211 ),
 .UNSPECIFIED., .F., .F. ) 
 B_SPLINE_CURVE_WITH_KNOTS ( ( 3, 2, 2, 3 ),
 ( 0.7089552238805972850, 0.7101990049751245593, 0.7114427860696519446, 0.7126865671641793298 ),
 .UNSPECIFIED. ) 
 CURVE ( )  GEOMETRIC_REPRESENTATION_ITEM ( )  RATIONAL_B_SPLINE_CURVE ( ( 0.9999999999999761302, 0.8660254037844625774, 1.000000000000000000, 0.8660254037844387076, 1.000000000000000000, 0.8660254037844148378, 1.000000000000023981 ) ) 
 REPRESENTATION_ITEM ( '' )  );
#12024 = CARTESIAN_POINT ( 'NONE',  ( 10.00000000000000000, 5.773502691896255534, -175.8750000000000000 ) ) ;
#12025 = DIRECTION ( 'NONE',  ( -0.000000000000000000, -0.000000000000000000, -1.000000000000000000 ) ) ;
#12027 = ORIENTED_EDGE ( 'NONE', *, *, #1670, .F. ) ;
#12026 = CARTESIAN_POINT ( 'NONE',  ( 10.81189881249999907, 6.242252689847868297, -103.4062500020483952 ) ) ;
#12028 = CYLINDRICAL_SURFACE ( 'NONE', #9004, 9.999999999999998224 ) ;
#12029 = VERTEX_POINT ( 'NONE', #21352 ) ;
#12030 = ORIENTED_EDGE ( 'NONE', *, *, #24028, .F. ) ;
#12031 = CARTESIAN_POINT ( 'NONE',  ( -5.405949406250003975, -9.363379034771801557, -29.03125000204837036 ) ) ;
#12032 = SECURITY_CLASSIFICATION_LEVEL ( 'unclassified' ) ;
#12033 = CARTESIAN_POINT ( 'NONE',  ( -10.81189881249999907, -6.242252689847864744, -78.46875000204838102 ) ) ;
#12034 = CARTESIAN_POINT ( 'NONE',  ( -4.999999999999996447, 8.660254037844387298, -127.8750000040967905 ) ) ;
#12035 = CARTESIAN_POINT ( 'NONE',  ( -9.999999999999998224, 1.224646799147353059E-15, -180.1250000040968189 ) ) ;
#12036 = CARTESIAN_POINT ( 'NONE',  ( 0.000000000000000000, 0.000000000000000000, -200.0000000000000000 ) ) ;
#12037 = CARTESIAN_POINT ( 'NONE',  ( -5.405949406249996869, 9.363379034771805109, -166.0312500020484094 ) ) ;
#12038 = CARTESIAN_POINT ( 'NONE',  ( -2.121150477449813534E-15, -11.54700538379251284, -10.25000000409676026 ) ) ;
#12039 = DIRECTION ( 'NONE',  ( 0.000000000000000000, 1.000000000000000000, 0.000000000000000000 ) ) ;
#12040 = EDGE_CURVE ( 'NONE', #42590, #25379, #18109, .T. ) ;
#12041 = CARTESIAN_POINT ( 'NONE',  ( 10.81189881249999729, 6.242252689847867408, -118.2187500020483810 ) ) ;
#12042 = CARTESIAN_POINT ( 'NONE',  ( -5.405949406250003975, -9.363379034771801557, -88.84375000204838102 ) ) ;
#12043 = CARTESIAN_POINT ( 'NONE',  ( 5.405949406249999534, 9.363379034771803333, -196.0937500020484094 ) ) ;
#12044 = CARTESIAN_POINT ( 'NONE',  ( -5.405949406250003975, -9.363379034771801557, -90.53125000204838102 ) ) ;
#12045 = CARTESIAN_POINT ( 'NONE',  ( 10.00000000000000000, 5.773502691896255534, -167.2500000040968189 ) ) ;
#12046 = CARTESIAN_POINT ( 'NONE',  ( -10.81189881249999729, 6.242252689847871849, -171.9062500020484094 ) ) ;
#12047 = CARTESIAN_POINT ( 'NONE',  ( -9.999999999999479527, -5.773502691896549521, -151.1250000000000000 ) ) ;
#12048 = CARTESIAN_POINT ( 'NONE',  ( 7.644554776091147741E-16, 12.48450537969573659, -172.1562500020484094 ) ) ;
#12049 = CARTESIAN_POINT ( 'NONE',  ( 10.81189881249999551, -6.242252689847874514, -186.1562500020484379 ) ) ;
#12050 = CARTESIAN_POINT ( 'NONE',  ( -5.405949406250003975, -9.363379034771801557, -42.34375000204837391 ) ) ;
#12051 = CARTESIAN_POINT ( 'NONE',  ( 5.000000000000000000, 8.660254037844385522, -167.1250000040967905 ) ) ;
#12052 = CARTESIAN_POINT ( 'NONE',  ( 10.81189881249999729, 0.000000000000000000, -1.531250002048373249 ) ) ;
#12053 = CARTESIAN_POINT ( 'NONE',  ( -2.293366432827344421E-15, -12.48450537969573659, -12.21875000204836148 ) ) ;
#12054 = CARTESIAN_POINT ( 'NONE',  ( 9.999999999999998224, 0.000000000000000000, -158.3750000040967905 ) ) ;
#12055 = CARTESIAN_POINT ( 'NONE',  ( -10.81189881249999907, -6.242252689847864744, -123.4687500020483810 ) ) ;
#12056 = CARTESIAN_POINT ( 'NONE',  ( 7.070501591499377789E-16, 11.54700538379251284, -93.12500000000000000 ) ) ;
#12057 = CARTESIAN_POINT ( 'NONE',  ( -5.405949406250003975, -9.363379034771801557, -24.53125000204836681 ) ) ;
#12058 = CARTESIAN_POINT ( 'NONE',  ( -4.999999999999996447, 8.660254037844387298, -105.3750000040967763 ) ) ;
#12059 = DIRECTION ( 'NONE',  ( -0.000000000000000000, -0.000000000000000000, -1.000000000000000000 ) ) ;
#12060 = CARTESIAN_POINT ( 'NONE',  ( -10.81189881249999907, -6.242252689847864744, -117.6562500020483952 ) ) ;
#12061 = CARTESIAN_POINT ( 'NONE',  ( 5.405949406249999534, 9.363379034771803333, -100.2812500020483952 ) ) ;
#12062 = ADVANCED_FACE ( 'NONE', ( #31304 ), #25466, .T. ) ;
#12063 = ORIENTED_EDGE ( 'NONE', *, *, #7526, .F. ) ;
#12064 = AXIS2_PLACEMENT_3D ( 'NONE', #13530, #33423, #20654 ) ;
#12065 = CARTESIAN_POINT ( 'NONE',  ( -4.999999999999996447, 8.660254037844387298, -88.87500000409677625 ) ) ;
#12066 = CARTESIAN_POINT ( 'NONE',  ( 45.00000000000000711, 5.510910596163090344E-15, -203.0000000000000000 ) ) ;
#12067 = CARTESIAN_POINT ( 'NONE',  ( 10.81189881249999551, -6.242252689847874514, -156.1562500020484094 ) ) ;
#12068 = CARTESIAN_POINT ( 'NONE',  ( -10.81189881249999907, -6.242252689847864744, -49.96875000204837391 ) ) ;
#12069 = EDGE_LOOP ( 'NONE', ( #40888, #39155, #10799, #30781 ) ) ;
#12070 = CARTESIAN_POINT ( 'NONE',  ( 7.070501591499377789E-16, 11.54700538379251284, -15.12499999999997691 ) ) ;
#12071 = CARTESIAN_POINT ( 'NONE',  ( 10.81189881249999551, -6.242252689847874514, -30.15625000204836326 ) ) ;
#12072 = CARTESIAN_POINT ( 'NONE',  ( -9.999999999999998224, 5.773502691896259087, -155.8749999999999716 ) ) ;
#12073 = CARTESIAN_POINT ( 'NONE',  ( -9.999999999999998224, 1.224646799147353059E-15, -18.12500000409675138 ) ) ;
#12074 = CARTESIAN_POINT ( 'NONE',  ( -5.000000000000003553, -8.660254037844383745, -196.0000000000000000 ) ) ;
#12076 = ORIENTED_EDGE ( 'NONE', *, *, #9301, .F. ) ;
#12075 = CARTESIAN_POINT ( 'NONE',  ( -10.81189881249999729, 1.324075727343319199E-15, -123.7812500020483952 ) ) ;
#12077 = CARTESIAN_POINT ( 'NONE',  ( 4.999999999999992006, -8.660254037844389075, -21.74999999999996447 ) ) ;
#12078 = CARTESIAN_POINT ( 'NONE',  ( 9.999999999999998224, 1.224646799147353059E-15, -99.99999999999998579 ) ) ;
#12079 = VECTOR ( 'NONE', #28965, 1000.000000000000000 ) ;
#12080 = ORIENTED_EDGE ( 'NONE', *, *, #34162, .T. ) ;
#12081 = CARTESIAN_POINT ( 'NONE',  ( -10.81189881249999907, -6.242252689847864744, -54.65625000204838102 ) ) ;
#12082 = COORDINATED_UNIVERSAL_TIME_OFFSET ( 6, 0, .AHEAD. ) ;
#12083 = CARTESIAN_POINT ( 'NONE',  ( -10.81189881249999729, 1.324075727343319199E-15, -113.0937500020483810 ) ) ;
#12085 = ORIENTED_EDGE ( 'NONE', *, *, #26407, .T. ) ;
#12084 = ORIENTED_EDGE ( 'NONE', *, *, #8000, .T. ) ;
#12086 = CIRCLE ( 'NONE', #29349, 15.00000000000001066 ) ;
#12087 = DIRECTION ( 'NONE',  ( -0.000000000000000000, -0.000000000000000000, -1.000000000000000000 ) ) ;
#12088 = LINE ( 'NONE', #1977, #820 ) ;
#12090 = ADVANCED_FACE ( 'NONE', ( #1736 ), #5814, .T. ) ;
#12089 = CARTESIAN_POINT ( 'NONE',  ( 7.644554776091147741E-16, 12.48450537969573659, -153.9687500020484094 ) ) ;
#12091 = CARTESIAN_POINT ( 'NONE',  ( 10.81189881249999729, 0.000000000000000000, -192.0312500020484094 ) ) ;
#12092 = CARTESIAN_POINT ( 'NONE',  ( -5.405949406249996869, 9.363379034771805109, -5.343750002048369474 ) ) ;
#12093 = CARTESIAN_POINT ( 'NONE',  ( -5.405949406249996869, 9.363379034771805109, -138.8437500020484094 ) ) ;
#12094 = CARTESIAN_POINT ( 'NONE',  ( 10.81189881249999551, -6.242252689847874514, -110.9687500020483810 ) ) ;
#12095 = CARTESIAN_POINT ( 'NONE',  ( 5.000000000000000000, 8.660254037844385522, -187.7500000000000000 ) ) ;
#12096 = CARTESIAN_POINT ( 'NONE',  ( -10.81189881249999907, -6.242252689847864744, -114.6562500020483952 ) ) ;
#12097 = CARTESIAN_POINT ( 'NONE',  ( 10.81189881249999907, 6.242252689847868297, -2.718750002048360592 ) ) ;
#12098 = CARTESIAN_POINT ( 'NONE',  ( -2.293366432827344421E-15, -12.48450537969573659, -126.2187500020483952 ) ) ;
#12099 = CARTESIAN_POINT ( 'NONE',  ( 7.644554776091147741E-16, 12.48450537969573659, -196.1562500020484094 ) ) ;
#12100 = CARTESIAN_POINT ( 'NONE',  ( -4.999999999999996447, 8.660254037844387298, -144.0000000000000000 ) ) ;
#12101 = CARTESIAN_POINT ( 'NONE',  ( -9.999999999999998224, 1.224646799147353059E-15, -8.749999999999952038 ) ) ;
#12102 = CARTESIAN_POINT ( 'NONE',  ( -5.405949406249996869, 9.363379034771805109, -68.34375000204836681 ) ) ;
#12103 = CARTESIAN_POINT ( 'NONE',  ( -2.293366432827344421E-15, -12.48450537969573659, -57.21875000204835970 ) ) ;
#12104 = CARTESIAN_POINT ( 'NONE',  ( -4.999999999999996447, 8.660254037844387298, -190.8750000040967905 ) ) ;
#12105 = CARTESIAN_POINT ( 'NONE',  ( -10.81189881249999729, 6.242252689847871849, -29.40625000204835615 ) ) ;
#12106 = CARTESIAN_POINT ( 'NONE',  ( 5.405949406249992428, -9.363379034771808662, -40.59375000204837391 ) ) ;
#12107 = CARTESIAN_POINT ( 'NONE',  ( -9.999999999999998224, 1.224646799147353059E-15, -136.2499999999999716 ) ) ;
#12108 = CARTESIAN_POINT ( 'NONE',  ( 10.81189881249999907, 6.242252689847868297, -142.2187500020484094 ) ) ;
#12109 = CARTESIAN_POINT ( 'NONE',  ( -2.121150477449813534E-15, -11.54700538379251284, -116.3749999999999858 ) ) ;
#12110 = ADVANCED_FACE ( 'NONE', ( #8631 ), #28493, .F. ) ;
#12111 = CARTESIAN_POINT ( 'NONE',  ( 9.999999999999998224, 0.000000000000000000, -200.0000000000000000 ) ) ;
#12112 = VECTOR ( 'NONE', #9547, 1000.000000000000000 ) ;
#12113 = CARTESIAN_POINT ( 'NONE',  ( 4.999999999999992006, -8.660254037844389075, -78.74999999999998579 ) ) ;
#12114 = CARTESIAN_POINT ( 'NONE',  ( 10.81189881249999907, 6.242252689847868297, -140.9062500020484094 ) ) ;
#12115 = CARTESIAN_POINT ( 'NONE',  ( 5.405949406249999534, 9.363379034771803333, -8.781250002048352599 ) ) ;
#12116 = EDGE_LOOP ( 'NONE', ( #15883, #7410, #35250, #37009 ) ) ;
#12117 = AXIS2_PLACEMENT_3D ( 'NONE', #3175, #13911, #159 ) ;
#12118 = LINE ( 'NONE', #38670, #17578 ) ;
#12119 = CARTESIAN_POINT ( 'NONE',  ( 7.070501591499377789E-16, 11.54700538379251284, -116.0000000040967763 ) ) ;
#12120 = CARTESIAN_POINT ( 'NONE',  ( -9.999999999999998224, 1.224646799147353059E-15, -128.7499999999999716 ) ) ;
#12121 = CARTESIAN_POINT ( 'NONE',  ( 5.405949406249992428, -9.363379034771808662, -76.59375000204838102 ) ) ;
#12122 = CARTESIAN_POINT ( 'NONE',  ( -5.000000000000003553, -8.660254037844383745, -44.49999999999998579 ) ) ;
#12123 = CARTESIAN_POINT ( 'NONE',  ( -9.999999999999998224, 5.773502691896259087, -22.75000000409677270 ) ) ;
#12124 = VECTOR ( 'NONE', #20301, 1000.000000000000000 ) ;
#12125 = CARTESIAN_POINT ( 'NONE',  ( 4.999999999999992006, -8.660254037844389075, -141.7500000000000000 ) ) ;
#12126 = CARTESIAN_POINT ( 'NONE',  ( 5.405949406249992428, -9.363379034771808662, -37.78125000204838102 ) ) ;
#12127 = FACE_OUTER_BOUND ( 'NONE', #34129, .T. ) ;
#12128 = CARTESIAN_POINT ( 'NONE',  ( -10.81189881249999729, 1.324075727343319199E-15, -147.7812500020483810 ) ) ;
#12129 = CARTESIAN_POINT ( 'NONE',  ( 10.81189881249999729, 0.000000000000000000, -150.0312500020483810 ) ) ;
#12130 = CARTESIAN_POINT ( 'NONE',  ( 9.999999999999998224, 0.000000000000000000, -51.49999999999996447 ) ) ;
#12131 = FACE_OUTER_BOUND ( 'NONE', #31522, .T. ) ;
#12132 = ORIENTED_EDGE ( 'NONE', *, *, #22674, .T. ) ;
#12133 = EDGE_LOOP ( 'NONE', ( #33495, #8860, #16467, #13801 ) ) ;
#12134 = ORIENTED_EDGE ( 'NONE', *, *, #19400, .F. ) ;
#12135 = CARTESIAN_POINT ( 'NONE',  ( 10.00000000000205347, -5.773502691895071592, -7.000000004096692763 ) ) ;
#12136 = CARTESIAN_POINT ( 'NONE',  ( 5.405949406249999534, 9.363379034771803333, -178.0937500020484094 ) ) ;
#12137 = CARTESIAN_POINT ( 'NONE',  ( 10.81189881249999551, -6.242252689847874514, -28.46875000204837036 ) ) ;
#12138 = CARTESIAN_POINT ( 'NONE',  ( 9.999999999999998224, 0.000000000000000000, -110.3750000040967763 ) ) ;
#12139 = CARTESIAN_POINT ( 'NONE',  ( 7.644554776091147741E-16, 12.48450537969573659, -167.4687500020483526 ) ) ;
#12140 = CARTESIAN_POINT ( 'NONE',  ( -10.81189881249999907, -6.242252689847864744, -156.4687500020484379 ) ) ;
#12141 = DIRECTION ( 'NONE',  ( -0.000000000000000000, -0.000000000000000000, 1.000000000000000000 ) ) ;
#12142 = CARTESIAN_POINT ( 'NONE',  ( 10.81189881249999551, -6.242252689847874514, -130.4687500020483810 ) ) ;
#12143 = CARTESIAN_POINT ( 'NONE',  ( -5.405949406250003975, -9.363379034771801557, -137.0312500020484094 ) ) ;
#12144 = CARTESIAN_POINT ( 'NONE',  ( 5.405949406249999534, 9.363379034771803333, -146.5937500020483810 ) ) ;
#12145 =( BOUNDED_CURVE ( )  B_SPLINE_CURVE ( 2, ( #33826, #6849, #20855, #16969, #17181, #30379, #811 ),
 .UNSPECIFIED., .F., .F. ) 
 B_SPLINE_CURVE_WITH_KNOTS ( ( 3, 2, 2, 3 ),
 ( 0.4477611940298508730, 0.4490049751243782028, 0.4502487562189055881, 0.4514925373134329734 ),
 .UNSPECIFIED. ) 
 CURVE ( )  GEOMETRIC_REPRESENTATION_ITEM ( )  RATIONAL_B_SPLINE_CURVE ( ( 0.9999999999999880096, 0.8660254037844506980, 1.000000000000000000, 0.8660254037844387076, 1.000000000000000000, 0.8660254037844267172, 1.000000000000011990 ) ) 
 REPRESENTATION_ITEM ( '' )  );
#12146 = CARTESIAN_POINT ( 'NONE',  ( -9.999999999999998224, 1.224646799147353059E-15, -70.24999999999998579 ) ) ;
#12147 = CARTESIAN_POINT ( 'NONE',  ( -9.999999999999998224, 5.773502691896259087, -173.8749999999999716 ) ) ;
#12148 = CARTESIAN_POINT ( 'NONE',  ( 10.81189881249999729, 0.000000000000000000, -77.84375000204838102 ) ) ;
#12149 = CARTESIAN_POINT ( 'NONE',  ( -0.06394991864857380026, 10.83468475260746544, -100.0000000000000142 ) ) ;
#12150 = CARTESIAN_POINT ( 'NONE',  ( 5.405949406249999534, 9.363379034771803333, -50.78125000204835970 ) ) ;
#12151 = CARTESIAN_POINT ( 'NONE',  ( -2.121150477449813534E-15, -11.54700538379251284, -149.3750000000000000 ) ) ;
#12152 = CARTESIAN_POINT ( 'NONE',  ( 10.81189881249999729, 0.000000000000000000, -166.3437500020484094 ) ) ;
#12153 = CARTESIAN_POINT ( 'NONE',  ( 10.00000000000000000, 5.773502691896255534, -133.8750000000000000 ) ) ;
#12154 = CARTESIAN_POINT ( 'NONE',  ( -10.81189881249999729, 1.324075727343319199E-15, -149.2812500020483810 ) ) ;
#12155 = CARTESIAN_POINT ( 'NONE',  ( -2.121150477449813534E-15, -11.54700538379251284, -29.37499999999994671 ) ) ;
#12156 = CARTESIAN_POINT ( 'NONE',  ( -10.81189881249999729, 1.324075727343319199E-15, -39.78125000204838102 ) ) ;
#12157 = CARTESIAN_POINT ( 'NONE',  ( 5.000000000000000000, 8.660254037844385522, -122.1250000040967905 ) ) ;
#12158 = CARTESIAN_POINT ( 'NONE',  ( 10.00000000000000000, 5.773502691896255534, -100.8750000000000000 ) ) ;
#12159 = VERTEX_POINT ( 'NONE', #11625 ) ;
#12160 =( BOUNDED_CURVE ( )  B_SPLINE_CURVE ( 2, ( #18875, #2691, #31850, #35505, #25363, #18226, #35078 ),
 .UNSPECIFIED., .F., .F. ) 
 B_SPLINE_CURVE_WITH_KNOTS ( ( 3, 2, 2, 3 ),
 ( 0.1828358208955224162, 0.1840796019900497738, 0.1853233830845771313, 0.1865671641791045166 ),
 .UNSPECIFIED. ) 
 CURVE ( )  GEOMETRIC_REPRESENTATION_ITEM ( )  RATIONAL_B_SPLINE_CURVE ( ( 0.9999999999999970024, 0.8660254037844417052, 1.000000000000000000, 0.8660254037844387076, 1.000000000000000000, 0.8660254037844357100, 1.000000000000002887 ) ) 
 REPRESENTATION_ITEM ( '' )  );
#12161 = CARTESIAN_POINT ( 'NONE',  ( -5.405949406249996869, 9.363379034771805109, -116.5312500020483952 ) ) ;
#12162 = CARTESIAN_POINT ( 'NONE',  ( 9.999999999999998224, 0.000000000000000000, -140.3750000040967905 ) ) ;
#12163 = CARTESIAN_POINT ( 'NONE',  ( 7.070501591499376803E-16, 11.54700538379251284, -159.1250000000000284 ) ) ;
#12164 = CARTESIAN_POINT ( 'NONE',  ( -5.405949406250003975, -9.363379034771801557, -182.0312500020483810 ) ) ;
#12165 = CARTESIAN_POINT ( 'NONE',  ( -4.999999999999996447, 8.660254037844387298, -46.87500000409677625 ) ) ;
#12166 = EDGE_CURVE ( 'NONE', #26513, #32487, #31285, .T. ) ;
#12167 = CARTESIAN_POINT ( 'NONE',  ( 9.999999999999998224, 0.000000000000000000, -174.8750000040967905 ) ) ;
#12168 = EDGE_CURVE ( 'NONE', #11337, #15716, #10329, .T. ) ;
#12169 = CARTESIAN_POINT ( 'NONE',  ( -10.81189881249999729, 6.242252689847871849, -69.90625000204839523 ) ) ;
#12170 = CARTESIAN_POINT ( 'NONE',  ( 9.999999999999998224, 0.000000000000000000, -23.37500000409675849 ) ) ;
#12171 = CARTESIAN_POINT ( 'NONE',  ( -10.81189881249999729, 6.242252689847871849, -168.9062500020483810 ) ) ;
#12172 = CARTESIAN_POINT ( 'NONE',  ( 0.000000000000000000, 0.000000000000000000, -200.0000000000000000 ) ) ;
#12173 = CYLINDRICAL_SURFACE ( 'NONE', #15106, 9.999999999999998224 ) ;
#12174 = VERTEX_POINT ( 'NONE', #41410 ) ;
#12175 = CARTESIAN_POINT ( 'NONE',  ( 0.000000000000000000, 0.000000000000000000, -200.0000000000000000 ) ) ;
#12176 = CARTESIAN_POINT ( 'NONE',  ( 9.999999999999998224, 0.000000000000000000, -123.8750000040967905 ) ) ;
#12177 = CARTESIAN_POINT ( 'NONE',  ( -5.000000000000003553, -8.660254037844383745, -71.49999999999998579 ) ) ;
#12179 = ORIENTED_EDGE ( 'NONE', *, *, #21511, .F. ) ;
#12178 = CARTESIAN_POINT ( 'NONE',  ( 5.405949406249999534, 9.363379034771803333, -74.78125000204838102 ) ) ;
#12180 = DIRECTION ( 'NONE',  ( 1.000000000000000000, 0.000000000000000000, 0.000000000000000000 ) ) ;
#12182 = VERTEX_POINT ( 'NONE', #25045 ) ;
#12181 = CARTESIAN_POINT ( 'NONE',  ( 10.00000000000025402, -5.773502691896113426, -140.1250000000000000 ) ) ;
#12183 = EDGE_LOOP ( 'NONE', ( #16198, #17481, #11421, #28012 ) ) ;
#12184 = CARTESIAN_POINT ( 'NONE',  ( -10.81189881249999729, -6.242252689847864744, -31.96875000204835970 ) ) ;
#12185 = CARTESIAN_POINT ( 'NONE',  ( -9.999999999998969713, -5.773502691896847949, -53.62499999999995737 ) ) ;
#12186 = CARTESIAN_POINT ( 'NONE',  ( 10.81189881249999907, 6.242252689847868297, -2.906250002048345937 ) ) ;
#12188 = ORIENTED_EDGE ( 'NONE', *, *, #11814, .F. ) ;
#12187 = CARTESIAN_POINT ( 'NONE',  ( -10.81189881249999729, 1.324075727343319199E-15, -59.09375000204835970 ) ) ;
#12189 = LINE ( 'NONE', #2083, #34636 ) ;
#12190 = CARTESIAN_POINT ( 'NONE',  ( 9.999999999999998224, 0.000000000000000000, -33.49999999999997158 ) ) ;
#12191 = CARTESIAN_POINT ( 'NONE',  ( 10.81189881249999729, 6.242252689847867408, -190.2187500020484094 ) ) ;
#12192 = CARTESIAN_POINT ( 'NONE',  ( -5.405949406249996869, 9.363379034771805109, -176.3437500020483810 ) ) ;
#12193 = CARTESIAN_POINT ( 'NONE',  ( 10.81189881249999907, 6.242252689847868297, -158.7187500020483810 ) ) ;
#12194 = CARTESIAN_POINT ( 'NONE',  ( -10.81189881249999729, 1.324075727343319199E-15, -170.0937500020484094 ) ) ;
#12195 = LINE ( 'NONE', #28419, #30896 ) ;
#12196 = CARTESIAN_POINT ( 'NONE',  ( -9.999999999999998224, 1.224646799147353059E-15, -102.1250000040967905 ) ) ;
#12197 = CARTESIAN_POINT ( 'NONE',  ( -9.999999999999998224, 1.224646799147353059E-15, -199.2500000000000000 ) ) ;
#12198 = CARTESIAN_POINT ( 'NONE',  ( -5.405949406250003975, -9.363379034771801557, -102.3437500020483810 ) ) ;
#12199 = CARTESIAN_POINT ( 'NONE',  ( 4.999999999999992006, -8.660254037844389075, -84.74999999999997158 ) ) ;
#12200 = CARTESIAN_POINT ( 'NONE',  ( -2.293366432827344421E-15, -12.48450537969573659, -75.40625000204838102 ) ) ;
#12201 = CARTESIAN_POINT ( 'NONE',  ( -10.81189881249999729, 6.242252689847871849, -92.21875000204839523 ) ) ;
#12202 = CARTESIAN_POINT ( 'NONE',  ( -10.81189881249999907, -6.242252689847864744, -63.65625000204838102 ) ) ;
#12203 = CARTESIAN_POINT ( 'NONE',  ( -10.00000000000000000, -5.773502691896251982, -150.0000000040967905 ) ) ;
#12204 = CARTESIAN_POINT ( 'NONE',  ( -2.121150477449813534E-15, -11.54700538379251284, -120.8749999999999858 ) ) ;
#12205 = ORIENTED_EDGE ( 'NONE', *, *, #24444, .T. ) ;
#12206 = CARTESIAN_POINT ( 'NONE',  ( -10.81189881249999729, 1.324075727343319199E-15, -149.2812500020483810 ) ) ;
#12207 = CARTESIAN_POINT ( 'NONE',  ( -10.81189881249999729, 6.242252689847871849, -161.4062500020483810 ) ) ;
#12208 = CARTESIAN_POINT ( 'NONE',  ( 0.000000000000000000, 0.000000000000000000, -200.0000000000000000 ) ) ;
#12209 = CARTESIAN_POINT ( 'NONE',  ( -2.121150477449813534E-15, -11.54700538379251284, -38.37499999999995737 ) ) ;
#12210 = CARTESIAN_POINT ( 'NONE',  ( -5.405949406250003975, -9.363379034771801557, -99.34375000204838102 ) ) ;
#12211 = ORIENTED_EDGE ( 'NONE', *, *, #37433, .F. ) ;
#12212 = CARTESIAN_POINT ( 'NONE',  ( 4.999999999999992006, -8.660254037844389075, -62.24999999999997158 ) ) ;
#12213 = CARTESIAN_POINT ( 'NONE',  ( -5.405949406250003975, -9.363379034771801557, -195.3437500020484094 ) ) ;
#12214 = CARTESIAN_POINT ( 'NONE',  ( 10.00000000000000000, 5.773502691896255534, -72.75000000409674783 ) ) ;
#12215 = EDGE_CURVE ( 'NONE', #740, #35303, #32992, .T. ) ;
#12216 = CARTESIAN_POINT ( 'NONE',  ( -9.999999999999998224, 1.224646799147353059E-15, -151.2500000000000000 ) ) ;
#12217 = CARTESIAN_POINT ( 'NONE',  ( 10.00000000000051159, -5.773502691895965988, -144.6250000000000000 ) ) ;
#12218 = CARTESIAN_POINT ( 'NONE',  ( -10.81189881249999907, -6.242252689847864744, -89.15625000204839523 ) ) ;
#12219 = CARTESIAN_POINT ( 'NONE',  ( -5.405949406249996869, 9.363379034771805109, -70.03125000204838102 ) ) ;
#12220 = EDGE_CURVE ( 'NONE', #40396, #5733, #31033, .T. ) ;
#12221 = CARTESIAN_POINT ( 'NONE',  ( -5.000000000000003553, -8.660254037844383745, -68.87500000409677625 ) ) ;
#12222 = CARTESIAN_POINT ( 'NONE',  ( -9.999999999999998224, 1.224646799147353059E-15, -26.74999999999996803 ) ) ;
#12223 = CARTESIAN_POINT ( 'NONE',  ( -10.81189881249999729, 6.242252689847871849, -24.71875000204837391 ) ) ;
#12224 = DIRECTION ( 'NONE',  ( 1.000000000000000000, 0.000000000000000000, 0.000000000000000000 ) ) ;
#12225 = CARTESIAN_POINT ( 'NONE',  ( -10.81189881249999907, -6.242252689847864744, -195.6562500020484094 ) ) ;
#12226 = CARTESIAN_POINT ( 'NONE',  ( 10.81189881249999729, 0.000000000000000000, -24.03125000204836681 ) ) ;
#12227 = CARTESIAN_POINT ( 'NONE',  ( 10.81189881249999551, -6.242252689847874514, -4.468750002048368586 ) ) ;
#12228 = LINE ( 'NONE', #26050, #34496 ) ;
#12229 =( BOUNDED_CURVE ( )  B_SPLINE_CURVE ( 2, ( #20577, #7214, #11502, #30537, #20366, #17542, #33766 ),
 .UNSPECIFIED., .F., .F. ) 
 B_SPLINE_CURVE_WITH_KNOTS ( ( 3, 2, 2, 3 ),
 ( 0.8134328358208956500, 0.8146766169154230353, 0.8159203980099504205, 0.8171641791044778058 ),
 .UNSPECIFIED. ) 
 CURVE ( )  GEOMETRIC_REPRESENTATION_ITEM ( )  RATIONAL_B_SPLINE_CURVE ( ( 0.9999999999999880096, 0.8660254037844506980, 1.000000000000000000, 0.8660254037844387076, 1.000000000000000000, 0.8660254037844148378, 1.000000000000023981 ) ) 
 REPRESENTATION_ITEM ( '' )  );
#12230 = CARTESIAN_POINT ( 'NONE',  ( -5.000000000000003553, -8.660254037844383745, -181.0000000000000000 ) ) ;
#12231 = APPROVAL ( #42069, 'UNSPECIFIED' ) ;
#12232 = CARTESIAN_POINT ( 'NONE',  ( -10.00000000000025580, 5.773502691896109873, -159.2500000040968189 ) ) ;
#12233 = CARTESIAN_POINT ( 'NONE',  ( -4.999999999999996447, 8.660254037844387298, -174.0000000000000284 ) ) ;
#12235 = ORIENTED_EDGE ( 'NONE', *, *, #2805, .F. ) ;
#12234 = CARTESIAN_POINT ( 'NONE',  ( 10.81189881249999551, -6.242252689847874514, -102.1562500020483952 ) ) ;
#12236 = CARTESIAN_POINT ( 'NONE',  ( -9.999999999999998224, 1.224646799147353059E-15, -155.7500000000000000 ) ) ;
#12237 = ORIENTED_EDGE ( 'NONE', *, *, #9328, .T. ) ;
#12238 = ORIENTED_EDGE ( 'NONE', *, *, #17223, .F. ) ;
#12239 = CARTESIAN_POINT ( 'NONE',  ( 10.81189881249999551, -6.242252689847874514, -30.15625000204836326 ) ) ;
#12240 = APPROVAL_DATE_TIME ( #41805, #30950 ) ;
#12241 = EDGE_CURVE ( 'NONE', #2493, #27376, #26304, .T. ) ;
#12242 = CARTESIAN_POINT ( 'NONE',  ( 5.405949406249992428, -9.363379034771808662, -81.09375000204838102 ) ) ;
#12243 = DIRECTION ( 'NONE',  ( -1.000000000000000000, 0.000000000000000000, 0.000000000000000000 ) ) ;
#12244 = AXIS2_PLACEMENT_3D ( 'NONE', #7807, #14239, #14462 ) ;
#12245 = VECTOR ( 'NONE', #13395, 1000.000000000000000 ) ;
#12246 = CARTESIAN_POINT ( 'NONE',  ( 10.81189881249999551, -6.242252689847874514, -197.9687500020484094 ) ) ;
#12247 = CARTESIAN_POINT ( 'NONE',  ( 10.00000000000051159, -5.773502691895965988, -127.0000000040967763 ) ) ;
#12248 = DIRECTION ( 'NONE',  ( -0.000000000000000000, -0.000000000000000000, 1.000000000000000000 ) ) ;
#12249 = CARTESIAN_POINT ( 'NONE',  ( 10.81189881249999907, 6.242252689847868297, -152.9062500020483810 ) ) ;
#12250 = CARTESIAN_POINT ( 'NONE',  ( 9.999999999999996447, -5.773502691896262640, -10.00000000409676026 ) ) ;
#12251 = FACE_OUTER_BOUND ( 'NONE', #12069, .T. ) ;
#12252 = CARTESIAN_POINT ( 'NONE',  ( -10.81189881249999729, 6.242252689847871849, -129.7187500020483810 ) ) ;
#12253 = CARTESIAN_POINT ( 'NONE',  ( -10.81189881249999729, -6.242252689847864744, -114.4687500020483810 ) ) ;
#12254 = CARTESIAN_POINT ( 'NONE',  ( -5.405949406250003975, -9.363379034771801557, -82.84375000204836681 ) ) ;
#12255 = CARTESIAN_POINT ( 'NONE',  ( -10.81189881249999729, 6.242252689847871849, -89.40625000204838102 ) ) ;
#12256 = CARTESIAN_POINT ( 'NONE',  ( -10.00000000000000000, -5.773502691896251982, -174.0000000040967905 ) ) ;
#12257 = CARTESIAN_POINT ( 'NONE',  ( 10.81189881249999729, 6.242252689847867408, -167.9062500020484094 ) ) ;
#12258 = CARTESIAN_POINT ( 'NONE',  ( 10.81189881249999729, 6.242252689847867408, -178.4062500020484094 ) ) ;
#12259 = CARTESIAN_POINT ( 'NONE',  ( -10.81189881249999729, 1.324075727343319199E-15, -186.7812500020484094 ) ) ;
#12260 = CARTESIAN_POINT ( 'NONE',  ( -5.405949406249996869, 9.363379034771805109, -42.84375000204837391 ) ) ;
#12261 = CARTESIAN_POINT ( 'NONE',  ( 4.999999999999992006, -8.660254037844389075, -167.6250000040967905 ) ) ;
#12262 = CARTESIAN_POINT ( 'NONE',  ( 5.405949406249999534, 9.363379034771803333, -2.781250002048374359 ) ) ;
#12263 = CARTESIAN_POINT ( 'NONE',  ( -10.81189881249999729, 1.324075727343319199E-15, -14.09375000204834905 ) ) ;
#12264 = CARTESIAN_POINT ( 'NONE',  ( 5.000000000000000000, 8.660254037844385522, -162.6250000040967905 ) ) ;
#12265 = CARTESIAN_POINT ( 'NONE',  ( -10.81189881249999729, 6.242252689847871849, -119.2187500020483810 ) ) ;
#12266 = CARTESIAN_POINT ( 'NONE',  ( -9.999999999999998224, 5.773502691896259087, -91.37499999999998579 ) ) ;
#12267 = CARTESIAN_POINT ( 'NONE',  ( -2.293366432827344421E-15, -12.48450537969573659, -16.90625000204837391 ) ) ;
#12268 = CARTESIAN_POINT ( 'NONE',  ( -4.999999999999996447, 8.660254037844387298, -100.8750000040967905 ) ) ;
#12269 = CARTESIAN_POINT ( 'NONE',  ( 9.999999999999998224, 1.224646799147353059E-15, -99.99999999999998579 ) ) ;
#12270 = CARTESIAN_POINT ( 'NONE',  ( -10.81189881249999907, -6.242252689847864744, -113.1562500020483952 ) ) ;
#12271 = CARTESIAN_POINT ( 'NONE',  ( 10.81189881249999729, 6.242252689847867408, -92.90625000204839523 ) ) ;
#12272 = VERTEX_POINT ( 'NONE', #38824 ) ;
#12273 =( BOUNDED_CURVE ( )  B_SPLINE_CURVE ( 2, ( #35743, #33138, #35941, #19739, #15851, #36361, #16063 ),
 .UNSPECIFIED., .F., .F. ) 
 B_SPLINE_CURVE_WITH_KNOTS ( ( 3, 2, 2, 3 ),
 ( 0.1977611940298507898, 0.1990049751243781750, 0.2002487562189055326, 0.2014925373134328901 ),
 .UNSPECIFIED. ) 
 CURVE ( )  GEOMETRIC_REPRESENTATION_ITEM ( )  RATIONAL_B_SPLINE_CURVE ( ( 0.9999999999999940048, 0.8660254037844447028, 1.000000000000000000, 0.8660254037844387076, 1.000000000000000000, 0.8660254037844327124, 1.000000000000005995 ) ) 
 REPRESENTATION_ITEM ( '' )  );
#12274 = CARTESIAN_POINT ( 'NONE',  ( 4.999999999999992006, -8.660254037844389075, -91.12500000409677625 ) ) ;
#12275 = CYLINDRICAL_SURFACE ( 'NONE', #24306, 60.00000000000000711 ) ;
#12276 = CARTESIAN_POINT ( 'NONE',  ( -10.81189881249999729, 1.324075727343319199E-15, -158.2812500020484094 ) ) ;
#12277 = CARTESIAN_POINT ( 'NONE',  ( 10.81189881249999551, -6.242252689847874514, -47.96875000204836681 ) ) ;
#12278 = ORIENTED_EDGE ( 'NONE', *, *, #17483, .F. ) ;
#12279 = CARTESIAN_POINT ( 'NONE',  ( 10.00000000000000000, 5.773502691896255534, -13.87499999999997158 ) ) ;
#12280 = CARTESIAN_POINT ( 'NONE',  ( 5.405949406249992428, -9.363379034771808662, -24.28125000204836681 ) ) ;
#12281 = CARTESIAN_POINT ( 'NONE',  ( 9.999999999999996447, -5.773502691896262640, -150.6250000000000000 ) ) ;
#12282 = VECTOR ( 'NONE', #39322, 1000.000000000000000 ) ;
#12283 = CARTESIAN_POINT ( 'NONE',  ( 7.070501591499377789E-16, 11.54700538379251284, -17.00000000409676559 ) ) ;
#12284 = FACE_OUTER_BOUND ( 'NONE', #16828, .T. ) ;
#12285 = EDGE_CURVE ( 'NONE', #35398, #6419, #12477, .T. ) ;
#12287 = VERTEX_POINT ( 'NONE', #25670 ) ;
#12286 = CARTESIAN_POINT ( 'NONE',  ( -5.405949406249996869, 9.363379034771805109, -128.5312500020484094 ) ) ;
#12288 = ORIENTED_EDGE ( 'NONE', *, *, #13812, .T. ) ;
#12289 = CARTESIAN_POINT ( 'NONE',  ( -2.293366432827344421E-15, -12.48450537969573659, -57.40625000204838102 ) ) ;
#12290 = PERSON_AND_ORGANIZATION_ROLE ( 'classification_officer' ) ;
#12291 = CARTESIAN_POINT ( 'NONE',  ( 7.644554776091147741E-16, 12.48450537969573659, -101.4687500020483668 ) ) ;
#12293 = VERTEX_POINT ( 'NONE', #19178 ) ;
#12292 = ORIENTED_EDGE ( 'NONE', *, *, #42320, .T. ) ;
#12294 = CARTESIAN_POINT ( 'NONE',  ( 9.999999999999998224, 0.000000000000000000, -170.3750000040968189 ) ) ;
#12295 = CARTESIAN_POINT ( 'NONE',  ( -9.999999999999998224, 1.224646799147353059E-15, -198.1250000040967905 ) ) ;
#12296 = CARTESIAN_POINT ( 'NONE',  ( -10.81189881249999729, 1.324075727343319199E-15, -161.0937500020484094 ) ) ;
#12297 = CARTESIAN_POINT ( 'NONE',  ( 5.405949406249999534, 9.363379034771803333, -188.7812500020484094 ) ) ;
#12298 = CARTESIAN_POINT ( 'NONE',  ( 10.81189881249999907, 6.242252689847868297, -4.218750002048367698 ) ) ;
#12299 = CARTESIAN_POINT ( 'NONE',  ( 0.000000000000000000, 0.000000000000000000, -99.99999999999998579 ) ) ;
#12300 = CARTESIAN_POINT ( 'NONE',  ( 7.644554776091147741E-16, 12.48450537969573659, -143.4687500020484094 ) ) ;
#12301 = VECTOR ( 'NONE', #30444, 1000.000000000000000 ) ;
#12302 = CARTESIAN_POINT ( 'NONE',  ( 10.81189881249999729, 0.000000000000000000, -110.8437500020483810 ) ) ;
#12303 = CARTESIAN_POINT ( 'NONE',  ( 10.81189881249999551, -6.242252689847874514, -118.6562500020483952 ) ) ;
#12304 = CARTESIAN_POINT ( 'NONE',  ( 4.999999999999992006, -8.660254037844389075, -194.6250000040967905 ) ) ;
#12305 = CARTESIAN_POINT ( 'NONE',  ( -10.81189881249999729, -6.242252689847864744, -120.4687500020483952 ) ) ;
#12306 = CARTESIAN_POINT ( 'NONE',  ( -2.293366432827344421E-15, -12.48450537969573659, -196.9062500020484094 ) ) ;
#12307 = CARTESIAN_POINT ( 'NONE',  ( 7.070501591499376803E-16, 11.54700538379251284, -179.0000000040967905 ) ) ;
#12308 = CARTESIAN_POINT ( 'NONE',  ( -4.999999999999996447, 8.660254037844387298, -142.5000000000000000 ) ) ;
#12309 = CARTESIAN_POINT ( 'NONE',  ( -9.999999999999998224, 5.773502691896259087, -11.87499999999996803 ) ) ;
#12310 = CARTESIAN_POINT ( 'NONE',  ( 5.405949406249999534, 9.363379034771803333, -71.59375000204836681 ) ) ;
#12311 = CARTESIAN_POINT ( 'NONE',  ( 10.81189881249999729, 0.000000000000000000, -53.84375000204835970 ) ) ;
#12312 = CARTESIAN_POINT ( 'NONE',  ( -9.999999999999998224, 5.773502691896259087, -184.7500000040968189 ) ) ;
#12313 = CARTESIAN_POINT ( 'NONE',  ( 10.81189881249999551, -6.242252689847874514, -30.15625000204836326 ) ) ;
#12314 = CARTESIAN_POINT ( 'NONE',  ( -10.81189881249999729, 1.324075727343319199E-15, -38.09375000204837391 ) ) ;
#12315 = CARTESIAN_POINT ( 'NONE',  ( -10.00000000000051337, 5.773502691895962435, -148.7500000040967620 ) ) ;
#12316 = CARTESIAN_POINT ( 'NONE',  ( -5.405949406249996869, 9.363379034771805109, -144.8437500020483810 ) ) ;
#12317 = CARTESIAN_POINT ( 'NONE',  ( -10.00000000000000000, -5.773502691896251982, -113.6249999999999858 ) ) ;
#12318 = CARTESIAN_POINT ( 'NONE',  ( -4.999999999999996447, 8.660254037844387298, -145.5000000000000000 ) ) ;
#12319 = CARTESIAN_POINT ( 'NONE',  ( -9.999999999999998224, 5.773502691896259087, -79.37500000000000000 ) ) ;
#12320 = CARTESIAN_POINT ( 'NONE',  ( 10.81189881249999907, 6.242252689847868297, -139.4062500020484094 ) ) ;
#12321 = CARTESIAN_POINT ( 'NONE',  ( -5.405949406249996869, 9.363379034771805109, -8.531250002048352599 ) ) ;
#12322 = ORIENTED_EDGE ( 'NONE', *, *, #13590, .F. ) ;
#12323 = CARTESIAN_POINT ( 'NONE',  ( 10.00000000000051159, -5.773502691895965988, -176.1250000000000000 ) ) ;
#12324 = CARTESIAN_POINT ( 'NONE',  ( -2.121150477449813534E-15, -11.54700538379251284, -112.2500000040967763 ) ) ;
#12325 = CARTESIAN_POINT ( 'NONE',  ( -9.999999999999998224, 1.224646799147353059E-15, -87.12500000409677625 ) ) ;
#12326 = CARTESIAN_POINT ( 'NONE',  ( -2.293366432827344421E-15, -12.48450537969573659, -76.71875000204838102 ) ) ;
#12327 = CARTESIAN_POINT ( 'NONE',  ( 5.000000000000000000, 8.660254037844385522, -42.24999999999997868 ) ) ;
#12328 = CARTESIAN_POINT ( 'NONE',  ( -9.999999999999998224, 5.773502691896259087, -24.25000000409676204 ) ) ;
#12329 = CARTESIAN_POINT ( 'NONE',  ( -2.293366432827344421E-15, -12.48450537969573659, -51.40625000204838102 ) ) ;
#12330 = CARTESIAN_POINT ( 'NONE',  ( 9.999999999999998224, 0.000000000000000000, -12.87500000409674783 ) ) ;
#12331 = CARTESIAN_POINT ( 'NONE',  ( 10.81189881249999551, -6.242252689847874514, -36.15625000204835970 ) ) ;
#12332 = DIRECTION ( 'NONE',  ( -0.4999999999999997224, -0.8660254037844388186, -0.000000000000000000 ) ) ;
#12333 = CARTESIAN_POINT ( 'NONE',  ( 10.81189881249999551, -6.242252689847874514, -147.1562500020484094 ) ) ;
#12334 = CARTESIAN_POINT ( 'NONE',  ( -2.293366432827344421E-15, -12.48450537969573659, -150.4062500020483810 ) ) ;
#12335 = CIRCLE ( 'NONE', #1324, 31.99999999999997158 ) ;
#12336 = CARTESIAN_POINT ( 'NONE',  ( -9.999999999999998224, 1.224646799147353059E-15, -174.1250000040968189 ) ) ;
#12337 = ORIENTED_EDGE ( 'NONE', *, *, #41795, .F. ) ;
#12338 = ORIENTED_EDGE ( 'NONE', *, *, #31811, .F. ) ;
#12339 = ORIENTED_EDGE ( 'NONE', *, *, #34353, .T. ) ;
#12340 = ADVANCED_FACE ( 'NONE', ( #15920 ), #200, .F. ) ;
#12341 = CARTESIAN_POINT ( 'NONE',  ( -1.040834085586084257E-14, 20.00000000000000711, 22.49999999999999289 ) ) ;
#12342 = CARTESIAN_POINT ( 'NONE',  ( -10.81189881249999729, 6.242252689847871849, -185.2187500020483810 ) ) ;
#12343 = CARTESIAN_POINT ( 'NONE',  ( -5.405949406250003975, -9.363379034771801557, -28.84375000204836326 ) ) ;
#12344 = FACE_OUTER_BOUND ( 'NONE', #42526, .T. ) ;
#12345 = CARTESIAN_POINT ( 'NONE',  ( 5.405949406249999534, 9.363379034771803333, -167.5937500020484094 ) ) ;
#12346 = CARTESIAN_POINT ( 'NONE',  ( -2.293366432827344421E-15, -12.48450537969573659, -154.7187500020483810 ) ) ;
#12347 =( BOUNDED_CURVE ( )  B_SPLINE_CURVE ( 2, ( #30928, #40825, #1363, #3957, #4165, #1584, #7188 ),
 .UNSPECIFIED., .F., .F. ) 
 B_SPLINE_CURVE_WITH_KNOTS ( ( 3, 2, 2, 3 ),
 ( 0.2611940298507463565, 0.2624378109452737418, 0.2636815920398011270, 0.2649253731343284568 ),
 .UNSPECIFIED. ) 
 CURVE ( )  GEOMETRIC_REPRESENTATION_ITEM ( )  RATIONAL_B_SPLINE_CURVE ( ( 0.9999999999999880096, 0.8660254037844506980, 1.000000000000000000, 0.8660254037844387076, 1.000000000000000000, 0.8660254037844267172, 1.000000000000011990 ) ) 
 REPRESENTATION_ITEM ( '' )  );
#12348 = CARTESIAN_POINT ( 'NONE',  ( 9.999999999999998224, 0.000000000000000000, -176.0000000000000000 ) ) ;
#12349 = CARTESIAN_POINT ( 'NONE',  ( -10.81189881249999907, -6.242252689847864744, -135.4687500020483810 ) ) ;
#12350 = CARTESIAN_POINT ( 'NONE',  ( -2.293366432827344421E-15, -12.48450537969573659, -139.9062500020484094 ) ) ;
#12351 = CARTESIAN_POINT ( 'NONE',  ( 7.644554776091147741E-16, 12.48450537969573659, -15.96875000204835615 ) ) ;
#12352 = CARTESIAN_POINT ( 'NONE',  ( -10.81189881249999729, 1.324075727343319199E-15, -149.0937500020483810 ) ) ;
#12353 = CARTESIAN_POINT ( 'NONE',  ( 10.00000000000051159, -5.773502691895965988, -152.1250000000000000 ) ) ;
#12354 = CARTESIAN_POINT ( 'NONE',  ( 9.999999999998969713, 5.773502691896851502, -11.25000000409674072 ) ) ;
#12355 = CARTESIAN_POINT ( 'NONE',  ( -9.999999999999998224, 1.224646799147353059E-15, -160.2500000000000000 ) ) ;
#12356 = CARTESIAN_POINT ( 'NONE',  ( -10.81189881249999729, 6.242252689847871849, -84.71875000204836681 ) ) ;
#12357 = CARTESIAN_POINT ( 'NONE',  ( 0.000000000000000000, 0.000000000000000000, -200.0000000000000000 ) ) ;
#12358 = CARTESIAN_POINT ( 'NONE',  ( -5.405949406250003975, -9.363379034771801557, -48.53125000204838813 ) ) ;
#12359 = CARTESIAN_POINT ( 'NONE',  ( -2.293366432827344421E-15, -12.48450537969573659, -60.21875000204837391 ) ) ;
#12360 = DIRECTION ( 'NONE',  ( 1.000000000000000000, 0.000000000000000000, 0.000000000000000000 ) ) ;
#12361 = CARTESIAN_POINT ( 'NONE',  ( -5.405949406249996869, 9.363379034771805109, -171.8437500020484094 ) ) ;
#12362 = CARTESIAN_POINT ( 'NONE',  ( -4.999999999999996447, 8.660254037844387298, -138.0000000000000000 ) ) ;
#12363 = CARTESIAN_POINT ( 'NONE',  ( 10.81189881249999729, 0.000000000000000000, -142.5312500020483810 ) ) ;
#12364 = CARTESIAN_POINT ( 'NONE',  ( -5.000000000000003553, -8.660254037844383745, -29.49999999999997158 ) ) ;
#12365 = CARTESIAN_POINT ( 'NONE',  ( 5.405949406249992428, -9.363379034771808662, -36.28125000204837391 ) ) ;
#12366 = CARTESIAN_POINT ( 'NONE',  ( 5.000000000000000000, 8.660254037844385522, -123.6250000040967905 ) ) ;
#12367 = CARTESIAN_POINT ( 'NONE',  ( 5.000000000000000000, 8.660254037844385522, -100.7499999999999858 ) ) ;
#12368 = EDGE_LOOP ( 'NONE', ( #28282, #26238, #35608, #32518 ) ) ;
#12369 = CARTESIAN_POINT ( 'NONE',  ( -10.81189881249999729, 1.324075727343319199E-15, -116.2812500020483952 ) ) ;
#12370 = CARTESIAN_POINT ( 'NONE',  ( -2.121150477449813534E-15, -11.54700538379251284, -142.2500000040967905 ) ) ;
#12371 = CARTESIAN_POINT ( 'NONE',  ( -9.999999999999998224, 1.224646799147353059E-15, -158.7500000000000000 ) ) ;
#12372 = AXIS2_PLACEMENT_3D ( 'NONE', #28237, #11589, #8168 ) ;
#12373 = EDGE_CURVE ( 'NONE', #34380, #21209, #17755, .T. ) ;
#12374 = CARTESIAN_POINT ( 'NONE',  ( 5.405949406249992428, -9.363379034771808662, -169.7812500020484094 ) ) ;
#12375 = CARTESIAN_POINT ( 'NONE',  ( -2.121150477449813534E-15, -11.54700538379251284, -46.25000000409676915 ) ) ;
#12376 = DIRECTION ( 'NONE',  ( -0.000000000000000000, -0.000000000000000000, 1.000000000000000000 ) ) ;
#12377 = CARTESIAN_POINT ( 'NONE',  ( 5.405949406249992428, -9.363379034771808662, -61.78125000204837391 ) ) ;
#12378 = CARTESIAN_POINT ( 'NONE',  ( 9.999999999999998224, 0.000000000000000000, -147.8750000040967905 ) ) ;
#12379 = CARTESIAN_POINT ( 'NONE',  ( 10.81189881249999551, -6.242252689847874514, -168.1562500020484094 ) ) ;
#12380 = CARTESIAN_POINT ( 'NONE',  ( 9.999999999999998224, 0.000000000000000000, -183.8750000040967905 ) ) ;
#12381 = CARTESIAN_POINT ( 'NONE',  ( 10.00000000000044764, -5.773502691896004180, -177.6249999999999716 ) ) ;
#12382 = ORIENTED_EDGE ( 'NONE', *, *, #32988, .F. ) ;
#12383 = CARTESIAN_POINT ( 'NONE',  ( 9.999999999999998224, 0.000000000000000000, -51.87500000409675494 ) ) ;
#12384 =( BOUNDED_CURVE ( )  B_SPLINE_CURVE ( 2, ( #22123, #42164, #12177, #12385, #2289, #41952, #15828 ),
 .UNSPECIFIED., .F., .F. ) 
 B_SPLINE_CURVE_WITH_KNOTS ( ( 3, 2, 2, 3 ),
 ( 0.6380597014925374344, 0.6393034825870648197, 0.6405472636815923160, 0.6417910447761195902 ),
 .UNSPECIFIED. ) 
 CURVE ( )  GEOMETRIC_REPRESENTATION_ITEM ( )  RATIONAL_B_SPLINE_CURVE ( ( 0.9999999999999880096, 0.8660254037844506980, 1.000000000000000000, 0.8660254037844387076, 1.000000000000000000, 0.8660254037844148378, 1.000000000000023981 ) ) 
 REPRESENTATION_ITEM ( '' )  );
#12385 = CARTESIAN_POINT ( 'NONE',  ( -2.121150477449813534E-15, -11.54700538379251284, -71.37499999999998579 ) ) ;
#12387 = EDGE_LOOP ( 'NONE', ( #11540, #31481, #17855, #38948 ) ) ;
#12386 = CARTESIAN_POINT ( 'NONE',  ( -10.81189881249999729, 6.242252689847871849, -74.40625000204836681 ) ) ;
#12389 = ORIENTED_EDGE ( 'NONE', *, *, #10314, .F. ) ;
#12388 = CARTESIAN_POINT ( 'NONE',  ( 4.999999999999992006, -8.660254037844389075, -188.6250000040967905 ) ) ;
#12390 = ORIENTED_EDGE ( 'NONE', *, *, #7748, .F. ) ;
#12391 = CARTESIAN_POINT ( 'NONE',  ( -5.405949406250003975, -9.363379034771801557, -31.84375000204836681 ) ) ;
#12393 = CARTESIAN_POINT ( 'NONE',  ( 4.999999999999992006, -8.660254037844389075, -170.6250000040968189 ) ) ;
#12392 =( BOUNDED_CURVE ( )  B_SPLINE_CURVE ( 2, ( #23013, #35761, #19970, #32939, #9833, #29701, #147 ),
 .UNSPECIFIED., .F., .F. ) 
 B_SPLINE_CURVE_WITH_KNOTS ( ( 3, 2, 2, 3 ),
 ( 0.2723880597014926574, 0.2736318407960199872, 0.2748756218905473725, 0.2761194029850747578 ),
 .UNSPECIFIED. ) 
 CURVE ( )  GEOMETRIC_REPRESENTATION_ITEM ( )  RATIONAL_B_SPLINE_CURVE ( ( 0.9999999999999880096, 0.8660254037844506980, 1.000000000000000000, 0.8660254037844387076, 1.000000000000000000, 0.8660254037844267172, 1.000000000000011990 ) ) 
 REPRESENTATION_ITEM ( '' )  );
#12394 = CARTESIAN_POINT ( 'NONE',  ( 7.644554776091147741E-16, 12.48450537969573659, -7.156250002048365921 ) ) ;
#12396 = ORIENTED_EDGE ( 'NONE', *, *, #31200, .F. ) ;
#12395 = CARTESIAN_POINT ( 'NONE',  ( -10.81189881249999729, 1.324075727343319199E-15, -54.59375000204835970 ) ) ;
#12397 = CARTESIAN_POINT ( 'NONE',  ( 4.999999999999992006, -8.660254037844389075, -109.1250000040967763 ) ) ;
#12398 = ADVANCED_FACE ( 'NONE', ( #39453 ), #28912, .T. ) ;
#12399 = CARTESIAN_POINT ( 'NONE',  ( 5.000000000000000000, 8.660254037844385522, -28.74999999999997158 ) ) ;
#12400 = CARTESIAN_POINT ( 'NONE',  ( -10.81189881249999729, 1.324075727343319199E-15, -186.5937500020483810 ) ) ;
#12401 = CARTESIAN_POINT ( 'NONE',  ( 5.405949406249992428, -9.363379034771808662, -174.0937500020484094 ) ) ;
#12402 = CARTESIAN_POINT ( 'NONE',  ( 5.405949406249992428, -9.363379034771808662, -156.0937500020483810 ) ) ;
#12403 = CARTESIAN_POINT ( 'NONE',  ( -5.405949406249996869, 9.363379034771805109, -167.3437500020484094 ) ) ;
#12404 = CARTESIAN_POINT ( 'NONE',  ( 9.999999999999998224, 0.000000000000000000, -200.0000000000000000 ) ) ;
#12405 =( BOUNDED_CURVE ( )  B_SPLINE_CURVE ( 2, ( #24935, #41297, #14535, #1839, #4848, #34640, #21027 ),
 .UNSPECIFIED., .F., .F. ) 
 B_SPLINE_CURVE_WITH_KNOTS ( ( 3, 2, 2, 3 ),
 ( 0.1604477611940298698, 0.1616915422885572551, 0.1629353233830845848, 0.1641791044776119424 ),
 .UNSPECIFIED. ) 
 CURVE ( )  GEOMETRIC_REPRESENTATION_ITEM ( )  RATIONAL_B_SPLINE_CURVE ( ( 0.9999999999999970024, 0.8660254037844417052, 1.000000000000000000, 0.8660254037844387076, 1.000000000000000000, 0.8660254037844387076, 1.000000000000000000 ) ) 
 REPRESENTATION_ITEM ( '' )  );
#12406 = CARTESIAN_POINT ( 'NONE',  ( 4.999999999999992006, -8.660254037844389075, -198.7500000000000000 ) ) ;
#12407 = CARTESIAN_POINT ( 'NONE',  ( 7.644554776091147741E-16, 12.48450537969573659, -105.9687500020483668 ) ) ;
#12408 = CARTESIAN_POINT ( 'NONE',  ( 0.000000000000000000, 0.000000000000000000, -200.0000000000000000 ) ) ;
#12409 = CARTESIAN_POINT ( 'NONE',  ( -5.405949406250003975, -9.363379034771801557, -74.03125000204838102 ) ) ;
#12410 = CARTESIAN_POINT ( 'NONE',  ( 10.81189881249999551, -6.242252689847874514, -95.96875000204838102 ) ) ;
#12411 = CARTESIAN_POINT ( 'NONE',  ( 10.81189881249999907, 6.242252689847868297, -56.90625000204837391 ) ) ;
#12412 = CARTESIAN_POINT ( 'NONE',  ( -4.999999999999996447, 8.660254037844387298, -145.8750000040967905 ) ) ;
#12413 = CARTESIAN_POINT ( 'NONE',  ( -9.999999999999998224, 5.773502691896259087, -119.8750000000000000 ) ) ;
#12414 = ORIENTED_EDGE ( 'NONE', *, *, #30168, .T. ) ;
#12415 = CARTESIAN_POINT ( 'NONE',  ( 10.81189881249999729, 0.000000000000000000, -145.5312500020483810 ) ) ;
#12416 = CARTESIAN_POINT ( 'NONE',  ( 10.81189881249999551, -6.242252689847874514, -156.1562500020484094 ) ) ;
#12417 = CARTESIAN_POINT ( 'NONE',  ( 10.81189881249999551, -6.242252689847874514, -195.1562500020484379 ) ) ;
#12418 = FACE_OUTER_BOUND ( 'NONE', #40832, .T. ) ;
#12419 = CARTESIAN_POINT ( 'NONE',  ( 10.81189881249999729, 0.000000000000000000, -86.84375000204836681 ) ) ;
#12420 = ORIENTED_EDGE ( 'NONE', *, *, #24247, .T. ) ;
#12421 = CARTESIAN_POINT ( 'NONE',  ( -9.999999999999998224, 5.773502691896259087, -65.87499999999998579 ) ) ;
#12422 = CARTESIAN_POINT ( 'NONE',  ( 10.81189881249999551, -6.242252689847874514, -190.4687500020484094 ) ) ;
#12423 = CARTESIAN_POINT ( 'NONE',  ( 9.999999999999996447, -5.773502691896262640, -71.50000000409676204 ) ) ;
#12424 = CARTESIAN_POINT ( 'NONE',  ( -2.121150477449813534E-15, -11.54700538379251284, -116.7500000040967905 ) ) ;
#12425 = CARTESIAN_POINT ( 'NONE',  ( 9.999999999999998224, 0.000000000000000000, -140.3750000040967905 ) ) ;
#12426 = CARTESIAN_POINT ( 'NONE',  ( -10.81189881249999729, 6.242252689847871849, -80.40625000204839523 ) ) ;
#12427 = CARTESIAN_POINT ( 'NONE',  ( 10.81189881249999729, 6.242252689847867408, -68.90625000204840944 ) ) ;
#12428 = CARTESIAN_POINT ( 'NONE',  ( 9.999999999999998224, 0.000000000000000000, -66.87500000409676204 ) ) ;
#12429 = CARTESIAN_POINT ( 'NONE',  ( 10.81189881249999907, 6.242252689847868297, -17.71875000204836681 ) ) ;
#12430 = CARTESIAN_POINT ( 'NONE',  ( -10.00000000000051337, 5.773502691895962435, -46.75000000409676915 ) ) ;
#12431 = CARTESIAN_POINT ( 'NONE',  ( 5.405949406249992428, -9.363379034771808662, -195.2812500020484094 ) ) ;
#12432 = CARTESIAN_POINT ( 'NONE',  ( 7.644554776091147741E-16, 12.48450537969573659, -19.15625000204837391 ) ) ;
#12433 = CARTESIAN_POINT ( 'NONE',  ( -10.81189881249999729, 1.324075727343319199E-15, -3.593750002048368142 ) ) ;
#12434 = CARTESIAN_POINT ( 'NONE',  ( 5.000000000000000000, 8.660254037844385522, -140.1250000040967905 ) ) ;
#12435 = VECTOR ( 'NONE', #3531, 1000.000000000000000 ) ;
#12436 = CARTESIAN_POINT ( 'NONE',  ( -10.00000000000025757, -5.773502691896102768, -181.1250000000000000 ) ) ;
#12437 = CARTESIAN_POINT ( 'NONE',  ( -5.000000000000003553, -8.660254037844383745, -137.5000000000000000 ) ) ;
#12438 = CARTESIAN_POINT ( 'NONE',  ( -9.999999999999998224, 5.773502691896259087, -173.8749999999999716 ) ) ;
#12439 = LINE ( 'NONE', #16303, #32433 ) ;
#12441 = ORIENTED_EDGE ( 'NONE', *, *, #37394, .F. ) ;
#12440 = CARTESIAN_POINT ( 'NONE',  ( -10.81189881249999907, -6.242252689847864744, -99.65625000204839523 ) ) ;
#12442 = CARTESIAN_POINT ( 'NONE',  ( 5.000000000000000000, 8.660254037844385522, -116.1250000040967905 ) ) ;
#12443 = ORIENTED_EDGE ( 'NONE', *, *, #7820, .T. ) ;
#12444 = ORIENTED_EDGE ( 'NONE', *, *, #23289, .T. ) ;
#12445 = CARTESIAN_POINT ( 'NONE',  ( 10.81189881249999729, 0.000000000000000000, -31.53125000204837391 ) ) ;
#12446 = ADVANCED_FACE ( 'NONE', ( #26510 ), #22852, .F. ) ;
#12447 = CARTESIAN_POINT ( 'NONE',  ( -10.81189881249999729, 6.242252689847871849, -78.71875000204838102 ) ) ;
#12448 = DIRECTION ( 'NONE',  ( 1.000000000000000000, 0.000000000000000000, 0.000000000000000000 ) ) ;
#12449 = ADVANCED_FACE ( 'NONE', ( #9469 ), #35810, .T. ) ;
#12450 = CARTESIAN_POINT ( 'NONE',  ( 10.18637341149928410, -0.5909213003623300375, -100.0000000000000000 ) ) ;
#12451 = EDGE_CURVE ( 'NONE', #9613, #40457, #13105, .T. ) ;
#12452 = ADVANCED_FACE ( 'NONE', ( #19386 ), #20018, .T. ) ;
#12453 = CARTESIAN_POINT ( 'NONE',  ( 9.999999999999998224, 0.000000000000000000, -108.4999999999999858 ) ) ;
#12454 = CARTESIAN_POINT ( 'NONE',  ( 9.999999999999998224, 0.000000000000000000, -72.87500000409677625 ) ) ;
#12455 = CARTESIAN_POINT ( 'NONE',  ( -10.81189881249999729, 6.242252689847871849, -156.9062500020483810 ) ) ;
#12456 = CARTESIAN_POINT ( 'NONE',  ( -9.999999999999998224, 1.224646799147353059E-15, -7.625000004096743389 ) ) ;
#12457 = DIRECTION ( 'NONE',  ( 1.000000000000000000, 0.000000000000000000, 0.000000000000000000 ) ) ;
#12458 = LOCAL_TIME ( 11, 57, 6.000000000000000000, #26002 ) ;
#12459 = CARTESIAN_POINT ( 'NONE',  ( -5.405949406249996869, 9.363379034771805109, -129.8437500020484094 ) ) ;
#12460 = CARTESIAN_POINT ( 'NONE',  ( -5.405949406249996869, 9.363379034771805109, -114.8437500020483810 ) ) ;
#12461 = CARTESIAN_POINT ( 'NONE',  ( 10.81189881249999551, -6.242252689847874514, -80.96875000204838102 ) ) ;
#12462 = CARTESIAN_POINT ( 'NONE',  ( -2.293366432827344421E-15, -12.48450537969573659, -84.40625000204838102 ) ) ;
#12463 = CARTESIAN_POINT ( 'NONE',  ( 7.070501591499377789E-16, 11.54700538379251284, -173.0000000040967905 ) ) ;
#12464 = DIRECTION ( 'NONE',  ( -0.000000000000000000, -0.000000000000000000, 1.000000000000000000 ) ) ;
#12465 = CARTESIAN_POINT ( 'NONE',  ( -2.293366432827344421E-15, -12.48450537969573659, -165.4062500020483526 ) ) ;
#12466 = CARTESIAN_POINT ( 'NONE',  ( -10.81189881249999907, -6.242252689847864744, -182.1562500020483810 ) ) ;
#12467 = CARTESIAN_POINT ( 'NONE',  ( -5.405949406250003975, -9.363379034771801557, -45.34375000204838102 ) ) ;
#12468 = CARTESIAN_POINT ( 'NONE',  ( 9.999999999999998224, 0.000000000000000000, -156.8750000040967905 ) ) ;
#12469 = CARTESIAN_POINT ( 'NONE',  ( -2.293366432827344421E-15, -12.48450537969573659, -4.906250002048355263 ) ) ;
#12470 = CARTESIAN_POINT ( 'NONE',  ( -2.293366432827344421E-15, -12.48450537969573659, -7.718750002048357040 ) ) ;
#12471 = CARTESIAN_POINT ( 'NONE',  ( -10.81189881249999729, 1.324075727343319199E-15, -111.5937500020483810 ) ) ;
#12472 = CARTESIAN_POINT ( 'NONE',  ( -9.999999999999998224, 5.773502691896259087, -92.87500000000000000 ) ) ;
#12473 = CARTESIAN_POINT ( 'NONE',  ( -10.81189881249999907, -6.242252689847864744, -20.15625000204837747 ) ) ;
#12474 = CARTESIAN_POINT ( 'NONE',  ( 10.00000000000000000, 5.773502691896255534, -95.25000000409679046 ) ) ;
#12475 = EDGE_CURVE ( 'NONE', #25614, #19247, #3003, .T. ) ;
#12476 =( BOUNDED_CURVE ( )  B_SPLINE_CURVE ( 2, ( #22091, #38485, #5700, #41281, #18851, #15800, #21656 ),
 .UNSPECIFIED., .F., .F. ) 
 B_SPLINE_CURVE_WITH_KNOTS ( ( 3, 2, 2, 3 ),
 ( 0.8208955223880598506, 0.8221393034825871249, 0.8233830845771146212, 0.8246268656716420065 ),
 .UNSPECIFIED. ) 
 CURVE ( )  GEOMETRIC_REPRESENTATION_ITEM ( )  RATIONAL_B_SPLINE_CURVE ( ( 0.9999999999999880096, 0.8660254037844506980, 1.000000000000000000, 0.8660254037844387076, 1.000000000000000000, 0.8660254037844148378, 1.000000000000023981 ) ) 
 REPRESENTATION_ITEM ( '' )  );
#12477 = LINE ( 'NONE', #16557, #16844 ) ;
#12478 = CARTESIAN_POINT ( 'NONE',  ( 10.81189881249999907, 6.242252689847868297, -115.4062500020484094 ) ) ;
#12479 = CARTESIAN_POINT ( 'NONE',  ( -10.81189881249999729, -6.242252689847864744, -92.15625000204836681 ) ) ;
#12480 = EDGE_LOOP ( 'NONE', ( #19404, #38003, #6343, #27634 ) ) ;
#12481 = CARTESIAN_POINT ( 'NONE',  ( 9.999999999999996447, -5.773502691896262640, -91.00000000409677625 ) ) ;
#12482 = CARTESIAN_POINT ( 'NONE',  ( 11.54700538379250396, 20.00000000000000711, 0.000000000000000000 ) ) ;
#12483 = CARTESIAN_POINT ( 'NONE',  ( 10.81189881249999551, -6.242252689847874514, -50.96875000204836681 ) ) ;
#12485 = ADVANCED_FACE ( 'NONE', ( #16127 ), #32776, .T. ) ;
#12484 = ORIENTED_EDGE ( 'NONE', *, *, #8111, .T. ) ;
#12486 = CARTESIAN_POINT ( 'NONE',  ( 5.000000000000000000, 8.660254037844385522, -19.74999999999996092 ) ) ;
#12487 = CARTESIAN_POINT ( 'NONE',  ( 10.81189881249999729, 6.242252689847867408, -22.40625000204837747 ) ) ;
#12488 = CARTESIAN_POINT ( 'NONE',  ( -9.999999999999998224, 5.773502691896259087, -149.8750000000000000 ) ) ;
#12489 = ADVANCED_FACE ( 'NONE', ( #30396 ), #33842, .F. ) ;
#12490 = CARTESIAN_POINT ( 'NONE',  ( 5.000000000000000000, 8.660254037844385522, -20.12500000409675494 ) ) ;
#12491 = VECTOR ( 'NONE', #732, 1000.000000000000000 ) ;
#12492 = CC_DESIGN_APPROVAL ( #31498, ( #36620 ) ) ;
#12493 = CARTESIAN_POINT ( 'NONE',  ( -2.121150477449813534E-15, -11.54700538379251284, -195.8750000000000284 ) ) ;
#12495 = ORIENTED_EDGE ( 'NONE', *, *, #20226, .F. ) ;
#12494 = CARTESIAN_POINT ( 'NONE',  ( -2.293366432827344421E-15, -12.48450537969573659, -126.4062500020483952 ) ) ;
#12496 = CARTESIAN_POINT ( 'NONE',  ( 10.00000000000102318, -5.773502691895667560, -12.62499999999993605 ) ) ;
#12497 = VERTEX_POINT ( 'NONE', #39869 ) ;
#12498 = CARTESIAN_POINT ( 'NONE',  ( -10.81189881249999729, 6.242252689847871849, -50.40625000204837391 ) ) ;
#12499 = PERSON_AND_ORGANIZATION ( #11915, #17965 ) ;
#12500 = VECTOR ( 'NONE', #41088, 1000.000000000000000 ) ;
#12501 = CARTESIAN_POINT ( 'NONE',  ( 10.81189881249999551, -6.242252689847874514, -104.9687500020483810 ) ) ;
#12503 = EDGE_LOOP ( 'NONE', ( #36489, #27113, #2761, #29347 ) ) ;
#12502 = EDGE_LOOP ( 'NONE', ( #31371, #19317, #9377, #18993 ) ) ;
#12504 = CARTESIAN_POINT ( 'NONE',  ( -9.999999999999998224, 1.224646799147353059E-15, -175.2500000000000284 ) ) ;
#12505 = CARTESIAN_POINT ( 'NONE',  ( 0.000000000000000000, 0.000000000000000000, -219.9999999999999716 ) ) ;
#12507 = EDGE_CURVE ( 'NONE', #35463, #9647, #29388, .T. ) ;
#12506 = CARTESIAN_POINT ( 'NONE',  ( 5.405949406249992428, -9.363379034771808662, -150.0937500020483810 ) ) ;
#12508 = CARTESIAN_POINT ( 'NONE',  ( 10.81189881249999551, -6.242252689847874514, -180.1562500020484379 ) ) ;
#12509 = CARTESIAN_POINT ( 'NONE',  ( 5.405949406249999534, 9.363379034771803333, -8.593750002048345493 ) ) ;
#12510 = DIRECTION ( 'NONE',  ( -0.000000000000000000, -0.000000000000000000, 1.000000000000000000 ) ) ;
#12511 = EDGE_CURVE ( 'NONE', #21406, #39053, #6199, .T. ) ;
#12512 = CARTESIAN_POINT ( 'NONE',  ( -5.405949406250003975, -9.363379034771801557, -141.3437500020483810 ) ) ;
#12513 = CARTESIAN_POINT ( 'NONE',  ( 10.81189881249999907, 6.242252689847868297, -100.2187500020483810 ) ) ;
#12514 = CARTESIAN_POINT ( 'NONE',  ( -9.999999999999998224, 1.224646799147353059E-15, -143.7500000000000000 ) ) ;
#12515 = CARTESIAN_POINT ( 'NONE',  ( 7.644554776091147741E-16, 12.48450537969573659, -104.6562500020483810 ) ) ;
#12516 = CARTESIAN_POINT ( 'NONE',  ( -5.000000000000003553, -8.660254037844383745, -190.3750000040967905 ) ) ;
#12517 = CARTESIAN_POINT ( 'NONE',  ( 10.81189881249999729, 0.000000000000000000, -119.8437500020483810 ) ) ;
#12518 = CARTESIAN_POINT ( 'NONE',  ( 10.81189881249999551, -6.242252689847874514, -187.6562500020484094 ) ) ;
#12519 =( BOUNDED_CURVE ( )  B_SPLINE_CURVE ( 2, ( #24273, #37420, #4829, #11501, #963, #24703, #27071 ),
 .UNSPECIFIED., .F., .F. ) 
 B_SPLINE_CURVE_WITH_KNOTS ( ( 3, 2, 2, 3 ),
 ( 0.5597014925373136052, 0.5609452736318409904, 0.5621890547263683757, 0.5634328358208957610 ),
 .UNSPECIFIED. ) 
 CURVE ( )  GEOMETRIC_REPRESENTATION_ITEM ( )  RATIONAL_B_SPLINE_CURVE ( ( 0.9999999999999761302, 0.8660254037844625774, 1.000000000000000000, 0.8660254037844387076, 1.000000000000000000, 0.8660254037844148378, 1.000000000000023981 ) ) 
 REPRESENTATION_ITEM ( '' )  );
#12520 = DIRECTION ( 'NONE',  ( 0.000000000000000000, 0.000000000000000000, 1.000000000000000000 ) ) ;
#12521 = CARTESIAN_POINT ( 'NONE',  ( -9.999999999999998224, 5.773502691896259087, -140.8750000000000000 ) ) ;
#12522 = CARTESIAN_POINT ( 'NONE',  ( -4.999999999999996447, 8.660254037844387298, -13.49999999999995737 ) ) ;
#12523 = CARTESIAN_POINT ( 'NONE',  ( 5.405949406249992428, -9.363379034771808662, -64.59375000204836681 ) ) ;
#12524 = CARTESIAN_POINT ( 'NONE',  ( -10.81189881249999907, -6.242252689847864744, -45.46875000204837391 ) ) ;
#12525 = CARTESIAN_POINT ( 'NONE',  ( -9.999999999999998224, 5.773502691896259087, -189.2500000040967905 ) ) ;
#12526 = CARTESIAN_POINT ( 'NONE',  ( -5.405949406250003975, -9.363379034771801557, -26.03125000204836681 ) ) ;
#12527 = CARTESIAN_POINT ( 'NONE',  ( -10.81189881249999729, 1.324075727343319199E-15, -35.09375000204836681 ) ) ;
#12528 = CARTESIAN_POINT ( 'NONE',  ( -2.121150477449813534E-15, -11.54700538379251284, -105.8749999999999858 ) ) ;
#12529 = CARTESIAN_POINT ( 'NONE',  ( -2.293366432827344421E-15, -12.48450537969573659, -147.2187500020484094 ) ) ;
#12530 = CARTESIAN_POINT ( 'NONE',  ( -9.999999999999998224, 5.773502691896259087, -112.3749999999999858 ) ) ;
#12531 = CARTESIAN_POINT ( 'NONE',  ( -9.999999999999998224, 1.224646799147353059E-15, -200.0000000000000000 ) ) ;
#12532 = CARTESIAN_POINT ( 'NONE',  ( 4.999999999999992006, -8.660254037844389075, -69.74999999999997158 ) ) ;
#12533 = CARTESIAN_POINT ( 'NONE',  ( -5.405949406249996869, 9.363379034771805109, -137.5312500020484094 ) ) ;
#12534 = CARTESIAN_POINT ( 'NONE',  ( -2.293366432827344421E-15, -12.48450537969573659, -114.4062500020483952 ) ) ;
#12535 = EDGE_CURVE ( 'NONE', #36340, #7903, #410, .T. ) ;
#12536 = EDGE_LOOP ( 'NONE', ( #2073, #42065, #22291, #32171 ) ) ;
#12537 = DIRECTION ( 'NONE',  ( -1.000000000000000000, 0.000000000000000000, -0.000000000000000000 ) ) ;
#12538 = CARTESIAN_POINT ( 'NONE',  ( 4.999999999999992006, -8.660254037844389075, -118.1250000040967905 ) ) ;
#12539 = CARTESIAN_POINT ( 'NONE',  ( 10.00000000000051159, -5.773502691895965988, -128.1250000000000000 ) ) ;
#12540 = CARTESIAN_POINT ( 'NONE',  ( 10.81189881249999729, 0.000000000000000000, -70.34375000204836681 ) ) ;
#12541 = CARTESIAN_POINT ( 'NONE',  ( -10.00000000000000000, -5.773502691896251982, -44.62499999999997158 ) ) ;
#12542 = AXIS2_PLACEMENT_3D ( 'NONE', #19922, #2905, #6556 ) ;
#12543 = CARTESIAN_POINT ( 'NONE',  ( 7.070501591499377789E-16, 11.54700538379251284, -27.50000000409677980 ) ) ;
#12544 = CARTESIAN_POINT ( 'NONE',  ( 10.81189881249999551, -6.242252689847874514, -51.15625000204837391 ) ) ;
#12545 = CARTESIAN_POINT ( 'NONE',  ( -2.121150477449813534E-15, -11.54700538379251284, -141.8750000000000000 ) ) ;
#12546 = CARTESIAN_POINT ( 'NONE',  ( -10.81189881249999907, -6.242252689847864744, -36.65625000204835970 ) ) ;
#12547 = LINE ( 'NONE', #3277, #16215 ) ;
#12548 = CARTESIAN_POINT ( 'NONE',  ( -2.293366432827344421E-15, -12.48450537969573659, -133.9062500020483810 ) ) ;
#12549 = CARTESIAN_POINT ( 'NONE',  ( 5.405949406249992428, -9.363379034771808662, -151.7812500020484094 ) ) ;
#12550 = CARTESIAN_POINT ( 'NONE',  ( -10.00000000000012790, -5.773502691896178263, -174.0000000040968473 ) ) ;
#12551 = ORIENTED_EDGE ( 'NONE', *, *, #32029, .T. ) ;
#12552 = ORIENTED_EDGE ( 'NONE', *, *, #27477, .T. ) ;
#12553 = ORIENTED_EDGE ( 'NONE', *, *, #14304, .T. ) ;
#12554 = FACE_OUTER_BOUND ( 'NONE', #14318, .T. ) ;
#12555 = CARTESIAN_POINT ( 'NONE',  ( 10.81189881249999551, -6.242252689847874514, -181.4687500020484094 ) ) ;
#12556 = VECTOR ( 'NONE', #18115, 1000.000000000000000 ) ;
#12557 = CARTESIAN_POINT ( 'NONE',  ( -5.405949406250003975, -9.363379034771801557, -27.34375000204835970 ) ) ;
#12558 = DIRECTION ( 'NONE',  ( -0.000000000000000000, -0.000000000000000000, -1.000000000000000000 ) ) ;
#12559 = CARTESIAN_POINT ( 'NONE',  ( -10.81189881249999729, 6.242252689847871849, -165.7187500020483810 ) ) ;
#12560 = CARTESIAN_POINT ( 'NONE',  ( -5.405949406249996869, 9.363379034771805109, -143.3437500020483810 ) ) ;
#12561 = CYLINDRICAL_SURFACE ( 'NONE', #34871, 9.999999999999998224 ) ;
#12562 = CARTESIAN_POINT ( 'NONE',  ( 10.81189881249999907, 6.242252689847868297, -133.2187500020483810 ) ) ;
#12563 = CARTESIAN_POINT ( 'NONE',  ( 10.81189881249999729, 0.000000000000000000, -139.5312500020484094 ) ) ;
#12564 = CARTESIAN_POINT ( 'NONE',  ( -5.405949406249996869, 9.363379034771805109, -20.34375000204835615 ) ) ;
#12565 = CARTESIAN_POINT ( 'NONE',  ( -10.81189881249999729, -6.242252689847864744, -142.9687500020483810 ) ) ;
#12566 = DIRECTION ( 'NONE',  ( -0.000000000000000000, -0.000000000000000000, -1.000000000000000000 ) ) ;
#12567 = CARTESIAN_POINT ( 'NONE',  ( 9.999999999999479527, 5.773502691896553074, -141.7500000040967620 ) ) ;
#12568 = CARTESIAN_POINT ( 'NONE',  ( 7.070501591499377789E-16, 11.54700538379251284, -163.6250000000000000 ) ) ;
#12569 = EDGE_CURVE ( 'NONE', #26056, #3950, #22197, .T. ) ;
#12570 = CARTESIAN_POINT ( 'NONE',  ( -2.293366432827344421E-15, -12.48450537969573659, -84.21875000204835260 ) ) ;
#12571 = CARTESIAN_POINT ( 'NONE',  ( -10.81189881249999729, 6.242252689847871849, -51.90625000204838813 ) ) ;
#12572 = CARTESIAN_POINT ( 'NONE',  ( -5.405949406249996869, 9.363379034771805109, -59.34375000204835970 ) ) ;
#12573 = FACE_OUTER_BOUND ( 'NONE', #17482, .T. ) ;
#12574 = CARTESIAN_POINT ( 'NONE',  ( -2.293366432827344421E-15, -12.48450537969573659, -168.2187500020483810 ) ) ;
#12575 = CARTESIAN_POINT ( 'NONE',  ( 9.999999999999996447, -5.773502691896262640, -138.6250000000000000 ) ) ;
#12576 = CARTESIAN_POINT ( 'NONE',  ( -10.81189881249999729, 6.242252689847871849, -144.9062500020484094 ) ) ;
#12577 = CARTESIAN_POINT ( 'NONE',  ( -9.999999999998456346, -5.773502691897145489, -24.00000000409674428 ) ) ;
#12578 = CARTESIAN_POINT ( 'NONE',  ( -2.121150477449813534E-15, -11.54700538379251284, -124.2500000040967763 ) ) ;
#12579 = CARTESIAN_POINT ( 'NONE',  ( -10.00000000000000000, -5.773502691896251982, -92.62499999999998579 ) ) ;
#12580 = ORIENTED_EDGE ( 'NONE', *, *, #30657, .T. ) ;
#12581 = CARTESIAN_POINT ( 'NONE',  ( 5.405949406249999534, 9.363379034771803333, -116.7812500020483952 ) ) ;
#12582 = CARTESIAN_POINT ( 'NONE',  ( -10.00000000000000000, -5.773502691896251982, -138.0000000040967905 ) ) ;
#12583 = DIRECTION ( 'NONE',  ( 1.000000000000000000, 0.000000000000000000, 0.000000000000000000 ) ) ;
#12584 = CARTESIAN_POINT ( 'NONE',  ( 5.405949406249999534, 9.363379034771803333, -169.2812500020484094 ) ) ;
#12585 = CARTESIAN_POINT ( 'NONE',  ( -4.999999999999996447, 8.660254037844387298, -52.87500000409675494 ) ) ;
#12586 = CARTESIAN_POINT ( 'NONE',  ( 4.999999999999992006, -8.660254037844389075, -98.24999999999998579 ) ) ;
#12587 = CARTESIAN_POINT ( 'NONE',  ( 5.405949406249999534, 9.363379034771803333, -61.28125000204837391 ) ) ;
#12588 = EDGE_CURVE ( 'NONE', #28849, #12029, #35696, .T. ) ;
#12589 = DIRECTION ( 'NONE',  ( 0.000000000000000000, 0.000000000000000000, 1.000000000000000000 ) ) ;
#12590 = CARTESIAN_POINT ( 'NONE',  ( 5.405949406249999534, 9.363379034771803333, -170.7812500020484094 ) ) ;
#12591 = CARTESIAN_POINT ( 'NONE',  ( 11.54700538379253061, -15.00000000000009770, 49.99999999999998579 ) ) ;
#12592 = CARTESIAN_POINT ( 'NONE',  ( -9.999999999999998224, 1.224646799147353059E-15, -34.62500000409676915 ) ) ;
#12593 = ORIENTED_EDGE ( 'NONE', *, *, #41196, .F. ) ;
#12594 = DIRECTION ( 'NONE',  ( -0.000000000000000000, -0.000000000000000000, -1.000000000000000000 ) ) ;
#12596 = ORIENTED_EDGE ( 'NONE', *, *, #16447, .F. ) ;
#12595 = CARTESIAN_POINT ( 'NONE',  ( -10.81189881249999729, 1.324075727343319199E-15, -69.78125000204838102 ) ) ;
#12597 = ORIENTED_EDGE ( 'NONE', *, *, #23293, .T. ) ;
#12598 = VERTEX_POINT ( 'NONE', #36638 ) ;
#12599 = CARTESIAN_POINT ( 'NONE',  ( 5.405949406249992428, -9.363379034771808662, -31.59375000204836681 ) ) ;
#12600 = CARTESIAN_POINT ( 'NONE',  ( 5.000000000000000000, 8.660254037844385522, -108.2499999999999858 ) ) ;
#12601 = CARTESIAN_POINT ( 'NONE',  ( -10.81189881249999907, -6.242252689847864744, -5.156250002048356151 ) ) ;
#12603 = ORIENTED_EDGE ( 'NONE', *, *, #19230, .T. ) ;
#12602 = CARTESIAN_POINT ( 'NONE',  ( -5.405949406249996869, 9.363379034771805109, -51.84375000204835260 ) ) ;
#12604 = CARTESIAN_POINT ( 'NONE',  ( -2.121150477449813534E-15, -11.54700538379251284, -3.874999999999953815 ) ) ;
#12605 = CARTESIAN_POINT ( 'NONE',  ( 4.999999999999992006, -8.660254037844389075, -29.24999999999997158 ) ) ;
#12606 = CARTESIAN_POINT ( 'NONE',  ( -2.293366432827344421E-15, -12.48450537969573659, -186.2187500020484094 ) ) ;
#12607 = CARTESIAN_POINT ( 'NONE',  ( 10.81189881249999729, 0.000000000000000000, -173.8437500020484094 ) ) ;
#12608 = CARTESIAN_POINT ( 'NONE',  ( -10.81189881249999729, 1.324075727343319199E-15, -158.0937500020483810 ) ) ;
#12610 = ADVANCED_FACE ( 'NONE', ( #7084 ), #30814, .T. ) ;
#12609 = CARTESIAN_POINT ( 'NONE',  ( -10.81189881249999729, 6.242252689847871849, -173.2187500020483810 ) ) ;
#12611 = CARTESIAN_POINT ( 'NONE',  ( -10.00000000000051337, 5.773502691895962435, -124.3749999999999858 ) ) ;
#12612 = CARTESIAN_POINT ( 'NONE',  ( -2.121150477449813534E-15, -11.54700538379251284, -24.87499999999998934 ) ) ;
#12613 = CARTESIAN_POINT ( 'NONE',  ( 9.999999999999996447, -5.773502691896262640, -183.6250000000000000 ) ) ;
#12614 = CARTESIAN_POINT ( 'NONE',  ( -10.81189881249999907, -6.242252689847864744, -105.4687500020483668 ) ) ;
#12615 = CARTESIAN_POINT ( 'NONE',  ( -2.121150477449813534E-15, -11.54700538379251284, -47.75000000409676204 ) ) ;
#12616 = CARTESIAN_POINT ( 'NONE',  ( -2.293366432827344421E-15, -12.48450537969573659, -76.90625000204839523 ) ) ;
#12617 = CARTESIAN_POINT ( 'NONE',  ( 0.000000000000000000, 0.000000000000000000, -99.99999999999998579 ) ) ;
#12618 = CARTESIAN_POINT ( 'NONE',  ( -5.405949406249996869, 9.363379034771805109, -81.84375000204838102 ) ) ;
#12619 = CARTESIAN_POINT ( 'NONE',  ( -2.293366432827344421E-15, -12.48450537969573659, -58.90625000204838102 ) ) ;
#12620 = CARTESIAN_POINT ( 'NONE',  ( -4.999999999999996447, 8.660254037844387298, -147.3750000040967905 ) ) ;
#12621 = CARTESIAN_POINT ( 'NONE',  ( 5.000000000000000000, 8.660254037844385522, -126.2499999999999716 ) ) ;
#12622 = ORIENTED_EDGE ( 'NONE', *, *, #39913, .F. ) ;
#12623 = CARTESIAN_POINT ( 'NONE',  ( 10.81189881249999551, -6.242252689847874514, -145.6562500020484094 ) ) ;
#12624 = CARTESIAN_POINT ( 'NONE',  ( 5.405949406249999534, 9.363379034771803333, -154.2812500020484094 ) ) ;
#12625 = CARTESIAN_POINT ( 'NONE',  ( -10.81189881249999907, -6.242252689847864744, -194.1562500020484094 ) ) ;
#12626 = CARTESIAN_POINT ( 'NONE',  ( -5.000000000000003553, -8.660254037844383745, -38.49999999999997868 ) ) ;
#12627 = CARTESIAN_POINT ( 'NONE',  ( -10.81189881249999907, -6.242252689847864744, -90.46875000204836681 ) ) ;
#12628 = EDGE_LOOP ( 'NONE', ( #13764, #28670, #6474, #1472 ) ) ;
#12629 = CARTESIAN_POINT ( 'NONE',  ( 5.000000000000000000, 8.660254037844385522, -63.24999999999997158 ) ) ;
#12630 = CARTESIAN_POINT ( 'NONE',  ( 10.81189881249999729, 0.000000000000000000, -190.3437500020484094 ) ) ;
#12631 = CARTESIAN_POINT ( 'NONE',  ( -9.999999999999998224, 5.773502691896259087, -73.75000000409676204 ) ) ;
#12632 = CYLINDRICAL_SURFACE ( 'NONE', #18972, 9.999999999999998224 ) ;
#12633 = DIRECTION ( 'NONE',  ( 0.000000000000000000, -0.9961946980917455452, -0.08715574274765837404 ) ) ;
#12634 = CARTESIAN_POINT ( 'NONE',  ( -5.405949406250003975, -9.363379034771801557, -87.53125000204838102 ) ) ;
#12635 = CARTESIAN_POINT ( 'NONE',  ( 5.405949406249999534, 9.363379034771803333, -64.28125000204836681 ) ) ;
#12636 =( BOUNDED_CURVE ( )  B_SPLINE_CURVE ( 2, ( #18450, #37232, #24739, #37886, #1213, #27536, #40668 ),
 .UNSPECIFIED., .F., .F. ) 
 B_SPLINE_CURVE_WITH_KNOTS ( ( 3, 2, 2, 3 ),
 ( 0.8917910447761197013, 0.8930348258706470865, 0.8942786069651743608, 0.8955223880597017461 ),
 .UNSPECIFIED. ) 
 CURVE ( )  GEOMETRIC_REPRESENTATION_ITEM ( )  RATIONAL_B_SPLINE_CURVE ( ( 0.9999999999999641398, 0.8660254037844745678, 1.000000000000000000, 0.8660254037844387076, 1.000000000000000000, 0.8660254037844148378, 1.000000000000023981 ) ) 
 REPRESENTATION_ITEM ( '' )  );
#12637 = CARTESIAN_POINT ( 'NONE',  ( 9.999999999999998224, 0.000000000000000000, -59.37500000409676204 ) ) ;
#12638 = CARTESIAN_POINT ( 'NONE',  ( -5.405949406250003975, -9.363379034771801557, -19.84375000204835615 ) ) ;
#12639 = VERTEX_POINT ( 'NONE', #11152 ) ;
#12640 = CARTESIAN_POINT ( 'NONE',  ( 5.405949406249992428, -9.363379034771808662, -193.7812500020484094 ) ) ;
#12641 = CARTESIAN_POINT ( 'NONE',  ( -5.405949406250003975, -9.363379034771801557, -12.53125000204835615 ) ) ;
#12642 = ADVANCED_FACE ( 'NONE', ( #24351 ), #40084, .T. ) ;
#12643 = CARTESIAN_POINT ( 'NONE',  ( 5.405949406249992428, -9.363379034771808662, -1.593750002048366365 ) ) ;
#12644 = CARTESIAN_POINT ( 'NONE',  ( -2.121150477449813534E-15, -11.54700538379251284, -110.7500000040967620 ) ) ;
#12645 = CARTESIAN_POINT ( 'NONE',  ( -1.040834085586084257E-14, -145.0000000000000000, 42.49999999999999289 ) ) ;
#12646 = CARTESIAN_POINT ( 'NONE',  ( 4.999999999999992006, -8.660254037844389075, -137.2499999999999716 ) ) ;
#12647 =( BOUNDED_CURVE ( )  B_SPLINE_CURVE ( 2, ( #28889, #41601, #5362, #18518, #25644, #41383, #2137 ),
 .UNSPECIFIED., .F., .F. ) 
 B_SPLINE_CURVE_WITH_KNOTS ( ( 3, 2, 2, 3 ),
 ( 0.3656716417910448325, 0.3669154228855722732, 0.3681592039800996030, 0.3694029850746270438 ),
 .UNSPECIFIED. ) 
 CURVE ( )  GEOMETRIC_REPRESENTATION_ITEM ( )  RATIONAL_B_SPLINE_CURVE ( ( 0.9999999999999940048, 0.8660254037844447028, 1.000000000000000000, 0.8660254037844387076, 1.000000000000000000, 0.8660254037844207220, 1.000000000000017986 ) ) 
 REPRESENTATION_ITEM ( '' )  );
#12648 = CARTESIAN_POINT ( 'NONE',  ( 10.00000000000000000, 5.773502691896255534, -177.3750000000000000 ) ) ;
#12649 = CARTESIAN_POINT ( 'NONE',  ( -9.999999999999998224, 1.224646799147353059E-15, -37.24999999999997868 ) ) ;
#12651 = VERTEX_POINT ( 'NONE', #7294 ) ;
#12650 = CARTESIAN_POINT ( 'NONE',  ( -5.405949406249996869, 9.363379034771805109, -98.53125000204839523 ) ) ;
#12652 = CARTESIAN_POINT ( 'NONE',  ( -10.00000000000102496, 5.773502691895664007, -37.37499999999992184 ) ) ;
#12653 = ORIENTED_EDGE ( 'NONE', *, *, #16256, .T. ) ;
#12654 = ORIENTED_EDGE ( 'NONE', *, *, #22021, .F. ) ;
#12655 = CARTESIAN_POINT ( 'NONE',  ( -5.405949406249996869, 9.363379034771805109, -38.34375000204837391 ) ) ;
#12656 = CARTESIAN_POINT ( 'NONE',  ( -10.81189881249999729, 6.242252689847871849, -29.40625000204835615 ) ) ;
#12657 = APPROVAL_STATUS ( 'not_yet_approved' ) ;
#12658 = CARTESIAN_POINT ( 'NONE',  ( -2.293366432827344421E-15, -12.48450537969573659, -78.21875000204838102 ) ) ;
#12659 = CARTESIAN_POINT ( 'NONE',  ( -5.405949406249996869, 9.363379034771805109, -198.8437500020484094 ) ) ;
#12660 = CARTESIAN_POINT ( 'NONE',  ( -4.999999999999996447, 8.660254037844387298, -124.5000000000000000 ) ) ;
#12661 = CARTESIAN_POINT ( 'NONE',  ( -4.999999999999996447, 8.660254037844387298, -49.49999999999998579 ) ) ;
#12662 = CARTESIAN_POINT ( 'NONE',  ( 7.644554776091147741E-16, 12.48450537969573659, -157.1562500020484094 ) ) ;
#12663 = CARTESIAN_POINT ( 'NONE',  ( 4.999999999999992006, -8.660254037844389075, -13.12500000409674783 ) ) ;
#12664 = CYLINDRICAL_SURFACE ( 'NONE', #561, 9.999999999999998224 ) ;
#12665 = CARTESIAN_POINT ( 'NONE',  ( -10.81189881249999907, -6.242252689847864744, -130.9687500020483810 ) ) ;
#12666 = CARTESIAN_POINT ( 'NONE',  ( -2.293366432827344421E-15, -12.48450537969573659, -94.90625000204838102 ) ) ;
#12667 = CARTESIAN_POINT ( 'NONE',  ( 5.405949406249999534, 9.363379034771803333, -110.5937500020483810 ) ) ;
#12668 = CARTESIAN_POINT ( 'NONE',  ( -2.293366432827344421E-15, -12.48450537969573659, -75.21875000204839523 ) ) ;
#12669 = CARTESIAN_POINT ( 'NONE',  ( -10.81189881249999729, 6.242252689847871849, -81.90625000204838102 ) ) ;
#12670 = CARTESIAN_POINT ( 'NONE',  ( 4.999999999999992006, -8.660254037844389075, -167.6250000040967905 ) ) ;
#12671 = CARTESIAN_POINT ( 'NONE',  ( 0.000000000000000000, 0.000000000000000000, -200.0000000000000000 ) ) ;
#12672 = CARTESIAN_POINT ( 'NONE',  ( -10.81189881249999729, -6.242252689847864744, -170.1562500020484094 ) ) ;
#12673 = CARTESIAN_POINT ( 'NONE',  ( 10.81189881249999551, -6.242252689847874514, -181.6562500020484379 ) ) ;
#12674 = CARTESIAN_POINT ( 'NONE',  ( 9.999999999999998224, 0.000000000000000000, -152.3750000040967905 ) ) ;
#12675 = CARTESIAN_POINT ( 'NONE',  ( 10.81189881249999729, 0.000000000000000000, -6.031250002048377468 ) ) ;
#12676 = CARTESIAN_POINT ( 'NONE',  ( -10.81189881249999907, -6.242252689847864744, -6.468750002048357040 ) ) ;
#12677 = CARTESIAN_POINT ( 'NONE',  ( 0.000000000000000000, 0.000000000000000000, -200.0000000000000000 ) ) ;
#12678 = CARTESIAN_POINT ( 'NONE',  ( -5.405949406249996869, 9.363379034771805109, -110.3437500020483810 ) ) ;
#12679 = CARTESIAN_POINT ( 'NONE',  ( 7.070501591499377789E-16, 11.54700538379251284, -88.62500000000000000 ) ) ;
#12680 = CARTESIAN_POINT ( 'NONE',  ( 5.405949406249999534, 9.363379034771803333, -8.781250002048352599 ) ) ;
#12681 = CARTESIAN_POINT ( 'NONE',  ( 10.00000000000000000, 5.773502691896255534, -98.25000000409677625 ) ) ;
#12682 = CARTESIAN_POINT ( 'NONE',  ( -10.00000000000051337, 5.773502691895962435, -150.2500000040967620 ) ) ;
#12683 = CARTESIAN_POINT ( 'NONE',  ( -5.405949406250003975, -9.363379034771801557, -107.0312500020483810 ) ) ;
#12684 = CARTESIAN_POINT ( 'NONE',  ( -2.293366432827344421E-15, -12.48450537969573659, -93.40625000204838102 ) ) ;
#12685 = ORIENTED_EDGE ( 'NONE', *, *, #3222, .T. ) ;
#12686 = CARTESIAN_POINT ( 'NONE',  ( -4.999999999999996447, 8.660254037844387298, -85.87500000409677625 ) ) ;
#12687 = CARTESIAN_POINT ( 'NONE',  ( -9.999999999999998224, 0.000000000000000000, -99.99999999999998579 ) ) ;
#12688 = CARTESIAN_POINT ( 'NONE',  ( -10.81189881249999907, -6.242252689847864744, -45.46875000204835970 ) ) ;
#12689 = ORIENTED_EDGE ( 'NONE', *, *, #30835, .T. ) ;
#12690 = CARTESIAN_POINT ( 'NONE',  ( -2.121150477449813534E-15, -11.54700538379251284, -17.37499999999997158 ) ) ;
#12691 = EDGE_CURVE ( 'NONE', #270, #7415, #1797, .T. ) ;
#12692 = CARTESIAN_POINT ( 'NONE',  ( -10.00000000000000000, -5.773502691896251982, -157.1250000000000284 ) ) ;
#12693 = CARTESIAN_POINT ( 'NONE',  ( -9.999999999999998224, 5.773502691896259087, -21.25000000409676915 ) ) ;
#12694 = EDGE_CURVE ( 'NONE', #25687, #26580, #8963, .T. ) ;
#12695 = CARTESIAN_POINT ( 'NONE',  ( -9.999999999999998224, 0.000000000000000000, -99.99999999999998579 ) ) ;
#12697 = ORIENTED_EDGE ( 'NONE', *, *, #30302, .F. ) ;
#12696 = CARTESIAN_POINT ( 'NONE',  ( -10.81189881249999729, 1.324075727343319199E-15, -122.2812500020483952 ) ) ;
#12698 = CARTESIAN_POINT ( 'NONE',  ( -9.999999999998969713, -5.773502691896847949, -22.12499999999995026 ) ) ;
#12699 = VERTEX_POINT ( 'NONE', #34912 ) ;
#12700 = CARTESIAN_POINT ( 'NONE',  ( 7.644554776091147741E-16, 12.48450537969573659, -55.15625000204837391 ) ) ;
#12701 = APPROVAL_DATE_TIME ( #29139, #12231 ) ;
#12702 = CARTESIAN_POINT ( 'NONE',  ( 5.405949406249992428, -9.363379034771808662, -103.5937500020483668 ) ) ;
#12704 = ORIENTED_EDGE ( 'NONE', *, *, #3546, .F. ) ;
#12703 = ORIENTED_EDGE ( 'NONE', *, *, #36279, .T. ) ;
#12705 = CARTESIAN_POINT ( 'NONE',  ( -9.999999999999998224, 1.224646799147353059E-15, -185.7500000000000000 ) ) ;
#12706 = CARTESIAN_POINT ( 'NONE',  ( -7.071067811865472841, -7.071067811865472841, -200.0000000000000000 ) ) ;
#12707 = CARTESIAN_POINT ( 'NONE',  ( -10.81189881249999907, -6.242252689847864744, -183.6562500020483810 ) ) ;
#12708 = CARTESIAN_POINT ( 'NONE',  ( -9.999999999999998224, 1.224646799147353059E-15, -174.1250000040968189 ) ) ;
#12709 = CARTESIAN_POINT ( 'NONE',  ( 9.999999999999998224, 0.000000000000000000, -161.3750000040967905 ) ) ;
#12710 = CARTESIAN_POINT ( 'NONE',  ( -5.405949406249996869, 9.363379034771805109, -137.3437500020484094 ) ) ;
#12711 =( BOUNDED_CURVE ( )  B_SPLINE_CURVE ( 2, ( #36467, #26549, #39697, #15961, #22461, #25915, #39489 ),
 .UNSPECIFIED., .F., .F. ) 
 B_SPLINE_CURVE_WITH_KNOTS ( ( 3, 2, 2, 3 ),
 ( 0.5186567164179105571, 0.5199004975124379424, 0.5211442786069653277, 0.5223880597014926019 ),
 .UNSPECIFIED. ) 
 CURVE ( )  GEOMETRIC_REPRESENTATION_ITEM ( )  RATIONAL_B_SPLINE_CURVE ( ( 0.9999999999999880096, 0.8660254037844506980, 1.000000000000000000, 0.8660254037844387076, 1.000000000000000000, 0.8660254037844267172, 1.000000000000011990 ) ) 
 REPRESENTATION_ITEM ( '' )  );
#12712 = CARTESIAN_POINT ( 'NONE',  ( -10.81189881249999729, 6.242252689847871849, -104.2187500020483810 ) ) ;
#12713 = DIRECTION ( 'NONE',  ( 1.000000000000000000, 0.000000000000000000, -0.000000000000000000 ) ) ;
#12714 = CARTESIAN_POINT ( 'NONE',  ( -10.81189881249999729, 1.324075727343319199E-15, -111.7812500020483810 ) ) ;
#12715 = CARTESIAN_POINT ( 'NONE',  ( -10.00000000000000000, -5.773502691896251982, -190.5000000040967905 ) ) ;
#12716 = CARTESIAN_POINT ( 'NONE',  ( 10.81189881249999729, 6.242252689847867408, -124.2187500020483952 ) ) ;
#12717 = CARTESIAN_POINT ( 'NONE',  ( 5.405949406249992428, -9.363379034771808662, -184.7812500020484094 ) ) ;
#12718 = AXIS2_PLACEMENT_3D ( 'NONE', #21678, #8316, #37442 ) ;
#12719 = CARTESIAN_POINT ( 'NONE',  ( -9.999999999999998224, 5.773502691896259087, -137.8750000000000000 ) ) ;
#12720 = CARTESIAN_POINT ( 'NONE',  ( 9.999999999999996447, -5.773502691896262640, -6.624999999999964473 ) ) ;
#12721 = CARTESIAN_POINT ( 'NONE',  ( 10.81189881249999729, 6.242252689847867408, -71.71875000204836681 ) ) ;
#12722 = CARTESIAN_POINT ( 'NONE',  ( -5.405949406250003975, -9.363379034771801557, -49.84375000204838102 ) ) ;
#12723 = UNCERTAINTY_MEASURE_WITH_UNIT (LENGTH_MEASURE( 1.000000000000000082E-05 ), #35513, 'distance_accuracy_value', 'NONE');
#12724 = CARTESIAN_POINT ( 'NONE',  ( -10.00000000000000000, -5.773502691896251982, -177.0000000040967620 ) ) ;
#12725 = CARTESIAN_POINT ( 'NONE',  ( -2.293366432827344421E-15, -12.48450537969573659, -25.90625000204838813 ) ) ;
#12726 = CARTESIAN_POINT ( 'NONE',  ( -10.81189881249999729, 6.242252689847871849, -27.71875000204837391 ) ) ;
#12727 = CARTESIAN_POINT ( 'NONE',  ( 5.000000000000000000, 8.660254037844385522, -27.62500000409676204 ) ) ;
#12728 = CARTESIAN_POINT ( 'NONE',  ( -2.293366432827344421E-15, -12.48450537969573659, -138.2187500020483810 ) ) ;
#12729 = CARTESIAN_POINT ( 'NONE',  ( -9.999999999999998224, 5.773502691896259087, -116.8750000000000000 ) ) ;
#12730 = CARTESIAN_POINT ( 'NONE',  ( -9.999999999999998224, 1.224646799147353059E-15, -163.2500000000000000 ) ) ;
#12731 = CARTESIAN_POINT ( 'NONE',  ( 10.00000000000000000, 5.773502691896255534, -70.87499999999998579 ) ) ;
#12732 = CARTESIAN_POINT ( 'NONE',  ( 10.81189881249999907, 6.242252689847868297, -128.9062500020483810 ) ) ;
#12733 = CARTESIAN_POINT ( 'NONE',  ( -5.405949406249996869, 9.363379034771805109, -118.0312500020483952 ) ) ;
#12734 = VERTEX_POINT ( 'NONE', #8787 ) ;
#12735 = CARTESIAN_POINT ( 'NONE',  ( 9.999999999999998224, 0.000000000000000000, -122.0000000000000000 ) ) ;
#12736 = CARTESIAN_POINT ( 'NONE',  ( -5.000000000000003553, -8.660254037844383745, -119.8750000040967905 ) ) ;
#12737 = CARTESIAN_POINT ( 'NONE',  ( -9.999999999999998224, 1.224646799147353059E-15, -169.2500000000000000 ) ) ;
#12738 = CARTESIAN_POINT ( 'NONE',  ( 7.644554776091147741E-16, 12.48450537969573659, -66.96875000204838102 ) ) ;
#12739 = VERTEX_POINT ( 'NONE', #5123 ) ;
#12740 = CARTESIAN_POINT ( 'NONE',  ( 10.00000000000000000, 5.773502691896255534, -45.37499999999997158 ) ) ;
#12741 = CARTESIAN_POINT ( 'NONE',  ( 9.999999999999996447, -5.773502691896262640, -16.00000000409677270 ) ) ;
#12742 = EDGE_CURVE ( 'NONE', #32685, #12182, #24561, .T. ) ;
#12743 = CARTESIAN_POINT ( 'NONE',  ( 7.644554776091147741E-16, 12.48450537969573659, -46.15625000204837391 ) ) ;
#12744 = DIRECTION ( 'NONE',  ( -0.000000000000000000, 1.000000000000000000, -0.000000000000000000 ) ) ;
#12745 = CARTESIAN_POINT ( 'NONE',  ( 10.00000000000000000, 5.773502691896255534, -44.25000000409676204 ) ) ;
#12746 = CARTESIAN_POINT ( 'NONE',  ( -5.405949406249996869, 9.363379034771805109, -32.53125000204837391 ) ) ;
#12747 = AXIS2_PLACEMENT_3D ( 'NONE', #41976, #9399, #35532 ) ;
#12748 = EDGE_CURVE ( 'NONE', #33637, #8113, #14729, .T. ) ;
#12749 = DIRECTION ( 'NONE',  ( -0.000000000000000000, -0.000000000000000000, -1.000000000000000000 ) ) ;
#12750 = CARTESIAN_POINT ( 'NONE',  ( 7.644554776091147741E-16, 12.48450537969573659, -139.1562500020483810 ) ) ;
#12751 = ADVANCED_FACE ( 'NONE', ( #31677 ), #21300, .F. ) ;
#12752 = CARTESIAN_POINT ( 'NONE',  ( -10.81189881249999729, 1.324075727343319199E-15, -146.2812500020483810 ) ) ;
#12753 = CC_DESIGN_DATE_AND_TIME_ASSIGNMENT ( #38634, #18989, ( #27668 ) ) ;
#12754 = CARTESIAN_POINT ( 'NONE',  ( -5.000000000000003553, -8.660254037844383745, -15.99999999999995914 ) ) ;
#12755 = ORIENTED_EDGE ( 'NONE', *, *, #3158, .F. ) ;
#12756 = AXIS2_PLACEMENT_3D ( 'NONE', #27241, #4372, #30284 ) ;
#12757 = EDGE_LOOP ( 'NONE', ( #16677, #38454 ) ) ;
#12758 = PRODUCT_DEFINITION_SHAPE ( 'NONE', 'NONE',  #42695 ) ;
#12759 = ORIENTED_EDGE ( 'NONE', *, *, #30711, .F. ) ;
#12760 = EDGE_CURVE ( 'NONE', #23937, #42482, #35502, .T. ) ;
#12761 = CARTESIAN_POINT ( 'NONE',  ( 9.999999999999998224, 0.000000000000000000, -120.5000000000000000 ) ) ;
#12762 =( BOUNDED_CURVE ( )  B_SPLINE_CURVE ( 2, ( #20099, #13185, #16635, #29195, #33292, #3718, #29837 ),
 .UNSPECIFIED., .F., .F. ) 
 B_SPLINE_CURVE_WITH_KNOTS ( ( 3, 2, 2, 3 ),
 ( 0.2686567164179105571, 0.2699004975124379424, 0.2711442786069652722, 0.2723880597014926574 ),
 .UNSPECIFIED. ) 
 CURVE ( )  GEOMETRIC_REPRESENTATION_ITEM ( )  RATIONAL_B_SPLINE_CURVE ( ( 0.9999999999999880096, 0.8660254037844506980, 1.000000000000000000, 0.8660254037844387076, 1.000000000000000000, 0.8660254037844267172, 1.000000000000011990 ) ) 
 REPRESENTATION_ITEM ( '' )  );
#12763 = CARTESIAN_POINT ( 'NONE',  ( -10.81189881249999907, -6.242252689847864744, -174.4687500020484094 ) ) ;
#12764 = CARTESIAN_POINT ( 'NONE',  ( 10.81189881249999729, 0.000000000000000000, -19.34375000204835260 ) ) ;
#12765 = LINE ( 'NONE', #6318, #12245 ) ;
#12766 = CARTESIAN_POINT ( 'NONE',  ( -10.81189881249999729, 6.242252689847871849, -162.7187500020483810 ) ) ;
#12767 = CARTESIAN_POINT ( 'NONE',  ( 10.81189881249999907, 6.242252689847868297, -145.2187500020484094 ) ) ;
#12768 = DIRECTION ( 'NONE',  ( 0.000000000000000000, 0.000000000000000000, -1.000000000000000000 ) ) ;
#12769 = CARTESIAN_POINT ( 'NONE',  ( -10.81189881249999907, -6.242252689847864744, -124.9687500020483810 ) ) ;
#12770 = VECTOR ( 'NONE', #23771, 1000.000000000000000 ) ;
#12771 = CARTESIAN_POINT ( 'NONE',  ( 10.81189881249999551, -6.242252689847874514, -130.6562500020484094 ) ) ;
#12772 = CARTESIAN_POINT ( 'NONE',  ( 10.81189881249999729, 0.000000000000000000, -19.34375000204835260 ) ) ;
#12773 = CARTESIAN_POINT ( 'NONE',  ( -5.405949406250003975, -9.363379034771801557, -145.8437500020483810 ) ) ;
#12774 = CARTESIAN_POINT ( 'NONE',  ( 9.415087197078790382, -5.361960122183175415, -179.9999999999999432 ) ) ;
#12775 = AXIS2_PLACEMENT_3D ( 'NONE', #24574, #4922, #37722 ) ;
#12776 = CARTESIAN_POINT ( 'NONE',  ( -9.999999999999998224, 1.224646799147353059E-15, -43.62500000409677625 ) ) ;
#12777 = CARTESIAN_POINT ( 'NONE',  ( -2.121150477449813534E-15, -11.54700538379251284, -162.8750000000000000 ) ) ;
#12778 = CARTESIAN_POINT ( 'NONE',  ( -5.405949406249996869, 9.363379034771805109, -1.031250002048372805 ) ) ;
#12779 = CARTESIAN_POINT ( 'NONE',  ( 10.81189881249999729, 0.000000000000000000, -74.84375000204838102 ) ) ;
#12780 = CARTESIAN_POINT ( 'NONE',  ( 5.405949406249999534, 9.363379034771803333, -47.78125000204838813 ) ) ;
#12781 = CARTESIAN_POINT ( 'NONE',  ( -2.293366432827344421E-15, -12.48450537969573659, -52.71875000204837391 ) ) ;
#12782 = CARTESIAN_POINT ( 'NONE',  ( 9.999999999999479527, 5.773502691896553074, -90.75000000409674783 ) ) ;
#12783 = CARTESIAN_POINT ( 'NONE',  ( -10.81189881249999729, 1.324075727343319199E-15, -165.5937500020484094 ) ) ;
#12784 = CARTESIAN_POINT ( 'NONE',  ( 5.000000000000000000, 8.660254037844385522, -139.7499999999999716 ) ) ;
#12785 = VECTOR ( 'NONE', #21593, 1000.000000000000000 ) ;
#12786 = CARTESIAN_POINT ( 'NONE',  ( -5.405949406249996869, 9.363379034771805109, -149.5312500020483810 ) ) ;
#12787 = CARTESIAN_POINT ( 'NONE',  ( 9.999999999999998224, 1.224646799147353059E-15, -99.99999999999998579 ) ) ;
#12788 = CARTESIAN_POINT ( 'NONE',  ( -10.00000000000000000, -5.773502691896251982, -111.0000000040967763 ) ) ;
#12789 = CARTESIAN_POINT ( 'NONE',  ( 9.999999999999998224, 0.000000000000000000, -94.99999999999998579 ) ) ;
#12790 = ORIENTED_EDGE ( 'NONE', *, *, #14180, .F. ) ;
#12791 = CARTESIAN_POINT ( 'NONE',  ( -10.81189881249999729, 6.242252689847871849, -117.9062500020483952 ) ) ;
#12792 = CARTESIAN_POINT ( 'NONE',  ( 5.000000000000000000, 8.660254037844385522, -138.6250000040967905 ) ) ;
#12793 = CARTESIAN_POINT ( 'NONE',  ( -9.999999999999998224, 1.224646799147353059E-15, -52.24999999999996447 ) ) ;
#12794 = CARTESIAN_POINT ( 'NONE',  ( 10.81189881249999729, 0.000000000000000000, -172.5312500020484094 ) ) ;
#12795 = CARTESIAN_POINT ( 'NONE',  ( -10.00000000000000000, -5.773502691896251982, -54.00000000409676915 ) ) ;
#12796 = FACE_OUTER_BOUND ( 'NONE', #41376, .T. ) ;
#12797 = CARTESIAN_POINT ( 'NONE',  ( -10.81189881249999729, 6.242252689847871849, -57.90625000204838813 ) ) ;
#12798 = PLANE ( 'NONE',  #6265 ) ;
#12799 = CARTESIAN_POINT ( 'NONE',  ( 5.405949406249992428, -9.363379034771808662, -157.7812500020484094 ) ) ;
#12800 = CARTESIAN_POINT ( 'NONE',  ( -5.405949406250003975, -9.363379034771801557, -142.8437500020483810 ) ) ;
#12801 = CARTESIAN_POINT ( 'NONE',  ( -10.00000000000051337, 5.773502691895962435, -100.3750000000000000 ) ) ;
#12802 = CARTESIAN_POINT ( 'NONE',  ( 9.999999999999998224, 0.000000000000000000, -177.5000000000000000 ) ) ;
#12803 = VERTEX_POINT ( 'NONE', #21944 ) ;
#12804 = CARTESIAN_POINT ( 'NONE',  ( -10.00000000000019185, 5.773502691896147176, -189.2500000040968189 ) ) ;
#12805 = VECTOR ( 'NONE', #13720, 1000.000000000000000 ) ;
#12806 = EDGE_CURVE ( 'NONE', #35300, #41736, #22603, .T. ) ;
#12808 = EDGE_LOOP ( 'NONE', ( #13955, #20092, #12580, #29190 ) ) ;
#12807 = CARTESIAN_POINT ( 'NONE',  ( -2.293366432827344421E-15, -12.48450537969573659, -67.90625000204840944 ) ) ;
#12809 = APPROVAL_STATUS ( 'not_yet_approved' ) ;
#12811 = ORIENTED_EDGE ( 'NONE', *, *, #4462, .T. ) ;
#12810 = CARTESIAN_POINT ( 'NONE',  ( 5.405949406249999534, 9.363379034771803333, -121.0937500020483952 ) ) ;
#12812 = ORIENTED_EDGE ( 'NONE', *, *, #31197, .T. ) ;
#12813 = CARTESIAN_POINT ( 'NONE',  ( 10.81189881249999729, 6.242252689847867408, -28.21875000204838813 ) ) ;
#12814 = FACE_OUTER_BOUND ( 'NONE', #52, .T. ) ;
#12815 = CARTESIAN_POINT ( 'NONE',  ( -5.405949406249996869, 9.363379034771805109, -195.8437500020484094 ) ) ;
#12816 = SHAPE_REPRESENTATION ( 'adapter', ( #39998 ), #11785 ) ;
#12817 = CARTESIAN_POINT ( 'NONE',  ( -10.81189881249999729, 1.324075727343319199E-15, -57.59375000204835970 ) ) ;
#12818 = DIRECTION ( 'NONE',  ( -0.000000000000000000, -0.000000000000000000, 1.000000000000000000 ) ) ;
#12819 = CARTESIAN_POINT ( 'NONE',  ( -5.000000000000003553, -8.660254037844383745, -24.99999999999996803 ) ) ;
#12820 = CARTESIAN_POINT ( 'NONE',  ( 10.81189881249999729, 0.000000000000000000, -191.8437500020484094 ) ) ;
#12821 = CARTESIAN_POINT ( 'NONE',  ( -5.405949406249996869, 9.363379034771805109, -168.8437500020484094 ) ) ;
#12822 = CARTESIAN_POINT ( 'NONE',  ( 7.644554776091147741E-16, 12.48450537969573659, -146.4687500020484094 ) ) ;
#12823 = CARTESIAN_POINT ( 'NONE',  ( 10.81189881249999729, 6.242252689847867408, -173.7187500020483810 ) ) ;
#12824 = CARTESIAN_POINT ( 'NONE',  ( 9.999999999999998224, 0.000000000000000000, -177.8750000040967905 ) ) ;
#12825 = CARTESIAN_POINT ( 'NONE',  ( 4.999999999999992006, -8.660254037844389075, -161.6250000040967905 ) ) ;
#12826 = CARTESIAN_POINT ( 'NONE',  ( 9.999999999999998224, 0.000000000000000000, -186.5000000000000000 ) ) ;
#12827 = CARTESIAN_POINT ( 'NONE',  ( 7.644554776091147741E-16, 12.48450537969573659, -93.96875000204838102 ) ) ;
#12828 = CARTESIAN_POINT ( 'NONE',  ( -2.121150477449813534E-15, -11.54700538379251284, -84.87500000000000000 ) ) ;
#12829 = CARTESIAN_POINT ( 'NONE',  ( 10.81189881249999551, -6.242252689847874514, -72.15625000204836681 ) ) ;
#12830 = CARTESIAN_POINT ( 'NONE',  ( 9.999999999999998224, 0.000000000000000000, -198.5000000000000000 ) ) ;
#12831 = CARTESIAN_POINT ( 'NONE',  ( -10.81189881249999729, 1.324075727343319199E-15, -188.0937500020483810 ) ) ;
#12832 = CARTESIAN_POINT ( 'NONE',  ( 7.644554776091147741E-16, 12.48450537969573659, -83.46875000204838102 ) ) ;
#12833 = VECTOR ( 'NONE', #2094, 1000.000000000000000 ) ;
#12834 = CARTESIAN_POINT ( 'NONE',  ( 10.81189881249999551, -6.242252689847874514, -57.15625000204837391 ) ) ;
#12835 = CARTESIAN_POINT ( 'NONE',  ( -9.999999999999998224, 5.773502691896259087, -147.2500000040967905 ) ) ;
#12836 = CARTESIAN_POINT ( 'NONE',  ( -4.999999999999996447, 8.660254037844387298, -113.9999999999999858 ) ) ;
#12837 = ORIENTED_EDGE ( 'NONE', *, *, #13221, .T. ) ;
#12838 = CARTESIAN_POINT ( 'NONE',  ( -5.405949406249996869, 9.363379034771805109, -140.5312500020484094 ) ) ;
#12839 = CARTESIAN_POINT ( 'NONE',  ( 10.81189881249999729, 0.000000000000000000, -153.0312500020484094 ) ) ;
#12840 = CARTESIAN_POINT ( 'NONE',  ( -5.405949406250003975, -9.363379034771801557, -197.0312500020484094 ) ) ;
#12841 = CARTESIAN_POINT ( 'NONE',  ( -9.999999999998456346, -5.773502691897145489, -52.12499999999994316 ) ) ;
#12842 = CARTESIAN_POINT ( 'NONE',  ( 5.405949406249999534, 9.363379034771803333, -94.09375000204838102 ) ) ;
#12843 = ORIENTED_EDGE ( 'NONE', *, *, #25949, .T. ) ;
#12844 = CARTESIAN_POINT ( 'NONE',  ( 7.070501591499377789E-16, 11.54700538379251284, -58.62499999999998579 ) ) ;
#12845 = CARTESIAN_POINT ( 'NONE',  ( 5.405949406249992428, -9.363379034771808662, -190.5937500020484094 ) ) ;
#12846 = CARTESIAN_POINT ( 'NONE',  ( -9.999999999999998224, 5.773502691896259087, -76.75000000409676204 ) ) ;
#12847 = DIRECTION ( 'NONE',  ( -0.000000000000000000, -0.000000000000000000, -1.000000000000000000 ) ) ;
#12848 = DIRECTION ( 'NONE',  ( 1.000000000000000000, 0.000000000000000000, 0.000000000000000000 ) ) ;
#12849 = CARTESIAN_POINT ( 'NONE',  ( -10.81189881249999729, 1.324075727343319199E-15, -84.78125000204838102 ) ) ;
#12850 = CARTESIAN_POINT ( 'NONE',  ( -10.81189881249999729, 6.242252689847871849, -65.40625000204839523 ) ) ;
#12851 = CARTESIAN_POINT ( 'NONE',  ( 4.999999999999992006, -8.660254037844389075, -58.12500000409676204 ) ) ;
#12852 = CARTESIAN_POINT ( 'NONE',  ( -10.81189881249999729, 6.242252689847871849, -21.71875000204837036 ) ) ;
#12853 = DIRECTION ( 'NONE',  ( -0.000000000000000000, -0.000000000000000000, -1.000000000000000000 ) ) ;
#12854 = CARTESIAN_POINT ( 'NONE',  ( 10.81189881249999551, -6.242252689847874514, -181.6562500020484379 ) ) ;
#12855 = CARTESIAN_POINT ( 'NONE',  ( -10.81189881249999907, -6.242252689847864744, -9.656250002048366810 ) ) ;
#12856 = CARTESIAN_POINT ( 'NONE',  ( -10.00000000000000000, -5.773502691896252870, -172.5000000040967905 ) ) ;
#12857 = CARTESIAN_POINT ( 'NONE',  ( 9.999999999999998224, 0.000000000000000000, -152.0000000000000000 ) ) ;
#12858 = CARTESIAN_POINT ( 'NONE',  ( -9.999999999999998224, 1.224646799147353059E-15, -137.7499999999999716 ) ) ;
#12859 = CARTESIAN_POINT ( 'NONE',  ( -4.999999999999996447, 8.660254037844387298, -178.5000000000000000 ) ) ;
#12860 = CARTESIAN_POINT ( 'NONE',  ( -10.00000000000102496, 5.773502691895664007, -1.374999999999948486 ) ) ;
#12862 = ORIENTED_EDGE ( 'NONE', *, *, #2974, .T. ) ;
#12861 = CARTESIAN_POINT ( 'NONE',  ( -5.405949406250003975, -9.363379034771801557, -93.53125000204838102 ) ) ;
#12863 = CARTESIAN_POINT ( 'NONE',  ( 9.999999999999998224, 0.000000000000000000, -200.0000000000000000 ) ) ;
#12864 = ORIENTED_EDGE ( 'NONE', *, *, #27809, .T. ) ;
#12865 = VERTEX_POINT ( 'NONE', #12216 ) ;
#12866 = CARTESIAN_POINT ( 'NONE',  ( -10.81189881249999729, 6.242252689847871849, -36.71875000204835970 ) ) ;
#12867 = CARTESIAN_POINT ( 'NONE',  ( -5.405949406250003975, -9.363379034771801557, -33.53125000204837391 ) ) ;
#12868 = SHAPE_DEFINITION_REPRESENTATION ( #33876, #31964 ) ;
#12869 = CARTESIAN_POINT ( 'NONE',  ( 10.81189881249999907, 6.242252689847868297, -79.21875000204838102 ) ) ;
#12870 = CARTESIAN_POINT ( 'NONE',  ( 10.00000000000102318, -5.773502691895667560, -83.50000000409673362 ) ) ;
#12871 = CARTESIAN_POINT ( 'NONE',  ( -10.81189881249999729, 1.324075727343319199E-15, -195.5937500020484094 ) ) ;
#12872 = ADVANCED_FACE ( 'NONE', ( #34274 ), #42625, .T. ) ;
#12873 = CYLINDRICAL_SURFACE ( 'NONE', #7450, 9.750000000000003553 ) ;
#12874 = CARTESIAN_POINT ( 'NONE',  ( 9.999999999999227285, 5.773502691896701400, -112.8749999999999716 ) ) ;
#12875 = CARTESIAN_POINT ( 'NONE',  ( 5.405949406249999534, 9.363379034771803333, -154.2812500020484094 ) ) ;
#12876 = CARTESIAN_POINT ( 'NONE',  ( -10.00000000000000000, -5.773502691896251982, -13.50000000409675849 ) ) ;
#12877 = CARTESIAN_POINT ( 'NONE',  ( 5.000000000000000000, 8.660254037844385522, -121.7500000000000000 ) ) ;
#12878 = CARTESIAN_POINT ( 'NONE',  ( 10.81189881249999907, 6.242252689847868297, -128.7187500020483810 ) ) ;
#12879 = CARTESIAN_POINT ( 'NONE',  ( 10.81189881249999551, -6.242252689847874514, -102.1562500020483952 ) ) ;
#12880 = CARTESIAN_POINT ( 'NONE',  ( -10.81189881249999729, 6.242252689847871849, -108.7187500020483810 ) ) ;
#12881 = CARTESIAN_POINT ( 'NONE',  ( 5.405949406249992428, -9.363379034771808662, -81.09375000204838102 ) ) ;
#12882 = CARTESIAN_POINT ( 'NONE',  ( 10.81189881249999729, 0.000000000000000000, -82.53125000204838102 ) ) ;
#12883 = CARTESIAN_POINT ( 'NONE',  ( -10.00000000000000000, -5.773502691896251982, -171.0000000040967905 ) ) ;
#12884 =( BOUNDED_CURVE ( )  B_SPLINE_CURVE ( 2, ( #24035, #1803, #28129, #20992, #33964, #4385, #30725 ),
 .UNSPECIFIED., .F., .F. ) 
 B_SPLINE_CURVE_WITH_KNOTS ( ( 3, 2, 2, 3 ),
 ( 0.1641791044776119424, 0.1654228855721392999, 0.1666666666666666574, 0.1679104477611940427 ),
 .UNSPECIFIED. ) 
 CURVE ( )  GEOMETRIC_REPRESENTATION_ITEM ( )  RATIONAL_B_SPLINE_CURVE ( ( 1.000000000000000000, 0.8660254037844387076, 1.000000000000000000, 0.8660254037844387076, 1.000000000000000000, 0.8660254037844387076, 1.000000000000000000 ) ) 
 REPRESENTATION_ITEM ( '' )  );
#12885 = CYLINDRICAL_SURFACE ( 'NONE', #41985, 9.999999999999998224 ) ;
#12886 = CARTESIAN_POINT ( 'NONE',  ( -10.81189881249999729, 1.324075727343319199E-15, -164.2812500020484094 ) ) ;
#12887 = CARTESIAN_POINT ( 'NONE',  ( -10.81189881249999729, 6.242252689847871849, -179.4062500020484094 ) ) ;
#12888 = CARTESIAN_POINT ( 'NONE',  ( 9.999999999999996447, -5.773502691896262640, -157.0000000040968189 ) ) ;
#12889 = CARTESIAN_POINT ( 'NONE',  ( -9.999999999999998224, 1.224646799147353059E-15, -178.2500000000000284 ) ) ;
#12890 = CARTESIAN_POINT ( 'NONE',  ( -10.81189881249999729, 1.324075727343319199E-15, -9.593750002048345493 ) ) ;
#12891 = CARTESIAN_POINT ( 'NONE',  ( 9.999999999999998224, 0.000000000000000000, -128.0000000000000000 ) ) ;
#12892 = CARTESIAN_POINT ( 'NONE',  ( -5.405949406250003975, -9.363379034771801557, -114.3437500020483810 ) ) ;
#12893 = CARTESIAN_POINT ( 'NONE',  ( 5.000000000000000000, 8.660254037844385522, -79.74999999999998579 ) ) ;
#12894 = CARTESIAN_POINT ( 'NONE',  ( -5.405949406250003975, -9.363379034771801557, -12.53125000204835615 ) ) ;
#12895 = CARTESIAN_POINT ( 'NONE',  ( -9.999999999999998224, 1.224646799147353059E-15, -100.6250000040967905 ) ) ;
#12896 = CARTESIAN_POINT ( 'NONE',  ( 10.81189881249999551, -6.242252689847874514, -109.6562500020483810 ) ) ;
#12897 = CARTESIAN_POINT ( 'NONE',  ( 5.405949406249999534, 9.363379034771803333, -94.28125000204838102 ) ) ;
#12898 = VERTEX_POINT ( 'NONE', #5765 ) ;
#12899 = CARTESIAN_POINT ( 'NONE',  ( -9.999999999999998224, 5.773502691896259087, -85.75000000409676204 ) ) ;
#12900 = CARTESIAN_POINT ( 'NONE',  ( 5.000000000000000000, 8.660254037844385522, -146.1250000040967905 ) ) ;
#12901 = CARTESIAN_POINT ( 'NONE',  ( 7.644554776091147741E-16, 12.48450537969573659, -38.46875000204835260 ) ) ;
#12902 = ORIENTED_EDGE ( 'NONE', *, *, #32403, .F. ) ;
#12903 = CARTESIAN_POINT ( 'NONE',  ( 7.070501591499377789E-16, 11.54700538379251284, -18.12499999999997513 ) ) ;
#12904 = CARTESIAN_POINT ( 'NONE',  ( 9.999999999999998224, 0.000000000000000000, -153.5000000000000000 ) ) ;
#12905 = CARTESIAN_POINT ( 'NONE',  ( -4.999999999999996447, 8.660254037844387298, -9.375000004096744277 ) ) ;
#12906 = CARTESIAN_POINT ( 'NONE',  ( -2.121150477449813534E-15, -11.54700538379251284, -198.8750000000000284 ) ) ;
#12908 = ORIENTED_EDGE ( 'NONE', *, *, #13545, .T. ) ;
#12907 = CARTESIAN_POINT ( 'NONE',  ( -2.293366432827344421E-15, -12.48450537969573659, -118.9062500020483952 ) ) ;
#12909 = CIRCLE ( 'NONE', #19152, 20.00000000000000355 ) ;
#12910 = CARTESIAN_POINT ( 'NONE',  ( 7.070501591499376803E-16, 11.54700538379251284, -117.5000000040967905 ) ) ;
#12911 = ORIENTED_EDGE ( 'NONE', *, *, #28516, .T. ) ;
#12912 = CARTESIAN_POINT ( 'NONE',  ( -10.81189881249999907, -6.242252689847864744, -57.65625000204838102 ) ) ;
#12913 = PERSON_AND_ORGANIZATION ( #11915, #17965 ) ;
#12914 = CARTESIAN_POINT ( 'NONE',  ( -10.81189881249999729, 6.242252689847871849, -99.71875000204839523 ) ) ;
#12915 = ORIENTED_EDGE ( 'NONE', *, *, #1201, .T. ) ;
#12916 = CARTESIAN_POINT ( 'NONE',  ( -4.999999999999996447, 8.660254037844387298, -51.37500000409675494 ) ) ;
#12917 = CARTESIAN_POINT ( 'NONE',  ( 9.999999999999998224, 0.000000000000000000, -54.49999999999996447 ) ) ;
#12918 = CARTESIAN_POINT ( 'NONE',  ( 7.644554776091147741E-16, 12.48450537969573659, -176.6562500020484094 ) ) ;
#12919 = CARTESIAN_POINT ( 'NONE',  ( 5.405949406249992428, -9.363379034771808662, -3.093750002048367698 ) ) ;
#12920 = CARTESIAN_POINT ( 'NONE',  ( -5.000000000000003553, -8.660254037844383745, -146.8750000040967905 ) ) ;
#12921 = EDGE_CURVE ( 'NONE', #22119, #7656, #33800, .T. ) ;
#12922 = CARTESIAN_POINT ( 'NONE',  ( 5.405949406249999534, 9.363379034771803333, -134.5937500020483810 ) ) ;
#12923 = CARTESIAN_POINT ( 'NONE',  ( -10.81189881249999729, 6.242252689847871849, -105.7187500020483668 ) ) ;
#12924 = LINE ( 'NONE', #14, #14574 ) ;
#12925 = CARTESIAN_POINT ( 'NONE',  ( 7.644554776091147741E-16, 12.48450537969573659, -110.6562500020483952 ) ) ;
#12926 = CARTESIAN_POINT ( 'NONE',  ( -4.999999999999996447, 8.660254037844387298, -195.3750000040967905 ) ) ;
#12927 = CARTESIAN_POINT ( 'NONE',  ( -10.81189881249999729, 1.324075727343319199E-15, -116.0937500020483810 ) ) ;
#12928 = CARTESIAN_POINT ( 'NONE',  ( -10.81189881249999729, -6.242252689847864744, -188.1562500020484094 ) ) ;
#12929 = CARTESIAN_POINT ( 'NONE',  ( 9.999999999999998224, 0.000000000000000000, -185.3750000040967905 ) ) ;
#12930 = CARTESIAN_POINT ( 'NONE',  ( -9.999999999999998224, 5.773502691896259087, -142.3750000000000000 ) ) ;
#12931 = CARTESIAN_POINT ( 'NONE',  ( 9.999999999999996447, -5.773502691896262640, -3.624999999999961364 ) ) ;
#12932 = CARTESIAN_POINT ( 'NONE',  ( 10.81189881249999551, -6.242252689847874514, -56.96875000204838102 ) ) ;
#12933 = CARTESIAN_POINT ( 'NONE',  ( 5.405949406249992428, -9.363379034771808662, -48.09375000204838102 ) ) ;
#12934 = CARTESIAN_POINT ( 'NONE',  ( -2.121150477449813534E-15, -11.54700538379251284, -182.7500000040967905 ) ) ;
#12935 = CARTESIAN_POINT ( 'NONE',  ( -10.81189881249999729, 6.242252689847871849, -18.90625000204837391 ) ) ;
#12936 = VECTOR ( 'NONE', #15433, 1000.000000000000000 ) ;
#12937 = CARTESIAN_POINT ( 'NONE',  ( -10.81189881249999729, 6.242252689847871849, -26.21875000204837391 ) ) ;
#12938 = CARTESIAN_POINT ( 'NONE',  ( -7.216878364870405349, -17.50000000000005684, 49.99999999999998579 ) ) ;
#12939 = CARTESIAN_POINT ( 'NONE',  ( 10.81189881249999729, 0.000000000000000000, -134.8437500020484094 ) ) ;
#12940 = CARTESIAN_POINT ( 'NONE',  ( 5.000000000000000000, 8.660254037844385522, -117.2500000000000000 ) ) ;
#12941 = VECTOR ( 'NONE', #21864, 1000.000000000000000 ) ;
#12942 = CARTESIAN_POINT ( 'NONE',  ( 5.000000000000000000, 8.660254037844385522, -111.2499999999999858 ) ) ;
#12943 = CARTESIAN_POINT ( 'NONE',  ( -9.999999999999998224, 1.224646799147353059E-15, -64.24999999999997158 ) ) ;
#12944 = CARTESIAN_POINT ( 'NONE',  ( 7.644554776091147741E-16, 12.48450537969573659, -131.6562500020483810 ) ) ;
#12945 = CARTESIAN_POINT ( 'NONE',  ( 5.405949406249992428, -9.363379034771808662, -117.2812500020483952 ) ) ;
#12946 = ORIENTED_EDGE ( 'NONE', *, *, #2253, .F. ) ;
#12947 = CARTESIAN_POINT ( 'NONE',  ( -9.999999999999998224, 1.224646799147353059E-15, -82.62500000409676204 ) ) ;
#12948 = CARTESIAN_POINT ( 'NONE',  ( 4.999999999999992006, -8.660254037844389075, -106.1250000040967763 ) ) ;
#12949 = DIRECTION ( 'NONE',  ( 1.000000000000000000, 0.000000000000000000, 0.000000000000000000 ) ) ;
#12950 = CARTESIAN_POINT ( 'NONE',  ( -2.293366432827344421E-15, -12.48450537969573659, -67.71875000204838102 ) ) ;
#12951 = ORIENTED_EDGE ( 'NONE', *, *, #20669, .F. ) ;
#12952 = CARTESIAN_POINT ( 'NONE',  ( -9.999999999999998224, 1.224646799147353059E-15, -41.74999999999997868 ) ) ;
#12953 = CARTESIAN_POINT ( 'NONE',  ( -5.000000000000003553, -8.660254037844383745, -19.37500000409675494 ) ) ;
#12954 = CARTESIAN_POINT ( 'NONE',  ( -5.405949406250003975, -9.363379034771801557, -45.53125000204838102 ) ) ;
#12955 = CARTESIAN_POINT ( 'NONE',  ( -4.999999999999996447, 8.660254037844387298, -16.49999999999995737 ) ) ;
#12956 = CARTESIAN_POINT ( 'NONE',  ( -5.000000000000003553, -8.660254037844383745, -34.37500000409676915 ) ) ;
#12957 = CARTESIAN_POINT ( 'NONE',  ( 5.405949406249999534, 9.363379034771803333, -37.28125000204837391 ) ) ;
#12958 = CARTESIAN_POINT ( 'NONE',  ( 9.999999999999479527, 5.773502691896553074, -117.7500000040968189 ) ) ;
#12959 = CARTESIAN_POINT ( 'NONE',  ( 10.81189881249999729, 0.000000000000000000, -141.0312500020483810 ) ) ;
#12960 = CARTESIAN_POINT ( 'NONE',  ( -10.81189881249999729, 6.242252689847871849, -153.9062500020483810 ) ) ;
#12961 = FACE_OUTER_BOUND ( 'NONE', #15238, .T. ) ;
#12962 = VERTEX_POINT ( 'NONE', #38776 ) ;
#12963 = ORIENTED_EDGE ( 'NONE', *, *, #25277, .T. ) ;
#12964 = ORIENTED_EDGE ( 'NONE', *, *, #20399, .F. ) ;
#12965 = VECTOR ( 'NONE', #2513, 1000.000000000000000 ) ;
#12966 =( BOUNDED_CURVE ( )  B_SPLINE_CURVE ( 2, ( #6636, #33191, #19574, #13085, #9451, #39223, #32757 ),
 .UNSPECIFIED., .F., .F. ) 
 B_SPLINE_CURVE_WITH_KNOTS ( ( 3, 2, 2, 3 ),
 ( 0.1044776119402986148, 0.1057213930348259306, 0.1069651741293532465, 0.1082089552238805485 ),
 .UNSPECIFIED. ) 
 CURVE ( )  GEOMETRIC_REPRESENTATION_ITEM ( )  RATIONAL_B_SPLINE_CURVE ( ( 0.9999999999999880096, 0.8660254037844506980, 1.000000000000000000, 0.8660254037844387076, 1.000000000000000000, 0.8660254037844431485, 0.9999999999999955591 ) ) 
 REPRESENTATION_ITEM ( '' )  );
#12967 = CARTESIAN_POINT ( 'NONE',  ( -5.000000000000003553, -8.660254037844383745, -104.4999999999999858 ) ) ;
#12968 = CARTESIAN_POINT ( 'NONE',  ( -2.293366432827344421E-15, -12.48450537969573659, -175.7187500020483810 ) ) ;
#12969 = CARTESIAN_POINT ( 'NONE',  ( 5.405949406249999534, 9.363379034771803333, -23.59375000204835970 ) ) ;
#12970 = CARTESIAN_POINT ( 'NONE',  ( 9.999999999999998224, 1.224646799147353059E-15, -99.99999999999998579 ) ) ;
#12971 = EDGE_CURVE ( 'NONE', #41419, #40786, #3173, .T. ) ;
#12972 = CARTESIAN_POINT ( 'NONE',  ( -5.405949406249996869, 9.363379034771805109, -156.8437500020483810 ) ) ;
#12973 = CARTESIAN_POINT ( 'NONE',  ( -5.405949406249996869, 9.363379034771805109, -141.8437500020483810 ) ) ;
#12974 = EDGE_CURVE ( 'NONE', #40153, #33328, #20789, .T. ) ;
#12975 = CARTESIAN_POINT ( 'NONE',  ( -2.293366432827344421E-15, -12.48450537969573659, -126.2187500020483952 ) ) ;
#12976 = CARTESIAN_POINT ( 'NONE',  ( 5.405949406249999534, 9.363379034771803333, -133.2812500020483810 ) ) ;
#12977 = CARTESIAN_POINT ( 'NONE',  ( 5.405949406249999534, 9.363379034771803333, -20.59375000204835615 ) ) ;
#12979 = EDGE_CURVE ( 'NONE', #16950, #13797, #16502, .T. ) ;
#12978 = CARTESIAN_POINT ( 'NONE',  ( 10.81189881249999729, 0.000000000000000000, -134.8437500020484094 ) ) ;
#12980 =( REPRESENTATION_RELATIONSHIP ('NONE','NONE', #21658, #6779 ) REPRESENTATION_RELATIONSHIP_WITH_TRANSFORMATION ( #28675 )SHAPE_REPRESENTATION_RELATIONSHIP( ) );
#12981 = CARTESIAN_POINT ( 'NONE',  ( -5.000000000000003553, -8.660254037844383745, -163.0000000000000000 ) ) ;
#12982 = CARTESIAN_POINT ( 'NONE',  ( -10.81189881249999729, 6.242252689847871849, -0.9062500020483588159 ) ) ;
#12983 = CARTESIAN_POINT ( 'NONE',  ( -5.405949406250003975, -9.363379034771801557, -69.34375000204836681 ) ) ;
#12984 = CARTESIAN_POINT ( 'NONE',  ( 10.81189881249999907, 6.242252689847868297, -38.90625000204835970 ) ) ;
#12985 = CARTESIAN_POINT ( 'NONE',  ( -10.81189881249999729, 6.242252689847871849, -54.71875000204837391 ) ) ;
#12986 = CARTESIAN_POINT ( 'NONE',  ( 9.999999999998969713, 5.773502691896851502, -57.37499999999996447 ) ) ;
#12987 = CARTESIAN_POINT ( 'NONE',  ( 7.644554776091147741E-16, 12.48450537969573659, -158.4687500020483810 ) ) ;
#12988 = CARTESIAN_POINT ( 'NONE',  ( 5.000000000000000000, 8.660254037844385522, -141.2500000000000000 ) ) ;
#12989 = CARTESIAN_POINT ( 'NONE',  ( -10.81189881249999729, 1.324075727343319199E-15, -138.7812500020483810 ) ) ;
#12990 = CC_DESIGN_PERSON_AND_ORGANIZATION_ASSIGNMENT ( #19359, #42441, ( #138 ) ) ;
#12991 = CARTESIAN_POINT ( 'NONE',  ( -9.999999999999998224, 1.224646799147353059E-15, -179.7500000000000284 ) ) ;
#12992 = CARTESIAN_POINT ( 'NONE',  ( 4.999999999999992006, -8.660254037844389075, -110.6250000040967763 ) ) ;
#12993 = CARTESIAN_POINT ( 'NONE',  ( -9.999999999999998224, 1.224646799147353059E-15, -88.24999999999998579 ) ) ;
#12994 = VERTEX_POINT ( 'NONE', #9832 ) ;
#12995 = CARTESIAN_POINT ( 'NONE',  ( -5.405949406250003975, -9.363379034771801557, -114.5312500020483952 ) ) ;
#12996 = CARTESIAN_POINT ( 'NONE',  ( 4.999999999999992006, -8.660254037844389075, -131.6250000040967620 ) ) ;
#12997 = CARTESIAN_POINT ( 'NONE',  ( -10.81189881249999729, 1.324075727343319199E-15, -176.2812500020484094 ) ) ;
#12998 = CARTESIAN_POINT ( 'NONE',  ( -9.999999999999998224, 5.773502691896259087, -39.25000000409676915 ) ) ;
#12999 = EDGE_CURVE ( 'NONE', #4387, #17690, #32725, .T. ) ;
#13000 = AXIS2_PLACEMENT_3D ( 'NONE', #38277, #14954, #12360 ) ;
#13001 = DIRECTION ( 'NONE',  ( -0.000000000000000000, -0.000000000000000000, 1.000000000000000000 ) ) ;
#13002 = CARTESIAN_POINT ( 'NONE',  ( -5.405949406249996869, 9.363379034771805109, -59.53125000204836681 ) ) ;
#13003 = CARTESIAN_POINT ( 'NONE',  ( -9.999999999999998224, 1.224646799147353059E-15, -155.7500000000000000 ) ) ;
#13004 = CARTESIAN_POINT ( 'NONE',  ( 10.81189881249999551, -6.242252689847874514, -165.1562500020483526 ) ) ;
#13005 = EDGE_CURVE ( 'NONE', #28518, #19199, #1537, .T. ) ;
#13006 = AXIS2_PLACEMENT_3D ( 'NONE', #8781, #2528, #6182 ) ;
#13007 = CARTESIAN_POINT ( 'NONE',  ( -10.81189881249999729, 1.324075727343319199E-15, -141.5937500020483810 ) ) ;
#13008 = CARTESIAN_POINT ( 'NONE',  ( -9.999999999999998224, 1.224646799147353059E-15, -166.6250000040967905 ) ) ;
#13009 = CYLINDRICAL_SURFACE ( 'NONE', #1365, 9.999999999999998224 ) ;
#13010 = EDGE_CURVE ( 'NONE', #7903, #19199, #32314, .T. ) ;
#13011 = ORIENTED_EDGE ( 'NONE', *, *, #36194, .F. ) ;
#13012 = CARTESIAN_POINT ( 'NONE',  ( -9.999999999999998224, 1.224646799147353059E-15, -130.6250000040967620 ) ) ;
#13013 =( BOUNDED_CURVE ( )  B_SPLINE_CURVE ( 2, ( #24844, #24627, #17902, #20937, #37774, #37559, #31099 ),
 .UNSPECIFIED., .F., .F. ) 
 B_SPLINE_CURVE_WITH_KNOTS ( ( 3, 2, 2, 3 ),
 ( 0.5335820895522389584, 0.5348258706467662327, 0.5360696517412936180, 0.5373134328358210032 ),
 .UNSPECIFIED. ) 
 CURVE ( )  GEOMETRIC_REPRESENTATION_ITEM ( )  RATIONAL_B_SPLINE_CURVE ( ( 0.9999999999999880096, 0.8660254037844506980, 1.000000000000000000, 0.8660254037844387076, 1.000000000000000000, 0.8660254037844267172, 1.000000000000011990 ) ) 
 REPRESENTATION_ITEM ( '' )  );
#13014 = AXIS2_PLACEMENT_3D ( 'NONE', #8246, #11669, #41664 ) ;
#13016 = ORIENTED_EDGE ( 'NONE', *, *, #8670, .F. ) ;
#13015 = CARTESIAN_POINT ( 'NONE',  ( -5.405949406250003975, -9.363379034771801557, -71.03125000204838102 ) ) ;
#13018 = ORIENTED_EDGE ( 'NONE', *, *, #21969, .T. ) ;
#13017 = CARTESIAN_POINT ( 'NONE',  ( -10.81189881249999907, -6.242252689847864744, -120.4687500020483810 ) ) ;
#13019 = EDGE_CURVE ( 'NONE', #10539, #23457, #2739, .T. ) ;
#13020 = VERTEX_POINT ( 'NONE', #29068 ) ;
#13021 = CARTESIAN_POINT ( 'NONE',  ( 5.405949406249992428, -9.363379034771808662, -18.09375000204835260 ) ) ;
#13022 = CARTESIAN_POINT ( 'NONE',  ( 10.81189881249999907, 6.242252689847868297, -199.2187500020484094 ) ) ;
#13023 =( BOUNDED_CURVE ( )  B_SPLINE_CURVE ( 2, ( #32863, #3295, #39533, #9963, #23141, #19890, #33073 ),
 .UNSPECIFIED., .F., .F. ) 
 B_SPLINE_CURVE_WITH_KNOTS ( ( 3, 2, 2, 3 ),
 ( 0.9440298507462689948, 0.9452736318407963800, 0.9465174129353237653, 0.9477611940298510396 ),
 .UNSPECIFIED. ) 
 CURVE ( )  GEOMETRIC_REPRESENTATION_ITEM ( )  RATIONAL_B_SPLINE_CURVE ( ( 0.9999999999999641398, 0.8660254037844745678, 1.000000000000000000, 0.8660254037844387076, 1.000000000000000000, 0.8660254037844028474, 1.000000000000035971 ) ) 
 REPRESENTATION_ITEM ( '' )  );
#13024 = CARTESIAN_POINT ( 'NONE',  ( -2.293366432827344421E-15, -12.48450537969573659, -48.21875000204836681 ) ) ;
#13025 = CARTESIAN_POINT ( 'NONE',  ( 0.000000000000000000, 0.000000000000000000, -99.99999999999998579 ) ) ;
#13026 = CARTESIAN_POINT ( 'NONE',  ( -2.121150477449813534E-15, -11.54700538379251284, -26.37499999999997868 ) ) ;
#13027 = CARTESIAN_POINT ( 'NONE',  ( -5.405949406250003975, -9.363379034771801557, -184.8437500020483810 ) ) ;
#13028 = CARTESIAN_POINT ( 'NONE',  ( -10.81189881249999729, 6.242252689847871849, -167.2187500020483810 ) ) ;
#13029 = CARTESIAN_POINT ( 'NONE',  ( 10.81189881249999729, 0.000000000000000000, -152.8437500020483810 ) ) ;
#13030 = CARTESIAN_POINT ( 'NONE',  ( -5.405949406249996869, 9.363379034771805109, -164.3437500020484094 ) ) ;
#13031 = LINE ( 'NONE', #6375, #28845 ) ;
#13032 = CARTESIAN_POINT ( 'NONE',  ( -10.00000000000015987, 5.773502691896167605, -193.3750000000000853 ) ) ;
#13033 = CARTESIAN_POINT ( 'NONE',  ( -4.999999999999996447, 8.660254037844387298, -187.5000000000000000 ) ) ;
#13034 = AXIS2_PLACEMENT_3D ( 'NONE', #24309, #31209, #4436 ) ;
#13035 = CARTESIAN_POINT ( 'NONE',  ( -10.81189881249999907, -6.242252689847864744, -96.46875000204838102 ) ) ;
#13036 = CARTESIAN_POINT ( 'NONE',  ( 10.81189881249999551, -6.242252689847874514, -78.15625000204838102 ) ) ;
#13037 = CARTESIAN_POINT ( 'NONE',  ( -5.000000000000003553, -8.660254037844383745, -131.8750000040967905 ) ) ;
#13038 = CARTESIAN_POINT ( 'NONE',  ( 5.405949406249999534, 9.363379034771803333, -190.0937500020483810 ) ) ;
#13039 = CARTESIAN_POINT ( 'NONE',  ( 5.405949406249999534, 9.363379034771803333, -166.2812500020484094 ) ) ;
#13040 = CARTESIAN_POINT ( 'NONE',  ( -10.81189881249999907, -6.242252689847864744, -60.65625000204838813 ) ) ;
#13041 = CARTESIAN_POINT ( 'NONE',  ( -5.000000000000003553, -8.660254037844383745, -137.8750000040967905 ) ) ;
#13042 = CARTESIAN_POINT ( 'NONE',  ( 9.999999999999998224, 0.000000000000000000, -111.4999999999999858 ) ) ;
#13043 = ORIENTED_EDGE ( 'NONE', *, *, #17790, .F. ) ;
#13044 = AXIS2_PLACEMENT_3D ( 'NONE', #11298, #24492, #8085 ) ;
#13045 = CARTESIAN_POINT ( 'NONE',  ( -10.81189881249999729, -6.242252689847864744, -138.6562500020484094 ) ) ;
#13046 = CARTESIAN_POINT ( 'NONE',  ( -5.405949406249996869, 9.363379034771805109, -155.5312500020484094 ) ) ;
#13047 = ADVANCED_FACE ( 'NONE', ( #42206 ), #12632, .T. ) ;
#13048 = CARTESIAN_POINT ( 'NONE',  ( -10.81189881249999907, -6.242252689847864744, -198.6562500020484094 ) ) ;
#13049 = CARTESIAN_POINT ( 'NONE',  ( -4.999999999999996447, 8.660254037844387298, -130.8750000040967905 ) ) ;
#13050 = CARTESIAN_POINT ( 'NONE',  ( 10.81189881249999907, 6.242252689847868297, -86.71875000204836681 ) ) ;
#13051 = ORIENTED_EDGE ( 'NONE', *, *, #8437, .T. ) ;
#13052 = CARTESIAN_POINT ( 'NONE',  ( -10.00000000000000000, -5.773502691896251982, -53.62499999999997868 ) ) ;
#13053 = CARTESIAN_POINT ( 'NONE',  ( 10.81189881249999907, 6.242252689847868297, -187.2187500020484094 ) ) ;
#13054 = CARTESIAN_POINT ( 'NONE',  ( -4.999999999999996447, 8.660254037844387298, -64.87500000409676204 ) ) ;
#13055 = CARTESIAN_POINT ( 'NONE',  ( -9.999999999999742428, -5.773502691896402084, -117.0000000040967763 ) ) ;
#13056 = CARTESIAN_POINT ( 'NONE',  ( 7.070501591499376803E-16, 11.54700538379251284, -12.50000000409677092 ) ) ;
#13057 = CARTESIAN_POINT ( 'NONE',  ( -10.81189881249999729, 1.324075727343319199E-15, -87.78125000204838102 ) ) ;
#13058 = CARTESIAN_POINT ( 'NONE',  ( 10.81189881249999729, 0.000000000000000000, -70.53125000204838102 ) ) ;
#13059 = CARTESIAN_POINT ( 'NONE',  ( 10.00000000000000000, 5.773502691896255534, -57.75000000409677625 ) ) ;
#13060 = CARTESIAN_POINT ( 'NONE',  ( 5.405949406249999534, 9.363379034771803333, -19.09375000204835260 ) ) ;
#13061 = CARTESIAN_POINT ( 'NONE',  ( 5.000000000000000000, 8.660254037844385522, -38.12500000409676915 ) ) ;
#13062 = CARTESIAN_POINT ( 'NONE',  ( -10.81189881249999729, 1.324075727343319199E-15, -188.2812500020484094 ) ) ;
#13063 = CARTESIAN_POINT ( 'NONE',  ( -10.81189881249999907, -6.242252689847864744, -12.65625000204837036 ) ) ;
#13064 = CARTESIAN_POINT ( 'NONE',  ( -2.121150477449813534E-15, -11.54700538379251284, -172.2500000040968189 ) ) ;
#13065 = DIRECTION ( 'NONE',  ( -0.000000000000000000, -0.000000000000000000, 1.000000000000000000 ) ) ;
#13066 = CYLINDRICAL_SURFACE ( 'NONE', #17609, 9.999999999999998224 ) ;
#13067 = CARTESIAN_POINT ( 'NONE',  ( -2.121150477449813534E-15, -11.54700538379251284, -167.3750000000000000 ) ) ;
#13068 = CARTESIAN_POINT ( 'NONE',  ( 5.000000000000000000, 8.660254037844385522, -97.74999999999998579 ) ) ;
#13069 = AXIS2_PLACEMENT_3D ( 'NONE', #20665, #4277, #30406 ) ;
#13071 = ORIENTED_EDGE ( 'NONE', *, *, #1972, .T. ) ;
#13070 = CARTESIAN_POINT ( 'NONE',  ( -5.405949406250003975, -9.363379034771801557, -92.03125000204838102 ) ) ;
#13072 = CARTESIAN_POINT ( 'NONE',  ( -9.999999999999872102, -5.773502691896326589, -163.1250000000000000 ) ) ;
#13074 = ORIENTED_EDGE ( 'NONE', *, *, #24533, .F. ) ;
#13073 = CARTESIAN_POINT ( 'NONE',  ( 4.999999999999992006, -8.660254037844389075, -153.7500000000000000 ) ) ;
#13075 = EDGE_LOOP ( 'NONE', ( #34062, #12812, #2969, #31590 ) ) ;
#13076 = CARTESIAN_POINT ( 'NONE',  ( 10.81189881249999907, 6.242252689847868297, -31.21875000204835260 ) ) ;
#13077 = CARTESIAN_POINT ( 'NONE',  ( 10.81189881249999907, 6.242252689847868297, -20.90625000204836681 ) ) ;
#13078 = CARTESIAN_POINT ( 'NONE',  ( -2.293366432827344421E-15, -12.48450537969573659, -75.21875000204839523 ) ) ;
#13079 = CARTESIAN_POINT ( 'NONE',  ( 9.999999999999866773, -5.773502691896336358, -173.5000000040967905 ) ) ;
#13080 = CARTESIAN_POINT ( 'NONE',  ( 5.405949406249992428, -9.363379034771808662, -190.5937500020484094 ) ) ;
#13081 = CARTESIAN_POINT ( 'NONE',  ( -4.999999999999996447, 8.660254037844387298, -98.99999999999998579 ) ) ;
#13082 = CARTESIAN_POINT ( 'NONE',  ( -5.000000000000003553, -8.660254037844383745, -143.8750000040967905 ) ) ;
#13083 = CARTESIAN_POINT ( 'NONE',  ( 10.81189881249999729, 0.000000000000000000, -157.5312500020484094 ) ) ;
#13084 = CARTESIAN_POINT ( 'NONE',  ( -4.999999999999996447, 8.660254037844387298, -4.875000004096769146 ) ) ;
#13085 = CARTESIAN_POINT ( 'NONE',  ( 7.070501591499376803E-16, 11.54700538379251284, -178.6250000000000000 ) ) ;
#13086 = CARTESIAN_POINT ( 'NONE',  ( 5.405949406249992428, -9.363379034771808662, -123.0937500020483952 ) ) ;
#13087 = CARTESIAN_POINT ( 'NONE',  ( -10.81189881249999729, 6.242252689847871849, -96.90625000204838102 ) ) ;
#13088 = CARTESIAN_POINT ( 'NONE',  ( -5.405949406250003975, -9.363379034771801557, -111.3437500020483810 ) ) ;
#13089 = CARTESIAN_POINT ( 'NONE',  ( 10.81189881249999729, 0.000000000000000000, -76.34375000204838102 ) ) ;
#13090 = CARTESIAN_POINT ( 'NONE',  ( -10.81189881249999729, 1.324075727343319199E-15, -87.78125000204838102 ) ) ;
#13091 = CARTESIAN_POINT ( 'NONE',  ( 9.999999999999996447, -5.773502691896262640, -163.0000000040967905 ) ) ;
#13092 = CARTESIAN_POINT ( 'NONE',  ( -9.999999999998456346, -5.773502691897145489, -67.12499999999997158 ) ) ;
#13093 = CARTESIAN_POINT ( 'NONE',  ( 10.81189881249999729, 0.000000000000000000, -166.5312500020484094 ) ) ;
#13094 = CARTESIAN_POINT ( 'NONE',  ( 7.644554776091147741E-16, 12.48450537969573659, -182.6562500020484094 ) ) ;
#13095 = CONICAL_SURFACE ( 'NONE', #40669, 31.99999999999997158, 0.7853981633974447263 ) ;
#13096 = EDGE_CURVE ( 'NONE', #25538, #36134, #38205, .T. ) ;
#13097 = CARTESIAN_POINT ( 'NONE',  ( -10.00000000000000000, -5.773502691896251982, -159.0000000040967905 ) ) ;
#13098 = CARTESIAN_POINT ( 'NONE',  ( -9.999999999999804601, -5.773502691896363892, -190.1250000000000284 ) ) ;
#13099 = CARTESIAN_POINT ( 'NONE',  ( -10.81189881249999729, 6.242252689847871849, -5.218750002048355263 ) ) ;
#13100 = CARTESIAN_POINT ( 'NONE',  ( 10.00000000000025402, -5.773502691896113426, -126.6249999999999858 ) ) ;
#13101 = CARTESIAN_POINT ( 'NONE',  ( -10.81189881249999729, 6.242252689847871849, -113.2187500020483952 ) ) ;
#13102 = CARTESIAN_POINT ( 'NONE',  ( -4.999999999999996447, 8.660254037844387298, -80.99999999999998579 ) ) ;
#13103 = CARTESIAN_POINT ( 'NONE',  ( -2.293366432827344421E-15, -12.48450537969573659, -13.90625000204836859 ) ) ;
#13104 = CARTESIAN_POINT ( 'NONE',  ( 5.000000000000000000, 8.660254037844385522, -96.62500000409677625 ) ) ;
#13105 = LINE ( 'NONE', #36014, #28630 ) ;
#13106 = CARTESIAN_POINT ( 'NONE',  ( -5.405949406249996869, 9.363379034771805109, -109.0312500020483810 ) ) ;
#13107 = CARTESIAN_POINT ( 'NONE',  ( 5.405949406249999534, 9.363379034771803333, -89.78125000204838102 ) ) ;
#13108 = ORIENTED_EDGE ( 'NONE', *, *, #20159, .F. ) ;
#13109 = CARTESIAN_POINT ( 'NONE',  ( 9.999999999999996447, -5.773502691896262640, -80.50000000409676204 ) ) ;
#13110 = CARTESIAN_POINT ( 'NONE',  ( -10.00000000000051337, 5.773502691895962435, -145.7500000040967905 ) ) ;
#13111 = CARTESIAN_POINT ( 'NONE',  ( -5.405949406250003975, -9.363379034771801557, -40.84375000204837391 ) ) ;
#13112 = EDGE_LOOP ( 'NONE', ( #18446, #16681, #13256, #6045 ) ) ;
#13113 = CARTESIAN_POINT ( 'NONE',  ( -2.121150477449813534E-15, -11.54700538379251284, -6.874999999999968026 ) ) ;
#13114 = CARTESIAN_POINT ( 'NONE',  ( -9.999999999999998224, 5.773502691896259087, -146.8750000000000000 ) ) ;
#13115 = CARTESIAN_POINT ( 'NONE',  ( -2.121150477449813534E-15, -11.54700538379251284, -13.25000000409676204 ) ) ;
#13116 = EDGE_CURVE ( 'NONE', #9902, #14006, #4801, .T. ) ;
#13117 = CARTESIAN_POINT ( 'NONE',  ( 7.070501591499377789E-16, 11.54700538379251284, -193.6250000000000000 ) ) ;
#13119 = ORIENTED_EDGE ( 'NONE', *, *, #13096, .T. ) ;
#13118 = CARTESIAN_POINT ( 'NONE',  ( -10.81189881249999729, 6.242252689847871849, -120.9062500020483952 ) ) ;
#13120 = FACE_OUTER_BOUND ( 'NONE', #29690, .T. ) ;
#13121 = ORIENTED_EDGE ( 'NONE', *, *, #19118, .F. ) ;
#13122 = CARTESIAN_POINT ( 'NONE',  ( -5.405949406249996869, 9.363379034771805109, -46.03125000204838813 ) ) ;
#13123 = DATE_AND_TIME ( #3, #37301 ) ;
#13124 = AXIS2_PLACEMENT_3D ( 'NONE', #1861, #28185, #19088 ) ;
#13125 = CARTESIAN_POINT ( 'NONE',  ( -5.405949406250003975, -9.363379034771801557, -103.8437500020483810 ) ) ;
#13126 = CARTESIAN_POINT ( 'NONE',  ( 5.405949406249992428, -9.363379034771808662, -126.2812500020483668 ) ) ;
#13127 = ORIENTED_EDGE ( 'NONE', *, *, #38472, .F. ) ;
#13128 = AXIS2_PLACEMENT_3D ( 'NONE', #15193, #35076, #35289 ) ;
#13129 = CARTESIAN_POINT ( 'NONE',  ( -9.999999999999998224, 1.224646799147353059E-15, -83.74999999999997158 ) ) ;
#13130 = FACE_OUTER_BOUND ( 'NONE', #35779, .T. ) ;
#13131 =( BOUNDED_CURVE ( )  B_SPLINE_CURVE ( 2, ( #4665, #27981, #18034, #17596, #14355, #41109, #15219, #17816, #1655, #40901, #28418, #18248, #27763, #11549, #40686, #37904, #34464, #11771, #5103, #27552, #18466, #11987, #31011, #11126, #14575, #11343, #1440, #37686, #4886, #31439, #24329, #37248, #14785, #24758, #24973, #37470, #8348, #38114, #5315, #20849, #21499, #31654, #7914, #7697, #2089, #34033, #32498, #18676, #2927, #25596, #32077, #12823, #5744, #22140, #35315, #12609, #32288, #16056, #42391, #42604, #15844, #29247, #26014, #6164, #5526, #35101, #39166, #41760, #18897, #42183, #35736, #9599, #8765, #22351, #38753, #2712, #19106, #25182, #9393, #8974, #12194, #29044, #3133, #2512, #5956, #28838, #16262, #19304, #15636, #25803, #28628, #38960, #9180, #22773, #35934, #31874, #6374, #21921, #19518, #25385, #35527, #41970, #12403, #22558, #32703, #29461, #38324, #2305, #15430, #38532, #7424, #29889, #13448, #29677, #27070, #16903, #26224, #33553, #26429, #16477, #10016, #39792, #10225, #16693, #22987, #543, #13030, #30535, #20158, #33349, #32913, #36144, #753, #39580, #33764, #26644, #328, #3769, #121, #19942, #13875, #3345, #39372, #19731, #36354, #33131, #23412, #23839, #13242, #17332, #9809, #30104, #23194, #6787, #6575, #3558, #36561, #26853, #7007, #13661, #20364, #23630, #3978, #40007, #10438, #36774, #7212, #17118, #30318, #40213, #10645, #36988, #20575, #4187, #40416, #18193, #21437, #31385, #24702, #11717, #41279, #4401, #1603, #27710, #8290, #11500, #37192, #24914, #10860, #38060, #30742, #11287, #41056, #37848, #17759, #8502, #24051, #17541, #1172, #30954, #14296, #21654, #1386, #14517, #27495, #14946, #4828, #14080, #34621, #40629, #11071, #24272, #40848, #14733, #5048, #24482, #7641, #37419, #37634, #27925, #28146, #20792, #33979, #1820, #7861, #34836, #8073, #21223, #34408, #21010, #34199, #5259, #4616, #17974, #31174, #18411, #962, #27278, #28789, #19260, #35685, #22089, #25337, #15376, #8927, #28994, #8716, #9551, #12352, #5902, #9343, #41498, #28576, #38912, #2877, #15162, #41706, #35890, #6113, #16007, #35476, #25966, #22511, #25124, #32451, #32028, #38483, #29202, #12144, #35264, #5698, #19056, #38700, #42342, #12773, #39116, #25550, #18848, #2457, #22725, #15588, #6327, #9134, #18626, #31600, #2033, #2664, #28361, #11932, #32238, #41920, #22304, #15798, #38270, #42134, #21870, #35049, #12565, #25759, #5477, #31822, #2257, #40167, #33078, #36309, #10180, #36096, #26385, #20317, #9967, #26175, #13192, #29624, #6740, #23146, #16642, #7165, #23579, #26595, #6530, #30057, #39537, #16855, #39321, #10599, #282, #36517, #39959, #29414, #16426, #26808, #33511, #3085, #67, #23785, #36726, #3934, #23365, #27021, #19894, #32867, #10390, #3504, #29844, #17072, #13403, #39745, #6954, #20110, #33300, #30269, #708, #36940, #3725, #3299, #501, #16213, #19472, #13616, #13827, #42554, #32657, #12978, #9761, #22942, #19681, #4567, #20963, #14470, #1339, #7382, #34363, #33934, #24005, #27878, #27660, #4141, #24655, #41010, #37798, #31124, #40586, #40801, #10812, #8029, #34149, #14689, #17927, #916, #31342, #17282, #18146, #37145, #17709, #4779, #1557, #24221, #1772, #30487, #4357, #7593, #11242, #28101, #30691, #30904, #11027, #41229, #11455, #37372, #24441, #20747, #21173, #37584, #8243, #21391, #14031, #14902, #27227, #11666, #17498, #34574, #7815, #1124, #5005, #24867, #27450, #20528, #33716, #40371, #14247, #32402, #12098, #38436, #11884, #9287, #41867, #8460, #15749, #8669, #41448, #35003, #22042, #35214, #41662, #5211, #25502, #38015, #12716, #2408, #15539, #15114, #18367, #25710, #21823, #15958, #8879, #25291, #28741, #25080, #2199, #38860, #28309, #21611, #1988, #18583, #15333, #5644, #6063, #38225, #42294, #28530, #31771, #5432, #18793, #35424, #31982, #29155, #12305, #38651, #28948, #31555, #5851, #12517, #42085, #9086, #22254, #19006, #32191, #34790, #2618, #2825, #22459, #35636, #19213, #26335, #32815, #13565, #6484, #22889, #36048, #13355, #35843, #42499, #30220, #9503, #6901, #33248, #26756, #20054, #6275, #19421, #448, #12927, #19631, #233, #36465, #16803, #22672, #23096, #39487, #33025, #3246, #16590, #6689, #9920, #3675, #30002, #32612, #7117, #3037, #36676, #26122, #36259, #23310, #39908, #17, #20271, #16164, #39276, #29360, #13140, #16372, #33459, #19840, #3454, #9710, #10339, #29792, #39065, #23527, #29572, #26546, #39695, #10131, #3886, #17021, #659, #25913, #27178, #4304, #7763, #40531, #7332, #23735, #24390, #865, #1504, #17443, #20694, #24170, #4092, #23953, #37531, #37097, #20481, #10762, #40321, #33882, #30639, #1071, #7972, #14638, #7540, #14195, #13981, #27394, #4512, #33668, #31070, #10974, #37317, #27610, #10550, #20907, #14416, #21121, #26961, #34089, #27826, #11192, #34310, #13777, #17655, #30850, #40117, #36886, #17874, #1287, #40750, #4725, #17234, #30435, #13288, #19558, #26268, #13915, #35981, #33391, #16949, #40048, #3814, #10061, #23456, #32744, #39420, #30146, #23239, #165, #3181, #7258, #9854, #36604, #23670, #19773, #376, #33175, #16307, #29503, #13497, #30363, #32956, #585, #26893 ),
 .UNSPECIFIED., .F., .F. ) 
 B_SPLINE_CURVE_WITH_KNOTS ( ( 3, 2, 2, 2, 2, 2, 2, 2, 2, 2, 2, 2, 2, 2, 2, 2, 2, 2, 2, 2, 2, 2, 2, 2, 2, 2, 2, 2, 2, 2, 2, 2, 2, 2, 2, 2, 2, 2, 2, 2, 2, 2, 2, 2, 2, 2, 2, 2, 2, 2, 2, 2, 2, 2, 2, 2, 2, 2, 2, 2, 2, 2, 2, 2, 2, 2, 2, 2, 2, 2, 2, 2, 2, 2, 2, 2, 2, 2, 2, 2, 2, 2, 2, 2, 2, 2, 2, 2, 2, 2, 2, 2, 2, 2, 2, 2, 2, 2, 2, 2, 2, 2, 2, 2, 2, 2, 2, 2, 2, 2, 2, 2, 2, 2, 2, 2, 2, 2, 2, 2, 2, 2, 2, 2, 2, 2, 2, 2, 2, 2, 2, 2, 2, 2, 2, 2, 2, 2, 2, 2, 2, 2, 2, 2, 2, 2, 2, 2, 2, 2, 2, 2, 2, 2, 2, 2, 2, 2, 2, 2, 2, 2, 2, 2, 2, 2, 2, 2, 2, 2, 2, 2, 2, 2, 2, 2, 2, 2, 2, 2, 2, 2, 2, 2, 2, 2, 2, 2, 2, 2, 2, 2, 2, 2, 2, 2, 2, 2, 2, 2, 2, 2, 2, 2, 2, 2, 2, 2, 2, 2, 2, 2, 2, 2, 2, 2, 2, 2, 2, 2, 2, 2, 2, 2, 2, 2, 2, 2, 2, 2, 2, 2, 2, 2, 2, 2, 2, 2, 2, 2, 2, 2, 2, 2, 2, 2, 2, 2, 2, 2, 2, 2, 2, 2, 2, 2, 2, 2, 2, 2, 2, 2, 2, 2, 2, 2, 2, 2, 2, 2, 2, 2, 2, 2, 2, 2, 2, 2, 2, 2, 2, 2, 2, 2, 2, 2, 2, 2, 2, 2, 2, 2, 2, 2, 2, 2, 2, 2, 2, 2, 2, 2, 2, 2, 2, 2, 2, 2, 2, 2, 2, 2, 2, 2, 2, 2, 2, 2, 2, 2, 2, 3 ),
 ( 0.09624740578742232988, 0.09701492537313433084, 0.09825870646766168837, 0.09950248756218905977, 0.1007462686567164173, 0.1019900497512437748, 0.1032338308457711462, 0.1044776119402985037, 0.1057213930348258751, 0.1069651741293532327, 0.1082089552238805902, 0.1094527363184079616, 0.1106965174129353191, 0.1119402985074626905, 0.1131840796019900480, 0.1144278606965174194, 0.1156716417910447769, 0.1169154228855721345, 0.1181592039800995059, 0.1194029850746268634, 0.1206467661691542348, 0.1218905472636815923, 0.1231343283582089498, 0.1243781094527363212, 0.1256218905472636926, 0.1268656716417910502, 0.1281094527363184077, 0.1293532338308457652, 0.1305970149253731227, 0.1318407960199005080, 0.1330845771144278655, 0.1343283582089552231, 0.1355721393034825806, 0.1368159203980099381, 0.1380597014925373234, 0.1393034825870646809, 0.1405472636815920384, 0.1417910447761193959, 0.1430348258706467535, 0.1442786069651741387, 0.1455223880597014963, 0.1467661691542288538, 0.1480099502487562113, 0.1492537313432835688, 0.1504975124378109541, 0.1517412935323383116, 0.1529850746268656692, 0.1542288557213930267, 0.1554726368159203842, 0.1567164179104477695, 0.1579601990049751270, 0.1592039800995024845, 0.1604477611940298420, 0.1616915422885572273, 0.1629353233830845848, 0.1641791044776119424, 0.1654228855721392999, 0.1666666666666666574, 0.1679104477611940427, 0.1691542288557214002, 0.1703980099502487577, 0.1716417910447761153, 0.1728855721393034728, 0.1741293532338308581, 0.1753731343283582156, 0.1766169154228855731, 0.1778606965174129306, 0.1791044776119402882, 0.1803482587064676734, 0.1815920398009950310, 0.1828358208955223885, 0.1840796019900497460, 0.1853233830845771035, 0.1865671641791044888, 0.1878109452736318463, 0.1890547263681592038, 0.1902985074626865614, 0.1915422885572139189, 0.1927860696517413042, 0.1940298507462686617, 0.1952736318407960192, 0.1965174129353233767, 0.1977611940298507343, 0.1990049751243781195, 0.2002487562189054771, 0.2014925373134328346, 0.2027363184079601921, 0.2039800995024875496, 0.2052238805970149349, 0.2064676616915422924, 0.2077114427860696499, 0.2089552238805970075, 0.2101990049751243927, 0.2114427860696517503, 0.2126865671641791078, 0.2139303482587064653, 0.2151741293532338228, 0.2164179104477612081, 0.2176616915422885656, 0.2189054726368159232, 0.2201492537313432807, 0.2213930348258706382, 0.2226368159203980235, 0.2238805970149253810, 0.2251243781094527385, 0.2263681592039800961, 0.2276119402985074536, 0.2288557213930348389, 0.2300995024875621964, 0.2313432835820895539, 0.2325870646766169114, 0.2338308457711442689, 0.2350746268656716542, 0.2363184079601990117, 0.2375621890547263693, 0.2388059701492537268, 0.2400497512437810843, 0.2412935323383084696, 0.2425373134328358271, 0.2437810945273631846, 0.2450248756218905422, 0.2462686567164178997, 0.2475124378109452850, 0.2487562189054726425, 0.2500000000000000000, 0.2512437810945273853, 0.2524875621890547150, 0.2537313432835821003, 0.2549751243781094301, 0.2562189054726368154, 0.2574626865671642006, 0.2587064676616915304, 0.2599502487562189157, 0.2611940298507462455, 0.2624378109452736307, 0.2636815920398010160, 0.2649253731343283458, 0.2661691542288557311, 0.2674129353233830608, 0.2686567164179104461, 0.2699004975124378314, 0.2711442786069651611, 0.2723880597014925464, 0.2736318407960198762, 0.2748756218905472615, 0.2761194029850746468, 0.2773631840796019765, 0.2786069651741293618, 0.2798507462686566916, 0.2810945273631840768, 0.2823383084577114621, 0.2835820895522387919, 0.2848258706467661772, 0.2860696517412935069, 0.2873134328358208922, 0.2885572139303482775, 0.2898009950248756073, 0.2910447761194029925, 0.2922885572139303223, 0.2935323383084577076, 0.2947761194029850929, 0.2960199004975124226, 0.2972636815920398079, 0.2985074626865671377, 0.2997512437810945229, 0.3009950248756219082, 0.3022388059701492380, 0.3034825870646766233, 0.3047263681592039530, 0.3059701492537313383, 0.3072139303482587236, 0.3084577114427860534, 0.3097014925373134386, 0.3109452736318407684, 0.3121890547263681537, 0.3134328358208955390, 0.3146766169154228687, 0.3159203980099502540, 0.3171641791044776393, 0.3184079601990049690, 0.3196517412935323543, 0.3208955223880596841, 0.3221393034825870694, 0.3233830845771144546, 0.3246268656716417844, 0.3258706467661691697, 0.3271144278606964995, 0.3283582089552238847, 0.3296019900497512700, 0.3308457711442785998, 0.3320895522388059851, 0.3333333333333333148, 0.3345771144278607001, 0.3358208955223880854, 0.3370646766169154152, 0.3383084577114428004, 0.3395522388059701302, 0.3407960199004975155, 0.3420398009950249008, 0.3432835820895522305, 0.3445273631840796158, 0.3457711442786069456, 0.3470149253731342753, 0.3482587064676616606, 0.3495024875621890459, 0.3507462686567164312, 0.3519900497512437054, 0.3532338308457710907, 0.3544776119402984760, 0.3557213930348258613, 0.3569651741293532465, 0.3582089552238805208, 0.3594527363184079061, 0.3606965174129352913, 0.3619402985074626766, 0.3631840796019900619, 0.3644278606965173362, 0.3656716417910447214, 0.3669154228855721067, 0.3681592039800994920, 0.3694029850746268773, 0.3706467661691541515, 0.3718905472636815368, 0.3731343283582089221, 0.3743781094527363074, 0.3756218905472636926, 0.3768656716417909669, 0.3781094527363183522, 0.3793532338308457375, 0.3805970149253731227, 0.3818407960199005080, 0.3830845771144277823, 0.3843283582089551675, 0.3855721393034825528, 0.3868159203980099381, 0.3880597014925373234, 0.3893034825870645976, 0.3905472636815919829, 0.3917910447761193682, 0.3930348258706467535, 0.3942786069651741387, 0.3955223880597014130, 0.3967661691542287983, 0.3980099502487561836, 0.3992537313432835688, 0.4004975124378109541, 0.4017412935323382284, 0.4029850746268656136, 0.4042288557213929989, 0.4054726368159203842, 0.4067164179104477695, 0.4079601990049750437, 0.4092039800995024290, 0.4104477611940299253, 0.4116915422885571996, 0.4129353233830845848, 0.4141791044776118591, 0.4154228855721392444, 0.4166666666666666297, 0.4179104477611940149, 0.4191542288557214002, 0.4203980099502486745, 0.4216417910447760597, 0.4228855721393034450, 0.4241293532338308303, 0.4253731343283582156, 0.4266169154228854898, 0.4278606965174128751, 0.4291044776119402604, 0.4303482587064677567, 0.4315920398009950310, 0.4328358208955223052, 0.4340796019900496905, 0.4353233830845770758, 0.4365671641791044610, 0.4378109452736318463, 0.4390547263681592316, 0.4402985074626865059, 0.4415422885572138911, 0.4427860696517413874, 0.4440298507462686617, 0.4452736318407960470, 0.4465174129353233212, 0.4477611940298507065, 0.4490049751243780918, 0.4502487562189054771, 0.4514925373134328623, 0.4527363184079601366, 0.4539800995024875219, 0.4552238805970150182, 0.4564676616915422924, 0.4577114427860696777, 0.4589552238805969520, 0.4601990049751243372, 0.4614427860696517225, 0.4626865671641791078, 0.4639303482587064931, 0.4651741293532337673, 0.4664179104477611526, 0.4676616915422885379, 0.4689054726368159232, 0.4701492537313433084, 0.4713930348258705827, 0.4726368159203979680, 0.4738805970149253532, 0.4751243781094528496, 0.4763681592039801238, 0.4776119402985073981, 0.4788557213930347833, 0.4800995024875621686, 0.4813432835820895539, 0.4825870646766169392, 0.4838308457711442134, 0.4850746268656715987, 0.4863184079601989840, 0.4875621890547264803, 0.4888059701492537545, 0.4900497512437810288, 0.4912935323383084141, 0.4925373134328357994, 0.4937810945273631846, 0.4942573560361783747 ),
 .UNSPECIFIED. ) 
 CURVE ( )  GEOMETRIC_REPRESENTATION_ITEM ( )  RATIONAL_B_SPLINE_CURVE ( ( 0.9366860366984448572, 0.9173261862270272182, 1.000000000000000000, 0.8660254037844387076, 1.000000000000000000, 0.8660254037844387076, 1.000000000000000000, 0.8660254037844387076, 1.000000000000000000, 0.8660254037844387076, 1.000000000000000000, 0.8660254037844387076, 1.000000000000000000, 0.8660254037844387076, 1.000000000000000000, 0.8660254037844387076, 1.000000000000000000, 0.8660254037844387076, 1.000000000000000000, 0.8660254037844387076, 1.000000000000000000, 0.8660254037844387076, 1.000000000000000000, 0.8660254037844387076, 1.000000000000000000, 0.8660254037844387076, 1.000000000000000000, 0.8660254037844387076, 1.000000000000000000, 0.8660254037844387076, 1.000000000000000000, 0.8660254037844387076, 1.000000000000000000, 0.8660254037844387076, 1.000000000000000000, 0.8660254037844387076, 1.000000000000000000, 0.8660254037844387076, 1.000000000000000000, 0.8660254037844387076, 1.000000000000000000, 0.8660254037844387076, 1.000000000000000000, 0.8660254037844387076, 1.000000000000000000, 0.8660254037844387076, 1.000000000000000000, 0.8660254037844387076, 1.000000000000000000, 0.8660254037844387076, 1.000000000000000000, 0.8660254037844387076, 1.000000000000000000, 0.8660254037844387076, 1.000000000000000000, 0.8660254037844387076, 1.000000000000000000, 0.8660254037844387076, 1.000000000000000000, 0.8660254037844387076, 1.000000000000000000, 0.8660254037844387076, 1.000000000000000000, 0.8660254037844387076, 1.000000000000000000, 0.8660254037844387076, 1.000000000000000000, 0.8660254037844387076, 1.000000000000000000, 0.8660254037844387076, 1.000000000000000000, 0.8660254037844387076, 1.000000000000000000, 0.8660254037844387076, 1.000000000000000000, 0.8660254037844387076, 1.000000000000000000, 0.8660254037844387076, 1.000000000000000000, 0.8660254037844387076, 1.000000000000000000, 0.8660254037844387076, 1.000000000000000000, 0.8660254037844387076, 1.000000000000000000, 0.8660254037844387076, 1.000000000000000000, 0.8660254037844387076, 1.000000000000000000, 0.8660254037844387076, 1.000000000000000000, 0.8660254037844387076, 1.000000000000000000, 0.8660254037844387076, 1.000000000000000000, 0.8660254037844387076, 1.000000000000000000, 0.8660254037844387076, 1.000000000000000000, 0.8660254037844387076, 1.000000000000000000, 0.8660254037844387076, 1.000000000000000000, 0.8660254037844387076, 1.000000000000000000, 0.8660254037844387076, 1.000000000000000000, 0.8660254037844387076, 1.000000000000000000, 0.8660254037844387076, 1.000000000000000000, 0.8660254037844387076, 1.000000000000000000, 0.8660254037844387076, 1.000000000000000000, 0.8660254037844387076, 1.000000000000000000, 0.8660254037844387076, 1.000000000000000000, 0.8660254037844387076, 1.000000000000000000, 0.8660254037844387076, 1.000000000000000000, 0.8660254037844387076, 1.000000000000000000, 0.8660254037844387076, 1.000000000000000000, 0.8660254037844387076, 1.000000000000000000, 0.8660254037844387076, 1.000000000000000000, 0.8660254037844387076, 1.000000000000000000, 0.8660254037844387076, 1.000000000000000000, 0.8660254037844387076, 1.000000000000000000, 0.8660254037844387076, 1.000000000000000000, 0.8660254037844387076, 1.000000000000000000, 0.8660254037844387076, 1.000000000000000000, 0.8660254037844387076, 1.000000000000000000, 0.8660254037844387076, 1.000000000000000000, 0.8660254037844387076, 1.000000000000000000, 0.8660254037844387076, 1.000000000000000000, 0.8660254037844387076, 1.000000000000000000, 0.8660254037844387076, 1.000000000000000000, 0.8660254037844387076, 1.000000000000000000, 0.8660254037844387076, 1.000000000000000000, 0.8660254037844387076, 1.000000000000000000, 0.8660254037844387076, 1.000000000000000000, 0.8660254037844387076, 1.000000000000000000, 0.8660254037844387076, 1.000000000000000000, 0.8660254037844387076, 1.000000000000000000, 0.8660254037844387076, 1.000000000000000000, 0.8660254037844387076, 1.000000000000000000, 0.8660254037844387076, 1.000000000000000000, 0.8660254037844387076, 1.000000000000000000, 0.8660254037844387076, 1.000000000000000000, 0.8660254037844387076, 1.000000000000000000, 0.8660254037844387076, 1.000000000000000000, 0.8660254037844387076, 1.000000000000000000, 0.8660254037844387076, 1.000000000000000000, 0.8660254037844387076, 1.000000000000000000, 0.8660254037844387076, 1.000000000000000000, 0.8660254037844387076, 1.000000000000000000, 0.8660254037844387076, 1.000000000000000000, 0.8660254037844387076, 1.000000000000000000, 0.8660254037844387076, 1.000000000000000000, 0.8660254037844387076, 1.000000000000000000, 0.8660254037844387076, 1.000000000000000000, 0.8660254037844387076, 1.000000000000000000, 0.8660254037844387076, 1.000000000000000000, 0.8660254037844387076, 1.000000000000000000, 0.8660254037844387076, 1.000000000000000000, 0.8660254037844387076, 1.000000000000000000, 0.8660254037844387076, 1.000000000000000000, 0.8660254037844387076, 1.000000000000000000, 0.8660254037844387076, 1.000000000000000000, 0.8660254037844387076, 1.000000000000000000, 0.8660254037844387076, 1.000000000000000000, 0.8660254037844387076, 1.000000000000000000, 0.8660254037844387076, 1.000000000000000000, 0.8660254037844387076, 1.000000000000000000, 0.8660254037844387076, 1.000000000000000000, 0.8660254037844387076, 1.000000000000000000, 0.8660254037844387076, 1.000000000000000000, 0.8660254037844387076, 1.000000000000000000, 0.8660254037844387076, 1.000000000000000000, 0.8660254037844387076, 1.000000000000000000, 0.8660254037844387076, 1.000000000000000000, 0.8660254037844387076, 1.000000000000000000, 0.8660254037844387076, 1.000000000000000000, 0.8660254037844387076, 1.000000000000000000, 0.8660254037844387076, 1.000000000000000000, 0.8660254037844387076, 1.000000000000000000, 0.8660254037844387076, 1.000000000000000000, 0.8660254037844387076, 1.000000000000000000, 0.8660254037844387076, 1.000000000000000000, 0.8660254037844387076, 1.000000000000000000, 0.8660254037844387076, 1.000000000000000000, 0.8660254037844387076, 1.000000000000000000, 0.8660254037844387076, 1.000000000000000000, 0.8660254037844387076, 1.000000000000000000, 0.8660254037844387076, 1.000000000000000000, 0.8660254037844387076, 1.000000000000000000, 0.8660254037844387076, 1.000000000000000000, 0.8660254037844387076, 1.000000000000000000, 0.8660254037844387076, 1.000000000000000000, 0.8660254037844387076, 1.000000000000000000, 0.8660254037844387076, 1.000000000000000000, 0.8660254037844387076, 1.000000000000000000, 0.8660254037844387076, 1.000000000000000000, 0.8660254037844387076, 1.000000000000000000, 0.8660254037844387076, 1.000000000000000000, 0.8660254037844387076, 1.000000000000000000, 0.8660254037844387076, 1.000000000000000000, 0.8660254037844387076, 1.000000000000000000, 0.8660254037844387076, 1.000000000000000000, 0.8660254037844387076, 1.000000000000000000, 0.8660254037844387076, 1.000000000000000000, 0.8660254037844387076, 1.000000000000000000, 0.8660254037844387076, 1.000000000000000000, 0.8660254037844387076, 1.000000000000000000, 0.8660254037844387076, 1.000000000000000000, 0.8660254037844387076, 1.000000000000000000, 0.8660254037844387076, 1.000000000000000000, 0.8660254037844387076, 1.000000000000000000, 0.8660254037844387076, 1.000000000000000000, 0.8660254037844387076, 1.000000000000000000, 0.8660254037844387076, 1.000000000000000000, 0.8660254037844387076, 1.000000000000000000, 0.8660254037844387076, 1.000000000000000000, 0.8660254037844387076, 1.000000000000000000, 0.8660254037844387076, 1.000000000000000000, 0.8660254037844387076, 1.000000000000000000, 0.8660254037844387076, 1.000000000000000000, 0.8660254037844387076, 1.000000000000000000, 0.8660254037844387076, 1.000000000000000000, 0.8660254037844387076, 1.000000000000000000, 0.8660254037844387076, 1.000000000000000000, 0.8660254037844387076, 1.000000000000000000, 0.8660254037844387076, 1.000000000000000000, 0.8660254037844387076, 1.000000000000000000, 0.8660254037844387076, 1.000000000000000000, 0.8660254037844387076, 1.000000000000000000, 0.8660254037844387076, 1.000000000000000000, 0.8660254037844387076, 1.000000000000000000, 0.8660254037844387076, 1.000000000000000000, 0.8660254037844387076, 1.000000000000000000, 0.8660254037844387076, 1.000000000000000000, 0.8660254037844387076, 1.000000000000000000, 0.8660254037844387076, 1.000000000000000000, 0.8660254037844387076, 1.000000000000000000, 0.8660254037844387076, 1.000000000000000000, 0.8660254037844387076, 1.000000000000000000, 0.8660254037844387076, 1.000000000000000000, 0.8660254037844387076, 1.000000000000000000, 0.8660254037844387076, 1.000000000000000000, 0.8660254037844387076, 1.000000000000000000, 0.8660254037844387076, 1.000000000000000000, 0.8660254037844387076, 1.000000000000000000, 0.8660254037844387076, 1.000000000000000000, 0.8660254037844387076, 1.000000000000000000, 0.8660254037844387076, 1.000000000000000000, 0.8660254037844387076, 1.000000000000000000, 0.8660254037844387076, 1.000000000000000000, 0.8660254037844387076, 1.000000000000000000, 0.8660254037844387076, 1.000000000000000000, 0.8660254037844387076, 1.000000000000000000, 0.8660254037844387076, 1.000000000000000000, 0.8660254037844387076, 1.000000000000000000, 0.8660254037844387076, 1.000000000000000000, 0.8660254037844387076, 1.000000000000000000, 0.8660254037844387076, 1.000000000000000000, 0.8660254037844387076, 1.000000000000000000, 0.8660254037844387076, 1.000000000000000000, 0.8660254037844387076, 1.000000000000000000, 0.8660254037844387076, 1.000000000000000000, 0.8660254037844387076, 1.000000000000000000, 0.8660254037844387076, 1.000000000000000000, 0.8660254037844387076, 1.000000000000000000, 0.8660254037844387076, 1.000000000000000000, 0.8660254037844387076, 1.000000000000000000, 0.8660254037844387076, 1.000000000000000000, 0.8660254037844387076, 1.000000000000000000, 0.8660254037844387076, 1.000000000000000000, 0.8660254037844387076, 1.000000000000000000, 0.8660254037844387076, 1.000000000000000000, 0.8660254037844387076, 1.000000000000000000, 0.8660254037844387076, 1.000000000000000000, 0.8660254037844387076, 1.000000000000000000, 0.8660254037844387076, 1.000000000000000000, 0.8660254037844387076, 1.000000000000000000, 0.8660254037844387076, 1.000000000000000000, 0.8660254037844387076, 1.000000000000000000, 0.8660254037844387076, 1.000000000000000000, 0.8660254037844387076, 1.000000000000000000, 0.8660254037844387076, 1.000000000000000000, 0.8660254037844387076, 1.000000000000000000, 0.8660254037844387076, 1.000000000000000000, 0.8660254037844387076, 1.000000000000000000, 0.8660254037844387076, 1.000000000000000000, 0.8660254037844387076, 1.000000000000000000, 0.8660254037844387076, 1.000000000000000000, 0.8660254037844387076, 1.000000000000000000, 0.8660254037844387076, 1.000000000000000000, 0.8660254037844387076, 1.000000000000000000, 0.8660254037844387076, 1.000000000000000000, 0.8660254037844387076, 1.000000000000000000, 0.8660254037844387076, 1.000000000000000000, 0.8660254037844387076, 1.000000000000000000, 0.8660254037844387076, 1.000000000000000000, 0.8660254037844387076, 1.000000000000000000, 0.8660254037844387076, 1.000000000000000000, 0.8660254037844387076, 1.000000000000000000, 0.8660254037844387076, 1.000000000000000000, 0.8660254037844387076, 1.000000000000000000, 0.8660254037844387076, 1.000000000000000000, 0.8660254037844387076, 1.000000000000000000, 0.8660254037844387076, 1.000000000000000000, 0.8660254037844387076, 1.000000000000000000, 0.8660254037844387076, 1.000000000000000000, 0.8660254037844387076, 1.000000000000000000, 0.8660254037844387076, 1.000000000000000000, 0.8660254037844387076, 1.000000000000000000, 0.8660254037844387076, 1.000000000000000000, 0.8660254037844387076, 1.000000000000000000, 0.8660254037844387076, 1.000000000000000000, 0.8660254037844387076, 1.000000000000000000, 0.8660254037844387076, 1.000000000000000000, 0.8660254037844387076, 1.000000000000000000, 0.8660254037844387076, 1.000000000000000000, 0.8660254037844387076, 1.000000000000000000, 0.8660254037844387076, 1.000000000000000000, 0.8660254037844387076, 1.000000000000000000, 0.8660254037844387076, 1.000000000000000000, 0.8660254037844387076, 1.000000000000000000, 0.8660254037844387076, 1.000000000000000000, 0.8660254037844387076, 1.000000000000000000, 0.8660254037844387076, 1.000000000000000000, 0.8660254037844387076, 1.000000000000000000, 0.8660254037844387076, 1.000000000000000000, 0.8660254037844387076, 1.000000000000000000, 0.8660254037844387076, 1.000000000000000000, 0.8660254037844387076, 1.000000000000000000, 0.8660254037844387076, 1.000000000000000000, 0.8660254037844387076, 1.000000000000000000, 0.8660254037844387076, 1.000000000000000000, 0.8660254037844387076, 1.000000000000000000, 0.8660254037844387076, 1.000000000000000000, 0.8660254037844387076, 1.000000000000000000, 0.8660254037844387076, 1.000000000000000000, 0.8660254037844387076, 1.000000000000000000, 0.8660254037844387076, 1.000000000000000000, 0.8660254037844387076, 1.000000000000000000, 0.8660254037844387076, 1.000000000000000000, 0.8660254037844387076, 1.000000000000000000, 0.8660254037844387076, 1.000000000000000000, 0.8660254037844387076, 1.000000000000000000, 0.8660254037844387076, 1.000000000000000000, 0.8660254037844387076, 1.000000000000000000, 0.8660254037844387076, 1.000000000000000000, 0.8660254037844387076, 1.000000000000000000, 0.8660254037844387076, 1.000000000000000000, 0.8660254037844387076, 1.000000000000000000, 0.8660254037844387076, 1.000000000000000000, 0.8660254037844387076, 1.000000000000000000, 0.8660254037844387076, 1.000000000000000000, 0.8660254037844387076, 1.000000000000000000, 0.8660254037844387076, 1.000000000000000000, 0.8660254037844387076, 1.000000000000000000, 0.8660254037844387076, 1.000000000000000000, 0.8660254037844387076, 1.000000000000000000, 0.8660254037844387076, 1.000000000000000000, 0.8660254037844387076, 1.000000000000000000, 0.8660254037844387076, 1.000000000000000000, 0.8660254037844387076, 1.000000000000000000, 0.8660254037844387076, 1.000000000000000000, 0.8660254037844387076, 1.000000000000000000, 0.8660254037844387076, 1.000000000000000000, 0.8660254037844387076, 1.000000000000000000, 0.8660254037844387076, 1.000000000000000000, 0.8660254037844387076, 1.000000000000000000, 0.8660254037844387076, 1.000000000000000000, 0.8660254037844387076, 1.000000000000000000, 0.8660254037844387076, 1.000000000000000000, 0.8660254037844387076, 1.000000000000000000, 0.8660254037844387076, 1.000000000000000000, 0.8660254037844387076, 1.000000000000000000, 0.9486992175574255892, 0.9366860366984515185 ) ) 
 REPRESENTATION_ITEM ( '' )  );
#13132 = CARTESIAN_POINT ( 'NONE',  ( -10.81189881249999729, 6.242252689847871849, -180.9062500020484094 ) ) ;
#13133 = CARTESIAN_POINT ( 'NONE',  ( -2.293366432827344421E-15, -12.48450537969573659, -0.2187500020483489072 ) ) ;
#13134 = CARTESIAN_POINT ( 'NONE',  ( -2.121150477449813534E-15, -11.54700538379251284, -146.7500000040967905 ) ) ;
#13135 = CARTESIAN_POINT ( 'NONE',  ( 5.405949406249992428, -9.363379034771808662, -130.5937500020483810 ) ) ;
#13136 = CARTESIAN_POINT ( 'NONE',  ( -5.405949406249996869, 9.363379034771805109, -99.84375000204838102 ) ) ;
#13137 = CARTESIAN_POINT ( 'NONE',  ( 9.999999999999998224, 0.000000000000000000, -158.0000000000000000 ) ) ;
#13138 = CARTESIAN_POINT ( 'NONE',  ( -5.405949406250003975, -9.363379034771801557, -110.0312500020483810 ) ) ;
#13139 = CARTESIAN_POINT ( 'NONE',  ( 7.070501591499377789E-16, 11.54700538379251284, -191.0000000040968189 ) ) ;
#13140 = CARTESIAN_POINT ( 'NONE',  ( 5.405949406249992428, -9.363379034771808662, -112.5937500020483810 ) ) ;
#13141 = CARTESIAN_POINT ( 'NONE',  ( 10.81189881249999729, 0.000000000000000000, -189.0312500020484094 ) ) ;
#13142 = EDGE_CURVE ( 'NONE', #17371, #15042, #33789, .T. ) ;
#13143 = CARTESIAN_POINT ( 'NONE',  ( 9.999999999999998224, 0.000000000000000000, -114.4999999999999858 ) ) ;
#13144 = CARTESIAN_POINT ( 'NONE',  ( -9.999999999999998224, 1.224646799147353059E-15, -140.7500000000000000 ) ) ;
#13145 = CARTESIAN_POINT ( 'NONE',  ( -10.00000000000000000, -5.773502691896251982, -7.124999999999964473 ) ) ;
#13146 = CARTESIAN_POINT ( 'NONE',  ( 10.81189881249999729, 6.242252689847867408, -58.21875000204836681 ) ) ;
#13147 = CARTESIAN_POINT ( 'NONE',  ( -10.81189881249999729, 6.242252689847871849, -51.71875000204836681 ) ) ;
#13148 = CARTESIAN_POINT ( 'NONE',  ( 4.999999999999992006, -8.660254037844389075, -179.6250000040968189 ) ) ;
#13149 = CARTESIAN_POINT ( 'NONE',  ( 10.81189881249999907, 6.242252689847868297, -22.40625000204837747 ) ) ;
#13150 = CARTESIAN_POINT ( 'NONE',  ( 5.405949406249992428, -9.363379034771808662, -30.09375000204836326 ) ) ;
#13151 = CARTESIAN_POINT ( 'NONE',  ( 4.999999999999992006, -8.660254037844389075, -105.7499999999999858 ) ) ;
#13152 = CARTESIAN_POINT ( 'NONE',  ( -5.405949406250003975, -9.363379034771801557, -141.3437500020483810 ) ) ;
#13153 = CARTESIAN_POINT ( 'NONE',  ( 9.999999999999996447, -5.773502691896262640, -107.1249999999999858 ) ) ;
#13154 = CARTESIAN_POINT ( 'NONE',  ( 10.81189881249999729, 0.000000000000000000, -34.53125000204837391 ) ) ;
#13155 = CARTESIAN_POINT ( 'NONE',  ( 7.070501591499376803E-16, 11.54700538379251284, -119.0000000040967763 ) ) ;
#13156 = CARTESIAN_POINT ( 'NONE',  ( 7.070501591499377789E-16, 11.54700538379251284, -64.62499999999998579 ) ) ;
#13157 = CARTESIAN_POINT ( 'NONE',  ( -5.405949406249996869, 9.363379034771805109, -134.5312500020484094 ) ) ;
#13158 = CARTESIAN_POINT ( 'NONE',  ( 10.81189881249999551, -6.242252689847874514, -117.1562500020483952 ) ) ;
#13159 = ORIENTED_EDGE ( 'NONE', *, *, #5686, .F. ) ;
#13160 = VECTOR ( 'NONE', #33278, 1000.000000000000000 ) ;
#13161 = CARTESIAN_POINT ( 'NONE',  ( 4.999999999999992006, -8.660254037844389075, -128.2499999999999716 ) ) ;
#13162 = CARTESIAN_POINT ( 'NONE',  ( 9.999999999999996447, -5.773502691896262640, -112.0000000040967763 ) ) ;
#13163 = CARTESIAN_POINT ( 'NONE',  ( 10.00000000000076916, -5.773502691895816774, -107.1249999999999574 ) ) ;
#13164 = CARTESIAN_POINT ( 'NONE',  ( 7.644554776091147741E-16, 12.48450537969573659, -63.96875000204837391 ) ) ;
#13165 = ORIENTED_EDGE ( 'NONE', *, *, #32906, .T. ) ;
#13166 = CARTESIAN_POINT ( 'NONE',  ( 7.070501591499377789E-16, 11.54700538379251284, -30.12499999999995026 ) ) ;
#13167 = CC_DESIGN_APPROVAL ( #40954, ( #33910 ) ) ;
#13168 = CARTESIAN_POINT ( 'NONE',  ( -5.000000000000003553, -8.660254037844383745, -17.87500000409675138 ) ) ;
#13169 = CARTESIAN_POINT ( 'NONE',  ( 10.81189881249999729, 6.242252689847867408, -40.40625000204836681 ) ) ;
#13170 = CARTESIAN_POINT ( 'NONE',  ( -10.00000000000076916, 5.773502691895813221, -111.2500000040967620 ) ) ;
#13171 = CARTESIAN_POINT ( 'NONE',  ( -4.999999999999996447, 8.660254037844387298, -34.87500000409676915 ) ) ;
#13172 = LINE ( 'NONE', #6932, #24550 ) ;
#13173 = CARTESIAN_POINT ( 'NONE',  ( 10.81189881249999551, -6.242252689847874514, -138.1562500020484094 ) ) ;
#13174 = AXIS2_PLACEMENT_3D ( 'NONE', #32440, #31591, #32228 ) ;
#13175 = CARTESIAN_POINT ( 'NONE',  ( -5.405949406249996869, 9.363379034771805109, -140.5312500020484094 ) ) ;
#13176 = EDGE_CURVE ( 'NONE', #37116, #34874, #26609, .T. ) ;
#13177 = CARTESIAN_POINT ( 'NONE',  ( -1.040834085586084257E-14, -20.00000000000000355, 22.49999999999999289 ) ) ;
#13178 = ORIENTED_EDGE ( 'NONE', *, *, #1177, .F. ) ;
#13179 = ORIENTED_EDGE ( 'NONE', *, *, #11626, .F. ) ;
#13180 = ORIENTED_EDGE ( 'NONE', *, *, #8656, .F. ) ;
#13181 = CARTESIAN_POINT ( 'NONE',  ( -9.999999999999742428, -5.773502691896402084, -121.5000000040967905 ) ) ;
#13182 = CARTESIAN_POINT ( 'NONE',  ( -2.293366432827344421E-15, -12.48450537969573659, -174.2187500020484094 ) ) ;
#13183 = ORGANIZATION ( 'NAUO-ORG1', 'UNSPECIFIED', 'UNSPECIFIED' ) ;
#13184 = CARTESIAN_POINT ( 'NONE',  ( 10.81189881249999551, -6.242252689847874514, -26.96875000204837747 ) ) ;
#13185 = CARTESIAN_POINT ( 'NONE',  ( 9.999999999999479527, 5.773502691896553074, -144.7500000040967620 ) ) ;
#13186 = CARTESIAN_POINT ( 'NONE',  ( 10.81189881249999729, 6.242252689847867408, -154.2187500020483810 ) ) ;
#13187 = CARTESIAN_POINT ( 'NONE',  ( -2.293366432827344421E-15, -12.48450537969573659, -148.7187500020484094 ) ) ;
#13188 = CARTESIAN_POINT ( 'NONE',  ( -5.000000000000003553, -8.660254037844383745, -116.4999999999999858 ) ) ;
#13189 = CARTESIAN_POINT ( 'NONE',  ( -10.81189881249999729, 6.242252689847871849, -129.7187500020483810 ) ) ;
#13190 = CARTESIAN_POINT ( 'NONE',  ( -2.293366432827344421E-15, -12.48450537969573659, -129.4062500020483810 ) ) ;
#13191 = CARTESIAN_POINT ( 'NONE',  ( 5.405949406249999534, 9.363379034771803333, -22.09375000204835615 ) ) ;
#13192 = CARTESIAN_POINT ( 'NONE',  ( -2.293366432827344421E-15, -12.48450537969573659, -141.2187500020483810 ) ) ;
#13193 = DIRECTION ( 'NONE',  ( 1.000000000000000000, 0.000000000000000000, 0.000000000000000000 ) ) ;
#13194 = CARTESIAN_POINT ( 'NONE',  ( 9.999999999999998224, 0.000000000000000000, -102.5000000000000000 ) ) ;
#13195 = CARTESIAN_POINT ( 'NONE',  ( -4.999999999999996447, 8.660254037844387298, -162.0000000000000000 ) ) ;
#13196 = CARTESIAN_POINT ( 'NONE',  ( 7.070501591499376803E-16, 11.54700538379251284, -56.00000000409676915 ) ) ;
#13197 = CARTESIAN_POINT ( 'NONE',  ( 10.81189881249999551, -6.242252689847874514, -70.46875000204840944 ) ) ;
#13198 = CARTESIAN_POINT ( 'NONE',  ( 5.405949406249992428, -9.363379034771808662, -43.78125000204838102 ) ) ;
#13199 = CARTESIAN_POINT ( 'NONE',  ( 10.81189881249999729, 0.000000000000000000, -53.84375000204835970 ) ) ;
#13200 = CARTESIAN_POINT ( 'NONE',  ( 9.999999999999998224, 0.000000000000000000, -90.87500000409677625 ) ) ;
#13201 = CARTESIAN_POINT ( 'NONE',  ( 7.644554776091147741E-16, 12.48450537969573659, -161.4687500020484094 ) ) ;
#13202 = CARTESIAN_POINT ( 'NONE',  ( -4.999999999999996447, 8.660254037844387298, -129.0000000000000000 ) ) ;
#13203 = CARTESIAN_POINT ( 'NONE',  ( 10.81189881249999551, -6.242252689847874514, -138.1562500020484094 ) ) ;
#13204 = LINE ( 'NONE', #23595, #17176 ) ;
#13205 = CARTESIAN_POINT ( 'NONE',  ( 9.999999999999996447, -5.773502691896262640, -112.0000000040967763 ) ) ;
#13206 = CARTESIAN_POINT ( 'NONE',  ( 9.999999999999998224, 0.000000000000000000, -88.99999999999998579 ) ) ;
#13207 = ORIENTED_EDGE ( 'NONE', *, *, #35723, .F. ) ;
#13208 = CARTESIAN_POINT ( 'NONE',  ( 10.81189881249999729, 6.242252689847867408, -107.9062500020483952 ) ) ;
#13209 = CARTESIAN_POINT ( 'NONE',  ( 5.000000000000000000, 8.660254037844385522, -129.6250000040967620 ) ) ;
#13210 = CARTESIAN_POINT ( 'NONE',  ( -9.999999999999998224, 1.224646799147353059E-15, -34.62500000409676915 ) ) ;
#13211 = CARTESIAN_POINT ( 'NONE',  ( -2.293366432827344421E-15, -12.48450537969573659, -162.4062500020483810 ) ) ;
#13212 = CARTESIAN_POINT ( 'NONE',  ( 5.000000000000000000, 8.660254037844385522, -38.12500000409676915 ) ) ;
#13213 = CYLINDRICAL_SURFACE ( 'NONE', #7669, 9.999999999999998224 ) ;
#13214 = CARTESIAN_POINT ( 'NONE',  ( -10.81189881249999729, 1.324075727343319199E-15, -60.78125000204836681 ) ) ;
#13215 = AXIS2_PLACEMENT_3D ( 'NONE', #2287, #38303, #28179 ) ;
#13216 = CYLINDRICAL_SURFACE ( 'NONE', #34519, 9.999999999999998224 ) ;
#13217 = CARTESIAN_POINT ( 'NONE',  ( 7.644554776091147741E-16, 12.48450537969573659, -163.1562500020484094 ) ) ;
#13218 = CARTESIAN_POINT ( 'NONE',  ( 5.405949406249999534, 9.363379034771803333, -131.5937500020483810 ) ) ;
#13219 = CARTESIAN_POINT ( 'NONE',  ( 9.999999999999998224, 0.000000000000000000, -105.8750000040967763 ) ) ;
#13221 = EDGE_CURVE ( 'NONE', #33014, #3489, #9213, .T. ) ;
#13220 = CARTESIAN_POINT ( 'NONE',  ( 10.00000000000011013, -5.773502691896197803, -195.6250000000000284 ) ) ;
#13222 = ORIENTED_EDGE ( 'NONE', *, *, #12694, .F. ) ;
#13223 =( BOUNDED_CURVE ( )  B_SPLINE_CURVE ( 2, ( #17751, #30947, #18786, #14510, #24696, #40842, #37627 ),
 .UNSPECIFIED., .F., .F. ) 
 B_SPLINE_CURVE_WITH_KNOTS ( ( 3, 2, 2, 3 ),
 ( 0.6231343283582090331, 0.6243781094527364184, 0.6256218905472638037, 0.6268656716417911889 ),
 .UNSPECIFIED. ) 
 CURVE ( )  GEOMETRIC_REPRESENTATION_ITEM ( )  RATIONAL_B_SPLINE_CURVE ( ( 0.9999999999999880096, 0.8660254037844506980, 1.000000000000000000, 0.8660254037844387076, 1.000000000000000000, 0.8660254037844267172, 1.000000000000011990 ) ) 
 REPRESENTATION_ITEM ( '' )  );
#13224 = ADVANCED_FACE ( 'NONE', ( #23221 ), #17565, .T. ) ;
#13225 = CARTESIAN_POINT ( 'NONE',  ( -9.999999999999998224, 0.000000000000000000, -99.99999999999998579 ) ) ;
#13226 = VECTOR ( 'NONE', #36020, 1000.000000000000000 ) ;
#13228 = ORIENTED_EDGE ( 'NONE', *, *, #1014, .T. ) ;
#13227 = CARTESIAN_POINT ( 'NONE',  ( -5.405949406249996869, 9.363379034771805109, -67.03125000204838102 ) ) ;
#13229 = COORDINATED_UNIVERSAL_TIME_OFFSET ( 6, 0, .AHEAD. ) ;
#13231 = ORIENTED_EDGE ( 'NONE', *, *, #6966, .T. ) ;
#13230 = CARTESIAN_POINT ( 'NONE',  ( -5.405949406250003975, -9.363379034771801557, -115.8437500020483810 ) ) ;
#13232 = ORIENTED_EDGE ( 'NONE', *, *, #31490, .F. ) ;
#13233 = CARTESIAN_POINT ( 'NONE',  ( -10.81189881249999729, 1.324075727343319199E-15, -20.09375000204835615 ) ) ;
#13234 = CARTESIAN_POINT ( 'NONE',  ( 5.405949406249992428, -9.363379034771808662, -198.0937500020484094 ) ) ;
#13235 = CARTESIAN_POINT ( 'NONE',  ( 5.405949406249992428, -9.363379034771808662, -49.59375000204838102 ) ) ;
#13236 = DIRECTION ( 'NONE',  ( -0.000000000000000000, -0.000000000000000000, 1.000000000000000000 ) ) ;
#13237 = CARTESIAN_POINT ( 'NONE',  ( 5.000000000000000000, 8.660254037844385522, -25.74999999999996803 ) ) ;
#13238 = EDGE_CURVE ( 'NONE', #29783, #38740, #10579, .T. ) ;
#13239 = CARTESIAN_POINT ( 'NONE',  ( -10.81189881249999729, 1.324075727343319199E-15, -182.0937500020483810 ) ) ;
#13240 = CARTESIAN_POINT ( 'NONE',  ( 7.644554776091147741E-16, 12.48450537969573659, -165.9687500020483810 ) ) ;
#13241 = CARTESIAN_POINT ( 'NONE',  ( 10.81189881249999551, -6.242252689847874514, -152.9687500020484094 ) ) ;
#13242 = CARTESIAN_POINT ( 'NONE',  ( 5.405949406249999534, 9.363379034771803333, -161.5937500020484094 ) ) ;
#13243 = CARTESIAN_POINT ( 'NONE',  ( -5.000000000000003553, -8.660254037844383745, -118.3750000040967905 ) ) ;
#13244 = CARTESIAN_POINT ( 'NONE',  ( 7.070501591499376803E-16, 11.54700538379251284, -193.6250000000000284 ) ) ;
#13245 = CARTESIAN_POINT ( 'NONE',  ( 10.00000000000000000, 5.773502691896255534, -187.8750000000000568 ) ) ;
#13246 = CARTESIAN_POINT ( 'NONE',  ( 7.644554776091147741E-16, 12.48450537969573659, -95.46875000204839523 ) ) ;
#13247 = CARTESIAN_POINT ( 'NONE',  ( -9.999999999999998224, 1.224646799147353059E-15, -137.7499999999999716 ) ) ;
#13248 = CARTESIAN_POINT ( 'NONE',  ( 10.81189881249999907, 6.242252689847868297, -68.90625000204839523 ) ) ;
#13249 = CARTESIAN_POINT ( 'NONE',  ( -9.999999999998969713, -5.773502691896847949, -5.624999999999936939 ) ) ;
#13250 = CARTESIAN_POINT ( 'NONE',  ( 7.644554776091147741E-16, 12.48450537969573659, -186.9687500020483810 ) ) ;
#13251 = EDGE_CURVE ( 'NONE', #23032, #34857, #19411, .T. ) ;
#13252 = CARTESIAN_POINT ( 'NONE',  ( -2.293366432827344421E-15, -12.48450537969573659, -163.9062500020483810 ) ) ;
#13253 = CARTESIAN_POINT ( 'NONE',  ( -5.405949406250003975, -9.363379034771801557, -50.03125000204838813 ) ) ;
#13254 = CARTESIAN_POINT ( 'NONE',  ( 9.999999999999998224, 0.000000000000000000, -135.8750000040967905 ) ) ;
#13255 = CARTESIAN_POINT ( 'NONE',  ( -9.999999999999998224, 1.224646799147353059E-15, -113.7499999999999858 ) ) ;
#13256 = ORIENTED_EDGE ( 'NONE', *, *, #18175, .T. ) ;
#13257 = CARTESIAN_POINT ( 'NONE',  ( -5.405949406250003975, -9.363379034771801557, -146.0312500020483810 ) ) ;
#13258 = CARTESIAN_POINT ( 'NONE',  ( 5.405949406249999534, 9.363379034771803333, -160.2812500020484094 ) ) ;
#13259 = AXIS2_PLACEMENT_3D ( 'NONE', #30871, #21581, #20715 ) ;
#13260 = CARTESIAN_POINT ( 'NONE',  ( -10.81189881249999907, -6.242252689847864744, -195.6562500020484094 ) ) ;
#13261 = DIRECTION ( 'NONE',  ( -1.000000000000000000, -0.000000000000000000, -0.000000000000000000 ) ) ;
#13262 = CARTESIAN_POINT ( 'NONE',  ( 7.644554776091147741E-16, 12.48450537969573659, -92.46875000204838102 ) ) ;
#13263 = ORIENTED_EDGE ( 'NONE', *, *, #5249, .T. ) ;
#13264 = CARTESIAN_POINT ( 'NONE',  ( -4.999999999999996447, 8.660254037844387298, -56.99999999999996447 ) ) ;
#13265 = CARTESIAN_POINT ( 'NONE',  ( 5.405949406249999534, 9.363379034771803333, -185.5937500020483810 ) ) ;
#13266 = CARTESIAN_POINT ( 'NONE',  ( 9.999999999999998224, 0.000000000000000000, -62.37500000409676204 ) ) ;
#13267 = DIRECTION ( 'NONE',  ( -1.000000000000000000, -0.000000000000000000, -0.000000000000000000 ) ) ;
#13268 = CARTESIAN_POINT ( 'NONE',  ( 5.405949406249999534, 9.363379034771803333, -80.78125000204838102 ) ) ;
#13269 = CARTESIAN_POINT ( 'NONE',  ( -2.293366432827344421E-15, -12.48450537969573659, -61.90625000204838813 ) ) ;
#13270 =( BOUNDED_CURVE ( )  B_SPLINE_CURVE ( 2, ( #1361, #14493, #37824, #8266, #21849, #31364, #8482 ),
 .UNSPECIFIED., .F., .F. ) 
 B_SPLINE_CURVE_WITH_KNOTS ( ( 3, 2, 2, 3 ),
 ( 0.6865671641791046831, 0.6878109452736320684, 0.6890547263681594536, 0.6902985074626868389 ),
 .UNSPECIFIED. ) 
 CURVE ( )  GEOMETRIC_REPRESENTATION_ITEM ( )  RATIONAL_B_SPLINE_CURVE ( ( 0.9999999999999761302, 0.8660254037844625774, 1.000000000000000000, 0.8660254037844387076, 1.000000000000000000, 0.8660254037844148378, 1.000000000000023981 ) ) 
 REPRESENTATION_ITEM ( '' )  );
#13271 = CARTESIAN_POINT ( 'NONE',  ( -9.999999999999998224, 1.224646799147353059E-15, -58.62500000409676204 ) ) ;
#13272 = CARTESIAN_POINT ( 'NONE',  ( 5.405949406249992428, -9.363379034771808662, -18.09375000204835260 ) ) ;
#13273 = CARTESIAN_POINT ( 'NONE',  ( -10.81189881249999907, -6.242252689847864744, -183.6562500020483810 ) ) ;
#13274 = CARTESIAN_POINT ( 'NONE',  ( -10.81189881249999907, -6.242252689847864744, -11.15625000204836859 ) ) ;
#13275 = CARTESIAN_POINT ( 'NONE',  ( 9.999999999999866773, -5.773502691896336358, -172.0000000040967620 ) ) ;
#13277 = EDGE_CURVE ( 'NONE', #15678, #33229, #35452, .T. ) ;
#13276 = CYLINDRICAL_SURFACE ( 'NONE', #2053, 9.999999999999998224 ) ;
#13278 = CARTESIAN_POINT ( 'NONE',  ( 9.999999999999998224, 0.000000000000000000, -48.49999999999998579 ) ) ;
#13279 = CYLINDRICAL_SURFACE ( 'NONE', #18303, 9.999999999999998224 ) ;
#13280 = ADVANCED_FACE ( 'NONE', ( #39605 ), #10039, .T. ) ;
#13281 =( BOUNDED_CURVE ( )  B_SPLINE_CURVE ( 2, ( #11762, #31864, #34670, #18888, #11542, #8338, #25376 ),
 .UNSPECIFIED., .F., .F. ) 
 B_SPLINE_CURVE_WITH_KNOTS ( ( 3, 2, 2, 3 ),
 ( 0.6044776119402985870, 0.6057213930348259723, 0.6069651741293533576, 0.6082089552238807428 ),
 .UNSPECIFIED. ) 
 CURVE ( )  GEOMETRIC_REPRESENTATION_ITEM ( )  RATIONAL_B_SPLINE_CURVE ( ( 0.9999999999999880096, 0.8660254037844506980, 1.000000000000000000, 0.8660254037844387076, 1.000000000000000000, 0.8660254037844267172, 1.000000000000011990 ) ) 
 REPRESENTATION_ITEM ( '' )  );
#13282 = CARTESIAN_POINT ( 'NONE',  ( 9.999999999999996447, -5.773502691896262640, -165.6250000000000000 ) ) ;
#13283 = DIRECTION ( 'NONE',  ( 1.000000000000000000, 0.000000000000000000, 0.000000000000000000 ) ) ;
#13284 = ADVANCED_FACE ( 'NONE', ( #33374 ), #3794, .T. ) ;
#13286 = ORIENTED_EDGE ( 'NONE', *, *, #35143, .F. ) ;
#13285 = CARTESIAN_POINT ( 'NONE',  ( 10.81189881249999551, -6.242252689847874514, -91.65625000204838102 ) ) ;
#13287 = DIRECTION ( 'NONE',  ( 1.000000000000000000, 0.000000000000000000, 0.000000000000000000 ) ) ;
#13289 = VERTEX_POINT ( 'NONE', #41526 ) ;
#13288 = CARTESIAN_POINT ( 'NONE',  ( 5.405949406249992428, -9.363379034771808662, -103.5937500020483668 ) ) ;
#13290 = ORIENTED_EDGE ( 'NONE', *, *, #11679, .T. ) ;
#13291 = CARTESIAN_POINT ( 'NONE',  ( -10.81189881249999729, 6.242252689847871849, -30.71875000204834905 ) ) ;
#13292 = CARTESIAN_POINT ( 'NONE',  ( 10.81189881249999551, -6.242252689847874514, -21.15625000204836681 ) ) ;
#13293 = CARTESIAN_POINT ( 'NONE',  ( -2.293366432827344421E-15, -12.48450537969573659, -70.71875000204839523 ) ) ;
#13294 = CARTESIAN_POINT ( 'NONE',  ( 4.999999999999992006, -8.660254037844389075, -173.6250000040968189 ) ) ;
#13295 = CARTESIAN_POINT ( 'NONE',  ( 10.81189881249999551, -6.242252689847874514, -194.9687500020484094 ) ) ;
#13296 = CARTESIAN_POINT ( 'NONE',  ( 7.644554776091147741E-16, 12.48450537969573659, -147.9687500020484094 ) ) ;
#13297 = ADVANCED_FACE ( 'NONE', ( #11741 ), #17786, .T. ) ;
#13298 = DIRECTION ( 'NONE',  ( -0.000000000000000000, -0.000000000000000000, -1.000000000000000000 ) ) ;
#13299 = DIRECTION ( 'NONE',  ( -0.000000000000000000, -0.000000000000000000, -1.000000000000000000 ) ) ;
#13300 = CARTESIAN_POINT ( 'NONE',  ( -5.405949406250003975, -9.363379034771801557, -149.0312500020483810 ) ) ;
#13301 = CARTESIAN_POINT ( 'NONE',  ( 4.999999999999992006, -8.660254037844389075, -5.625000004096769146 ) ) ;
#13302 = CARTESIAN_POINT ( 'NONE',  ( 4.999999999999992006, -8.660254037844389075, -80.24999999999998579 ) ) ;
#13303 = CARTESIAN_POINT ( 'NONE',  ( 5.405949406249992428, -9.363379034771808662, -121.5937500020483952 ) ) ;
#13304 = CARTESIAN_POINT ( 'NONE',  ( -9.999999999999998224, 1.224646799147353059E-15, -103.2500000000000000 ) ) ;
#13305 = CARTESIAN_POINT ( 'NONE',  ( 10.81189881249999907, 6.242252689847868297, -88.40625000204839523 ) ) ;
#13306 = CARTESIAN_POINT ( 'NONE',  ( -5.405949406249996869, 9.363379034771805109, -104.3437500020483810 ) ) ;
#13307 = CARTESIAN_POINT ( 'NONE',  ( 7.644554776091147741E-16, 12.48450537969573659, -80.46875000204838102 ) ) ;
#13308 = CARTESIAN_POINT ( 'NONE',  ( -10.81189881249999729, 1.324075727343319199E-15, -81.78125000204839523 ) ) ;
#13309 = CARTESIAN_POINT ( 'NONE',  ( -4.999999999999996447, 8.660254037844387298, -165.3750000040967905 ) ) ;
#13310 = DIRECTION ( 'NONE',  ( -0.000000000000000000, -0.000000000000000000, 1.000000000000000000 ) ) ;
#13311 = CARTESIAN_POINT ( 'NONE',  ( -10.81189881249999729, 6.242252689847871849, -165.9062500020483810 ) ) ;
#13312 = CARTESIAN_POINT ( 'NONE',  ( -5.405949406250003975, -9.363379034771801557, -180.5312500020483810 ) ) ;
#13313 = CARTESIAN_POINT ( 'NONE',  ( 9.999999999999998224, 0.000000000000000000, -158.3750000040967905 ) ) ;
#13314 = CARTESIAN_POINT ( 'NONE',  ( -9.999999999999742428, -5.773502691896402084, -157.1250000000000000 ) ) ;
#13315 = CARTESIAN_POINT ( 'NONE',  ( 7.644554776091147741E-16, 12.48450537969573659, -5.468750002048355263 ) ) ;
#13316 = DIRECTION ( 'NONE',  ( 1.000000000000000000, 0.000000000000000000, 0.000000000000000000 ) ) ;
#13317 = CARTESIAN_POINT ( 'NONE',  ( 10.81189881249999907, 6.242252689847868297, -112.2187500020483810 ) ) ;
#13318 = CARTESIAN_POINT ( 'NONE',  ( -9.999999999999998224, 1.224646799147353059E-15, -80.74999999999998579 ) ) ;
#13319 = CARTESIAN_POINT ( 'NONE',  ( -10.81189881249999729, 6.242252689847871849, -14.40625000204837036 ) ) ;
#13320 = CARTESIAN_POINT ( 'NONE',  ( 9.999999999999998224, 0.000000000000000000, -89.37500000409677625 ) ) ;
#13321 = DIRECTION ( 'NONE',  ( -0.000000000000000000, -0.000000000000000000, -1.000000000000000000 ) ) ;
#13322 = CARTESIAN_POINT ( 'NONE',  ( 5.405949406249999534, 9.363379034771803333, -110.7812500020483810 ) ) ;
#13323 = CARTESIAN_POINT ( 'NONE',  ( 5.405949406249999534, 9.363379034771803333, -82.28125000204838102 ) ) ;
#13324 = ORIENTED_EDGE ( 'NONE', *, *, #21485, .T. ) ;
#13325 = CARTESIAN_POINT ( 'NONE',  ( -4.999999999999996447, 8.660254037844387298, -84.37500000409677625 ) ) ;
#13326 = DIRECTION ( 'NONE',  ( -0.000000000000000000, -0.000000000000000000, 1.000000000000000000 ) ) ;
#13327 = CARTESIAN_POINT ( 'NONE',  ( -2.293366432827344421E-15, -12.48450537969573659, -42.21875000204835970 ) ) ;
#13328 = ORIENTED_EDGE ( 'NONE', *, *, #28926, .F. ) ;
#13329 = CARTESIAN_POINT ( 'NONE',  ( 9.999999999999998224, 0.000000000000000000, -6.499999999999977796 ) ) ;
#13330 = CARTESIAN_POINT ( 'NONE',  ( 9.999999999999998224, 0.000000000000000000, -144.5000000000000000 ) ) ;
#13331 = CARTESIAN_POINT ( 'NONE',  ( 9.999999999999998224, 0.000000000000000000, -31.99999999999997158 ) ) ;
#13332 = CARTESIAN_POINT ( 'NONE',  ( 9.999999999999996447, -5.773502691896262640, -8.500000004096758488 ) ) ;
#13333 = CARTESIAN_POINT ( 'NONE',  ( 4.999999999999992006, -8.660254037844389075, -191.2500000000000000 ) ) ;
#13334 = CARTESIAN_POINT ( 'NONE',  ( -2.121150477449813534E-15, -11.54700538379251284, -155.7500000040968189 ) ) ;
#13336 = ORIENTED_EDGE ( 'NONE', *, *, #431, .T. ) ;
#13335 = CARTESIAN_POINT ( 'NONE',  ( -10.81189881249999729, 1.324075727343319199E-15, -119.2812500020483952 ) ) ;
#13337 = CARTESIAN_POINT ( 'NONE',  ( 11.54700538379250396, 20.00000000000000711, 45.00000000000009237 ) ) ;
#13338 = ORIENTED_EDGE ( 'NONE', *, *, #13221, .F. ) ;
#13339 = CARTESIAN_POINT ( 'NONE',  ( 5.405949406249992428, -9.363379034771808662, -46.78125000204838813 ) ) ;
#13340 = PERSON_AND_ORGANIZATION ( #11915, #17965 ) ;
#13341 = EDGE_CURVE ( 'NONE', #21669, #22182, #34055, .T. ) ;
#13342 = CARTESIAN_POINT ( 'NONE',  ( -5.405949406250003975, -9.363379034771801557, -91.84375000204838102 ) ) ;
#13343 = CARTESIAN_POINT ( 'NONE',  ( 10.81189881249999551, -6.242252689847874514, -121.6562500020483952 ) ) ;
#13344 = ORIENTED_EDGE ( 'NONE', *, *, #32270, .F. ) ;
#13345 =( BOUNDED_CURVE ( )  B_SPLINE_CURVE ( 2, ( #15128, #2421, #15345, #5865, #38450, #31355, #18597 ),
 .UNSPECIFIED., .F., .F. ) 
 B_SPLINE_CURVE_WITH_KNOTS ( ( 3, 2, 2, 3 ),
 ( 0.3134328358208955390, 0.3146766169154229242, 0.3159203980099503650, 0.3171641791044778058 ),
 .UNSPECIFIED. ) 
 CURVE ( )  GEOMETRIC_REPRESENTATION_ITEM ( )  RATIONAL_B_SPLINE_CURVE ( ( 1.000000000000000000, 0.8660254037844387076, 1.000000000000000000, 0.8660254037844387076, 1.000000000000000000, 0.8660254037844207220, 1.000000000000017986 ) ) 
 REPRESENTATION_ITEM ( '' )  );
#13346 = CARTESIAN_POINT ( 'NONE',  ( -9.999999999999227285, -5.773502691896698735, -112.1249999999999574 ) ) ;
#13347 = CARTESIAN_POINT ( 'NONE',  ( 10.00000000000051159, -5.773502691895965988, -116.1249999999999716 ) ) ;
#13348 = CARTESIAN_POINT ( 'NONE',  ( -10.81189881249999729, 6.242252689847871849, -177.9062500020484094 ) ) ;
#13349 = FACE_BOUND ( 'NONE', #14661, .T. ) ;
#13350 = CARTESIAN_POINT ( 'NONE',  ( 10.81189881249999729, 0.000000000000000000, -128.8437500020484094 ) ) ;
#13351 = CARTESIAN_POINT ( 'NONE',  ( -5.405949406249996869, 9.363379034771805109, -101.3437500020483810 ) ) ;
#13352 = CARTESIAN_POINT ( 'NONE',  ( -4.999999999999996447, 8.660254037844387298, -115.8750000040967905 ) ) ;
#13353 = CARTESIAN_POINT ( 'NONE',  ( -2.293366432827344421E-15, -12.48450537969573659, -109.9062500020483952 ) ) ;
#13354 = CARTESIAN_POINT ( 'NONE',  ( 9.999999999999996447, -5.773502691896262640, -190.0000000040968189 ) ) ;
#13355 = CARTESIAN_POINT ( 'NONE',  ( -10.81189881249999729, 1.324075727343319199E-15, -117.5937500020483810 ) ) ;
#13356 = CARTESIAN_POINT ( 'NONE',  ( -5.405949406249996869, 9.363379034771805109, -185.5312500020484094 ) ) ;
#13357 = CARTESIAN_POINT ( 'NONE',  ( 5.000000000000000000, 8.660254037844385522, -6.625000004096770923 ) ) ;
#13358 = CARTESIAN_POINT ( 'NONE',  ( 9.999999999999998224, 0.000000000000000000, -134.3750000040967905 ) ) ;
#13359 = CARTESIAN_POINT ( 'NONE',  ( -2.121150477449813534E-15, -11.54700538379251284, -131.3750000000000000 ) ) ;
#13360 = CARTESIAN_POINT ( 'NONE',  ( 9.999999999999998224, 0.000000000000000000, -4.999999999999976907 ) ) ;
#13361 = CARTESIAN_POINT ( 'NONE',  ( -10.81189881249999729, 6.242252689847871849, -63.71875000204838102 ) ) ;
#13362 = CARTESIAN_POINT ( 'NONE',  ( 5.405949406249999534, 9.363379034771803333, -49.09375000204838102 ) ) ;
#13363 = CARTESIAN_POINT ( 'NONE',  ( 10.00000000000000000, 5.773502691896255534, -179.2500000040967905 ) ) ;
#13364 = CARTESIAN_POINT ( 'NONE',  ( 5.405949406249999534, 9.363379034771803333, -17.78125000204835970 ) ) ;
#13365 = CARTESIAN_POINT ( 'NONE',  ( -10.81189881249999729, 6.242252689847871849, -32.21875000204835260 ) ) ;
#13366 = CARTESIAN_POINT ( 'NONE',  ( 9.999999999999998224, 0.000000000000000000, -158.3750000040967905 ) ) ;
#13367 = CARTESIAN_POINT ( 'NONE',  ( -5.405949406249996869, 9.363379034771805109, -138.8437500020484094 ) ) ;
#13368 = CARTESIAN_POINT ( 'NONE',  ( -9.999999999999998224, 5.773502691896259087, -101.8749999999999858 ) ) ;
#13369 = CARTESIAN_POINT ( 'NONE',  ( 10.81189881249999907, 6.242252689847868297, -32.90625000204835970 ) ) ;
#13370 = CARTESIAN_POINT ( 'NONE',  ( -4.999999999999996447, 8.660254037844387298, -110.9999999999999858 ) ) ;
#13371 = CARTESIAN_POINT ( 'NONE',  ( 7.070501591499377789E-16, 11.54700538379251284, -70.62500000000000000 ) ) ;
#13372 = CARTESIAN_POINT ( 'NONE',  ( -10.81189881249999729, 6.242252689847871849, -131.4062500020484094 ) ) ;
#13373 = CARTESIAN_POINT ( 'NONE',  ( 10.81189881249999551, -6.242252689847874514, -118.6562500020483952 ) ) ;
#13374 = VERTEX_POINT ( 'NONE', #15188 ) ;
#13375 = CARTESIAN_POINT ( 'NONE',  ( -9.999999999999998224, 1.224646799147353059E-15, -142.2500000000000000 ) ) ;
#13376 = CARTESIAN_POINT ( 'NONE',  ( -10.00000000000000000, -5.773502691896251982, -105.0000000040967763 ) ) ;
#13377 = CARTESIAN_POINT ( 'NONE',  ( 4.999999999999992006, -8.660254037844389075, -146.2500000000000000 ) ) ;
#13378 = CARTESIAN_POINT ( 'NONE',  ( 7.644554776091147741E-16, 12.48450537969573659, -65.46875000204838102 ) ) ;
#13379 = ORIENTED_EDGE ( 'NONE', *, *, #11416, .F. ) ;
#13380 = CARTESIAN_POINT ( 'NONE',  ( -2.121150477449813534E-15, -11.54700538379251284, -36.87499999999996447 ) ) ;
#13381 = CARTESIAN_POINT ( 'NONE',  ( -10.00000000000000000, -5.773502691896251982, -18.00000000409676559 ) ) ;
#13382 = CARTESIAN_POINT ( 'NONE',  ( -10.81189881249999729, 1.324075727343319199E-15, -39.78125000204838102 ) ) ;
#13383 = DIRECTION ( 'NONE',  ( -0.000000000000000000, -0.000000000000000000, 1.000000000000000000 ) ) ;
#13384 = CARTESIAN_POINT ( 'NONE',  ( -2.121150477449813534E-15, -11.54700538379251284, -34.25000000409675494 ) ) ;
#13385 = DIRECTION ( 'NONE',  ( -0.000000000000000000, -0.000000000000000000, 1.000000000000000000 ) ) ;
#13386 = CARTESIAN_POINT ( 'NONE',  ( 10.81189881249999907, 6.242252689847868297, -142.4062500020484094 ) ) ;
#13387 = CARTESIAN_POINT ( 'NONE',  ( 7.070501591499376803E-16, 11.54700538379251284, -122.0000000040967905 ) ) ;
#13388 = ORIENTED_EDGE ( 'NONE', *, *, #39942, .T. ) ;
#13389 =( BOUNDED_CURVE ( )  B_SPLINE_CURVE ( 2, ( #28319, #24877, #42305, #41879, #6287, #9299, #9929 ),
 .UNSPECIFIED., .F., .F. ) 
 B_SPLINE_CURVE_WITH_KNOTS ( ( 3, 2, 2, 3 ),
 ( 0.4514925373134329734, 0.4527363184079603031, 0.4539800995024877439, 0.4552238805970150737 ),
 .UNSPECIFIED. ) 
 CURVE ( )  GEOMETRIC_REPRESENTATION_ITEM ( )  RATIONAL_B_SPLINE_CURVE ( ( 0.9999999999999880096, 0.8660254037844506980, 1.000000000000000000, 0.8660254037844387076, 1.000000000000000000, 0.8660254037844207220, 1.000000000000017986 ) ) 
 REPRESENTATION_ITEM ( '' )  );
#13390 = ORIENTED_EDGE ( 'NONE', *, *, #6442, .T. ) ;
#13391 = ORIENTED_EDGE ( 'NONE', *, *, #40732, .T. ) ;
#13392 = DIRECTION ( 'NONE',  ( -0.000000000000000000, -0.000000000000000000, 1.000000000000000000 ) ) ;
#13393 = CARTESIAN_POINT ( 'NONE',  ( 10.81189881249999729, 0.000000000000000000, -172.3437500020484094 ) ) ;
#13394 = CARTESIAN_POINT ( 'NONE',  ( -10.81189881249999907, -6.242252689847864744, -22.96875000204837747 ) ) ;
#13395 = DIRECTION ( 'NONE',  ( -0.000000000000000000, -0.000000000000000000, 1.000000000000000000 ) ) ;
#13396 = CARTESIAN_POINT ( 'NONE',  ( -5.405949406249996869, 9.363379034771805109, -152.3437500020483810 ) ) ;
#13397 = CARTESIAN_POINT ( 'NONE',  ( 7.644554776091147741E-16, 12.48450537969573659, -143.4687500020483810 ) ) ;
#13398 = EDGE_CURVE ( 'NONE', #27752, #28591, #24497, .T. ) ;
#13399 = CARTESIAN_POINT ( 'NONE',  ( -9.999999999999998224, 1.224646799147353059E-15, -22.24999999999996447 ) ) ;
#13400 = CARTESIAN_POINT ( 'NONE',  ( 5.405949406249999534, 9.363379034771803333, -122.5937500020483952 ) ) ;
#13401 = CARTESIAN_POINT ( 'NONE',  ( 5.405949406249999534, 9.363379034771803333, -134.7812500020483810 ) ) ;
#13402 = CARTESIAN_POINT ( 'NONE',  ( -10.81189881249999729, 1.324075727343319199E-15, -6.593750002048370362 ) ) ;
#13403 = CARTESIAN_POINT ( 'NONE',  ( -10.81189881249999729, -6.242252689847864744, -136.9687500020483810 ) ) ;
#13404 = CARTESIAN_POINT ( 'NONE',  ( 100.0000000000000284, -40.00000000000001421, -160.0000000000000000 ) ) ;
#13405 = CARTESIAN_POINT ( 'NONE',  ( -9.999999999999998224, 1.224646799147353059E-15, -182.7500000000000000 ) ) ;
#13406 = CARTESIAN_POINT ( 'NONE',  ( -9.999999999999998224, 5.773502691896259087, -158.8749999999999716 ) ) ;
#13407 = CARTESIAN_POINT ( 'NONE',  ( -9.999999999999998224, 1.224646799147353059E-15, -99.12500000409677625 ) ) ;
#13408 = CARTESIAN_POINT ( 'NONE',  ( 5.405949406249999534, 9.363379034771803333, -73.09375000204838102 ) ) ;
#13409 = CARTESIAN_POINT ( 'NONE',  ( -10.81189881249999907, -6.242252689847864744, -41.15625000204836681 ) ) ;
#13410 = CARTESIAN_POINT ( 'NONE',  ( -10.81189881249999729, 6.242252689847871849, -51.71875000204836681 ) ) ;
#13411 = CARTESIAN_POINT ( 'NONE',  ( 7.070501591499376803E-16, 11.54700538379251284, -57.12499999999997868 ) ) ;
#13412 = CARTESIAN_POINT ( 'NONE',  ( 7.644554776091147741E-16, 12.48450537969573659, -165.9687500020483810 ) ) ;
#13413 = CARTESIAN_POINT ( 'NONE',  ( 9.999999999999998224, 0.000000000000000000, -126.5000000000000000 ) ) ;
#13414 = CARTESIAN_POINT ( 'NONE',  ( -5.405949406250003975, -9.363379034771801557, -137.0312500020484094 ) ) ;
#13415 = CARTESIAN_POINT ( 'NONE',  ( 10.00000000000051159, -5.773502691895965988, -150.6250000000000000 ) ) ;
#13416 = CARTESIAN_POINT ( 'NONE',  ( -5.000000000000003553, -8.660254037844383745, -115.3750000040967905 ) ) ;
#13417 = CARTESIAN_POINT ( 'NONE',  ( 5.000000000000000000, 8.660254037844385522, -91.74999999999998579 ) ) ;
#13418 = VERTEX_POINT ( 'NONE', #27735 ) ;
#13419 = CARTESIAN_POINT ( 'NONE',  ( 5.405949406249999534, 9.363379034771803333, -110.7812500020483810 ) ) ;
#13420 = CARTESIAN_POINT ( 'NONE',  ( 9.999999999999996447, -5.773502691896262640, -134.5000000040967905 ) ) ;
#13421 = CARTESIAN_POINT ( 'NONE',  ( 5.405949406249992428, -9.363379034771808662, -162.2812500020484094 ) ) ;
#13422 = CARTESIAN_POINT ( 'NONE',  ( -10.00000000000000000, -5.773502691896251982, -43.50000000409675494 ) ) ;
#13423 = CARTESIAN_POINT ( 'NONE',  ( -10.81189881249999729, 6.242252689847871849, -50.40625000204837391 ) ) ;
#13424 = VECTOR ( 'NONE', #15867, 1000.000000000000000 ) ;
#13425 = CARTESIAN_POINT ( 'NONE',  ( -9.999999999999998224, 1.224646799147353059E-15, -73.24999999999998579 ) ) ;
#13426 = CARTESIAN_POINT ( 'NONE',  ( -10.81189881249999729, 1.324075727343319199E-15, -161.2812500020484094 ) ) ;
#13427 = CARTESIAN_POINT ( 'NONE',  ( 10.81189881249999551, -6.242252689847874514, -134.9687500020483810 ) ) ;
#13428 = CARTESIAN_POINT ( 'NONE',  ( 9.999999999999998224, 0.000000000000000000, -31.99999999999997158 ) ) ;
#13429 = CARTESIAN_POINT ( 'NONE',  ( -9.999999999999996447, 5.773502691896259975, -173.8750000000000000 ) ) ;
#13430 = VERTEX_POINT ( 'NONE', #34645 ) ;
#13431 = CARTESIAN_POINT ( 'NONE',  ( -2.121150477449813534E-15, -11.54700538379251284, -30.87499999999995381 ) ) ;
#13433 = ORIENTED_EDGE ( 'NONE', *, *, #29248, .T. ) ;
#13432 = CARTESIAN_POINT ( 'NONE',  ( 10.81189881249999907, 6.242252689847868297, -73.40625000204836681 ) ) ;
#13434 = PERSON_AND_ORGANIZATION ( #11915, #17965 ) ;
#13436 = ORIENTED_EDGE ( 'NONE', *, *, #34791, .T. ) ;
#13435 = CARTESIAN_POINT ( 'NONE',  ( -10.81189881249999729, 1.324075727343319199E-15, -120.5937500020483952 ) ) ;
#13437 = ORIENTED_EDGE ( 'NONE', *, *, #41440, .F. ) ;
#13438 = VECTOR ( 'NONE', #23100, 1000.000000000000000 ) ;
#13439 = CARTESIAN_POINT ( 'NONE',  ( 10.81189881249999729, 0.000000000000000000, -17.84375000204835260 ) ) ;
#13440 = CARTESIAN_POINT ( 'NONE',  ( 7.644554776091147741E-16, 12.48450537969573659, -195.9687500020484094 ) ) ;
#13441 = CARTESIAN_POINT ( 'NONE',  ( 5.405949406249999534, 9.363379034771803333, -44.59375000204837391 ) ) ;
#13442 = CARTESIAN_POINT ( 'NONE',  ( 10.00000000000051159, -5.773502691895965988, -71.50000000409676204 ) ) ;
#13443 = CYLINDRICAL_SURFACE ( 'NONE', #4548, 9.999999999999998224 ) ;
#13444 = CARTESIAN_POINT ( 'NONE',  ( 10.81189881249999729, 6.242252689847867408, -178.2187500020484094 ) ) ;
#13445 = AXIS2_PLACEMENT_3D ( 'NONE', #11056, #17315, #3962 ) ;
#13446 = CARTESIAN_POINT ( 'NONE',  ( 5.405949406249992428, -9.363379034771808662, -168.0937500020484094 ) ) ;
#13447 = CARTESIAN_POINT ( 'NONE',  ( -2.293366432827344421E-15, -12.48450537969573659, -150.2187500020483810 ) ) ;
#13448 = CARTESIAN_POINT ( 'NONE',  ( 5.405949406249999534, 9.363379034771803333, -166.0937500020484094 ) ) ;
#13449 = CARTESIAN_POINT ( 'NONE',  ( 10.00000000000051159, -5.773502691895965988, -118.0000000040967763 ) ) ;
#13450 = CARTESIAN_POINT ( 'NONE',  ( 9.999999999999998224, 0.000000000000000000, -161.3750000040967905 ) ) ;
#13451 = CARTESIAN_POINT ( 'NONE',  ( 7.070501591499377789E-16, 11.54700538379251284, -184.6250000000000000 ) ) ;
#13452 = CARTESIAN_POINT ( 'NONE',  ( 5.405949406249999534, 9.363379034771803333, -95.59375000204838102 ) ) ;
#13453 = DIRECTION ( 'NONE',  ( -0.000000000000000000, -0.000000000000000000, 1.000000000000000000 ) ) ;
#13454 = CARTESIAN_POINT ( 'NONE',  ( -10.81189881249999729, 1.324075727343319199E-15, -69.78125000204838102 ) ) ;
#13455 = DIRECTION ( 'NONE',  ( -0.000000000000000000, -0.000000000000000000, -1.000000000000000000 ) ) ;
#13456 = ADVANCED_FACE ( 'NONE', ( #40871 ), #1411, .T. ) ;
#13457 = CARTESIAN_POINT ( 'NONE',  ( -10.81189881249999729, 1.324075727343319199E-15, -189.5937500020483810 ) ) ;
#13458 = CARTESIAN_POINT ( 'NONE',  ( -2.293366432827344421E-15, -12.48450537969573659, -124.9062500020483810 ) ) ;
#13459 = CARTESIAN_POINT ( 'NONE',  ( 5.405949406249992428, -9.363379034771808662, -160.7812500020484094 ) ) ;
#13460 = EDGE_CURVE ( 'NONE', #15306, #24289, #11312, .T. ) ;
#13461 = CARTESIAN_POINT ( 'NONE',  ( -5.405949406249996869, 9.363379034771805109, -50.53125000204835970 ) ) ;
#13462 = CARTESIAN_POINT ( 'NONE',  ( -2.121150477449813534E-15, -11.54700538379251284, -139.2500000040967905 ) ) ;
#13463 = CARTESIAN_POINT ( 'NONE',  ( -9.999999999999998224, 5.773502691896259087, -115.3749999999999858 ) ) ;
#13464 = ORIENTED_EDGE ( 'NONE', *, *, #9837, .F. ) ;
#13465 = CARTESIAN_POINT ( 'NONE',  ( -10.81189881249999729, 1.324075727343319199E-15, -135.7812500020483810 ) ) ;
#13466 = CARTESIAN_POINT ( 'NONE',  ( 5.405949406249999534, 9.363379034771803333, -149.7812500020483810 ) ) ;
#13467 = APPLICATION_CONTEXT ( 'configuration controlled 3d designs of mechanical parts and assemblies' ) ;
#13468 = CARTESIAN_POINT ( 'NONE',  ( -10.81189881249999729, 6.242252689847871849, -188.4062500020484094 ) ) ;
#13469 = CARTESIAN_POINT ( 'NONE',  ( -9.999999999999227285, -5.773502691896698735, -125.6249999999999574 ) ) ;
#13470 = CARTESIAN_POINT ( 'NONE',  ( 5.405949406249992428, -9.363379034771808662, -84.09375000204836681 ) ) ;
#13471 = EDGE_LOOP ( 'NONE', ( #17054, #40046, #32542, #32157 ) ) ;
#13472 = CARTESIAN_POINT ( 'NONE',  ( 9.999999999999998224, 0.000000000000000000, -60.49999999999997158 ) ) ;
#13473 = CARTESIAN_POINT ( 'NONE',  ( 10.81189881249999907, 6.242252689847868297, -182.7187500020484094 ) ) ;
#13474 = CARTESIAN_POINT ( 'NONE',  ( 7.070501591499377789E-16, 11.54700538379251284, -65.00000000409677625 ) ) ;
#13475 = CARTESIAN_POINT ( 'NONE',  ( 9.999999999999998224, 0.000000000000000000, -171.5000000000000000 ) ) ;
#13476 =( BOUNDED_CURVE ( )  B_SPLINE_CURVE ( 2, ( #30035, #34715, #3915, #479, #13595, #688, #33695 ),
 .UNSPECIFIED., .F., .F. ) 
 B_SPLINE_CURVE_WITH_KNOTS ( ( 3, 2, 2, 3 ),
 ( 0.7014925373134330844, 0.7027363184079604697, 0.7039800995024877439, 0.7052238805970151292 ),
 .UNSPECIFIED. ) 
 CURVE ( )  GEOMETRIC_REPRESENTATION_ITEM ( )  RATIONAL_B_SPLINE_CURVE ( ( 0.9999999999999761302, 0.8660254037844625774, 1.000000000000000000, 0.8660254037844387076, 1.000000000000000000, 0.8660254037844148378, 1.000000000000023981 ) ) 
 REPRESENTATION_ITEM ( '' )  );
#13477 = CARTESIAN_POINT ( 'NONE',  ( -10.00000000000012790, -5.773502691896177375, -175.5000000040967905 ) ) ;
#13478 = CARTESIAN_POINT ( 'NONE',  ( -10.81189881249999729, 6.242252689847871849, -75.90625000204838102 ) ) ;
#13479 = AXIS2_PLACEMENT_3D ( 'NONE', #21434, #40627, #8070 ) ;
#13480 = CARTESIAN_POINT ( 'NONE',  ( -10.81189881249999729, 6.242252689847871849, -56.40625000204837391 ) ) ;
#13481 = AXIS2_PLACEMENT_3D ( 'NONE', #23665, #30141, #29497 ) ;
#13482 = CARTESIAN_POINT ( 'NONE',  ( 4.999999999999992006, -8.660254037844389075, -56.62500000409676204 ) ) ;
#13483 = CARTESIAN_POINT ( 'NONE',  ( 10.81189881249999907, 6.242252689847868297, -13.21875000204836148 ) ) ;
#13484 = DIRECTION ( 'NONE',  ( 1.000000000000000000, 0.000000000000000000, 0.000000000000000000 ) ) ;
#13485 = CARTESIAN_POINT ( 'NONE',  ( -2.293366432827344421E-15, -12.48450537969573659, -187.9062500020484094 ) ) ;
#13486 = CARTESIAN_POINT ( 'NONE',  ( -2.293366432827344421E-15, -12.48450537969573659, -10.90625000204836681 ) ) ;
#13487 = CARTESIAN_POINT ( 'NONE',  ( -9.999999999999998224, 1.224646799147353059E-15, -172.6250000040968189 ) ) ;
#13488 = CARTESIAN_POINT ( 'NONE',  ( 4.999999999999992006, -8.660254037844389075, -161.2500000000000000 ) ) ;
#13489 = AXIS2_PLACEMENT_3D ( 'NONE', #29354, #16366, #36251 ) ;
#13490 = CARTESIAN_POINT ( 'NONE',  ( 100.0000000000000142, 19.99999999999999645, -170.0000000000000000 ) ) ;
#13491 = CARTESIAN_POINT ( 'NONE',  ( 0.000000000000000000, 0.000000000000000000, -99.99999999999998579 ) ) ;
#13492 = CARTESIAN_POINT ( 'NONE',  ( -4.999999999999996447, 8.660254037844387298, -169.5000000000000000 ) ) ;
#13493 = DIRECTION ( 'NONE',  ( -0.000000000000000000, -0.000000000000000000, 1.000000000000000000 ) ) ;
#13495 = VERTEX_POINT ( 'NONE', #24726 ) ;
#13494 = CARTESIAN_POINT ( 'NONE',  ( -10.81189881249999729, 6.242252689847871849, -96.90625000204838102 ) ) ;
#13496 = CARTESIAN_POINT ( 'NONE',  ( -9.999999999999998224, 1.224646799147353059E-15, -181.6250000040967905 ) ) ;
#13498 = VERTEX_POINT ( 'NONE', #8097 ) ;
#13497 = CARTESIAN_POINT ( 'NONE',  ( 10.81189881249999729, 0.000000000000000000, -100.3437500020483810 ) ) ;
#13499 = ORIENTED_EDGE ( 'NONE', *, *, #24915, .T. ) ;
#13500 = CARTESIAN_POINT ( 'NONE',  ( -10.81189881249999729, 1.324075727343319199E-15, -36.59375000204836681 ) ) ;
#13501 = CARTESIAN_POINT ( 'NONE',  ( 10.81189881249999907, 6.242252689847868297, -19.40625000204837747 ) ) ;
#13502 = CARTESIAN_POINT ( 'NONE',  ( 10.81189881249999729, 0.000000000000000000, -74.84375000204838102 ) ) ;
#13503 = CARTESIAN_POINT ( 'NONE',  ( -4.999999999999996447, 8.660254037844387298, -104.9999999999999858 ) ) ;
#13504 = CARTESIAN_POINT ( 'NONE',  ( 10.81189881249999729, 0.000000000000000000, -196.3437500020484094 ) ) ;
#13505 = CARTESIAN_POINT ( 'NONE',  ( -10.81189881249999907, -6.242252689847864744, -148.9687500020484094 ) ) ;
#13506 = VECTOR ( 'NONE', #7961, 1000.000000000000000 ) ;
#13507 = CARTESIAN_POINT ( 'NONE',  ( 9.999999999999998224, 0.000000000000000000, -120.8750000040967905 ) ) ;
#13508 = CARTESIAN_POINT ( 'NONE',  ( 5.405949406249999534, 9.363379034771803333, -145.2812500020483810 ) ) ;
#13509 = CARTESIAN_POINT ( 'NONE',  ( -9.999999999999998224, 5.773502691896259087, -0.2500000040967449433 ) ) ;
#13510 = CARTESIAN_POINT ( 'NONE',  ( -11.54700538379251817, 15.00000000000010836, 49.99999999999998579 ) ) ;
#13511 = CARTESIAN_POINT ( 'NONE',  ( 5.405949406249992428, -9.363379034771808662, -120.0937500020483952 ) ) ;
#13512 = CARTESIAN_POINT ( 'NONE',  ( 9.999999999999479527, 5.773502691896553074, -141.3750000000000000 ) ) ;
#13513 = CARTESIAN_POINT ( 'NONE',  ( 10.81189881249999729, 0.000000000000000000, -91.53125000204838102 ) ) ;
#13514 = ADVANCED_FACE ( 'NONE', ( #28385 ), #11095, .T. ) ;
#13515 = CARTESIAN_POINT ( 'NONE',  ( 5.405949406249999534, 9.363379034771803333, -109.0937500020483810 ) ) ;
#13516 = CARTESIAN_POINT ( 'NONE',  ( 7.644554776091147741E-16, 12.48450537969573659, -71.46875000204835260 ) ) ;
#13517 = CARTESIAN_POINT ( 'NONE',  ( 7.644554776091147741E-16, 12.48450537969573659, -74.65625000204838102 ) ) ;
#13518 = CARTESIAN_POINT ( 'NONE',  ( 5.000000000000000000, 8.660254037844385522, -159.6250000040967905 ) ) ;
#13519 = EDGE_CURVE ( 'NONE', #22340, #11539, #24298, .T. ) ;
#13520 =( BOUNDED_CURVE ( )  B_SPLINE_CURVE ( 2, ( #27885, #33725, #37805, #7600, #34583, #5013, #30277 ),
 .UNSPECIFIED., .F., .F. ) 
 B_SPLINE_CURVE_WITH_KNOTS ( ( 3, 2, 2, 3 ),
 ( 0.4067164179104478250, 0.4079601990049751548, 0.4092039800995025400, 0.4104477611940299253 ),
 .UNSPECIFIED. ) 
 CURVE ( )  GEOMETRIC_REPRESENTATION_ITEM ( )  RATIONAL_B_SPLINE_CURVE ( ( 0.9999999999999940048, 0.8660254037844447028, 1.000000000000000000, 0.8660254037844387076, 1.000000000000000000, 0.8660254037844327124, 1.000000000000005995 ) ) 
 REPRESENTATION_ITEM ( '' )  );
#13521 = PLANE ( 'NONE',  #24803 ) ;
#13522 = CARTESIAN_POINT ( 'NONE',  ( 7.644554776091147741E-16, 12.48450537969573659, -157.1562500020484094 ) ) ;
#13523 = CARTESIAN_POINT ( 'NONE',  ( 10.81189881249999551, -6.242252689847874514, -175.6562500020484094 ) ) ;
#13524 = CARTESIAN_POINT ( 'NONE',  ( -5.000000000000003553, -8.660254037844383745, -190.0000000000000000 ) ) ;
#13525 = CARTESIAN_POINT ( 'NONE',  ( -10.81189881249999729, 1.324075727343319199E-15, -0.5937500020483654772 ) ) ;
#13526 = CARTESIAN_POINT ( 'NONE',  ( 10.81189881249999551, -6.242252689847874514, -103.4687500020483810 ) ) ;
#13527 = CARTESIAN_POINT ( 'NONE',  ( -9.999999999999998224, 5.773502691896259087, -82.37499999999998579 ) ) ;
#13528 = CARTESIAN_POINT ( 'NONE',  ( 5.405949406249999534, 9.363379034771803333, -5.781250002048377468 ) ) ;
#13529 = CARTESIAN_POINT ( 'NONE',  ( -9.999999999999998224, 1.224646799147353059E-15, -87.12500000409677625 ) ) ;
#13530 = CARTESIAN_POINT ( 'NONE',  ( 11.54700538379253416, -19.99999999999999289, 49.99999999999998579 ) ) ;
#13531 = CC_DESIGN_DATE_AND_TIME_ASSIGNMENT ( #1274, #17861, ( #33910 ) ) ;
#13532 = CARTESIAN_POINT ( 'NONE',  ( 7.644554776091147741E-16, 12.48450537969573659, -104.6562500020483810 ) ) ;
#13533 = CARTESIAN_POINT ( 'NONE',  ( -10.81189881249999729, -6.242252689847864744, -81.65625000204839523 ) ) ;
#13534 = VERTEX_POINT ( 'NONE', #4639 ) ;
#13535 =( BOUNDED_CURVE ( )  B_SPLINE_CURVE ( 2, ( #18782, #41858, #25492, #9076, #18356, #22242, #41651 ),
 .UNSPECIFIED., .F., .F. ) 
 B_SPLINE_CURVE_WITH_KNOTS ( ( 3, 2, 2, 3 ),
 ( 0.1417910447761193959, 0.1430348258706467535, 0.1442786069651741387, 0.1455223880597014963 ),
 .UNSPECIFIED. ) 
 CURVE ( )  GEOMETRIC_REPRESENTATION_ITEM ( )  RATIONAL_B_SPLINE_CURVE ( ( 1.000000000000000000, 0.8660254037844387076, 1.000000000000000000, 0.8660254037844387076, 1.000000000000000000, 0.8660254037844387076, 1.000000000000000000 ) ) 
 REPRESENTATION_ITEM ( '' )  );
#13536 = CARTESIAN_POINT ( 'NONE',  ( -9.999999999999998224, 1.224646799147353059E-15, -85.62500000409677625 ) ) ;
#13537 = CARTESIAN_POINT ( 'NONE',  ( -10.00000000000051337, 5.773502691895962435, -47.87499999999995737 ) ) ;
#13538 = CARTESIAN_POINT ( 'NONE',  ( -10.81189881249999729, 1.324075727343319199E-15, -41.09375000204837391 ) ) ;
#13539 = VERTEX_POINT ( 'NONE', #4855 ) ;
#13540 = CARTESIAN_POINT ( 'NONE',  ( -4.999999999999996447, 8.660254037844387298, -5.999999999999977796 ) ) ;
#13541 = CARTESIAN_POINT ( 'NONE',  ( 9.999999999999998224, 0.000000000000000000, -147.5000000000000000 ) ) ;
#13542 = CARTESIAN_POINT ( 'NONE',  ( -10.00000000000051337, 5.773502691895962435, -45.25000000409674783 ) ) ;
#13543 = CARTESIAN_POINT ( 'NONE',  ( 10.00000000000000000, 5.773502691896255534, -15.75000000409676559 ) ) ;
#13544 = LOCAL_TIME ( 11, 57, 6.000000000000000000, #19990 ) ;
#13545 = EDGE_CURVE ( 'NONE', #223, #18722, #37871, .T. ) ;
#13546 = CARTESIAN_POINT ( 'NONE',  ( -9.999999999999998224, 5.773502691896259087, -193.3750000000000000 ) ) ;
#13547 = CARTESIAN_POINT ( 'NONE',  ( -9.999999999999998224, 1.224646799147353059E-15, -156.1250000040967905 ) ) ;
#13549 = VERTEX_POINT ( 'NONE', #21462 ) ;
#13548 = CARTESIAN_POINT ( 'NONE',  ( 7.644554776091147741E-16, 12.48450537969573659, -116.6562500020483952 ) ) ;
#13550 = CARTESIAN_POINT ( 'NONE',  ( 10.00000000000051159, -5.773502691895965988, -74.50000000409676204 ) ) ;
#13551 = ORIENTED_EDGE ( 'NONE', *, *, #14202, .F. ) ;
#13552 = CARTESIAN_POINT ( 'NONE',  ( -10.81189881249999907, -6.242252689847864744, -45.65625000204837391 ) ) ;
#13553 = DATE_AND_TIME ( #13970, #21470 ) ;
#13554 = CARTESIAN_POINT ( 'NONE',  ( 7.644554776091147741E-16, 12.48450537969573659, -98.46875000204839523 ) ) ;
#13555 = CARTESIAN_POINT ( 'NONE',  ( 7.644554776091147741E-16, 12.48450537969573659, -125.6562500020483810 ) ) ;
#13556 = ORIENTED_EDGE ( 'NONE', *, *, #11329, .T. ) ;
#13557 = LINE ( 'NONE', #3444, #28028 ) ;
#13558 = CARTESIAN_POINT ( 'NONE',  ( 5.405949406249999534, 9.363379034771803333, -172.2812500020484094 ) ) ;
#13559 = CARTESIAN_POINT ( 'NONE',  ( 9.999999999999612754, 5.773502691896477579, -155.2500000040967905 ) ) ;
#13560 = CARTESIAN_POINT ( 'NONE',  ( 5.405949406249992428, -9.363379034771808662, -135.0937500020483810 ) ) ;
#13561 = CARTESIAN_POINT ( 'NONE',  ( 10.81189881249999907, 6.242252689847868297, -97.21875000204836681 ) ) ;
#13562 = CARTESIAN_POINT ( 'NONE',  ( 9.999999999999998224, 0.000000000000000000, -155.0000000000000000 ) ) ;
#13563 = CARTESIAN_POINT ( 'NONE',  ( 5.405949406249999534, 9.363379034771803333, -103.2812500020483952 ) ) ;
#13564 = CARTESIAN_POINT ( 'NONE',  ( 10.00000000000000000, 5.773502691896255534, -183.7500000040968189 ) ) ;
#13565 = CARTESIAN_POINT ( 'NONE',  ( 5.405949406249999534, 9.363379034771803333, -118.0937500020483810 ) ) ;
#13566 = CARTESIAN_POINT ( 'NONE',  ( -5.405949406250003975, -9.363379034771801557, -174.5312500020484094 ) ) ;
#13567 = CARTESIAN_POINT ( 'NONE',  ( 7.070501591499376803E-16, 11.54700538379251284, -3.124999999999950262 ) ) ;
#13568 = CARTESIAN_POINT ( 'NONE',  ( 9.999999999999548805, 5.773502691896515771, -181.8749999999999716 ) ) ;
#13569 = CARTESIAN_POINT ( 'NONE',  ( 10.00000000000000000, 5.773502691896255534, -7.874999999999964473 ) ) ;
#13570 = CARTESIAN_POINT ( 'NONE',  ( -10.81189881249999729, 6.242252689847871849, -59.21875000204836681 ) ) ;
#13571 = CARTESIAN_POINT ( 'NONE',  ( -5.405949406249996869, 9.363379034771805109, -39.84375000204837391 ) ) ;
#13572 = CARTESIAN_POINT ( 'NONE',  ( 9.999999999999996447, -5.773502691896262640, -179.5000000040968189 ) ) ;
#13573 = CARTESIAN_POINT ( 'NONE',  ( -10.81189881249999729, 1.324075727343319199E-15, -18.78125000204835970 ) ) ;
#13574 = CARTESIAN_POINT ( 'NONE',  ( 10.81189881249999907, 6.242252689847868297, -26.71875000204837391 ) ) ;
#13575 = CYLINDRICAL_SURFACE ( 'NONE', #38506, 9.999999999999998224 ) ;
#13576 = CARTESIAN_POINT ( 'NONE',  ( -5.405949406250003975, -9.363379034771801557, -127.8437500020483952 ) ) ;
#13577 = CARTESIAN_POINT ( 'NONE',  ( 5.000000000000000000, 8.660254037844385522, -103.7500000000000000 ) ) ;
#13578 = CARTESIAN_POINT ( 'NONE',  ( 5.405949406249999534, 9.363379034771803333, -40.28125000204838102 ) ) ;
#13579 = CARTESIAN_POINT ( 'NONE',  ( 9.999999999999479527, 5.773502691896553074, -119.2500000040967620 ) ) ;
#13580 = CARTESIAN_POINT ( 'NONE',  ( 7.070501591499377789E-16, 11.54700538379251284, -57.12499999999997868 ) ) ;
#13581 = CARTESIAN_POINT ( 'NONE',  ( 10.81189881249999551, -6.242252689847874514, -129.1562500020483810 ) ) ;
#13582 = CARTESIAN_POINT ( 'NONE',  ( 10.81189881249999729, 6.242252689847867408, -110.9062500020483952 ) ) ;
#13583 = VERTEX_POINT ( 'NONE', #14542 ) ;
#13584 = CYLINDRICAL_SURFACE ( 'NONE', #27923, 9.999999999999998224 ) ;
#13585 = CARTESIAN_POINT ( 'NONE',  ( 5.000000000000000000, 8.660254037844385522, -108.6250000040967763 ) ) ;
#13586 = CARTESIAN_POINT ( 'NONE',  ( -10.00000000000025580, 5.773502691896109873, -161.8749999999999716 ) ) ;
#13587 = CARTESIAN_POINT ( 'NONE',  ( -10.81189881249999729, 6.242252689847871849, -69.71875000204838102 ) ) ;
#13588 = EDGE_LOOP ( 'NONE', ( #24252, #15623, #16044, #38313 ) ) ;
#13589 = CARTESIAN_POINT ( 'NONE',  ( 9.999999999999998224, 0.000000000000000000, -36.49999999999997868 ) ) ;
#13590 = EDGE_CURVE ( 'NONE', #22548, #40153, #23836, .T. ) ;
#13591 = CARTESIAN_POINT ( 'NONE',  ( 4.999999999999992006, -8.660254037844389075, -20.62500000409675494 ) ) ;
#13592 = CARTESIAN_POINT ( 'NONE',  ( -5.405949406250003975, -9.363379034771801557, -32.03125000204837391 ) ) ;
#13593 = CARTESIAN_POINT ( 'NONE',  ( -9.999999999999998224, 1.224646799147353059E-15, -34.62500000409676915 ) ) ;
#13594 = CARTESIAN_POINT ( 'NONE',  ( 9.999999999999996447, -5.773502691896262640, -37.00000000409676204 ) ) ;
#13595 = CARTESIAN_POINT ( 'NONE',  ( -4.999999999999996447, 8.660254037844387298, -57.37500000409676204 ) ) ;
#13596 = CARTESIAN_POINT ( 'NONE',  ( 10.81189881249999907, 6.242252689847868297, -139.4062500020484094 ) ) ;
#13597 =( BOUNDED_CURVE ( )  B_SPLINE_CURVE ( 2, ( #17963, #31163, #1594, #27266, #28137, #34397, #40621 ),
 .UNSPECIFIED., .F., .F. ) 
 B_SPLINE_CURVE_WITH_KNOTS ( ( 3, 2, 2, 3 ),
 ( 0.05223880597014930738, 0.05348258706467667184, 0.05472636815920402936, 0.05597014925373139382 ),
 .UNSPECIFIED. ) 
 CURVE ( )  GEOMETRIC_REPRESENTATION_ITEM ( )  RATIONAL_B_SPLINE_CURVE ( ( 0.9999999999999940048, 0.8660254037844447028, 1.000000000000000000, 0.8660254037844387076, 1.000000000000000000, 0.8660254037844334896, 1.000000000000005329 ) ) 
 REPRESENTATION_ITEM ( '' )  );
#13598 = CARTESIAN_POINT ( 'NONE',  ( -9.999999999999998224, 1.224646799147353059E-15, -121.6250000040967905 ) ) ;
#13599 = ORIENTED_EDGE ( 'NONE', *, *, #25277, .F. ) ;
#13600 = ORIENTED_EDGE ( 'NONE', *, *, #17595, .F. ) ;
#13601 = CARTESIAN_POINT ( 'NONE',  ( 9.999999999999998224, 0.000000000000000000, -162.5000000000000000 ) ) ;
#13602 = CARTESIAN_POINT ( 'NONE',  ( 7.644554776091147741E-16, 12.48450537969573659, -176.4687500020483810 ) ) ;
#13603 = CARTESIAN_POINT ( 'NONE',  ( -10.81189881249999907, -6.242252689847864744, -192.6562500020484094 ) ) ;
#13604 = CARTESIAN_POINT ( 'NONE',  ( -10.81189881249999729, 6.242252689847871849, -21.71875000204837036 ) ) ;
#13605 = CARTESIAN_POINT ( 'NONE',  ( 9.999999999999998224, 0.000000000000000000, -123.5000000000000000 ) ) ;
#13606 = CARTESIAN_POINT ( 'NONE',  ( 5.000000000000000000, 8.660254037844385522, -150.2500000000000000 ) ) ;
#13607 = AXIS2_PLACEMENT_3D ( 'NONE', #4457, #17600, #10921 ) ;
#13608 = CARTESIAN_POINT ( 'NONE',  ( -2.293366432827344421E-15, -12.48450537969573659, -157.7187500020483810 ) ) ;
#13609 = VECTOR ( 'NONE', #24330, 1000.000000000000000 ) ;
#13610 = CARTESIAN_POINT ( 'NONE',  ( -2.293366432827344421E-15, -12.48450537969573659, -133.7187500020483810 ) ) ;
#13611 = CARTESIAN_POINT ( 'NONE',  ( 10.00000000000051159, -5.773502691895965988, -116.1249999999999716 ) ) ;
#13612 = CARTESIAN_POINT ( 'NONE',  ( 7.644554776091147741E-16, 12.48450537969573659, -125.4687500020483952 ) ) ;
#13613 = CARTESIAN_POINT ( 'NONE',  ( -5.000000000000003553, -8.660254037844383745, -193.3750000040967905 ) ) ;
#13614 = CARTESIAN_POINT ( 'NONE',  ( -5.405949406250003975, -9.363379034771801557, -134.0312500020484094 ) ) ;
#13615 = CARTESIAN_POINT ( 'NONE',  ( 5.405949406249992428, -9.363379034771808662, -10.59375000204834727 ) ) ;
#13616 = CARTESIAN_POINT ( 'NONE',  ( -5.405949406250003975, -9.363379034771801557, -135.3437500020484094 ) ) ;
#13617 = CARTESIAN_POINT ( 'NONE',  ( 4.999999999999992006, -8.660254037844389075, -129.7499999999999716 ) ) ;
#13618 = CARTESIAN_POINT ( 'NONE',  ( 9.999999999999998224, 0.000000000000000000, -177.8750000040967905 ) ) ;
#13619 = CARTESIAN_POINT ( 'NONE',  ( -10.00000000000000000, -5.773502691896251982, -152.6250000000000284 ) ) ;
#13620 = CARTESIAN_POINT ( 'NONE',  ( 5.405949406249999534, 9.363379034771803333, -1.281250002048373027 ) ) ;
#13621 = CARTESIAN_POINT ( 'NONE',  ( -10.81189881249999729, -6.242252689847864744, -81.46875000204838102 ) ) ;
#13622 = CARTESIAN_POINT ( 'NONE',  ( -10.81189881249999729, 6.242252689847871849, -71.21875000204839523 ) ) ;
#13623 = CARTESIAN_POINT ( 'NONE',  ( 7.644554776091147741E-16, 12.48450537969573659, -43.15625000204838102 ) ) ;
#13624 = CARTESIAN_POINT ( 'NONE',  ( 10.81189881249999907, 6.242252689847868297, -53.71875000204837391 ) ) ;
#13625 = CARTESIAN_POINT ( 'NONE',  ( 10.81189881249999551, -6.242252689847874514, -163.4687500020483810 ) ) ;
#13626 = CARTESIAN_POINT ( 'NONE',  ( 4.999999999999992006, -8.660254037844389075, -129.7499999999999716 ) ) ;
#13627 = CARTESIAN_POINT ( 'NONE',  ( -10.81189881249999729, 6.242252689847871849, -140.4062500020484094 ) ) ;
#13628 = LINE ( 'NONE', #39335, #37178 ) ;
#13629 = CARTESIAN_POINT ( 'NONE',  ( -9.999999999999998224, 5.773502691896259087, -86.87499999999998579 ) ) ;
#13630 = CARTESIAN_POINT ( 'NONE',  ( 7.644554776091147741E-16, 12.48450537969573659, -17.65625000204836681 ) ) ;
#13631 = ORIENTED_EDGE ( 'NONE', *, *, #7629, .T. ) ;
#13632 = CARTESIAN_POINT ( 'NONE',  ( -10.81189881249999729, 1.324075727343319199E-15, -107.2812500020483810 ) ) ;
#13633 = CARTESIAN_POINT ( 'NONE',  ( 7.070501591499377789E-16, 11.54700538379251284, -131.0000000040967905 ) ) ;
#13634 = CARTESIAN_POINT ( 'NONE',  ( 9.999999999999998224, 0.000000000000000000, -177.5000000000000000 ) ) ;
#13635 = CARTESIAN_POINT ( 'NONE',  ( 9.999999999999998224, 0.000000000000000000, -45.87500000409677625 ) ) ;
#13636 = DIRECTION ( 'NONE',  ( 1.000000000000000000, 0.000000000000000000, 0.000000000000000000 ) ) ;
#13637 = CARTESIAN_POINT ( 'NONE',  ( -5.405949406249996869, 9.363379034771805109, -49.03125000204838813 ) ) ;
#13638 =( BOUNDED_CURVE ( )  B_SPLINE_CURVE ( 2, ( #9720, #19642, #12727, #25924, #32826, #6701, #19853 ),
 .UNSPECIFIED., .F., .F. ) 
 B_SPLINE_CURVE_WITH_KNOTS ( ( 3, 2, 2, 3 ),
 ( 0.8507462686567166532, 0.8519900497512440385, 0.8532338308457714238, 0.8544776119402988090 ),
 .UNSPECIFIED. ) 
 CURVE ( )  GEOMETRIC_REPRESENTATION_ITEM ( )  RATIONAL_B_SPLINE_CURVE ( ( 0.9999999999999761302, 0.8660254037844625774, 1.000000000000000000, 0.8660254037844387076, 1.000000000000000000, 0.8660254037844028474, 1.000000000000035971 ) ) 
 REPRESENTATION_ITEM ( '' )  );
#13639 = CARTESIAN_POINT ( 'NONE',  ( -9.999999999999998224, 1.224646799147353059E-15, -194.7500000000000000 ) ) ;
#13640 = CARTESIAN_POINT ( 'NONE',  ( 7.644554776091147741E-16, 12.48450537969573659, -160.1562500020484094 ) ) ;
#13641 = CARTESIAN_POINT ( 'NONE',  ( 5.405949406249992428, -9.363379034771808662, -135.0937500020483810 ) ) ;
#13642 = CARTESIAN_POINT ( 'NONE',  ( -9.999999999999998224, 1.224646799147353059E-15, -139.6250000040967905 ) ) ;
#13643 = CARTESIAN_POINT ( 'NONE',  ( 9.999999999999479527, 5.773502691896553074, -151.8749999999999716 ) ) ;
#13644 = AXIS2_PLACEMENT_3D ( 'NONE', #13404, #3726, #33301 ) ;
#13645 = EDGE_LOOP ( 'NONE', ( #17252, #15517 ) ) ;
#13646 = LINE ( 'NONE', #32896, #15526 ) ;
#13647 = EDGE_CURVE ( 'NONE', #3490, #6420, #13597, .T. ) ;
#13649 = ORIENTED_EDGE ( 'NONE', *, *, #17359, .T. ) ;
#13648 = CARTESIAN_POINT ( 'NONE',  ( -5.405949406250003975, -9.363379034771801557, -62.03125000204837391 ) ) ;
#13650 = DATE_TIME_ROLE ( 'creation_date' ) ;
#13652 = VERTEX_POINT ( 'NONE', #41045 ) ;
#13651 = CARTESIAN_POINT ( 'NONE',  ( 5.405949406249999534, 9.363379034771803333, -118.0937500020483810 ) ) ;
#13653 = CARTESIAN_POINT ( 'NONE',  ( -10.81189881249999729, 1.324075727343319199E-15, -24.59375000204835970 ) ) ;
#13654 = CARTESIAN_POINT ( 'NONE',  ( -2.293366432827344421E-15, -12.48450537969573659, -198.2187500020484379 ) ) ;
#13655 = CARTESIAN_POINT ( 'NONE',  ( 5.405949406249999534, 9.363379034771803333, -49.09375000204838102 ) ) ;
#13656 = FACE_OUTER_BOUND ( 'NONE', #1541, .T. ) ;
#13657 = CARTESIAN_POINT ( 'NONE',  ( -10.00000000000025580, 5.773502691896109873, -151.7500000040967336 ) ) ;
#13658 = CARTESIAN_POINT ( 'NONE',  ( 7.644554776091147741E-16, 12.48450537969573659, -180.9687500020484094 ) ) ;
#13659 = CARTESIAN_POINT ( 'NONE',  ( -10.81189881249999907, -6.242252689847864744, -160.9687500020484094 ) ) ;
#13660 = CARTESIAN_POINT ( 'NONE',  ( 7.644554776091147741E-16, 12.48450537969573659, -152.4687500020483810 ) ) ;
#13661 = CARTESIAN_POINT ( 'NONE',  ( 10.81189881249999729, 6.242252689847867408, -160.2187500020483810 ) ) ;
#13662 = CARTESIAN_POINT ( 'NONE',  ( -9.999999999999998224, 1.224646799147353059E-15, -200.0000000000000000 ) ) ;
#13663 = CARTESIAN_POINT ( 'NONE',  ( 4.999999999999992006, -8.660254037844389075, -177.7500000000000284 ) ) ;
#13664 = CARTESIAN_POINT ( 'NONE',  ( -10.81189881249999729, 6.242252689847871849, -98.21875000204838102 ) ) ;
#13665 = EDGE_CURVE ( 'NONE', #10245, #39524, #5944, .T. ) ;
#13666 = CARTESIAN_POINT ( 'NONE',  ( 5.000000000000000000, 8.660254037844385522, -34.74999999999997868 ) ) ;
#13667 = CARTESIAN_POINT ( 'NONE',  ( -5.405949406250003975, -9.363379034771801557, -69.53125000204838102 ) ) ;
#13668 = CARTESIAN_POINT ( 'NONE',  ( -9.999999999999998224, 1.224646799147353059E-15, -81.12500000409677625 ) ) ;
#13669 = CARTESIAN_POINT ( 'NONE',  ( 5.405949406249992428, -9.363379034771808662, -183.0937500020483810 ) ) ;
#13670 = CARTESIAN_POINT ( 'NONE',  ( 5.405949406249992428, -9.363379034771808662, -120.2812500020483952 ) ) ;
#13671 = VECTOR ( 'NONE', #9350, 1000.000000000000000 ) ;
#13672 = CARTESIAN_POINT ( 'NONE',  ( 5.405949406249992428, -9.363379034771808662, -159.2812500020484094 ) ) ;
#13673 = CARTESIAN_POINT ( 'NONE',  ( 10.81189881249999729, 0.000000000000000000, -51.03125000204835970 ) ) ;
#13674 = CARTESIAN_POINT ( 'NONE',  ( 10.00000000000000000, 5.773502691896255534, -138.7500000040967905 ) ) ;
#13675 = CARTESIAN_POINT ( 'NONE',  ( -4.999999999999996447, 8.660254037844387298, -104.9999999999999858 ) ) ;
#13676 = EDGE_CURVE ( 'NONE', #23080, #30728, #22446, .T. ) ;
#13677 = VERTEX_POINT ( 'NONE', #1162 ) ;
#13678 = CARTESIAN_POINT ( 'NONE',  ( 5.405949406249999534, 9.363379034771803333, -136.2812500020483810 ) ) ;
#13679 = CARTESIAN_POINT ( 'NONE',  ( -5.405949406250003975, -9.363379034771801557, -152.0312500020484094 ) ) ;
#13680 = CARTESIAN_POINT ( 'NONE',  ( 10.81189881249999907, 6.242252689847868297, -187.4062500020484379 ) ) ;
#13681 = CARTESIAN_POINT ( 'NONE',  ( -10.81189881249999907, -6.242252689847864744, -79.96875000204836681 ) ) ;
#13682 = VERTEX_POINT ( 'NONE', #953 ) ;
#13683 = CARTESIAN_POINT ( 'NONE',  ( -5.000000000000003553, -8.660254037844383745, -54.99999999999996447 ) ) ;
#13684 = CARTESIAN_POINT ( 'NONE',  ( -5.405949406250003975, -9.363379034771801557, -178.8437500020483810 ) ) ;
#13685 = CARTESIAN_POINT ( 'NONE',  ( -4.999999999999996447, 8.660254037844387298, -67.87500000409677625 ) ) ;
#13686 = CARTESIAN_POINT ( 'NONE',  ( -2.121150477449813534E-15, -11.54700538379251284, -158.3750000000000000 ) ) ;
#13687 = CARTESIAN_POINT ( 'NONE',  ( 10.81189881249999907, 6.242252689847868297, -76.40625000204839523 ) ) ;
#13688 = CARTESIAN_POINT ( 'NONE',  ( 10.81189881249999729, 0.000000000000000000, -60.03125000204836681 ) ) ;
#13689 = CARTESIAN_POINT ( 'NONE',  ( 7.070501591499377789E-16, 11.54700538379251284, -48.50000000409676915 ) ) ;
#13690 = CARTESIAN_POINT ( 'NONE',  ( 10.81189881249999907, 6.242252689847868297, -7.218750002048357040 ) ) ;
#13691 = CARTESIAN_POINT ( 'NONE',  ( -8.675003188131697129, -4.974413003141673784, -0.0003472602639886801512 ) ) ;
#13692 = CARTESIAN_POINT ( 'NONE',  ( -2.293366432827344421E-15, -12.48450537969573659, -181.9062500020483810 ) ) ;
#13693 = CARTESIAN_POINT ( 'NONE',  ( 7.644554776091147741E-16, 12.48450537969573659, -4.156250002048361480 ) ) ;
#13694 = LINE ( 'NONE', #23230, #37308 ) ;
#13695 = CARTESIAN_POINT ( 'NONE',  ( 5.000000000000000000, 8.660254037844385522, -176.1250000040968189 ) ) ;
#13696 = CARTESIAN_POINT ( 'NONE',  ( -10.00000000000038547, 5.773502691896036154, -154.3749999999999716 ) ) ;
#13697 = FACE_OUTER_BOUND ( 'NONE', #14935, .T. ) ;
#13698 = LINE ( 'NONE', #10475, #29645 ) ;
#13700 = ORIENTED_EDGE ( 'NONE', *, *, #39523, .T. ) ;
#13699 = CARTESIAN_POINT ( 'NONE',  ( 10.81189881249999907, 6.242252689847868297, -91.40625000204836681 ) ) ;
#13701 = CARTESIAN_POINT ( 'NONE',  ( 0.000000000000000000, 0.000000000000000000, -200.0000000000000000 ) ) ;
#13702 = EDGE_CURVE ( 'NONE', #26311, #3284, #21427, .T. ) ;
#13704 = VERTEX_POINT ( 'NONE', #20783 ) ;
#13703 = CYLINDRICAL_SURFACE ( 'NONE', #24797, 9.999999999999998224 ) ;
#13705 = VERTEX_POINT ( 'NONE', #14071 ) ;
#13706 = CARTESIAN_POINT ( 'NONE',  ( -5.405949406250003975, -9.363379034771801557, -22.84375000204835615 ) ) ;
#13707 = CARTESIAN_POINT ( 'NONE',  ( -10.81189881249999729, 6.242252689847871849, -20.40625000204837747 ) ) ;
#13708 = PERSON_AND_ORGANIZATION_ROLE ( 'classification_officer' ) ;
#13709 = AXIS2_PLACEMENT_3D ( 'NONE', #16523, #793, #36182 ) ;
#13710 = CARTESIAN_POINT ( 'NONE',  ( -5.405949406249996869, 9.363379034771805109, -69.84375000204836681 ) ) ;
#13711 = CARTESIAN_POINT ( 'NONE',  ( -9.999999999999998224, 1.224646799147353059E-15, -104.7499999999999858 ) ) ;
#13712 = CARTESIAN_POINT ( 'NONE',  ( 9.999999999999996447, -5.773502691896262640, -48.62499999999997868 ) ) ;
#13713 = CARTESIAN_POINT ( 'NONE',  ( 7.644554776091147741E-16, 12.48450537969573659, -192.9687500020483810 ) ) ;
#13714 = CARTESIAN_POINT ( 'NONE',  ( -5.405949406249996869, 9.363379034771805109, -147.8437500020483810 ) ) ;
#13715 = VECTOR ( 'NONE', #21338, 1000.000000000000000 ) ;
#13716 = CARTESIAN_POINT ( 'NONE',  ( 10.81189881249999551, -6.242252689847874514, -147.1562500020484094 ) ) ;
#13717 = CARTESIAN_POINT ( 'NONE',  ( 7.070501591499377789E-16, 11.54700538379251284, -6.500000004096742501 ) ) ;
#13718 = CARTESIAN_POINT ( 'NONE',  ( 9.999999999999998224, 1.224646799147353059E-15, -99.99999999999998579 ) ) ;
#13719 = CARTESIAN_POINT ( 'NONE',  ( -5.405949406249996869, 9.363379034771805109, -123.8437500020483952 ) ) ;
#13720 = DIRECTION ( 'NONE',  ( -0.000000000000000000, -0.000000000000000000, 1.000000000000000000 ) ) ;
#13721 = CARTESIAN_POINT ( 'NONE',  ( -2.293366432827344421E-15, -12.48450537969573659, -91.90625000204838102 ) ) ;
#13722 = CARTESIAN_POINT ( 'NONE',  ( -10.81189881249999729, -6.242252689847864744, -96.46875000204839523 ) ) ;
#13723 =( BOUNDED_CURVE ( )  B_SPLINE_CURVE ( 2, ( #6553, #3111, #30084, #26622, #19282, #19918, #22535 ),
 .UNSPECIFIED., .F., .F. ) 
 B_SPLINE_CURVE_WITH_KNOTS ( ( 3, 2, 2, 3 ),
 ( 0.7686567164179105571, 0.7699004975124379424, 0.7711442786069654387, 0.7723880597014927130 ),
 .UNSPECIFIED. ) 
 CURVE ( )  GEOMETRIC_REPRESENTATION_ITEM ( )  RATIONAL_B_SPLINE_CURVE ( ( 0.9999999999999880096, 0.8660254037844506980, 1.000000000000000000, 0.8660254037844387076, 1.000000000000000000, 0.8660254037844148378, 1.000000000000023981 ) ) 
 REPRESENTATION_ITEM ( '' )  );
#13724 = CARTESIAN_POINT ( 'NONE',  ( 5.405949406249992428, -9.363379034771808662, -72.09375000204836681 ) ) ;
#13725 = CARTESIAN_POINT ( 'NONE',  ( -10.81189881249999907, -6.242252689847864744, -75.65625000204839523 ) ) ;
#13726 = CARTESIAN_POINT ( 'NONE',  ( -5.000000000000003553, -8.660254037844383745, -164.8750000040967905 ) ) ;
#13727 = CARTESIAN_POINT ( 'NONE',  ( 10.81189881249999551, -6.242252689847874514, -156.1562500020483526 ) ) ;
#13728 = CARTESIAN_POINT ( 'NONE',  ( 10.81189881249999729, 0.000000000000000000, -171.0312500020484094 ) ) ;
#13729 = CARTESIAN_POINT ( 'NONE',  ( -10.00000000000031797, 5.773502691896072569, -184.3750000000000568 ) ) ;
#13730 = DIRECTION ( 'NONE',  ( -0.000000000000000000, -0.000000000000000000, 1.000000000000000000 ) ) ;
#13731 = CARTESIAN_POINT ( 'NONE',  ( 4.999999999999992006, -8.660254037844389075, -108.7499999999999858 ) ) ;
#13732 = CARTESIAN_POINT ( 'NONE',  ( -10.81189881249999729, 6.242252689847871849, -107.2187500020483810 ) ) ;
#13733 = CARTESIAN_POINT ( 'NONE',  ( -9.999999999999998224, 1.224646799147353059E-15, -79.24999999999998579 ) ) ;
#13734 = CARTESIAN_POINT ( 'NONE',  ( -5.405949406249996869, 9.363379034771805109, -7.031250002048378356 ) ) ;
#13735 = CARTESIAN_POINT ( 'NONE',  ( 9.999999999999998224, 0.000000000000000000, -92.37500000409677625 ) ) ;
#13736 = CARTESIAN_POINT ( 'NONE',  ( 5.000000000000000000, 8.660254037844385522, -168.6250000040967905 ) ) ;
#13737 = CARTESIAN_POINT ( 'NONE',  ( -10.81189881249999729, 1.324075727343319199E-15, -104.2812500020483810 ) ) ;
#13738 = CARTESIAN_POINT ( 'NONE',  ( 10.81189881249999729, 6.242252689847867408, -85.40625000204836681 ) ) ;
#13739 = CARTESIAN_POINT ( 'NONE',  ( 9.999999999999998224, 0.000000000000000000, -78.87500000409677625 ) ) ;
#13740 = CARTESIAN_POINT ( 'NONE',  ( -10.00000000000076916, 5.773502691895813221, -133.7500000040967905 ) ) ;
#13741 = CARTESIAN_POINT ( 'NONE',  ( -10.81189881249999907, -6.242252689847864744, -30.46875000204835260 ) ) ;
#13742 = EDGE_LOOP ( 'NONE', ( #2129, #3961, #13391, #2182 ) ) ;
#13743 = CARTESIAN_POINT ( 'NONE',  ( -10.00000000000000000, -5.773502691896251982, -10.12499999999998401 ) ) ;
#13744 = CIRCLE ( 'NONE', #37172, 25.00000000000000000 ) ;
#13745 = CARTESIAN_POINT ( 'NONE',  ( -2.293366432827344421E-15, -12.48450537969573659, -27.40625000204838102 ) ) ;
#13746 = CARTESIAN_POINT ( 'NONE',  ( 4.999999999999992006, -8.660254037844389075, -147.7500000000000000 ) ) ;
#13747 = CARTESIAN_POINT ( 'NONE',  ( 9.999999999999998224, 0.000000000000000000, -132.5000000000000000 ) ) ;
#13748 = CARTESIAN_POINT ( 'NONE',  ( -9.999999999999998224, 5.773502691896259087, -13.75000000409676382 ) ) ;
#13749 = CARTESIAN_POINT ( 'NONE',  ( -4.999999999999996447, 8.660254037844387298, -192.0000000000000000 ) ) ;
#13750 = EDGE_CURVE ( 'NONE', #26724, #6996, #28253, .T. ) ;
#13751 = CARTESIAN_POINT ( 'NONE',  ( -10.00000000000051337, 5.773502691895962435, -95.87499999999998579 ) ) ;
#13753 = ORIENTED_EDGE ( 'NONE', *, *, #6261, .F. ) ;
#13752 = CARTESIAN_POINT ( 'NONE',  ( -10.81189881249999729, 1.324075727343319199E-15, -117.7812500020483952 ) ) ;
#13754 = CARTESIAN_POINT ( 'NONE',  ( 9.999999999998969713, 5.773502691896851502, -36.75000000409674072 ) ) ;
#13755 = EDGE_CURVE ( 'NONE', #23881, #15716, #4178, .T. ) ;
#13756 = ORIENTED_EDGE ( 'NONE', *, *, #33653, .T. ) ;
#13757 = ADVANCED_FACE ( 'NONE', ( #5039, #4391 ), #18184, .F. ) ;
#13758 = ORIENTED_EDGE ( 'NONE', *, *, #8291, .F. ) ;
#13759 =( BOUNDED_CURVE ( )  B_SPLINE_CURVE ( 2, ( #15518, #2601, #39047, #6044, #6468, #12496, #32383 ),
 .UNSPECIFIED., .F., .F. ) 
 B_SPLINE_CURVE_WITH_KNOTS ( ( 3, 2, 2, 3 ),
 ( 0.9291044776119405935, 0.9303482587064679787, 0.9315920398009952530, 0.9328358208955226383 ),
 .UNSPECIFIED. ) 
 CURVE ( )  GEOMETRIC_REPRESENTATION_ITEM ( )  RATIONAL_B_SPLINE_CURVE ( ( 0.9999999999999641398, 0.8660254037844745678, 1.000000000000000000, 0.8660254037844387076, 1.000000000000000000, 0.8660254037844148378, 1.000000000000023981 ) ) 
 REPRESENTATION_ITEM ( '' )  );
#13760 = CARTESIAN_POINT ( 'NONE',  ( -5.405949406249996869, 9.363379034771805109, -43.03125000204838102 ) ) ;
#13761 = APPLICATION_PROTOCOL_DEFINITION ( 'international standard', 'config_control_design', 1994, #42159 ) ;
#13762 = CARTESIAN_POINT ( 'NONE',  ( 10.81189881249999551, -6.242252689847874514, -94.46875000204838102 ) ) ;
#13763 = CARTESIAN_POINT ( 'NONE',  ( 10.81189881249999729, 0.000000000000000000, -124.5312500020483952 ) ) ;
#13764 = ORIENTED_EDGE ( 'NONE', *, *, #34132, .T. ) ;
#13765 = FACE_OUTER_BOUND ( 'NONE', #37296, .T. ) ;
#13766 = CARTESIAN_POINT ( 'NONE',  ( 0.000000000000000000, 0.000000000000000000, -200.0000000000000000 ) ) ;
#13767 =( BOUNDED_CURVE ( )  B_SPLINE_CURVE ( 2, ( #15642, #39171, #8979, #12615, #25389, #22563, #42397 ),
 .UNSPECIFIED., .F., .F. ) 
 B_SPLINE_CURVE_WITH_KNOTS ( ( 3, 2, 2, 3 ),
 ( 0.7500000000000001110, 0.7512437810945274963, 0.7524875621890549926, 0.7537313432835822669 ),
 .UNSPECIFIED. ) 
 CURVE ( )  GEOMETRIC_REPRESENTATION_ITEM ( )  RATIONAL_B_SPLINE_CURVE ( ( 0.9999999999999880096, 0.8660254037844506980, 1.000000000000000000, 0.8660254037844387076, 1.000000000000000000, 0.8660254037844148378, 1.000000000000023981 ) ) 
 REPRESENTATION_ITEM ( '' )  );
#13768 = CARTESIAN_POINT ( 'NONE',  ( -5.405949406249996869, 9.363379034771805109, -175.0312500020484094 ) ) ;
#13769 = DIRECTION ( 'NONE',  ( -0.000000000000000000, -0.000000000000000000, 1.000000000000000000 ) ) ;
#13770 = AXIS2_PLACEMENT_3D ( 'NONE', #15200, #18231, #8330 ) ;
#13771 = EDGE_CURVE ( 'NONE', #3969, #26141, #32669, .T. ) ;
#13772 = CARTESIAN_POINT ( 'NONE',  ( 10.81189881249999551, -6.242252689847874514, -134.9687500020483810 ) ) ;
#13773 = CARTESIAN_POINT ( 'NONE',  ( 10.81189881249999729, 0.000000000000000000, -97.34375000204838102 ) ) ;
#13774 = FACE_OUTER_BOUND ( 'NONE', #42682, .T. ) ;
#13775 = CARTESIAN_POINT ( 'NONE',  ( -5.405949406250003975, -9.363379034771801557, -102.5312500020483952 ) ) ;
#13776 = CARTESIAN_POINT ( 'NONE',  ( -9.999999999999998224, 1.224646799147353059E-15, -184.6250000040967905 ) ) ;
#13777 = CARTESIAN_POINT ( 'NONE',  ( 10.81189881249999551, -6.242252689847874514, -104.9687500020483810 ) ) ;
#13778 = CARTESIAN_POINT ( 'NONE',  ( -5.405949406249996869, 9.363379034771805109, -181.0312500020483810 ) ) ;
#13779 =( BOUNDED_CURVE ( )  B_SPLINE_CURVE ( 2, ( #3237, #29994, #16363, #32602, #440, #3445, #26327 ),
 .UNSPECIFIED., .F., .F. ) 
 B_SPLINE_CURVE_WITH_KNOTS ( ( 3, 2, 2, 3 ),
 ( 0.3619402985074628432, 0.3631840796019901729, 0.3644278606965175027, 0.3656716417910448325 ),
 .UNSPECIFIED. ) 
 CURVE ( )  GEOMETRIC_REPRESENTATION_ITEM ( )  RATIONAL_B_SPLINE_CURVE ( ( 0.9999999999999820144, 0.8660254037844566932, 1.000000000000000000, 0.8660254037844387076, 1.000000000000000000, 0.8660254037844327124, 1.000000000000005995 ) ) 
 REPRESENTATION_ITEM ( '' )  );
#13780 = CARTESIAN_POINT ( 'NONE',  ( 9.999999999999998224, 0.000000000000000000, -3.499999999999975131 ) ) ;
#13781 = CARTESIAN_POINT ( 'NONE',  ( 5.405949406249992428, -9.363379034771808662, -178.7812500020484094 ) ) ;
#13782 = CARTESIAN_POINT ( 'NONE',  ( 10.81189881249999907, 6.242252689847868297, -193.4062500020484094 ) ) ;
#13783 = CARTESIAN_POINT ( 'NONE',  ( 5.405949406249992428, -9.363379034771808662, -61.59375000204836681 ) ) ;
#13784 = CARTESIAN_POINT ( 'NONE',  ( 10.81189881249999907, 6.242252689847868297, -41.71875000204835260 ) ) ;
#13785 = CARTESIAN_POINT ( 'NONE',  ( -9.999999999999998224, 5.773502691896259087, -169.7500000040967905 ) ) ;
#13786 = CARTESIAN_POINT ( 'NONE',  ( -10.81189881249999729, 6.242252689847871849, -20.40625000204837747 ) ) ;
#13787 = CARTESIAN_POINT ( 'NONE',  ( -10.81189881249999729, 6.242252689847871849, -24.71875000204837391 ) ) ;
#13788 = CARTESIAN_POINT ( 'NONE',  ( 9.999999999999998224, 0.000000000000000000, -108.8750000040967763 ) ) ;
#13789 = CARTESIAN_POINT ( 'NONE',  ( -10.81189881249999907, -6.242252689847864744, -127.9687500020483810 ) ) ;
#13790 = CARTESIAN_POINT ( 'NONE',  ( 9.999999999999996447, -5.773502691896262640, -105.6249999999999858 ) ) ;
#13791 = CARTESIAN_POINT ( 'NONE',  ( 10.81189881249999551, -6.242252689847874514, -30.15625000204835615 ) ) ;
#13792 = EDGE_CURVE ( 'NONE', #12497, #6518, #30942, .T. ) ;
#13793 = CARTESIAN_POINT ( 'NONE',  ( -2.121150477449813534E-15, -11.54700538379251284, -168.8750000000000000 ) ) ;
#13794 = CARTESIAN_POINT ( 'NONE',  ( -4.999999999999996447, 8.660254037844387298, -55.49999999999996447 ) ) ;
#13795 = CARTESIAN_POINT ( 'NONE',  ( -5.405949406250003975, -9.363379034771801557, -126.5312500020483952 ) ) ;
#13796 = CARTESIAN_POINT ( 'NONE',  ( -10.81189881249999729, 6.242252689847871849, -110.4062500020483810 ) ) ;
#13797 = VERTEX_POINT ( 'NONE', #4607 ) ;
#13798 = CARTESIAN_POINT ( 'NONE',  ( 9.999999999999998224, 0.000000000000000000, -99.87500000409679046 ) ) ;
#13799 = CARTESIAN_POINT ( 'NONE',  ( -2.121150477449813534E-15, -11.54700538379251284, -194.7500000040967905 ) ) ;
#13800 = CARTESIAN_POINT ( 'NONE',  ( -10.81189881249999907, -6.242252689847864744, -55.96875000204836681 ) ) ;
#13801 = ORIENTED_EDGE ( 'NONE', *, *, #7755, .T. ) ;
#13802 = CARTESIAN_POINT ( 'NONE',  ( 7.070501591499377789E-16, 11.54700538379251284, -34.62499999999995737 ) ) ;
#13803 = CARTESIAN_POINT ( 'NONE',  ( -5.405949406249996869, 9.363379034771805109, -34.03125000204837391 ) ) ;
#13804 = CARTESIAN_POINT ( 'NONE',  ( 9.999999999999998224, 0.000000000000000000, -200.0000000000000000 ) ) ;
#13805 = CARTESIAN_POINT ( 'NONE',  ( -9.999999999999998224, 5.773502691896259087, -37.75000000409674783 ) ) ;
#13806 = CARTESIAN_POINT ( 'NONE',  ( 5.000000000000000000, 8.660254037844385522, -161.1250000040967905 ) ) ;
#13807 = VECTOR ( 'NONE', #32172, 1000.000000000000000 ) ;
#13808 = CARTESIAN_POINT ( 'NONE',  ( -10.81189881249999729, 6.242252689847871849, -143.4062500020484094 ) ) ;
#13809 = CARTESIAN_POINT ( 'NONE',  ( 4.999999999999992006, -8.660254037844389075, -119.6250000040967905 ) ) ;
#13810 = EDGE_LOOP ( 'NONE', ( #1431, #16491, #12027, #23516 ) ) ;
#13811 = ADVANCED_FACE ( 'NONE', ( #11277 ), #32017, .T. ) ;
#13812 = EDGE_CURVE ( 'NONE', #23552, #22272, #29292, .T. ) ;
#13813 = EDGE_LOOP ( 'NONE', ( #12596, #30413, #18179, #28086 ) ) ;
#13814 = CARTESIAN_POINT ( 'NONE',  ( 7.070501591499376803E-16, 11.54700538379251284, -114.1249999999999858 ) ) ;
#13815 = DIRECTION ( 'NONE',  ( 1.000000000000000000, 1.502314598737160017E-16, 0.000000000000000000 ) ) ;
#13816 = CARTESIAN_POINT ( 'NONE',  ( -10.81189881249999907, -6.242252689847864744, -165.4687500020484094 ) ) ;
#13817 = CARTESIAN_POINT ( 'NONE',  ( -10.81189881249999729, 6.242252689847871849, -197.4062500020484379 ) ) ;
#13818 = CARTESIAN_POINT ( 'NONE',  ( -2.293366432827344421E-15, -12.48450537969573659, -15.21875000204835615 ) ) ;
#13819 = DIRECTION ( 'NONE',  ( -0.000000000000000000, -0.000000000000000000, 1.000000000000000000 ) ) ;
#13820 = CARTESIAN_POINT ( 'NONE',  ( 5.405949406249992428, -9.363379034771808662, -156.0937500020483810 ) ) ;
#13821 = CARTESIAN_POINT ( 'NONE',  ( 10.81189881249999551, -6.242252689847874514, -139.4687500020483810 ) ) ;
#13822 = CARTESIAN_POINT ( 'NONE',  ( 0.000000000000000000, 0.000000000000000000, -99.99999999999998579 ) ) ;
#13823 = CARTESIAN_POINT ( 'NONE',  ( -5.405949406249996869, 9.363379034771805109, -114.8437500020483810 ) ) ;
#13824 = CARTESIAN_POINT ( 'NONE',  ( -2.121150477449813534E-15, -11.54700538379251284, -196.2500000040967905 ) ) ;
#13825 = CARTESIAN_POINT ( 'NONE',  ( -10.81189881249999729, 6.242252689847871849, -122.4062500020483952 ) ) ;
#13826 = CARTESIAN_POINT ( 'NONE',  ( -10.81189881249999907, -6.242252689847864744, -7.968750002048352599 ) ) ;
#13828 = EDGE_CURVE ( 'NONE', #5087, #24099, #7573, .T. ) ;
#13827 = CARTESIAN_POINT ( 'NONE',  ( -2.293366432827344421E-15, -12.48450537969573659, -135.2187500020483810 ) ) ;
#13829 = CARTESIAN_POINT ( 'NONE',  ( -10.00000000000102496, 5.773502691895664007, -63.25000000409674783 ) ) ;
#13830 = CARTESIAN_POINT ( 'NONE',  ( -9.999999999999998224, 1.224646799147353059E-15, -155.7500000000000000 ) ) ;
#13831 = CARTESIAN_POINT ( 'NONE',  ( 4.999999999999992006, -8.660254037844389075, -21.74999999999996447 ) ) ;
#13832 =( GEOMETRIC_REPRESENTATION_CONTEXT ( 3 ) GLOBAL_UNCERTAINTY_ASSIGNED_CONTEXT ( ( #33340 ) ) GLOBAL_UNIT_ASSIGNED_CONTEXT ( ( #31640, #5940, #25165 ) ) REPRESENTATION_CONTEXT ( 'NONE', 'WORKASPACE' ) );
#13833 = CARTESIAN_POINT ( 'NONE',  ( 5.405949406249992428, -9.363379034771808662, -87.09375000204836681 ) ) ;
#13834 = CARTESIAN_POINT ( 'NONE',  ( -2.293366432827344421E-15, -12.48450537969573659, -63.21875000204839523 ) ) ;
#13835 = CARTESIAN_POINT ( 'NONE',  ( -2.121150477449813534E-15, -11.54700538379251284, -158.7500000040968189 ) ) ;
#13836 = CARTESIAN_POINT ( 'NONE',  ( -5.405949406250003975, -9.363379034771801557, -42.53125000204838102 ) ) ;
#13837 = CARTESIAN_POINT ( 'NONE',  ( -10.81189881249999729, 1.324075727343319199E-15, -48.59375000204838102 ) ) ;
#13838 = CARTESIAN_POINT ( 'NONE',  ( -9.999999999999998224, 1.224646799147353059E-15, -200.0000000000000000 ) ) ;
#13839 = CARTESIAN_POINT ( 'NONE',  ( -2.293366432827344421E-15, -12.48450537969573659, -151.7187500020483810 ) ) ;
#13840 = CARTESIAN_POINT ( 'NONE',  ( -9.999999999999998224, 1.224646799147353059E-15, -128.7499999999999716 ) ) ;
#13841 = CARTESIAN_POINT ( 'NONE',  ( 10.81189881249999729, 0.000000000000000000, -129.0312500020484094 ) ) ;
#13842 = CARTESIAN_POINT ( 'NONE',  ( 0.000000000000000000, 0.000000000000000000, -200.0000000000000000 ) ) ;
#13843 = CARTESIAN_POINT ( 'NONE',  ( -9.999999999999998224, 5.773502691896259087, -83.87499999999998579 ) ) ;
#13844 = CARTESIAN_POINT ( 'NONE',  ( -10.81189881249999729, 6.242252689847871849, -17.40625000204838457 ) ) ;
#13845 = ORIENTED_EDGE ( 'NONE', *, *, #3429, .T. ) ;
#13846 = CARTESIAN_POINT ( 'NONE',  ( -5.405949406249996869, 9.363379034771805109, -107.5312500020483810 ) ) ;
#13847 = CARTESIAN_POINT ( 'NONE',  ( 9.999999999999998224, 0.000000000000000000, -132.8750000040967905 ) ) ;
#13848 = DIRECTION ( 'NONE',  ( -0.000000000000000000, -0.000000000000000000, 1.000000000000000000 ) ) ;
#13849 = CARTESIAN_POINT ( 'NONE',  ( -5.000000000000003553, -8.660254037844383745, -41.87500000409677625 ) ) ;
#13850 =( BOUNDED_CURVE ( )  B_SPLINE_CURVE ( 2, ( #545, #26226, #33133, #9601, #22988, #2929, #40010 ),
 .UNSPECIFIED., .F., .F. ) 
 B_SPLINE_CURVE_WITH_KNOTS ( ( 3, 2, 2, 3 ),
 ( 0.05223880597014930738, 0.05348258706467667184, 0.05472636815920402936, 0.05597014925373139382 ),
 .UNSPECIFIED. ) 
 CURVE ( )  GEOMETRIC_REPRESENTATION_ITEM ( )  RATIONAL_B_SPLINE_CURVE ( ( 0.9999999999999940048, 0.8660254037844447028, 1.000000000000000000, 0.8660254037844387076, 1.000000000000000000, 0.8660254037844334896, 1.000000000000005329 ) ) 
 REPRESENTATION_ITEM ( '' )  );
#13851 = CARTESIAN_POINT ( 'NONE',  ( -9.999999999999998224, 1.224646799147353059E-15, -58.62500000409676204 ) ) ;
#13852 = CARTESIAN_POINT ( 'NONE',  ( 10.81189881249999729, 0.000000000000000000, -49.53125000204838813 ) ) ;
#13853 = CARTESIAN_POINT ( 'NONE',  ( 9.999999999999998224, 0.000000000000000000, -24.49999999999996447 ) ) ;
#13854 = CARTESIAN_POINT ( 'NONE',  ( -10.81189881249999729, 6.242252689847871849, -156.9062500020483810 ) ) ;
#13855 = CARTESIAN_POINT ( 'NONE',  ( -10.81189881249999907, -6.242252689847864744, -132.4687500020483810 ) ) ;
#13856 = DIRECTION ( 'NONE',  ( -0.000000000000000000, -0.000000000000000000, 1.000000000000000000 ) ) ;
#13857 = ORIENTED_EDGE ( 'NONE', *, *, #5970, .F. ) ;
#13858 = CARTESIAN_POINT ( 'NONE',  ( 5.000000000000000000, 8.660254037844385522, -177.2500000000000284 ) ) ;
#13859 = CIRCLE ( 'NONE', #6295, 20.00000000000000000 ) ;
#13860 = LOCAL_TIME ( 11, 57, 6.000000000000000000, #24851 ) ;
#13862 = ORIENTED_EDGE ( 'NONE', *, *, #36084, .T. ) ;
#13861 = CARTESIAN_POINT ( 'NONE',  ( 7.644554776091147741E-16, 12.48450537969573659, -62.65625000204838813 ) ) ;
#13863 = DATE_TIME_ROLE ( 'classification_date' ) ;
#13865 = VERTEX_POINT ( 'NONE', #35674 ) ;
#13864 = CARTESIAN_POINT ( 'NONE',  ( -10.81189881249999907, -6.242252689847864744, -111.4687500020483810 ) ) ;
#13866 = CARTESIAN_POINT ( 'NONE',  ( -5.405949406249996869, 9.363379034771805109, -18.84375000204835260 ) ) ;
#13867 = CARTESIAN_POINT ( 'NONE',  ( -2.293366432827344421E-15, -12.48450537969573659, -189.2187500020484094 ) ) ;
#13869 = ADVANCED_FACE ( 'NONE', ( #22079 ), #28984, .T. ) ;
#13868 = CARTESIAN_POINT ( 'NONE',  ( 7.644554776091147741E-16, 12.48450537969573659, -45.96875000204837391 ) ) ;
#13870 = CARTESIAN_POINT ( 'NONE',  ( -6.596080831067816064, -7.719381798922900551, 5.985441654281310823E-15 ) ) ;
#13871 = CARTESIAN_POINT ( 'NONE',  ( -4.999999999999996447, 8.660254037844387298, -180.0000000000000000 ) ) ;
#13872 = CARTESIAN_POINT ( 'NONE',  ( 10.81189881249999729, 6.242252689847867408, -179.7187500020484094 ) ) ;
#13873 = CARTESIAN_POINT ( 'NONE',  ( 10.81189881249999907, 6.242252689847868297, -163.2187500020483810 ) ) ;
#13874 = CARTESIAN_POINT ( 'NONE',  ( 5.405949406249992428, -9.363379034771808662, -139.5937500020483810 ) ) ;
#13875 = CARTESIAN_POINT ( 'NONE',  ( -10.81189881249999729, 1.324075727343319199E-15, -162.5937500020484094 ) ) ;
#13876 = CARTESIAN_POINT ( 'NONE',  ( -9.999999999999998224, 1.224646799147353059E-15, -94.24999999999998579 ) ) ;
#13877 = CARTESIAN_POINT ( 'NONE',  ( -10.00000000000000000, -5.773502691896251982, -181.1249999999999716 ) ) ;
#13878 = CARTESIAN_POINT ( 'NONE',  ( 5.405949406249992428, -9.363379034771808662, -93.09375000204838102 ) ) ;
#13879 = CARTESIAN_POINT ( 'NONE',  ( 5.000000000000000000, 8.660254037844385522, -138.2499999999999716 ) ) ;
#13880 = CARTESIAN_POINT ( 'NONE',  ( -5.405949406250003975, -9.363379034771801557, -66.53125000204838102 ) ) ;
#13881 = LINE ( 'NONE', #17125, #14351 ) ;
#13882 = CARTESIAN_POINT ( 'NONE',  ( -5.405949406250003975, -9.363379034771801557, -175.8437500020483810 ) ) ;
#13883 = CARTESIAN_POINT ( 'NONE',  ( 10.81189881249999729, 0.000000000000000000, -126.0312500020483952 ) ) ;
#13884 = CARTESIAN_POINT ( 'NONE',  ( 10.81189881249999729, 0.000000000000000000, -162.0312500020484094 ) ) ;
#13885 = CARTESIAN_POINT ( 'NONE',  ( 7.644554776091147741E-16, 12.48450537969573659, -52.15625000204838102 ) ) ;
#13886 = CARTESIAN_POINT ( 'NONE',  ( -5.000000000000003553, -8.660254037844383745, -136.3750000040967905 ) ) ;
#13887 = CARTESIAN_POINT ( 'NONE',  ( -5.000000000000003553, -8.660254037844383745, -108.9999999999999858 ) ) ;
#13888 = EDGE_CURVE ( 'NONE', #7309, #5998, #25237, .T. ) ;
#13889 = VECTOR ( 'NONE', #36176, 1000.000000000000000 ) ;
#13890 =( BOUNDED_CURVE ( )  B_SPLINE_CURVE ( 2, ( #39800, #13249, #10232, #6583, #38966, #7014, #36150 ),
 .UNSPECIFIED., .F., .F. ) 
 B_SPLINE_CURVE_WITH_KNOTS ( ( 3, 2, 2, 3 ),
 ( 0.9664179104477613746, 0.9676616915422887599, 0.9689054726368161452, 0.9701492537313435305 ),
 .UNSPECIFIED. ) 
 CURVE ( )  GEOMETRIC_REPRESENTATION_ITEM ( )  RATIONAL_B_SPLINE_CURVE ( ( 0.9999999999999761302, 0.8660254037844625774, 1.000000000000000000, 0.8660254037844387076, 1.000000000000000000, 0.8660254037844148378, 1.000000000000023981 ) ) 
 REPRESENTATION_ITEM ( '' )  );
#13891 = EDGE_LOOP ( 'NONE', ( #16572, #5713, #22697, #41266 ) ) ;
#13892 = CARTESIAN_POINT ( 'NONE',  ( -5.405949406250003975, -9.363379034771801557, -135.5312500020484094 ) ) ;
#13893 = CARTESIAN_POINT ( 'NONE',  ( 10.81189881249999907, 6.242252689847868297, -148.4062500020484094 ) ) ;
#13894 = CARTESIAN_POINT ( 'NONE',  ( -5.405949406250003975, -9.363379034771801557, -186.5312500020484094 ) ) ;
#13895 = CARTESIAN_POINT ( 'NONE',  ( 5.405949406249999534, 9.363379034771803333, -80.59375000204838102 ) ) ;
#13896 = ORIENTED_EDGE ( 'NONE', *, *, #41795, .T. ) ;
#13897 = CARTESIAN_POINT ( 'NONE',  ( 4.999999999999992006, -8.660254037844389075, -53.24999999999996447 ) ) ;
#13898 = CARTESIAN_POINT ( 'NONE',  ( 5.405949406249999534, 9.363379034771803333, -181.0937500020483810 ) ) ;
#13899 = CARTESIAN_POINT ( 'NONE',  ( 5.000000000000000000, 8.660254037844385522, -65.12500000409676204 ) ) ;
#13900 = CARTESIAN_POINT ( 'NONE',  ( -9.999999999999998224, 1.224646799147353059E-15, -200.0000000000000000 ) ) ;
#13901 = LINE ( 'NONE', #4427, #22927 ) ;
#13902 = CARTESIAN_POINT ( 'NONE',  ( -2.293366432827344421E-15, -12.48450537969573659, -79.90625000204839523 ) ) ;
#13903 = CARTESIAN_POINT ( 'NONE',  ( 5.405949406249992428, -9.363379034771808662, -55.78125000204836681 ) ) ;
#13904 = CARTESIAN_POINT ( 'NONE',  ( 4.999999999999992006, -8.660254037844389075, -49.12500000409678336 ) ) ;
#13905 = CARTESIAN_POINT ( 'NONE',  ( -5.405949406250003975, -9.363379034771801557, -10.84375000204834727 ) ) ;
#13906 = DIRECTION ( 'NONE',  ( -0.000000000000000000, -0.000000000000000000, 1.000000000000000000 ) ) ;
#13907 = CARTESIAN_POINT ( 'NONE',  ( 5.405949406249992428, -9.363379034771808662, -174.2812500020484094 ) ) ;
#13908 = CARTESIAN_POINT ( 'NONE',  ( -2.293366432827344421E-15, -12.48450537969573659, -4.906250002048362369 ) ) ;
#13909 = CARTESIAN_POINT ( 'NONE',  ( 9.999999999999998224, 0.000000000000000000, -87.49999999999998579 ) ) ;
#13910 = CARTESIAN_POINT ( 'NONE',  ( -5.000000000000003553, -8.660254037844383745, -161.5000000000000000 ) ) ;
#13911 = DIRECTION ( 'NONE',  ( 0.000000000000000000, 0.000000000000000000, -1.000000000000000000 ) ) ;
#13912 = DIRECTION ( 'NONE',  ( -0.000000000000000000, -0.000000000000000000, 1.000000000000000000 ) ) ;
#13914 = ORIENTED_EDGE ( 'NONE', *, *, #25430, .F. ) ;
#13913 = CARTESIAN_POINT ( 'NONE',  ( 10.81189881249999729, 0.000000000000000000, -85.53125000204838102 ) ) ;
#13916 = ORIENTED_EDGE ( 'NONE', *, *, #30429, .F. ) ;
#13915 = CARTESIAN_POINT ( 'NONE',  ( 10.81189881249999729, 6.242252689847867408, -103.2187500020483810 ) ) ;
#13917 = ORIENTED_EDGE ( 'NONE', *, *, #30576, .T. ) ;
#13918 = AXIS2_PLACEMENT_3D ( 'NONE', #1058, #40519, #28033 ) ;
#13919 = EDGE_CURVE ( 'NONE', #26513, #3816, #6104, .T. ) ;
#13920 = CARTESIAN_POINT ( 'NONE',  ( -5.405949406250003975, -9.363379034771801557, -30.34375000204836326 ) ) ;
#13921 = CARTESIAN_POINT ( 'NONE',  ( 10.81189881249999729, 0.000000000000000000, -10.53125000204835260 ) ) ;
#13922 = APPROVAL_DATE_TIME ( #30368, #29638 ) ;
#13923 = CARTESIAN_POINT ( 'NONE',  ( -2.293366432827344421E-15, -12.48450537969573659, -67.71875000204838102 ) ) ;
#13924 = CARTESIAN_POINT ( 'NONE',  ( -9.999999999999998224, 1.224646799147353059E-15, -92.74999999999998579 ) ) ;
#13925 = CARTESIAN_POINT ( 'NONE',  ( -9.999999999999998224, 1.224646799147353059E-15, -43.24999999999998579 ) ) ;
#13926 = CARTESIAN_POINT ( 'NONE',  ( -10.81189881249999907, -6.242252689847864744, -184.9687500020484094 ) ) ;
#13927 = CARTESIAN_POINT ( 'NONE',  ( 5.405949406249992428, -9.363379034771808662, -0.09375000204836503315 ) ) ;
#13928 = CARTESIAN_POINT ( 'NONE',  ( 9.999999999999998224, 0.000000000000000000, -147.5000000000000000 ) ) ;
#13929 = CARTESIAN_POINT ( 'NONE',  ( 7.070501591499376803E-16, 11.54700538379251284, -144.1250000000000000 ) ) ;
#13930 = VECTOR ( 'NONE', #2379, 1000.000000000000000 ) ;
#13931 = CARTESIAN_POINT ( 'NONE',  ( -9.999999999999998224, 1.224646799147353059E-15, -200.0000000000000000 ) ) ;
#13932 = CARTESIAN_POINT ( 'NONE',  ( -10.81189881249999729, 1.324075727343319199E-15, -123.5937500020483952 ) ) ;
#13933 = CARTESIAN_POINT ( 'NONE',  ( 9.999999999999998224, 1.224646799147353059E-15, -99.99999999999998579 ) ) ;
#13934 = CARTESIAN_POINT ( 'NONE',  ( 10.81189881249999907, 6.242252689847868297, -94.40625000204836681 ) ) ;
#13935 = CARTESIAN_POINT ( 'NONE',  ( -10.81189881249999729, 1.324075727343319199E-15, -96.59375000204838102 ) ) ;
#13936 = EDGE_CURVE ( 'NONE', #4873, #21320, #42122, .T. ) ;
#13937 = CARTESIAN_POINT ( 'NONE',  ( 5.405949406249992428, -9.363379034771808662, -66.09375000204836681 ) ) ;
#13938 = CARTESIAN_POINT ( 'NONE',  ( -10.81189881249999907, -6.242252689847864744, -72.65625000204836681 ) ) ;
#13939 = CARTESIAN_POINT ( 'NONE',  ( -5.000000000000003553, -8.660254037844383745, -158.8750000040967905 ) ) ;
#13940 = CARTESIAN_POINT ( 'NONE',  ( 10.81189881249999551, -6.242252689847874514, -154.6562500020484094 ) ) ;
#13941 = CARTESIAN_POINT ( 'NONE',  ( 10.81189881249999729, 0.000000000000000000, -172.5312500020484094 ) ) ;
#13942 = DIRECTION ( 'NONE',  ( -0.000000000000000000, -0.000000000000000000, -1.000000000000000000 ) ) ;
#13943 = DIRECTION ( 'NONE',  ( -0.000000000000000000, -0.000000000000000000, -1.000000000000000000 ) ) ;
#13944 = CARTESIAN_POINT ( 'NONE',  ( 5.405949406249992428, -9.363379034771808662, -105.0937500020483810 ) ) ;
#13945 = DIRECTION ( 'NONE',  ( 1.000000000000000000, 0.000000000000000000, 0.000000000000000000 ) ) ;
#13946 = CARTESIAN_POINT ( 'NONE',  ( 10.00000000000000000, 5.773502691896255534, -75.37499999999998579 ) ) ;
#13947 = CARTESIAN_POINT ( 'NONE',  ( 7.644554776091147741E-16, 12.48450537969573659, -2.656250002048360592 ) ) ;
#13948 = CARTESIAN_POINT ( 'NONE',  ( -2.121150477449813534E-15, -11.54700538379251284, -92.75000000409677625 ) ) ;
#13949 = CARTESIAN_POINT ( 'NONE',  ( -4.999999999999996447, 8.660254037844387298, -168.3750000040967905 ) ) ;
#13950 = CARTESIAN_POINT ( 'NONE',  ( 7.644554776091147741E-16, 12.48450537969573659, -100.1562500020483952 ) ) ;
#13951 = CARTESIAN_POINT ( 'NONE',  ( -5.405949406249996869, 9.363379034771805109, -86.53125000204838102 ) ) ;
#13952 = CARTESIAN_POINT ( 'NONE',  ( -9.999999999999998224, 1.224646799147353059E-15, -79.62500000409677625 ) ) ;
#13953 = CARTESIAN_POINT ( 'NONE',  ( 5.000000000000000000, 8.660254037844385522, -19.74999999999996092 ) ) ;
#13954 = CARTESIAN_POINT ( 'NONE',  ( -2.293366432827344421E-15, -12.48450537969573659, -33.21875000204835260 ) ) ;
#13955 = ORIENTED_EDGE ( 'NONE', *, *, #19077, .F. ) ;
#13956 = CARTESIAN_POINT ( 'NONE',  ( -9.999999999999998224, 1.224646799147353059E-15, -7.249999999999978684 ) ) ;
#13957 = CARTESIAN_POINT ( 'NONE',  ( -5.405949406250003975, -9.363379034771801557, -27.53125000204836681 ) ) ;
#13958 = CARTESIAN_POINT ( 'NONE',  ( -10.81189881249999729, 6.242252689847871849, -9.718750002048361480 ) ) ;
#13959 = CARTESIAN_POINT ( 'NONE',  ( 9.999999999999998224, 0.000000000000000000, -45.87500000409677625 ) ) ;
#13960 = CARTESIAN_POINT ( 'NONE',  ( 4.999999999999992006, -8.660254037844389075, -2.625000004096766926 ) ) ;
#13961 = CARTESIAN_POINT ( 'NONE',  ( -10.81189881249999729, 1.324075727343319199E-15, -134.2812500020483810 ) ) ;
#13962 = CARTESIAN_POINT ( 'NONE',  ( -9.999999999999998224, 5.773502691896259087, -187.3750000000000000 ) ) ;
#13963 = CARTESIAN_POINT ( 'NONE',  ( 10.00000000000031619, -5.773502691896077010, -184.0000000040967905 ) ) ;
#13965 = ORIENTED_EDGE ( 'NONE', *, *, #15257, .T. ) ;
#13964 = CARTESIAN_POINT ( 'NONE',  ( 5.405949406249999534, 9.363379034771803333, -107.7812500020483810 ) ) ;
#13966 = CYLINDRICAL_SURFACE ( 'NONE', #29669, 9.999999999999998224 ) ;
#13967 = ORIENTED_EDGE ( 'NONE', *, *, #35080, .F. ) ;
#13968 = ORIENTED_EDGE ( 'NONE', *, *, #109, .T. ) ;
#13969 = CARTESIAN_POINT ( 'NONE',  ( -10.81189881249999729, 1.324075727343319199E-15, -48.78125000204838813 ) ) ;
#13970 = CALENDAR_DATE ( 2026, 28, 9 ) ;
#13971 = CARTESIAN_POINT ( 'NONE',  ( -10.81189881249999729, 1.324075727343319199E-15, -92.09375000204838102 ) ) ;
#13972 = CARTESIAN_POINT ( 'NONE',  ( 5.405949406249999534, 9.363379034771803333, -122.7812500020483952 ) ) ;
#13973 = ORIENTED_EDGE ( 'NONE', *, *, #31492, .F. ) ;
#13974 = CARTESIAN_POINT ( 'NONE',  ( 7.644554776091147741E-16, 12.48450537969573659, -192.9687500020484094 ) ) ;
#13975 = CARTESIAN_POINT ( 'NONE',  ( 5.405949406249999534, 9.363379034771803333, -175.2812500020484094 ) ) ;
#13976 = CARTESIAN_POINT ( 'NONE',  ( -10.81189881249999729, -6.242252689847864744, -126.4687500020483810 ) ) ;
#13977 = CARTESIAN_POINT ( 'NONE',  ( -10.81189881249999729, 1.324075727343319199E-15, -92.09375000204838102 ) ) ;
#13978 = CARTESIAN_POINT ( 'NONE',  ( 0.000000000000000000, 0.000000000000000000, -200.0000000000000000 ) ) ;
#13979 = CARTESIAN_POINT ( 'NONE',  ( -5.405949406250003975, -9.363379034771801557, -104.0312500020483810 ) ) ;
#13980 = CARTESIAN_POINT ( 'NONE',  ( -9.999999999999998224, 5.773502691896259087, -186.2500000040967905 ) ) ;
#13981 = CARTESIAN_POINT ( 'NONE',  ( -10.81189881249999729, 1.324075727343319199E-15, -107.0937500020483810 ) ) ;
#13982 = CARTESIAN_POINT ( 'NONE',  ( 10.81189881249999551, -6.242252689847874514, -177.1562500020484094 ) ) ;
#13983 = CARTESIAN_POINT ( 'NONE',  ( 9.999999999999998224, 0.000000000000000000, -171.5000000000000000 ) ) ;
#13984 = CARTESIAN_POINT ( 'NONE',  ( -5.000000000000003553, -8.660254037844383745, -152.8750000040967905 ) ) ;
#13985 = CARTESIAN_POINT ( 'NONE',  ( -5.405949406250003975, -9.363379034771801557, -192.5312500020484094 ) ) ;
#13986 = CARTESIAN_POINT ( 'NONE',  ( -10.81189881249999729, -6.242252689847864744, -49.96875000204835970 ) ) ;
#13987 = CARTESIAN_POINT ( 'NONE',  ( 10.81189881249999907, 6.242252689847868297, -40.21875000204835970 ) ) ;
#13988 = CARTESIAN_POINT ( 'NONE',  ( 5.000000000000000000, 8.660254037844385522, -170.1250000040968189 ) ) ;
#13989 = CARTESIAN_POINT ( 'NONE',  ( 5.405949406249992428, -9.363379034771808662, -10.78125000204835438 ) ) ;
#13990 = CARTESIAN_POINT ( 'NONE',  ( 7.644554776091147741E-16, 12.48450537969573659, -24.96875000204837391 ) ) ;
#13991 = CARTESIAN_POINT ( 'NONE',  ( 0.000000000000000000, 0.000000000000000000, -99.99999999999998579 ) ) ;
#13992 = CARTESIAN_POINT ( 'NONE',  ( 10.81189881249999551, -6.242252689847874514, -133.4687500020483810 ) ) ;
#13993 = ADVANCED_FACE ( 'NONE', ( #12554 ), #22499, .T. ) ;
#13994 = CARTESIAN_POINT ( 'NONE',  ( -9.999999999999998224, 5.773502691896259087, -107.8749999999999858 ) ) ;
#13995 = CARTESIAN_POINT ( 'NONE',  ( -5.405949406249996869, 9.363379034771805109, -31.03125000204837036 ) ) ;
#13996 = DIRECTION ( 'NONE',  ( -1.000000000000000000, 0.000000000000000000, 0.000000000000000000 ) ) ;
#13997 = EDGE_CURVE ( 'NONE', #37997, #24776, #38461, .T. ) ;
#13998 = CARTESIAN_POINT ( 'NONE',  ( 5.000000000000000000, 8.660254037844385522, -55.74999999999996447 ) ) ;
#13999 = CARTESIAN_POINT ( 'NONE',  ( -10.81189881249999907, -6.242252689847864744, -122.1562500020484094 ) ) ;
#14000 = CARTESIAN_POINT ( 'NONE',  ( -10.81189881249999729, 1.324075727343319199E-15, -105.7812500020483810 ) ) ;
#14001 = ORIENTED_EDGE ( 'NONE', *, *, #1047, .T. ) ;
#14002 = CARTESIAN_POINT ( 'NONE',  ( -10.00000000000025580, 5.773502691896109873, -160.3750000000000000 ) ) ;
#14003 = CARTESIAN_POINT ( 'NONE',  ( 10.00000000000000000, 5.773502691896255534, -102.7500000040967905 ) ) ;
#14004 = DIRECTION ( 'NONE',  ( 1.000000000000000000, 0.000000000000000000, 0.000000000000000000 ) ) ;
#14005 = CARTESIAN_POINT ( 'NONE',  ( -5.405949406249996869, 9.363379034771805109, -56.34375000204835970 ) ) ;
#14006 = VERTEX_POINT ( 'NONE', #42331 ) ;
#14007 = CARTESIAN_POINT ( 'NONE',  ( 9.999999999999998224, 0.000000000000000000, -34.99999999999997868 ) ) ;
#14008 = CARTESIAN_POINT ( 'NONE',  ( -10.81189881249999729, 1.324075727343319199E-15, -36.78125000204837391 ) ) ;
#14009 = LINE ( 'NONE', #9945, #39354 ) ;
#14010 = CARTESIAN_POINT ( 'NONE',  ( 9.999999999999998224, 0.000000000000000000, -29.37500000409676204 ) ) ;
#14011 =( BOUNDED_CURVE ( )  B_SPLINE_CURVE ( 2, ( #10745, #23508, #9030, #20252, #638, #13550, #3437 ),
 .UNSPECIFIED., .F., .F. ) 
 B_SPLINE_CURVE_WITH_KNOTS ( ( 3, 2, 2, 3 ),
 ( 0.6156716417910449435, 0.6169154228855723288, 0.6181592039800996030, 0.6194029850746269883 ),
 .UNSPECIFIED. ) 
 CURVE ( )  GEOMETRIC_REPRESENTATION_ITEM ( )  RATIONAL_B_SPLINE_CURVE ( ( 0.9999999999999761302, 0.8660254037844625774, 1.000000000000000000, 0.8660254037844387076, 1.000000000000000000, 0.8660254037844267172, 1.000000000000011990 ) ) 
 REPRESENTATION_ITEM ( '' )  );
#14012 = CARTESIAN_POINT ( 'NONE',  ( -9.999999999999998224, 1.224646799147353059E-15, -160.6250000040967905 ) ) ;
#14013 = CARTESIAN_POINT ( 'NONE',  ( 10.81189881249999551, -6.242252689847874514, -141.1562500020484094 ) ) ;
#14014 = CARTESIAN_POINT ( 'NONE',  ( 7.070501591499376803E-16, 11.54700538379251284, -129.5000000040967905 ) ) ;
#14015 = VERTEX_POINT ( 'NONE', #12761 ) ;
#14016 =( BOUNDED_CURVE ( )  B_SPLINE_CURVE ( 2, ( #14404, #37088, #34729, #40739, #17864, #30840, #4295 ),
 .UNSPECIFIED., .F., .F. ) 
 B_SPLINE_CURVE_WITH_KNOTS ( ( 3, 2, 2, 3 ),
 ( 0.1268656716417910224, 0.1281094527363183799, 0.1293532338308457652, 0.1305970149253731227 ),
 .UNSPECIFIED. ) 
 CURVE ( )  GEOMETRIC_REPRESENTATION_ITEM ( )  RATIONAL_B_SPLINE_CURVE ( ( 1.000000000000003109, 0.8660254037844358210, 1.000000000000000000, 0.8660254037844387076, 1.000000000000000000, 0.8660254037844387076, 1.000000000000000000 ) ) 
 REPRESENTATION_ITEM ( '' )  );
#14017 = VERTEX_POINT ( 'NONE', #8707 ) ;
#14018 = CARTESIAN_POINT ( 'NONE',  ( 0.000000000000000000, 20.00000000000000000, -219.9999999999999716 ) ) ;
#14019 = DIRECTION ( 'NONE',  ( -0.000000000000000000, -0.000000000000000000, 1.000000000000000000 ) ) ;
#14020 = CARTESIAN_POINT ( 'NONE',  ( -10.81189881249999729, 1.324075727343319199E-15, -165.5937500020484094 ) ) ;
#14021 = CARTESIAN_POINT ( 'NONE',  ( -5.405949406250003975, -9.363379034771801557, -195.5312500020484094 ) ) ;
#14022 = CARTESIAN_POINT ( 'NONE',  ( -5.405949406249996869, 9.363379034771805109, -14.34375000204834905 ) ) ;
#14023 = CARTESIAN_POINT ( 'NONE',  ( -9.999999999999998224, 1.224646799147353059E-15, -138.1250000040967620 ) ) ;
#14024 = CARTESIAN_POINT ( 'NONE',  ( 10.81189881249999551, -6.242252689847874514, -145.4687500020484094 ) ) ;
#14025 = CARTESIAN_POINT ( 'NONE',  ( -5.405949406249996869, 9.363379034771805109, -134.3437500020484094 ) ) ;
#14026 = CARTESIAN_POINT ( 'NONE',  ( -10.81189881249999907, -6.242252689847864744, -102.6562500020483952 ) ) ;
#14027 = CARTESIAN_POINT ( 'NONE',  ( -10.81189881249999729, 6.242252689847871849, -120.7187500020483952 ) ) ;
#14028 = CARTESIAN_POINT ( 'NONE',  ( -10.00000000000000000, -5.773502691896251982, -196.5000000040967905 ) ) ;
#14029 = CARTESIAN_POINT ( 'NONE',  ( -10.81189881249999729, 6.242252689847871849, -120.9062500020483952 ) ) ;
#14030 = CARTESIAN_POINT ( 'NONE',  ( 10.81189881249999729, 0.000000000000000000, -11.84375000204834727 ) ) ;
#14031 = CARTESIAN_POINT ( 'NONE',  ( -10.81189881249999729, 6.242252689847871849, -128.2187500020483810 ) ) ;
#14032 = CARTESIAN_POINT ( 'NONE',  ( -2.121150477449813534E-15, -11.54700538379251284, -54.87499999999997158 ) ) ;
#14033 = CARTESIAN_POINT ( 'NONE',  ( 7.070501591499376803E-16, 11.54700538379251284, -5.000000004096767370 ) ) ;
#14034 = CARTESIAN_POINT ( 'NONE',  ( 9.999999999999996447, -5.773502691896262640, -155.1250000000000000 ) ) ;
#14035 = CARTESIAN_POINT ( 'NONE',  ( 9.999999999999996447, -5.773502691896262640, -20.12499999999997868 ) ) ;
#14036 = CARTESIAN_POINT ( 'NONE',  ( -10.81189881249999729, 6.242252689847871849, -83.21875000204836681 ) ) ;
#14037 = CARTESIAN_POINT ( 'NONE',  ( 10.81189881249999551, -6.242252689847874514, -62.96875000204838813 ) ) ;
#14038 = CARTESIAN_POINT ( 'NONE',  ( -9.999999999999998224, 1.224646799147353059E-15, -169.6250000040967905 ) ) ;
#14039 = CARTESIAN_POINT ( 'NONE',  ( 5.405949406249999534, 9.363379034771803333, -35.78125000204837391 ) ) ;
#14040 = CARTESIAN_POINT ( 'NONE',  ( -5.405949406250003975, -9.363379034771801557, -43.84375000204837391 ) ) ;
#14041 = CARTESIAN_POINT ( 'NONE',  ( 9.999999999999998224, 0.000000000000000000, -186.5000000000000000 ) ) ;
#14042 = CARTESIAN_POINT ( 'NONE',  ( 7.644554776091147741E-16, 12.48450537969573659, -156.9687500020484094 ) ) ;
#14043 = EDGE_CURVE ( 'NONE', #42118, #37834, #38052, .T. ) ;
#14044 = CARTESIAN_POINT ( 'NONE',  ( 4.999999999999992006, -8.660254037844389075, -131.2499999999999716 ) ) ;
#14045 = CARTESIAN_POINT ( 'NONE',  ( -5.405949406250003975, -9.363379034771801557, -131.0312500020484094 ) ) ;
#14046 = CARTESIAN_POINT ( 'NONE',  ( 10.53161979936726844, 2.338297538395752273, -180.0000000000000568 ) ) ;
#14047 = CARTESIAN_POINT ( 'NONE',  ( -9.999999999999998224, 1.224646799147353059E-15, -83.74999999999997158 ) ) ;
#14048 = CARTESIAN_POINT ( 'NONE',  ( -2.293366432827344421E-15, -12.48450537969573659, -19.90625000204837747 ) ) ;
#14049 = EDGE_CURVE ( 'NONE', #7881, #41377, #4549, .T. ) ;
#14050 = ORIENTED_EDGE ( 'NONE', *, *, #16994, .T. ) ;
#14051 = CARTESIAN_POINT ( 'NONE',  ( 10.81189881249999551, -6.242252689847874514, -111.1562500020483952 ) ) ;
#14052 = CARTESIAN_POINT ( 'NONE',  ( -9.999999999999998224, 5.773502691896259087, -123.2500000040967763 ) ) ;
#14053 = CARTESIAN_POINT ( 'NONE',  ( -9.999999999999227285, -5.773502691896698735, -112.1249999999999574 ) ) ;
#14054 = ADVANCED_FACE ( 'NONE', ( #25328 ), #38473, .F. ) ;
#14055 = CARTESIAN_POINT ( 'NONE',  ( -9.999999999999998224, 5.773502691896259087, -30.25000000409675849 ) ) ;
#14056 = CARTESIAN_POINT ( 'NONE',  ( -9.999999999998456346, -5.773502691897145489, -58.50000000409673362 ) ) ;
#14057 = PRODUCT_DEFINITION ( 'UNKNOWN', '', #26987, #29581 ) ;
#14058 = CARTESIAN_POINT ( 'NONE',  ( 10.81189881249999729, 0.000000000000000000, -55.53125000204836681 ) ) ;
#14059 = FACE_OUTER_BOUND ( 'NONE', #29173, .T. ) ;
#14060 = CARTESIAN_POINT ( 'NONE',  ( 10.81189881249999729, 0.000000000000000000, -151.5312500020484094 ) ) ;
#14061 = CARTESIAN_POINT ( 'NONE',  ( 10.81189881249999729, 0.000000000000000000, -134.8437500020484094 ) ) ;
#14062 = CARTESIAN_POINT ( 'NONE',  ( -9.999999999999998224, 1.224646799147353059E-15, -103.6250000040967763 ) ) ;
#14063 = ORIENTED_EDGE ( 'NONE', *, *, #24260, .F. ) ;
#14064 = CARTESIAN_POINT ( 'NONE',  ( 9.999999999999872102, 5.773502691896329253, -164.2500000040968189 ) ) ;
#14065 = ORIENTED_EDGE ( 'NONE', *, *, #6580, .T. ) ;
#14066 = EDGE_CURVE ( 'NONE', #22153, #15045, #42544, .T. ) ;
#14067 = ORIENTED_EDGE ( 'NONE', *, *, #18568, .F. ) ;
#14068 = DATE_AND_TIME ( #37782, #37266 ) ;
#14070 = EDGE_LOOP ( 'NONE', ( #18613, #15321, #9371, #33335, #11303, #26518, #40941, #34241 ) ) ;
#14069 = CARTESIAN_POINT ( 'NONE',  ( 10.81189881249999907, 6.242252689847868297, -109.2187500020483810 ) ) ;
#14071 = CARTESIAN_POINT ( 'NONE',  ( -9.999999999999998224, 1.224646799147353059E-15, -131.7499999999999716 ) ) ;
#14072 = CARTESIAN_POINT ( 'NONE',  ( -10.81189881249999907, -6.242252689847864744, -192.4687500020484094 ) ) ;
#14073 = CARTESIAN_POINT ( 'NONE',  ( 7.644554776091147741E-16, 12.48450537969573659, -35.46875000204835260 ) ) ;
#14074 = CARTESIAN_POINT ( 'NONE',  ( 9.999999999999998224, 0.000000000000000000, -153.8750000040967905 ) ) ;
#14075 = CYLINDRICAL_SURFACE ( 'NONE', #10052, 9.999999999999998224 ) ;
#14076 = CARTESIAN_POINT ( 'NONE',  ( 5.405949406249992428, -9.363379034771808662, -178.5937500020484094 ) ) ;
#14077 = CARTESIAN_POINT ( 'NONE',  ( 10.81189881249999729, 0.000000000000000000, -158.8437500020483810 ) ) ;
#14078 = CARTESIAN_POINT ( 'NONE',  ( -9.999999999999804601, 5.773502691896371886, -178.3750000000000284 ) ) ;
#14079 = CARTESIAN_POINT ( 'NONE',  ( -2.293366432827344421E-15, -12.48450537969573659, -139.7187500020483810 ) ) ;
#14080 = CARTESIAN_POINT ( 'NONE',  ( 10.81189881249999729, 6.242252689847867408, -154.2187500020483810 ) ) ;
#14081 = CARTESIAN_POINT ( 'NONE',  ( 9.999999999999998224, 0.000000000000000000, -126.8750000040967905 ) ) ;
#14082 = CARTESIAN_POINT ( 'NONE',  ( 7.070501591499376803E-16, 11.54700538379251284, -102.5000000040967905 ) ) ;
#14083 = CARTESIAN_POINT ( 'NONE',  ( 4.999999999999992006, -8.660254037844389075, -176.2500000000000284 ) ) ;
#14084 = CARTESIAN_POINT ( 'NONE',  ( 10.81189881249999729, 0.000000000000000000, -92.84375000204838102 ) ) ;
#14085 = CARTESIAN_POINT ( 'NONE',  ( -5.405949406249996869, 9.363379034771805109, -70.03125000204838102 ) ) ;
#14086 = CARTESIAN_POINT ( 'NONE',  ( -9.999999999999996447, 5.773502691896259975, -168.2500000040968189 ) ) ;
#14087 = CARTESIAN_POINT ( 'NONE',  ( 5.405949406249992428, -9.363379034771808662, -181.5937500020483810 ) ) ;
#14088 = CARTESIAN_POINT ( 'NONE',  ( -5.405949406249996869, 9.363379034771805109, -121.0312500020483952 ) ) ;
#14089 = CARTESIAN_POINT ( 'NONE',  ( 5.405949406249999534, 9.363379034771803333, -155.7812500020484094 ) ) ;
#14090 =( BOUNDED_CURVE ( )  B_SPLINE_CURVE ( 2, ( #5050, #21873, #31602, #11934, #18196, #31387, #14948 ),
 .UNSPECIFIED., .F., .F. ) 
 B_SPLINE_CURVE_WITH_KNOTS ( ( 3, 2, 2, 3 ),
 ( 0.1492537313432835966, 0.1504975124378109819, 0.1517412935323383116, 0.1529850746268656692 ),
 .UNSPECIFIED. ) 
 CURVE ( )  GEOMETRIC_REPRESENTATION_ITEM ( )  RATIONAL_B_SPLINE_CURVE ( ( 0.9999999999999970024, 0.8660254037844417052, 1.000000000000000000, 0.8660254037844387076, 1.000000000000000000, 0.8660254037844387076, 1.000000000000000000 ) ) 
 REPRESENTATION_ITEM ( '' )  );
#14091 = CARTESIAN_POINT ( 'NONE',  ( -5.405949406250003975, -9.363379034771801557, -56.03125000204836681 ) ) ;
#14092 = CARTESIAN_POINT ( 'NONE',  ( -5.000000000000003553, -8.660254037844383745, -131.8750000040967905 ) ) ;
#14093 = CARTESIAN_POINT ( 'NONE',  ( -2.121150477449813534E-15, -11.54700538379251284, -105.8749999999999858 ) ) ;
#14094 = EDGE_LOOP ( 'NONE', ( #2187, #21914, #19775, #30239 ) ) ;
#14095 = CARTESIAN_POINT ( 'NONE',  ( -5.405949406250003975, -9.363379034771801557, -132.5312500020484094 ) ) ;
#14096 = CARTESIAN_POINT ( 'NONE',  ( -2.121150477449813534E-15, -11.54700538379251284, -148.2500000040968189 ) ) ;
#14097 = CARTESIAN_POINT ( 'NONE',  ( 5.405949406249999534, 9.363379034771803333, -146.7812500020483810 ) ) ;
#14098 = CARTESIAN_POINT ( 'NONE',  ( 5.405949406249992428, -9.363379034771808662, -184.7812500020484094 ) ) ;
#14099 = EDGE_LOOP ( 'NONE', ( #32225, #19559, #20891, #25578 ) ) ;
#14100 = CARTESIAN_POINT ( 'NONE',  ( 9.999999999999996447, -5.773502691896262640, -47.12499999999996447 ) ) ;
#14101 = CARTESIAN_POINT ( 'NONE',  ( 5.405949406249999534, 9.363379034771803333, -176.5937500020484094 ) ) ;
#14102 = AXIS2_PLACEMENT_3D ( 'NONE', #25416, #9423, #12224 ) ;
#14103 = CARTESIAN_POINT ( 'NONE',  ( 7.070501591499377789E-16, 11.54700538379251284, -56.00000000409676915 ) ) ;
#14104 = CARTESIAN_POINT ( 'NONE',  ( -9.999999999999998224, 1.224646799147353059E-15, -109.6250000040967763 ) ) ;
#14105 = CARTESIAN_POINT ( 'NONE',  ( 10.00000000000025402, -5.773502691896113426, -158.1250000000000284 ) ) ;
#14106 = CARTESIAN_POINT ( 'NONE',  ( -5.405949406249996869, 9.363379034771805109, -74.53125000204838102 ) ) ;
#14107 = CARTESIAN_POINT ( 'NONE',  ( -10.81189881249999729, -6.242252689847864744, -63.65625000204837391 ) ) ;
#14108 = CARTESIAN_POINT ( 'NONE',  ( -9.999999999999998224, 1.224646799147353059E-15, -51.12500000409675494 ) ) ;
#14109 = CARTESIAN_POINT ( 'NONE',  ( 10.81189881249999551, -6.242252689847874514, -10.46875000204835793 ) ) ;
#14110 = CARTESIAN_POINT ( 'NONE',  ( -4.999999999999996447, 8.660254037844387298, -88.49999999999998579 ) ) ;
#14111 = CARTESIAN_POINT ( 'NONE',  ( 7.644554776091147741E-16, 12.48450537969573659, -179.6562500020484094 ) ) ;
#14112 = EDGE_CURVE ( 'NONE', #32436, #35302, #22931, .T. ) ;
#14113 = CARTESIAN_POINT ( 'NONE',  ( 5.405949406249999534, 9.363379034771803333, -7.281250002048378356 ) ) ;
#14114 = CARTESIAN_POINT ( 'NONE',  ( 0.000000000000000000, 0.000000000000000000, -99.99999999999998579 ) ) ;
#14115 = CARTESIAN_POINT ( 'NONE',  ( 7.070501591499376803E-16, 11.54700538379251284, -198.1250000000000284 ) ) ;
#14116 = CYLINDRICAL_SURFACE ( 'NONE', #133, 25.00000000000000000 ) ;
#14117 = CARTESIAN_POINT ( 'NONE',  ( -5.000000000000003553, -8.660254037844383745, -154.0000000000000000 ) ) ;
#14118 = CARTESIAN_POINT ( 'NONE',  ( 11.54700538379250396, 20.00000000000000711, 0.000000000000000000 ) ) ;
#14120 = EDGE_LOOP ( 'NONE', ( #41156, #36022, #3283, #29879 ) ) ;
#14119 = CARTESIAN_POINT ( 'NONE',  ( -5.405949406249996869, 9.363379034771805109, -85.03125000204838102 ) ) ;
#14121 =( NAMED_UNIT ( * ) PLANE_ANGLE_UNIT ( ) SI_UNIT ( $, .RADIAN. ) );
#14123 = ORIENTED_EDGE ( 'NONE', *, *, #11142, .F. ) ;
#14122 = CARTESIAN_POINT ( 'NONE',  ( 10.00000000000051159, -5.773502691895965988, -122.5000000040967763 ) ) ;
#14124 = ORIENTED_EDGE ( 'NONE', *, *, #29172, .F. ) ;
#14125 = CARTESIAN_POINT ( 'NONE',  ( 5.405949406249992428, -9.363379034771808662, -40.59375000204837391 ) ) ;
#14126 = CARTESIAN_POINT ( 'NONE',  ( 5.405949406249992428, -9.363379034771808662, -30.09375000204836326 ) ) ;
#14127 = VECTOR ( 'NONE', #33042, 1000.000000000000000 ) ;
#14128 = CARTESIAN_POINT ( 'NONE',  ( 7.644554776091147741E-16, 12.48450537969573659, -10.15625000204837924 ) ) ;
#14129 = CARTESIAN_POINT ( 'NONE',  ( 7.644554776091147741E-16, 12.48450537969573659, -66.96875000204838102 ) ) ;
#14130 = CARTESIAN_POINT ( 'NONE',  ( -10.00000000000012434, 5.773502691896184480, -163.7500000040967905 ) ) ;
#14131 = CARTESIAN_POINT ( 'NONE',  ( -5.000000000000003553, -8.660254037844383745, -44.49999999999998579 ) ) ;
#14132 = CARTESIAN_POINT ( 'NONE',  ( 7.644554776091147741E-16, 12.48450537969573659, -182.4687500020484094 ) ) ;
#14133 = CARTESIAN_POINT ( 'NONE',  ( -10.81189881249999729, 6.242252689847871849, -167.2187500020483810 ) ) ;
#14134 =( BOUNDED_CURVE ( )  B_SPLINE_CURVE ( 2, ( #33350, #7213, #32914, #16478, #3135, #42392, #39581 ),
 .UNSPECIFIED., .F., .F. ) 
 B_SPLINE_CURVE_WITH_KNOTS ( ( 3, 2, 2, 3 ),
 ( 0.3731343283582090331, 0.3743781094527363629, 0.3756218905472638037, 0.3768656716417911334 ),
 .UNSPECIFIED. ) 
 CURVE ( )  GEOMETRIC_REPRESENTATION_ITEM ( )  RATIONAL_B_SPLINE_CURVE ( ( 0.9999999999999940048, 0.8660254037844447028, 1.000000000000000000, 0.8660254037844387076, 1.000000000000000000, 0.8660254037844267172, 1.000000000000011990 ) ) 
 REPRESENTATION_ITEM ( '' )  );
#14135 = CARTESIAN_POINT ( 'NONE',  ( 5.405949406249992428, -9.363379034771808662, -1.593750002048366365 ) ) ;
#14136 = DIRECTION ( 'NONE',  ( -0.000000000000000000, -0.000000000000000000, 1.000000000000000000 ) ) ;
#14137 = CARTESIAN_POINT ( 'NONE',  ( 10.00000000000154010, -5.773502691895370020, -20.50000000409673007 ) ) ;
#14138 = FACE_OUTER_BOUND ( 'NONE', #9566, .T. ) ;
#14139 = CARTESIAN_POINT ( 'NONE',  ( -5.405949406249996869, 9.363379034771805109, -116.3437500020483810 ) ) ;
#14140 = DIRECTION ( 'NONE',  ( -0.000000000000000000, -0.000000000000000000, 1.000000000000000000 ) ) ;
#14141 = CARTESIAN_POINT ( 'NONE',  ( -5.405949406249996869, 9.363379034771805109, -88.03125000204838102 ) ) ;
#14142 = CARTESIAN_POINT ( 'NONE',  ( -10.81189881249999729, -6.242252689847864744, -99.46875000204838102 ) ) ;
#14143 = CARTESIAN_POINT ( 'NONE',  ( -5.405949406250003975, -9.363379034771801557, -69.34375000204836681 ) ) ;
#14144 = VECTOR ( 'NONE', #694, 1000.000000000000000 ) ;
#14145 = CARTESIAN_POINT ( 'NONE',  ( 10.81189881249999551, -6.242252689847874514, -79.65625000204838102 ) ) ;
#14146 = CARTESIAN_POINT ( 'NONE',  ( -9.999999999999998224, 5.773502691896259087, -157.7500000040967905 ) ) ;
#14147 = CARTESIAN_POINT ( 'NONE',  ( -4.999999999999996447, 8.660254037844387298, -135.0000000000000000 ) ) ;
#14148 = CIRCLE ( 'NONE', #6604, 9.999999999999998224 ) ;
#14149 = CARTESIAN_POINT ( 'NONE',  ( 10.81189881249999729, 6.242252689847867408, -155.9062500020483810 ) ) ;
#14150 = CARTESIAN_POINT ( 'NONE',  ( -2.293366432827344421E-15, -12.48450537969573659, -174.4062500020483810 ) ) ;
#14151 = CARTESIAN_POINT ( 'NONE',  ( -5.405949406249996869, 9.363379034771805109, -0.8437500020483656993 ) ) ;
#14152 = CARTESIAN_POINT ( 'NONE',  ( 9.999999999999998224, 0.000000000000000000, -108.8750000040967763 ) ) ;
#14153 = CARTESIAN_POINT ( 'NONE',  ( -2.293366432827344421E-15, -12.48450537969573659, -108.2187500020483668 ) ) ;
#14154 = CARTESIAN_POINT ( 'NONE',  ( -9.999999999999998224, 1.224646799147353059E-15, -184.6250000040967905 ) ) ;
#14155 = CARTESIAN_POINT ( 'NONE',  ( 5.000000000000000000, 8.660254037844385522, -73.74999999999998579 ) ) ;
#14156 = CARTESIAN_POINT ( 'NONE',  ( 10.81189881249999907, 6.242252689847868297, -4.406250002048361480 ) ) ;
#14157 = CARTESIAN_POINT ( 'NONE',  ( 7.070501591499377789E-16, 11.54700538379251284, -93.50000000409677625 ) ) ;
#14158 = AXIS2_PLACEMENT_3D ( 'NONE', #31807, #5035, #28979 ) ;
#14159 = CARTESIAN_POINT ( 'NONE',  ( -5.000000000000003553, -8.660254037844383745, -172.0000000000000000 ) ) ;
#14160 = CARTESIAN_POINT ( 'NONE',  ( 5.405949406249992428, -9.363379034771808662, -97.78125000204839523 ) ) ;
#14161 = CARTESIAN_POINT ( 'NONE',  ( -5.405949406250003975, -9.363379034771801557, -86.03125000204838102 ) ) ;
#14162 = CARTESIAN_POINT ( 'NONE',  ( 5.000000000000000000, 8.660254037844385522, -72.62500000409677625 ) ) ;
#14163 = CARTESIAN_POINT ( 'NONE',  ( 10.00000000000000000, 5.773502691896255534, -168.3750000000000000 ) ) ;
#14164 = CARTESIAN_POINT ( 'NONE',  ( 7.644554776091147741E-16, 12.48450537969573659, -30.96875000204835260 ) ) ;
#14165 = EDGE_LOOP ( 'NONE', ( #30572, #5279, #8659, #38093 ) ) ;
#14166 = CARTESIAN_POINT ( 'NONE',  ( -9.999999999999998224, 5.773502691896259087, -2.874999999999949374 ) ) ;
#14167 = CARTESIAN_POINT ( 'NONE',  ( -10.81189881249999907, -6.242252689847864744, -26.15625000204838102 ) ) ;
#14168 = CARTESIAN_POINT ( 'NONE',  ( -10.81189881249999729, -6.242252689847864744, -12.46875000204837391 ) ) ;
#14169 = DIRECTION ( 'NONE',  ( 1.000000000000000000, 0.000000000000000000, 0.000000000000000000 ) ) ;
#14170 = CARTESIAN_POINT ( 'NONE',  ( -9.999999999999998224, 1.224646799147353059E-15, -1.625000004096766038 ) ) ;
#14171 = CARTESIAN_POINT ( 'NONE',  ( -2.293366432827344421E-15, -12.48450537969573659, -127.9062500020483952 ) ) ;
#14172 = CARTESIAN_POINT ( 'NONE',  ( -5.000000000000003553, -8.660254037844383745, -181.0000000000000000 ) ) ;
#14173 = DIRECTION ( 'NONE',  ( -0.000000000000000000, -0.000000000000000000, -1.000000000000000000 ) ) ;
#14175 = ORIENTED_EDGE ( 'NONE', *, *, #15377, .F. ) ;
#14174 = CARTESIAN_POINT ( 'NONE',  ( 5.405949406249999534, 9.363379034771803333, -109.2812500020483810 ) ) ;
#14176 = CARTESIAN_POINT ( 'NONE',  ( 9.999999999999998224, 0.000000000000000000, -39.87500000409676915 ) ) ;
#14177 = ORIENTED_EDGE ( 'NONE', *, *, #21602, .T. ) ;
#14178 = AXIS2_PLACEMENT_3D ( 'NONE', #32601, #35413, #22447 ) ;
#14179 = ORIENTED_EDGE ( 'NONE', *, *, #5896, .T. ) ;
#14180 = EDGE_CURVE ( 'NONE', #40199, #19714, #6520, .T. ) ;
#14181 = CARTESIAN_POINT ( 'NONE',  ( -5.405949406250003975, -9.363379034771801557, -39.53125000204838102 ) ) ;
#14182 = MECHANICAL_CONTEXT ( 'NONE', #25362, 'mechanical' ) ;
#14183 = CARTESIAN_POINT ( 'NONE',  ( -2.293366432827344421E-15, -12.48450537969573659, -97.71875000204838102 ) ) ;
#14184 = CARTESIAN_POINT ( 'NONE',  ( 0.000000000000000000, 0.000000000000000000, -200.0000000000000000 ) ) ;
#14185 = CARTESIAN_POINT ( 'NONE',  ( 0.000000000000000000, 0.000000000000000000, -99.99999999999998579 ) ) ;
#14186 = CARTESIAN_POINT ( 'NONE',  ( -10.81189881249999729, 1.324075727343319199E-15, -195.5937500020484094 ) ) ;
#14187 = CARTESIAN_POINT ( 'NONE',  ( -10.81189881249999729, 1.324075727343319199E-15, -176.2812500020484094 ) ) ;
#14188 = CARTESIAN_POINT ( 'NONE',  ( 0.000000000000000000, 0.000000000000000000, -223.0000000000000000 ) ) ;
#14189 = CARTESIAN_POINT ( 'NONE',  ( 5.405949406249992428, -9.363379034771808662, -124.5937500020483952 ) ) ;
#14190 = CARTESIAN_POINT ( 'NONE',  ( 5.405949406249992428, -9.363379034771808662, -91.59375000204838102 ) ) ;
#14191 = CARTESIAN_POINT ( 'NONE',  ( 5.405949406249999534, 9.363379034771803333, -5.781250002048377468 ) ) ;
#14192 = CARTESIAN_POINT ( 'NONE',  ( 5.000000000000000000, 8.660254037844385522, -113.1250000040967763 ) ) ;
#14193 = CARTESIAN_POINT ( 'NONE',  ( -10.81189881249999907, -6.242252689847864744, -98.15625000204839523 ) ) ;
#14194 = CARTESIAN_POINT ( 'NONE',  ( -9.999999999999998224, 1.224646799147353059E-15, -186.1250000040967905 ) ) ;
#14195 = CARTESIAN_POINT ( 'NONE',  ( -10.81189881249999729, 6.242252689847871849, -107.2187500020483810 ) ) ;
#14196 = CARTESIAN_POINT ( 'NONE',  ( 5.405949406249992428, -9.363379034771808662, -181.7812500020483810 ) ) ;
#14197 = CARTESIAN_POINT ( 'NONE',  ( 4.999999999999992006, -8.660254037844389075, -107.2499999999999858 ) ) ;
#14198 = CARTESIAN_POINT ( 'NONE',  ( -9.999999999999612754, -5.773502691896474914, -153.0000000040967620 ) ) ;
#14199 = CARTESIAN_POINT ( 'NONE',  ( -4.999999999999996447, 8.660254037844387298, 2.775557561562891351E-14 ) ) ;
#14200 = CARTESIAN_POINT ( 'NONE',  ( -2.293366432827344421E-15, -12.48450537969573659, -54.21875000204838102 ) ) ;
#14201 = CARTESIAN_POINT ( 'NONE',  ( -5.405949406249996869, 9.363379034771805109, -42.84375000204837391 ) ) ;
#14202 = EDGE_CURVE ( 'NONE', #13652, #23080, #28709, .T. ) ;
#14203 = CARTESIAN_POINT ( 'NONE',  ( 5.000000000000000000, 8.660254037844385522, -174.6250000040968189 ) ) ;
#14204 = CARTESIAN_POINT ( 'NONE',  ( -10.81189881249999729, 6.242252689847871849, -8.406250002048372139 ) ) ;
#14205 = CARTESIAN_POINT ( 'NONE',  ( -5.405949406249996869, 9.363379034771805109, -18.84375000204835260 ) ) ;
#14206 = CARTESIAN_POINT ( 'NONE',  ( -2.121150477449813534E-15, -11.54700538379251284, -124.2500000040967763 ) ) ;
#14207 = CARTESIAN_POINT ( 'NONE',  ( -10.81189881249999729, 6.242252689847871849, -131.2187500020483810 ) ) ;
#14208 = CARTESIAN_POINT ( 'NONE',  ( -5.000000000000003553, -8.660254037844383745, -95.49999999999998579 ) ) ;
#14209 = CARTESIAN_POINT ( 'NONE',  ( -2.293366432827344421E-15, -12.48450537969573659, -31.90625000204835970 ) ) ;
#14210 = CARTESIAN_POINT ( 'NONE',  ( -10.00000000000000000, -5.773502691896251982, -117.0000000040967905 ) ) ;
#14211 = CARTESIAN_POINT ( 'NONE',  ( 7.070501591499376803E-16, 11.54700538379251284, -158.0000000040968189 ) ) ;
#14212 = CARTESIAN_POINT ( 'NONE',  ( 7.070501591499377789E-16, 11.54700538379251284, -63.12499999999998579 ) ) ;
#14213 = CARTESIAN_POINT ( 'NONE',  ( -2.293366432827344421E-15, -12.48450537969573659, -126.4062500020483952 ) ) ;
#14214 = CARTESIAN_POINT ( 'NONE',  ( 5.405949406249992428, -9.363379034771808662, -106.7812500020483810 ) ) ;
#14215 = EDGE_LOOP ( 'NONE', ( #9487, #24639, #22003, #11533 ) ) ;
#14216 = CARTESIAN_POINT ( 'NONE',  ( 5.000000000000000000, 8.660254037844385522, -8.125000004096744277 ) ) ;
#14217 = CARTESIAN_POINT ( 'NONE',  ( -2.121150477449813534E-15, -11.54700538379251284, -98.75000000409677625 ) ) ;
#14218 = DIRECTION ( 'NONE',  ( -0.000000000000000000, -0.000000000000000000, -1.000000000000000000 ) ) ;
#14219 = CARTESIAN_POINT ( 'NONE',  ( 5.405949406249992428, -9.363379034771808662, -166.7812500020484094 ) ) ;
#14220 = CARTESIAN_POINT ( 'NONE',  ( 10.81189881249999729, 0.000000000000000000, -58.34375000204835970 ) ) ;
#14221 = ORIENTED_EDGE ( 'NONE', *, *, #13665, .F. ) ;
#14222 = CARTESIAN_POINT ( 'NONE',  ( 5.000000000000000000, 8.660254037844385522, -22.74999999999996447 ) ) ;
#14223 = CARTESIAN_POINT ( 'NONE',  ( -2.293366432827344421E-15, -12.48450537969573659, -37.90625000204837391 ) ) ;
#14224 = CARTESIAN_POINT ( 'NONE',  ( -10.00000000000000000, -5.773502691896251982, -164.6249999999999716 ) ) ;
#14225 = CARTESIAN_POINT ( 'NONE',  ( 9.999999999999998224, 0.000000000000000000, -200.0000000000000000 ) ) ;
#14226 = CARTESIAN_POINT ( 'NONE',  ( -9.999999999999998224, 5.773502691896259087, -31.75000000409675138 ) ) ;
#14227 = CARTESIAN_POINT ( 'NONE',  ( 5.405949406249992428, -9.363379034771808662, -132.2812500020483810 ) ) ;
#14228 = CARTESIAN_POINT ( 'NONE',  ( 7.070501591499376803E-16, 11.54700538379251284, -75.50000000409677625 ) ) ;
#14229 = CARTESIAN_POINT ( 'NONE',  ( 9.999999999999998224, 0.000000000000000000, -51.87500000409675494 ) ) ;
#14230 = ORIENTED_EDGE ( 'NONE', *, *, #15090, .F. ) ;
#14231 = ADVANCED_FACE ( 'NONE', ( #3713 ), #487, .T. ) ;
#14233 = ORIENTED_EDGE ( 'NONE', *, *, #41980, .T. ) ;
#14232 = VERTEX_POINT ( 'NONE', #19883 ) ;
#14234 = FACE_OUTER_BOUND ( 'NONE', #15082, .T. ) ;
#14235 = CARTESIAN_POINT ( 'NONE',  ( 5.000000000000000000, 8.660254037844385522, -174.6250000040968189 ) ) ;
#14236 = CARTESIAN_POINT ( 'NONE',  ( 5.405949406249999534, 9.363379034771803333, -163.0937500020484094 ) ) ;
#14237 = CARTESIAN_POINT ( 'NONE',  ( 10.81189881249999729, 0.000000000000000000, -199.5312500020484094 ) ) ;
#14238 = CARTESIAN_POINT ( 'NONE',  ( -5.405949406249996869, 9.363379034771805109, -15.84375000204835082 ) ) ;
#14239 = DIRECTION ( 'NONE',  ( -0.000000000000000000, -0.000000000000000000, 1.000000000000000000 ) ) ;
#14240 = CARTESIAN_POINT ( 'NONE',  ( -10.81189881249999729, -6.242252689847864744, -148.9687500020484094 ) ) ;
#14241 = CARTESIAN_POINT ( 'NONE',  ( -2.293366432827344421E-15, -12.48450537969573659, -139.7187500020483810 ) ) ;
#14242 = CARTESIAN_POINT ( 'NONE',  ( -2.293366432827344421E-15, -12.48450537969573659, -106.9062500020483952 ) ) ;
#14243 = CARTESIAN_POINT ( 'NONE',  ( 5.405949406249999534, 9.363379034771803333, -121.0937500020483952 ) ) ;
#14244 = CARTESIAN_POINT ( 'NONE',  ( -2.121150477449813534E-15, -11.54700538379251284, -197.7500000040967905 ) ) ;
#14245 = CARTESIAN_POINT ( 'NONE',  ( -5.405949406249996869, 9.363379034771805109, -124.0312500020483952 ) ) ;
#14246 = CARTESIAN_POINT ( 'NONE',  ( 5.405949406249999534, 9.363379034771803333, -7.093750002048371250 ) ) ;
#14247 = CARTESIAN_POINT ( 'NONE',  ( -10.81189881249999729, -6.242252689847864744, -126.4687500020483810 ) ) ;
#14248 = CARTESIAN_POINT ( 'NONE',  ( -10.81189881249999729, 1.324075727343319199E-15, -198.7812500020484094 ) ) ;
#14249 = CARTESIAN_POINT ( 'NONE',  ( -2.121150477449813534E-15, -11.54700538379251284, -196.2500000040967905 ) ) ;
#14250 = CARTESIAN_POINT ( 'NONE',  ( -9.999999999999998224, 5.773502691896259087, -157.3749999999999716 ) ) ;
#14251 = CARTESIAN_POINT ( 'NONE',  ( -10.00000000000000000, -5.773502691896251982, -17.62499999999997158 ) ) ;
#14252 = CARTESIAN_POINT ( 'NONE',  ( 10.81189881249999551, -6.242252689847874514, -76.46875000204838102 ) ) ;
#14253 = CARTESIAN_POINT ( 'NONE',  ( 5.405949406249992428, -9.363379034771808662, -61.59375000204836681 ) ) ;
#14254 = CARTESIAN_POINT ( 'NONE',  ( -9.999999999999998224, 1.224646799147353059E-15, -19.62500000409675494 ) ) ;
#14255 = CARTESIAN_POINT ( 'NONE',  ( -5.405949406250003975, -9.363379034771801557, -36.53125000204837391 ) ) ;
#14256 = CARTESIAN_POINT ( 'NONE',  ( -10.81189881249999907, -6.242252689847864744, -48.46875000204837391 ) ) ;
#14257 = FACE_OUTER_BOUND ( 'NONE', #8491, .T. ) ;
#14258 = CARTESIAN_POINT ( 'NONE',  ( 10.81189881249999551, -6.242252689847874514, -157.4687500020484094 ) ) ;
#14259 = CARTESIAN_POINT ( 'NONE',  ( 5.000000000000000000, 8.660254037844385522, -120.2500000000000000 ) ) ;
#14260 = CARTESIAN_POINT ( 'NONE',  ( -5.405949406249996869, 9.363379034771805109, -131.5312500020484094 ) ) ;
#14261 = CARTESIAN_POINT ( 'NONE',  ( 9.169708609005772004, 5.423292144399351145, -179.9999999999999716 ) ) ;
#14262 = CARTESIAN_POINT ( 'NONE',  ( -2.121150477449813534E-15, -11.54700538379251284, -84.87500000000000000 ) ) ;
#14263 = CARTESIAN_POINT ( 'NONE',  ( 10.81189881249999551, -6.242252689847874514, -15.15625000204837214 ) ) ;
#14264 =( BOUNDED_CURVE ( )  B_SPLINE_CURVE ( 2, ( #7732, #17848, #31471, #38148, #37285, #1476, #14611 ),
 .UNSPECIFIED., .F., .F. ) 
 B_SPLINE_CURVE_WITH_KNOTS ( ( 3, 2, 2, 3 ),
 ( 0.2835820895522389029, 0.2848258706467662882, 0.2860696517412936180, 0.2873134328358210032 ),
 .UNSPECIFIED. ) 
 CURVE ( )  GEOMETRIC_REPRESENTATION_ITEM ( )  RATIONAL_B_SPLINE_CURVE ( ( 0.9999999999999880096, 0.8660254037844506980, 1.000000000000000000, 0.8660254037844387076, 1.000000000000000000, 0.8660254037844267172, 1.000000000000011990 ) ) 
 REPRESENTATION_ITEM ( '' )  );
#14265 = ORIENTED_EDGE ( 'NONE', *, *, #4286, .F. ) ;
#14266 = CARTESIAN_POINT ( 'NONE',  ( -5.405949406249996869, 9.363379034771805109, -104.5312500020483810 ) ) ;
#14267 = CARTESIAN_POINT ( 'NONE',  ( 5.000000000000000000, 8.660254037844385522, -123.6250000040967905 ) ) ;
#14268 = CARTESIAN_POINT ( 'NONE',  ( -5.000000000000003553, -8.660254037844383745, -56.87500000409676204 ) ) ;
#14269 = CARTESIAN_POINT ( 'NONE',  ( -9.999999999999998224, 5.773502691896259087, -34.75000000409674783 ) ) ;
#14270 = FACE_OUTER_BOUND ( 'NONE', #26058, .T. ) ;
#14271 = CARTESIAN_POINT ( 'NONE',  ( 10.81189881249999907, 6.242252689847868297, -55.40625000204837391 ) ) ;
#14272 = LINE ( 'NONE', #24248, #37957 ) ;
#14273 = CARTESIAN_POINT ( 'NONE',  ( 5.405949406249992428, -9.363379034771808662, -151.7812500020484094 ) ) ;
#14274 = CARTESIAN_POINT ( 'NONE',  ( 10.81189881249999729, 0.000000000000000000, -125.8437500020483952 ) ) ;
#14275 = CARTESIAN_POINT ( 'NONE',  ( 9.999999999999998224, 0.000000000000000000, -143.0000000000000000 ) ) ;
#14276 = ORIENTED_EDGE ( 'NONE', *, *, #9830, .T. ) ;
#14277 = CARTESIAN_POINT ( 'NONE',  ( 5.000000000000000000, 8.660254037844385522, -31.74999999999997158 ) ) ;
#14278 = EDGE_LOOP ( 'NONE', ( #35544, #34332, #10216, #37555 ) ) ;
#14279 = ORIENTED_EDGE ( 'NONE', *, *, #35208, .T. ) ;
#14280 = VECTOR ( 'NONE', #36831, 1000.000000000000000 ) ;
#14281 = EDGE_CURVE ( 'NONE', #6102, #16786, #11017, .T. ) ;
#14283 = ORIENTED_EDGE ( 'NONE', *, *, #18832, .F. ) ;
#14282 = CARTESIAN_POINT ( 'NONE',  ( -10.81189881249999729, 1.324075727343319199E-15, -114.5937500020483810 ) ) ;
#14284 = AXIS2_PLACEMENT_3D ( 'NONE', #7698, #14136, #15003 ) ;
#14285 = EDGE_CURVE ( 'NONE', #18018, #23066, #23566, .T. ) ;
#14286 = EDGE_CURVE ( 'NONE', #25687, #14871, #3922, .T. ) ;
#14287 = CARTESIAN_POINT ( 'NONE',  ( 5.405949406249999534, 9.363379034771803333, -187.0937500020483810 ) ) ;
#14288 = CARTESIAN_POINT ( 'NONE',  ( -2.293366432827344421E-15, -12.48450537969573659, -42.21875000204835970 ) ) ;
#14289 = CARTESIAN_POINT ( 'NONE',  ( 4.999999999999992006, -8.660254037844389075, -155.6250000040967905 ) ) ;
#14290 = CARTESIAN_POINT ( 'NONE',  ( 4.999999999999992006, -8.660254037844389075, -31.12500000409676559 ) ) ;
#14291 = CARTESIAN_POINT ( 'NONE',  ( -5.405949406249996869, 9.363379034771805109, -168.8437500020484094 ) ) ;
#14292 = CARTESIAN_POINT ( 'NONE',  ( 10.81189881249999729, 0.000000000000000000, -157.3437500020483810 ) ) ;
#14293 = CC_DESIGN_PERSON_AND_ORGANIZATION_ASSIGNMENT ( #5787, #28467, ( #37345 ) ) ;
#14294 = CARTESIAN_POINT ( 'NONE',  ( -5.000000000000003553, -8.660254037844383745, -76.37500000409677625 ) ) ;
#14295 = CARTESIAN_POINT ( 'NONE',  ( -10.81189881249999907, -6.242252689847864744, -141.4687500020484094 ) ) ;
#14296 = CARTESIAN_POINT ( 'NONE',  ( -10.81189881249999729, 1.324075727343319199E-15, -155.0937500020483810 ) ) ;
#14297 = CARTESIAN_POINT ( 'NONE',  ( 9.999999999999998224, 0.000000000000000000, -53.37500000409675494 ) ) ;
#14298 = CARTESIAN_POINT ( 'NONE',  ( 7.070501591499377789E-16, 11.54700538379251284, -181.6250000000000000 ) ) ;
#14299 = CARTESIAN_POINT ( 'NONE',  ( -2.293366432827344421E-15, -12.48450537969573659, -87.21875000204838102 ) ) ;
#14300 = CARTESIAN_POINT ( 'NONE',  ( -9.999999999999998224, 1.224646799147353059E-15, -148.6250000040967905 ) ) ;
#14301 = CARTESIAN_POINT ( 'NONE',  ( 10.81189881249999551, -6.242252689847874514, -57.15625000204837391 ) ) ;
#14302 = CARTESIAN_POINT ( 'NONE',  ( -8.659811548901195977, -5.000849327365069819, 0.000000000000000000 ) ) ;
#14303 = CARTESIAN_POINT ( 'NONE',  ( 7.644554776091147741E-16, 12.48450537969573659, -180.9687500020484094 ) ) ;
#14304 = EDGE_CURVE ( 'NONE', #18939, #24456, #15180, .T. ) ;
#14305 = CARTESIAN_POINT ( 'NONE',  ( 5.405949406249992428, -9.363379034771808662, -114.2812500020483952 ) ) ;
#14306 = CARTESIAN_POINT ( 'NONE',  ( 10.81189881249999551, -6.242252689847874514, -151.6562500020484094 ) ) ;
#14307 = CARTESIAN_POINT ( 'NONE',  ( 9.999999999999998224, 0.000000000000000000, -137.0000000000000000 ) ) ;
#14308 = CARTESIAN_POINT ( 'NONE',  ( 5.405949406249992428, -9.363379034771808662, -48.28125000204838813 ) ) ;
#14309 = CARTESIAN_POINT ( 'NONE',  ( 9.999999999999996447, -5.773502691896262640, -133.0000000040967905 ) ) ;
#14310 = CARTESIAN_POINT ( 'NONE',  ( 10.00000000000000000, 5.773502691896255534, -108.3749999999999858 ) ) ;
#14311 = ORIENTED_EDGE ( 'NONE', *, *, #31628, .F. ) ;
#14312 = CARTESIAN_POINT ( 'NONE',  ( 5.405949406249999534, 9.363379034771803333, -122.7812500020483952 ) ) ;
#14313 = CARTESIAN_POINT ( 'NONE',  ( -10.00000000000000000, -5.773502691896251982, -148.5000000040967905 ) ) ;
#14314 = CARTESIAN_POINT ( 'NONE',  ( 5.405949406249992428, -9.363379034771808662, -145.7812500020483810 ) ) ;
#14315 = EDGE_CURVE ( 'NONE', #31960, #29666, #3075, .T. ) ;
#14316 = CARTESIAN_POINT ( 'NONE',  ( -2.293366432827344421E-15, -12.48450537969573659, -187.9062500020484094 ) ) ;
#14317 = AXIS2_PLACEMENT_3D ( 'NONE', #23038, #26488, #23681 ) ;
#14318 = EDGE_LOOP ( 'NONE', ( #586, #2021, #1592, #2555 ) ) ;
#14319 = CARTESIAN_POINT ( 'NONE',  ( -5.000000000000003553, -8.660254037844383745, -45.99999999999998579 ) ) ;
#14320 = CARTESIAN_POINT ( 'NONE',  ( 10.81189881249999729, 0.000000000000000000, -178.3437500020483810 ) ) ;
#14321 = CARTESIAN_POINT ( 'NONE',  ( -4.999999999999996447, 8.660254037844387298, -61.87500000409676204 ) ) ;
#14322 = EDGE_CURVE ( 'NONE', #27758, #41802, #26584, .T. ) ;
#14323 = AXIS2_PLACEMENT_3D ( 'NONE', #32452, #9968, #26176 ) ;
#14324 = CARTESIAN_POINT ( 'NONE',  ( 5.000000000000000000, 8.660254037844385522, -21.62500000409675494 ) ) ;
#14325 = CARTESIAN_POINT ( 'NONE',  ( 0.000000000000000000, 0.000000000000000000, -200.0000000000000000 ) ) ;
#14326 = CARTESIAN_POINT ( 'NONE',  ( 10.81189881249999729, 0.000000000000000000, -73.53125000204838102 ) ) ;
#14327 = CARTESIAN_POINT ( 'NONE',  ( -2.293366432827344421E-15, -12.48450537969573659, -54.40625000204838102 ) ) ;
#14328 = CARTESIAN_POINT ( 'NONE',  ( 5.000000000000000000, 8.660254037844385522, -53.12500000409675494 ) ) ;
#14329 = CARTESIAN_POINT ( 'NONE',  ( 10.81189881249999729, 0.000000000000000000, -13.34375000204834905 ) ) ;
#14330 = CARTESIAN_POINT ( 'NONE',  ( 9.999999999999998224, 0.000000000000000000, -200.0000000000000000 ) ) ;
#14331 = CARTESIAN_POINT ( 'NONE',  ( -10.81189881249999729, 6.242252689847871849, -173.4062500020483810 ) ) ;
#14332 = CARTESIAN_POINT ( 'NONE',  ( 5.405949406249992428, -9.363379034771808662, -6.281250002048377468 ) ) ;
#14333 = DIRECTION ( 'NONE',  ( 0.000000000000000000, 0.000000000000000000, 1.000000000000000000 ) ) ;
#14334 = FACE_OUTER_BOUND ( 'NONE', #28722, .T. ) ;
#14335 = ADVANCED_FACE ( 'NONE', ( #39734 ), #6943, .T. ) ;
#14336 = CARTESIAN_POINT ( 'NONE',  ( -9.999999999999998224, 0.000000000000000000, -99.99999999999998579 ) ) ;
#14337 = CARTESIAN_POINT ( 'NONE',  ( 5.000000000000000000, 8.660254037844385522, -177.2500000000000284 ) ) ;
#14338 = CARTESIAN_POINT ( 'NONE',  ( 0.000000000000000000, 0.000000000000000000, -200.0000000000000000 ) ) ;
#14340 = ORIENTED_EDGE ( 'NONE', *, *, #27221, .T. ) ;
#14339 = CARTESIAN_POINT ( 'NONE',  ( 5.405949406249999534, 9.363379034771803333, -82.28125000204838102 ) ) ;
#14341 = SHAPE_REPRESENTATION_RELATIONSHIP ( 'NONE' , 'NONE' ,  #6779, #27907 ) ;
#14343 = VERTEX_POINT ( 'NONE', #23354 ) ;
#14342 = CARTESIAN_POINT ( 'NONE',  ( 9.999999999999998224, 0.000000000000000000, -173.3750000040968189 ) ) ;
#14344 = VERTEX_POINT ( 'NONE', #13601 ) ;
#14345 = CARTESIAN_POINT ( 'NONE',  ( -5.405949406250003975, -9.363379034771801557, -34.84375000204836681 ) ) ;
#14346 = CARTESIAN_POINT ( 'NONE',  ( -2.293366432827344421E-15, -12.48450537969573659, -27.21875000204838102 ) ) ;
#14347 = CARTESIAN_POINT ( 'NONE',  ( -10.81189881249999729, 6.242252689847871849, -14.40625000204836859 ) ) ;
#14348 = CARTESIAN_POINT ( 'NONE',  ( -2.293366432827344421E-15, -12.48450537969573659, -61.71875000204838102 ) ) ;
#14349 = CARTESIAN_POINT ( 'NONE',  ( 9.999999999998969713, 5.773502691896851502, -28.87499999999995381 ) ) ;
#14350 = CARTESIAN_POINT ( 'NONE',  ( 9.999999999999998224, 0.000000000000000000, -43.99999999999998579 ) ) ;
#14351 = VECTOR ( 'NONE', #23846, 1000.000000000000000 ) ;
#14352 = CARTESIAN_POINT ( 'NONE',  ( -10.81189881249999729, 6.242252689847871849, -182.2187500020484379 ) ) ;
#14353 =( BOUNDED_CURVE ( )  B_SPLINE_CURVE ( 2, ( #28894, #25651, #2141, #21552, #34733, #15054, #35369 ),
 .UNSPECIFIED., .F., .F. ) 
 B_SPLINE_CURVE_WITH_KNOTS ( ( 3, 2, 2, 3 ),
 ( 0.6082089552238807428, 0.6094527363184080171, 0.6106965174129354024, 0.6119402985074627876 ),
 .UNSPECIFIED. ) 
 CURVE ( )  GEOMETRIC_REPRESENTATION_ITEM ( )  RATIONAL_B_SPLINE_CURVE ( ( 0.9999999999999880096, 0.8660254037844506980, 1.000000000000000000, 0.8660254037844387076, 1.000000000000000000, 0.8660254037844267172, 1.000000000000011990 ) ) 
 REPRESENTATION_ITEM ( '' )  );
#14354 = CARTESIAN_POINT ( 'NONE',  ( -10.81189881249999729, 1.324075727343319199E-15, -162.5937500020484094 ) ) ;
#14355 = CARTESIAN_POINT ( 'NONE',  ( 5.405949406249999534, 9.363379034771803333, -179.5937500020484094 ) ) ;
#14356 = CARTESIAN_POINT ( 'NONE',  ( 9.999999999999998224, 0.000000000000000000, -104.3750000040967763 ) ) ;
#14357 = DIRECTION ( 'NONE',  ( 0.000000000000000000, 0.000000000000000000, -1.000000000000000000 ) ) ;
#14358 = CYLINDRICAL_SURFACE ( 'NONE', #1922, 9.999999999999998224 ) ;
#14359 = CARTESIAN_POINT ( 'NONE',  ( -5.405949406250003975, -9.363379034771801557, -115.8437500020483810 ) ) ;
#14360 = LINE ( 'NONE', #41339, #18364 ) ;
#14361 = CARTESIAN_POINT ( 'NONE',  ( 7.644554776091147741E-16, 12.48450537969573659, -79.15625000204838102 ) ) ;
#14362 = CARTESIAN_POINT ( 'NONE',  ( -2.293366432827344421E-15, -12.48450537969573659, -100.7187500020483952 ) ) ;
#14363 = CARTESIAN_POINT ( 'NONE',  ( 7.644554776091147741E-16, 12.48450537969573659, -66.96875000204838102 ) ) ;
#14364 = CARTESIAN_POINT ( 'NONE',  ( 10.81189881249999907, 6.242252689847868297, -76.40625000204839523 ) ) ;
#14365 = CARTESIAN_POINT ( 'NONE',  ( 7.070501591499377789E-16, 11.54700538379251284, -153.5000000040967905 ) ) ;
#14366 = CARTESIAN_POINT ( 'NONE',  ( -9.999999999999998224, 1.224646799147353059E-15, -128.7499999999999716 ) ) ;
#14367 = ADVANCED_FACE ( 'NONE', ( #39945 ), #695, .T. ) ;
#14368 = CARTESIAN_POINT ( 'NONE',  ( -10.81189881249999729, 6.242252689847871849, -159.9062500020483810 ) ) ;
#14369 = CARTESIAN_POINT ( 'NONE',  ( -10.81189881249999729, 1.324075727343319199E-15, -170.2812500020484094 ) ) ;
#14370 = DIRECTION ( 'NONE',  ( -1.000000000000000000, 0.000000000000000000, 0.000000000000000000 ) ) ;
#14371 = CARTESIAN_POINT ( 'NONE',  ( 7.070501591499376803E-16, 11.54700538379251284, -159.5000000040968189 ) ) ;
#14372 = CARTESIAN_POINT ( 'NONE',  ( -10.81189881249999907, -6.242252689847864744, -106.9687500020483668 ) ) ;
#14373 = CARTESIAN_POINT ( 'NONE',  ( -9.999999999999998224, 0.000000000000000000, -99.99999999999998579 ) ) ;
#14374 = CARTESIAN_POINT ( 'NONE',  ( 10.00000000000000000, 5.773502691896255534, -76.87499999999997158 ) ) ;
#14375 = CARTESIAN_POINT ( 'NONE',  ( 10.81189881249999729, 0.000000000000000000, -3.031250002048374803 ) ) ;
#14376 = CARTESIAN_POINT ( 'NONE',  ( -10.00000000000000000, -5.773502691896251982, -81.00000000409677625 ) ) ;
#14377 = DIRECTION ( 'NONE',  ( 1.000000000000000000, 0.000000000000000000, 0.000000000000000000 ) ) ;
#14378 = CARTESIAN_POINT ( 'NONE',  ( 7.644554776091147741E-16, 12.48450537969573659, -103.1562500020483952 ) ) ;
#14379 = CARTESIAN_POINT ( 'NONE',  ( -5.405949406250003975, -9.363379034771801557, -72.53125000204838102 ) ) ;
#14380 = CARTESIAN_POINT ( 'NONE',  ( -2.121150477449813534E-15, -11.54700538379251284, -79.25000000409677625 ) ) ;
#14381 = CARTESIAN_POINT ( 'NONE',  ( 9.999999999999998224, 0.000000000000000000, -198.8750000040967905 ) ) ;
#14382 = CARTESIAN_POINT ( 'NONE',  ( -2.293366432827344421E-15, -12.48450537969573659, -30.21875000204835260 ) ) ;
#14383 = ORIENTED_EDGE ( 'NONE', *, *, #37564, .F. ) ;
#14384 = CARTESIAN_POINT ( 'NONE',  ( -5.000000000000003553, -8.660254037844383745, -3.999999999999976019 ) ) ;
#14385 = CARTESIAN_POINT ( 'NONE',  ( 7.644554776091147741E-16, 12.48450537969573659, -26.65625000204838102 ) ) ;
#14386 = CARTESIAN_POINT ( 'NONE',  ( 7.644554776091147741E-16, 12.48450537969573659, -11.46875000204836859 ) ) ;
#14387 = CARTESIAN_POINT ( 'NONE',  ( -9.999999999998969713, -5.773502691896847949, -64.50000000409674783 ) ) ;
#14388 = CARTESIAN_POINT ( 'NONE',  ( 10.00000000000000000, 5.773502691896255534, -0.7500000040967513826 ) ) ;
#14389 = CARTESIAN_POINT ( 'NONE',  ( -10.81189881249999729, 1.324075727343319199E-15, -129.7812500020483810 ) ) ;
#14390 = CARTESIAN_POINT ( 'NONE',  ( -5.000000000000003553, -8.660254037844383745, -185.5000000000000000 ) ) ;
#14391 = CARTESIAN_POINT ( 'NONE',  ( -9.999999999999868550, 5.773502691896333694, -175.7500000040967905 ) ) ;
#14392 = AXIS2_PLACEMENT_3D ( 'NONE', #8573, #4471, #37704 ) ;
#14394 = ORIENTED_EDGE ( 'NONE', *, *, #4298, .T. ) ;
#14393 = CARTESIAN_POINT ( 'NONE',  ( -2.293366432827344421E-15, -12.48450537969573659, -112.9062500020483952 ) ) ;
#14395 = CARTESIAN_POINT ( 'NONE',  ( -9.999999999999998224, 1.224646799147353059E-15, -200.0000000000000000 ) ) ;
#14396 = ORIENTED_EDGE ( 'NONE', *, *, #1965, .T. ) ;
#14397 = VERTEX_POINT ( 'NONE', #27211 ) ;
#14398 =( BOUNDED_CURVE ( )  B_SPLINE_CURVE ( 2, ( #17175, #10702, #32753, #40060, #16963, #29731, #13507 ),
 .UNSPECIFIED., .F., .F. ) 
 B_SPLINE_CURVE_WITH_KNOTS ( ( 3, 2, 2, 3 ),
 ( 0.3843283582089552786, 0.3855721393034826638, 0.3868159203980099936, 0.3880597014925373789 ),
 .UNSPECIFIED. ) 
 CURVE ( )  GEOMETRIC_REPRESENTATION_ITEM ( )  RATIONAL_B_SPLINE_CURVE ( ( 0.9999999999999940048, 0.8660254037844447028, 1.000000000000000000, 0.8660254037844387076, 1.000000000000000000, 0.8660254037844327124, 1.000000000000005995 ) ) 
 REPRESENTATION_ITEM ( '' )  );
#14399 = VECTOR ( 'NONE', #9668, 1000.000000000000000 ) ;
#14400 = CARTESIAN_POINT ( 'NONE',  ( -2.293366432827344421E-15, -12.48450537969573659, -36.40625000204835970 ) ) ;
#14401 = APPLICATION_PROTOCOL_DEFINITION ( 'international standard', 'config_control_design', 1994, #34764 ) ;
#14402 = CARTESIAN_POINT ( 'NONE',  ( -5.405949406249996869, 9.363379034771805109, -86.34375000204836681 ) ) ;
#14403 = DIRECTION ( 'NONE',  ( -1.000000000000000000, 0.000000000000000000, -0.000000000000000000 ) ) ;
#14404 = CARTESIAN_POINT ( 'NONE',  ( 9.999999999999998224, 0.000000000000000000, -174.5000000000000284 ) ) ;
#14405 =( BOUNDED_CURVE ( )  B_SPLINE_CURVE ( 2, ( #37357, #34562, #11014, #4554, #41215, #11873, #31329 ),
 .UNSPECIFIED., .F., .F. ) 
 B_SPLINE_CURVE_WITH_KNOTS ( ( 3, 2, 2, 3 ),
 ( 0.08208955223880604057, 0.08333333333333339810, 0.08457711442786078337, 0.08582089552238814090 ),
 .UNSPECIFIED. ) 
 CURVE ( )  GEOMETRIC_REPRESENTATION_ITEM ( )  RATIONAL_B_SPLINE_CURVE ( ( 0.9999999999999924505, 0.8660254037844461461, 1.000000000000000000, 0.8660254037844387076, 1.000000000000000000, 0.8660254037844297148, 1.000000000000008882 ) ) 
 REPRESENTATION_ITEM ( '' )  );
#14406 = CARTESIAN_POINT ( 'NONE',  ( 9.999999999999998224, 0.000000000000000000, -200.0000000000000000 ) ) ;
#14407 = CARTESIAN_POINT ( 'NONE',  ( 10.81189881249999551, -6.242252689847874514, -171.1562500020484094 ) ) ;
#14408 = CARTESIAN_POINT ( 'NONE',  ( -10.00000000000102496, 5.773502691895664007, -58.37499999999997158 ) ) ;
#14409 = EDGE_CURVE ( 'NONE', #18779, #17639, #34246, .T. ) ;
#14410 = CARTESIAN_POINT ( 'NONE',  ( -2.293366432827344421E-15, -12.48450537969573659, -121.7187500020483952 ) ) ;
#14411 = CARTESIAN_POINT ( 'NONE',  ( 10.81189881249999551, -6.242252689847874514, -95.96875000204838102 ) ) ;
#14412 = DIRECTION ( 'NONE',  ( -0.000000000000000000, -0.000000000000000000, 1.000000000000000000 ) ) ;
#14413 = CARTESIAN_POINT ( 'NONE',  ( 9.999999999999742428, 5.773502691896404748, -154.8749999999999716 ) ) ;
#14414 = CARTESIAN_POINT ( 'NONE',  ( -10.81189881249999907, -6.242252689847864744, -99.65625000204839523 ) ) ;
#14415 = CARTESIAN_POINT ( 'NONE',  ( 7.070501591499377789E-16, 11.54700538379251284, -182.0000000040968189 ) ) ;
#14416 = CARTESIAN_POINT ( 'NONE',  ( -5.405949406249996869, 9.363379034771805109, -105.8437500020483810 ) ) ;
#14417 = CARTESIAN_POINT ( 'NONE',  ( 10.81189881249999551, -6.242252689847874514, -175.6562500020484094 ) ) ;
#14418 = CARTESIAN_POINT ( 'NONE',  ( -2.121150477449813534E-15, -11.54700538379251284, -107.3749999999999858 ) ) ;
#14419 = CARTESIAN_POINT ( 'NONE',  ( 9.999999999999998224, 0.000000000000000000, -164.3750000040967905 ) ) ;
#14420 = CARTESIAN_POINT ( 'NONE',  ( 7.644554776091147741E-16, 12.48450537969573659, -194.6562500020484094 ) ) ;
#14421 = CARTESIAN_POINT ( 'NONE',  ( 10.81189881249999729, 0.000000000000000000, -53.84375000204835970 ) ) ;
#14422 = VECTOR ( 'NONE', #3864, 1000.000000000000000 ) ;
#14423 = CARTESIAN_POINT ( 'NONE',  ( -9.999999999999998224, 5.773502691896259087, -172.7500000040967905 ) ) ;
#14424 = CARTESIAN_POINT ( 'NONE',  ( 5.405949406249992428, -9.363379034771808662, -12.28125000204835438 ) ) ;
#14425 = CARTESIAN_POINT ( 'NONE',  ( -2.293366432827344421E-15, -12.48450537969573659, -24.21875000204837036 ) ) ;
#14426 = CARTESIAN_POINT ( 'NONE',  ( 10.00000000000025402, -5.773502691896113426, -158.5000000040968473 ) ) ;
#14427 = CARTESIAN_POINT ( 'NONE',  ( 5.405949406249999534, 9.363379034771803333, -127.0937500020483668 ) ) ;
#14428 = CARTESIAN_POINT ( 'NONE',  ( 4.999999999999992006, -8.660254037844389075, -95.24999999999998579 ) ) ;
#14429 = CARTESIAN_POINT ( 'NONE',  ( -10.81189881249999729, 1.324075727343319199E-15, -27.78125000204837036 ) ) ;
#14430 = CARTESIAN_POINT ( 'NONE',  ( -2.121150477449813534E-15, -11.54700538379251284, -103.2500000040967763 ) ) ;
#14431 = CARTESIAN_POINT ( 'NONE',  ( 9.999999999999998224, 0.000000000000000000, -102.5000000000000000 ) ) ;
#14432 = CARTESIAN_POINT ( 'NONE',  ( 5.000000000000000000, 8.660254037844385522, -54.24999999999996447 ) ) ;
#14433 = CARTESIAN_POINT ( 'NONE',  ( 5.405949406249992428, -9.363379034771808662, -121.7812500020483952 ) ) ;
#14434 = CARTESIAN_POINT ( 'NONE',  ( -10.81189881249999729, -6.242252689847864744, -111.6562500020483952 ) ) ;
#14435 = EDGE_CURVE ( 'NONE', #28591, #34451, #1545, .T. ) ;
#14436 = VERTEX_POINT ( 'NONE', #21380 ) ;
#14437 = CARTESIAN_POINT ( 'NONE',  ( 0.000000000000000000, 0.000000000000000000, -200.0000000000000000 ) ) ;
#14438 = CARTESIAN_POINT ( 'NONE',  ( 9.999999999999998224, 0.000000000000000000, -101.3750000040967905 ) ) ;
#14439 = CARTESIAN_POINT ( 'NONE',  ( 7.070501591499376803E-16, 11.54700538379251284, -91.62500000000000000 ) ) ;
#14440 = CARTESIAN_POINT ( 'NONE',  ( -10.81189881249999729, 1.324075727343319199E-15, -164.2812500020484094 ) ) ;
#14441 = CARTESIAN_POINT ( 'NONE',  ( -10.81189881249999907, -6.242252689847864744, -57.46875000204836681 ) ) ;
#14442 = ORIENTED_EDGE ( 'NONE', *, *, #35792, .F. ) ;
#14443 = CARTESIAN_POINT ( 'NONE',  ( 7.070501591499377789E-16, 11.54700538379251284, -27.12499999999998224 ) ) ;
#14444 = CARTESIAN_POINT ( 'NONE',  ( 10.81189881249999729, 0.000000000000000000, -36.03125000204837391 ) ) ;
#14445 = CARTESIAN_POINT ( 'NONE',  ( 10.00000000000000000, 5.773502691896255534, -163.8750000000000000 ) ) ;
#14446 = CARTESIAN_POINT ( 'NONE',  ( 0.000000000000000000, 0.000000000000000000, -200.0000000000000000 ) ) ;
#14447 = CARTESIAN_POINT ( 'NONE',  ( 5.000000000000000000, 8.660254037844385522, -24.62500000409675849 ) ) ;
#14448 = CARTESIAN_POINT ( 'NONE',  ( 5.000000000000000000, 8.660254037844385522, -168.2500000000000000 ) ) ;
#14449 = CARTESIAN_POINT ( 'NONE',  ( -2.293366432827344421E-15, -12.48450537969573659, -130.9062500020483810 ) ) ;
#14450 = CARTESIAN_POINT ( 'NONE',  ( -4.999999999999996447, 8.660254037844387298, -110.9999999999999858 ) ) ;
#14451 = DIRECTION ( 'NONE',  ( -0.000000000000000000, -0.000000000000000000, 1.000000000000000000 ) ) ;
#14452 = ORIENTED_EDGE ( 'NONE', *, *, #4812, .T. ) ;
#14453 = VECTOR ( 'NONE', #10901, 1000.000000000000000 ) ;
#14455 = ORIENTED_EDGE ( 'NONE', *, *, #3225, .F. ) ;
#14454 = ORIENTED_EDGE ( 'NONE', *, *, #22828, .T. ) ;
#14456 = DIRECTION ( 'NONE',  ( -0.000000000000000000, -0.000000000000000000, -1.000000000000000000 ) ) ;
#14457 = CARTESIAN_POINT ( 'NONE',  ( -5.000000000000003553, -8.660254037844383745, -146.8750000040967905 ) ) ;
#14459 = ADVANCED_FACE ( 'NONE', ( #17915 ), #37133, .T. ) ;
#14458 = CARTESIAN_POINT ( 'NONE',  ( 5.405949406249992428, -9.363379034771808662, -162.0937500020484094 ) ) ;
#14460 = CARTESIAN_POINT ( 'NONE',  ( -10.81189881249999729, 6.242252689847871849, -198.9062500020484094 ) ) ;
#14461 = CARTESIAN_POINT ( 'NONE',  ( -10.81189881249999729, 6.242252689847871849, -12.71875000204837747 ) ) ;
#14462 = DIRECTION ( 'NONE',  ( 1.000000000000000000, 0.000000000000000000, 0.000000000000000000 ) ) ;
#14463 = CARTESIAN_POINT ( 'NONE',  ( 10.81189881249999729, 0.000000000000000000, -145.3437500020483810 ) ) ;
#14464 = CARTESIAN_POINT ( 'NONE',  ( -10.81189881249999729, 6.242252689847871849, -134.2187500020483810 ) ) ;
#14465 = CARTESIAN_POINT ( 'NONE',  ( 7.644554776091147741E-16, 12.48450537969573659, -109.1562500020483810 ) ) ;
#14466 = CARTESIAN_POINT ( 'NONE',  ( -10.81189881249999907, -6.242252689847864744, -117.4687500020483952 ) ) ;
#14467 = CARTESIAN_POINT ( 'NONE',  ( -9.999999999999998224, 5.773502691896259087, -195.2500000040967905 ) ) ;
#14468 = CARTESIAN_POINT ( 'NONE',  ( -10.81189881249999907, -6.242252689847864744, -122.1562500020484094 ) ) ;
#14469 = CARTESIAN_POINT ( 'NONE',  ( 7.644554776091147741E-16, 12.48450537969573659, 0.5312499979516547288 ) ) ;
#14470 = CARTESIAN_POINT ( 'NONE',  ( -10.81189881249999729, 1.324075727343319199E-15, -134.0937500020483810 ) ) ;
#14471 = CARTESIAN_POINT ( 'NONE',  ( 9.999999999999998224, 0.000000000000000000, -123.5000000000000000 ) ) ;
#14472 = CARTESIAN_POINT ( 'NONE',  ( -9.999999999999998224, 1.224646799147353059E-15, -146.7500000000000000 ) ) ;
#14473 = CARTESIAN_POINT ( 'NONE',  ( 9.999999999999996447, -5.773502691896262640, -21.62499999999997868 ) ) ;
#14474 = CARTESIAN_POINT ( 'NONE',  ( -5.405949406250003975, -9.363379034771801557, -78.34375000204838102 ) ) ;
#14475 = CARTESIAN_POINT ( 'NONE',  ( -2.293366432827344421E-15, -12.48450537969573659, -67.71875000204838102 ) ) ;
#14476 = CARTESIAN_POINT ( 'NONE',  ( -5.000000000000003553, -8.660254037844383745, -170.5000000000000000 ) ) ;
#14477 = CARTESIAN_POINT ( 'NONE',  ( 5.405949406249999534, 9.363379034771803333, -31.28125000204837036 ) ) ;
#14478 = CARTESIAN_POINT ( 'NONE',  ( 5.405949406249992428, -9.363379034771808662, -45.09375000204837391 ) ) ;
#14479 = CARTESIAN_POINT ( 'NONE',  ( -9.999999999999998224, 1.224646799147353059E-15, -114.1250000040967763 ) ) ;
#14480 = CARTESIAN_POINT ( 'NONE',  ( 10.81189881249999551, -6.242252689847874514, -155.9687500020484094 ) ) ;
#14481 = CARTESIAN_POINT ( 'NONE',  ( 10.00000000000000000, 5.773502691896255534, -118.8749999999999858 ) ) ;
#14482 = CARTESIAN_POINT ( 'NONE',  ( -10.81189881249999729, 6.242252689847871849, -129.9062500020483810 ) ) ;
#14483 = CARTESIAN_POINT ( 'NONE',  ( 6.569481213899460492, 8.192167785318885009, -179.9999999999999716 ) ) ;
#14484 = CARTESIAN_POINT ( 'NONE',  ( 10.00000000000000000, 5.773502691896255534, -79.87499999999998579 ) ) ;
#14485 = CARTESIAN_POINT ( 'NONE',  ( -2.293366432827344421E-15, -12.48450537969573659, -21.40625000204837036 ) ) ;
#14486 = EDGE_LOOP ( 'NONE', ( #13845, #38765, #18452, #33651 ) ) ;
#14487 = CARTESIAN_POINT ( 'NONE',  ( 10.81189881249999729, 0.000000000000000000, -103.5312500020483810 ) ) ;
#14488 = CARTESIAN_POINT ( 'NONE',  ( -10.00000000000000000, -5.773502691896251982, -126.0000000040967905 ) ) ;
#14489 = CARTESIAN_POINT ( 'NONE',  ( 9.999999999999998224, 0.000000000000000000, -153.8750000040967905 ) ) ;
#14490 = AXIS2_PLACEMENT_3D ( 'NONE', #8797, #9428, #25420 ) ;
#14491 = CARTESIAN_POINT ( 'NONE',  ( -4.999999999999996447, 8.660254037844387298, -34.87500000409676915 ) ) ;
#14492 = EDGE_CURVE ( 'NONE', #36795, #32436, #41653, .T. ) ;
#14493 = CARTESIAN_POINT ( 'NONE',  ( 9.999999999998969713, 5.773502691896851502, -61.87499999999997158 ) ) ;
#14494 = CARTESIAN_POINT ( 'NONE',  ( 5.405949406249999534, 9.363379034771803333, -44.78125000204838102 ) ) ;
#14495 = CARTESIAN_POINT ( 'NONE',  ( -2.121150477449813534E-15, -11.54700538379251284, -40.25000000409676204 ) ) ;
#14496 = CARTESIAN_POINT ( 'NONE',  ( 10.81189881249999551, -6.242252689847874514, -156.1562500020484094 ) ) ;
#14497 = CARTESIAN_POINT ( 'NONE',  ( 10.81189881249999729, 0.000000000000000000, -128.8437500020484094 ) ) ;
#14498 = CARTESIAN_POINT ( 'NONE',  ( -9.999999999999998224, 1.224646799147353059E-15, -181.6250000040967905 ) ) ;
#14499 = VERTEX_POINT ( 'NONE', #20734 ) ;
#14500 = LINE ( 'NONE', #8275, #19694 ) ;
#14501 = ORIENTED_EDGE ( 'NONE', *, *, #18720, .F. ) ;
#14502 = ORIENTED_EDGE ( 'NONE', *, *, #28516, .F. ) ;
#14504 = ORIENTED_EDGE ( 'NONE', *, *, #37512, .T. ) ;
#14503 = CARTESIAN_POINT ( 'NONE',  ( -10.81189881249999729, 1.324075727343319199E-15, -108.5937500020483810 ) ) ;
#14505 = DIRECTION ( 'NONE',  ( 0.000000000000000000, -0.000000000000000000, 1.000000000000000000 ) ) ;
#14506 = CARTESIAN_POINT ( 'NONE',  ( -2.293366432827344421E-15, -12.48450537969573659, -187.7187500020484094 ) ) ;
#14507 = APPROVAL_PERSON_ORGANIZATION ( #315, #5680, #39992 ) ;
#14508 = CARTESIAN_POINT ( 'NONE',  ( 7.644554776091147741E-16, 12.48450537969573659, -42.96875000204835970 ) ) ;
#14509 = CARTESIAN_POINT ( 'NONE',  ( -7.481659653677922073, -6.786049171891036735, 9.002545116942492289E-15 ) ) ;
#14510 = CARTESIAN_POINT ( 'NONE',  ( -2.121150477449813534E-15, -11.54700538379251284, -74.37499999999997158 ) ) ;
#14511 = CARTESIAN_POINT ( 'NONE',  ( -5.405949406250003975, -9.363379034771801557, -168.3437500020484094 ) ) ;
#14512 = CARTESIAN_POINT ( 'NONE',  ( -2.293366432827344421E-15, -12.48450537969573659, -163.7187500020483810 ) ) ;
#14513 = CARTESIAN_POINT ( 'NONE',  ( 7.070501591499376803E-16, 11.54700538379251284, -178.6250000000000000 ) ) ;
#14514 = CARTESIAN_POINT ( 'NONE',  ( 7.644554776091147741E-16, 12.48450537969573659, -144.9687500020483810 ) ) ;
#14515 = CARTESIAN_POINT ( 'NONE',  ( -10.81189881249999729, 6.242252689847871849, -146.4062500020484094 ) ) ;
#14516 =( BOUNDED_CURVE ( )  B_SPLINE_CURVE ( 2, ( #3656, #26731, #27158, #425, #20033, #13751, #39885 ),
 .UNSPECIFIED., .F., .F. ) 
 B_SPLINE_CURVE_WITH_KNOTS ( ( 3, 2, 2, 3 ),
 ( 0.5149253731343285123, 0.5161691542288557866, 0.5174129353233831718, 0.5186567164179105571 ),
 .UNSPECIFIED. ) 
 CURVE ( )  GEOMETRIC_REPRESENTATION_ITEM ( )  RATIONAL_B_SPLINE_CURVE ( ( 0.9999999999999880096, 0.8660254037844506980, 1.000000000000000000, 0.8660254037844387076, 1.000000000000000000, 0.8660254037844267172, 1.000000000000011990 ) ) 
 REPRESENTATION_ITEM ( '' )  );
#14517 = CARTESIAN_POINT ( 'NONE',  ( -2.293366432827344421E-15, -12.48450537969573659, -154.7187500020483810 ) ) ;
#14518 = CARTESIAN_POINT ( 'NONE',  ( 4.999999999999992006, -8.660254037844389075, -93.74999999999998579 ) ) ;
#14519 = CARTESIAN_POINT ( 'NONE',  ( 9.999999999999998224, 0.000000000000000000, -200.0000000000000000 ) ) ;
#14520 = CARTESIAN_POINT ( 'NONE',  ( -9.999999999999998224, 5.773502691896259087, -178.3750000000000000 ) ) ;
#14521 = CARTESIAN_POINT ( 'NONE',  ( -10.81189881249999729, 6.242252689847871849, -92.21875000204838102 ) ) ;
#14522 = LINE ( 'NONE', #40853, #5899 ) ;
#14523 = CARTESIAN_POINT ( 'NONE',  ( -2.293366432827344421E-15, -12.48450537969573659, -57.40625000204838102 ) ) ;
#14524 = CARTESIAN_POINT ( 'NONE',  ( -9.999999999999998224, 1.224646799147353059E-15, -145.6250000040967905 ) ) ;
#14525 = CARTESIAN_POINT ( 'NONE',  ( -5.405949406250003975, -9.363379034771801557, -181.8437500020483810 ) ) ;
#14526 = CARTESIAN_POINT ( 'NONE',  ( -10.81189881249999729, 6.242252689847871849, -114.9062500020483952 ) ) ;
#14527 = CARTESIAN_POINT ( 'NONE',  ( -10.81189881249999729, -6.242252689847864744, -153.6562500020484094 ) ) ;
#14528 = CARTESIAN_POINT ( 'NONE',  ( 0.000000000000000000, 0.000000000000000000, -99.99999999999998579 ) ) ;
#14529 = CARTESIAN_POINT ( 'NONE',  ( 10.81189881249999551, -6.242252689847874514, -48.15625000204837391 ) ) ;
#14530 = CARTESIAN_POINT ( 'NONE',  ( 4.999999999999992006, -8.660254037844389075, -131.6250000040967620 ) ) ;
#14531 = CARTESIAN_POINT ( 'NONE',  ( -2.121150477449813534E-15, -11.54700538379251284, -107.3749999999999716 ) ) ;
#14532 = ORIENTED_EDGE ( 'NONE', *, *, #9837, .T. ) ;
#14533 = CARTESIAN_POINT ( 'NONE',  ( -10.81189881249999729, 1.324075727343319199E-15, -129.7812500020483810 ) ) ;
#14534 = CARTESIAN_POINT ( 'NONE',  ( 7.070501591499377789E-16, 11.54700538379251284, -144.5000000040967905 ) ) ;
#14535 = CARTESIAN_POINT ( 'NONE',  ( -5.000000000000003553, -8.660254037844383745, -167.5000000000000000 ) ) ;
#14536 = CARTESIAN_POINT ( 'NONE',  ( -10.81189881249999907, -6.242252689847864744, -182.1562500020483810 ) ) ;
#14537 = ORIENTED_EDGE ( 'NONE', *, *, #36496, .F. ) ;
#14538 = CARTESIAN_POINT ( 'NONE',  ( 4.999999999999992006, -8.660254037844389075, -50.24999999999998579 ) ) ;
#14539 = CARTESIAN_POINT ( 'NONE',  ( 10.81189881249999907, 6.242252689847868297, -173.7187500020484094 ) ) ;
#14540 = CARTESIAN_POINT ( 'NONE',  ( 9.999999999999998224, 0.000000000000000000, -60.87500000409676204 ) ) ;
#14541 = EDGE_CURVE ( 'NONE', #33113, #37078, #24031, .T. ) ;
#14542 = CARTESIAN_POINT ( 'NONE',  ( -9.214310226692173294E-15, -125.0000000000000000, 32.24999999999999289 ) ) ;
#14543 = FACE_OUTER_BOUND ( 'NONE', #17105, .T. ) ;
#14544 = ADVANCED_FACE ( 'NONE', ( #21161 ), #34347, .T. ) ;
#14545 = CARTESIAN_POINT ( 'NONE',  ( -2.293366432827344421E-15, -12.48450537969573659, -70.90625000204839523 ) ) ;
#14546 = CARTESIAN_POINT ( 'NONE',  ( -10.81189881249999729, 1.324075727343319199E-15, -51.78125000204835970 ) ) ;
#14547 = AXIS2_PLACEMENT_3D ( 'NONE', #29437, #35500, #29224 ) ;
#14548 = CARTESIAN_POINT ( 'NONE',  ( -4.999999999999996447, 8.660254037844387298, -42.37500000409677625 ) ) ;
#14549 = CARTESIAN_POINT ( 'NONE',  ( 5.405949406249992428, -9.363379034771808662, -3.093750002048367698 ) ) ;
#14550 = CARTESIAN_POINT ( 'NONE',  ( -9.999999999999998224, 0.000000000000000000, -99.99999999999998579 ) ) ;
#14551 = CARTESIAN_POINT ( 'NONE',  ( -10.81189881249999729, 6.242252689847871849, -179.4062500020484094 ) ) ;
#14552 = CC_DESIGN_APPROVAL ( #12231, ( #9061 ) ) ;
#14553 = CARTESIAN_POINT ( 'NONE',  ( -2.121150477449813534E-15, -11.54700538379251284, -73.25000000409676204 ) ) ;
#14554 = CARTESIAN_POINT ( 'NONE',  ( -9.999999999999998224, 0.000000000000000000, -99.99999999999998579 ) ) ;
#14555 = DIRECTION ( 'NONE',  ( -0.000000000000000000, -0.000000000000000000, -1.000000000000000000 ) ) ;
#14556 = DIRECTION ( 'NONE',  ( -0.000000000000000000, -0.000000000000000000, -1.000000000000000000 ) ) ;
#14557 = FACE_OUTER_BOUND ( 'NONE', #9436, .T. ) ;
#14558 = VECTOR ( 'NONE', #18836, 1000.000000000000000 ) ;
#14560 = ORIENTED_EDGE ( 'NONE', *, *, #14541, .F. ) ;
#14559 = CARTESIAN_POINT ( 'NONE',  ( -5.405949406249996869, 9.363379034771805109, -86.53125000204838102 ) ) ;
#14562 = VERTEX_POINT ( 'NONE', #8230 ) ;
#14561 = CARTESIAN_POINT ( 'NONE',  ( 9.999999999999998224, 0.000000000000000000, -200.0000000000000000 ) ) ;
#14563 = PRODUCT ( 'adapter', 'adapter', '', ( #16678 ) ) ;
#14564 = VERTEX_POINT ( 'NONE', #20516 ) ;
#14565 = CARTESIAN_POINT ( 'NONE',  ( 7.644554776091147741E-16, 12.48450537969573659, -33.96875000204834549 ) ) ;
#14566 = CARTESIAN_POINT ( 'NONE',  ( 5.405949406249992428, -9.363379034771808662, -28.59375000204836326 ) ) ;
#14567 = CARTESIAN_POINT ( 'NONE',  ( -5.405949406250003975, -9.363379034771801557, -17.03125000204835970 ) ) ;
#14568 = CARTESIAN_POINT ( 'NONE',  ( -10.81189881249999729, 6.242252689847871849, -63.71875000204838102 ) ) ;
#14569 = CARTESIAN_POINT ( 'NONE',  ( -2.121150477449813534E-15, -11.54700538379251284, -17.75000000409676204 ) ) ;
#14570 = CARTESIAN_POINT ( 'NONE',  ( 9.999999999999998224, 0.000000000000000000, -42.49999999999998579 ) ) ;
#14571 = ADVANCED_FACE ( 'NONE', ( #4129 ), #27865, .T. ) ;
#14572 = CARTESIAN_POINT ( 'NONE',  ( 5.405949406249992428, -9.363379034771808662, -186.0937500020483810 ) ) ;
#14573 = CARTESIAN_POINT ( 'NONE',  ( -10.81189881249999729, 6.242252689847871849, -165.7187500020483810 ) ) ;
#14574 = VECTOR ( 'NONE', #6481, 1000.000000000000000 ) ;
#14575 = CARTESIAN_POINT ( 'NONE',  ( 5.405949406249992428, -9.363379034771808662, -177.0937500020484094 ) ) ;
#14576 = CARTESIAN_POINT ( 'NONE',  ( 7.070501591499376803E-16, 11.54700538379251284, -132.1250000000000000 ) ) ;
#14577 = CARTESIAN_POINT ( 'NONE',  ( -9.999999999999998224, 1.224646799147353059E-15, -140.7500000000000000 ) ) ;
#14578 = DIRECTION ( 'NONE',  ( 0.000000000000000000, 0.000000000000000000, 1.000000000000000000 ) ) ;
#14579 = CARTESIAN_POINT ( 'NONE',  ( 9.999999999999998224, 0.000000000000000000, -186.5000000000000000 ) ) ;
#14580 = LOCAL_TIME ( 11, 57, 6.000000000000000000, #38799 ) ;
#14581 = CARTESIAN_POINT ( 'NONE',  ( -10.81189881249999729, 1.324075727343319199E-15, -110.0937500020483810 ) ) ;
#14582 = DIRECTION ( 'NONE',  ( -0.000000000000000000, -0.000000000000000000, 1.000000000000000000 ) ) ;
#14583 = CARTESIAN_POINT ( 'NONE',  ( -5.405949406250003975, -9.363379034771801557, -86.03125000204838102 ) ) ;
#14584 = CARTESIAN_POINT ( 'NONE',  ( -2.293366432827344421E-15, -12.48450537969573659, -102.2187500020483668 ) ) ;
#14585 = CARTESIAN_POINT ( 'NONE',  ( 5.405949406249999534, 9.363379034771803333, -62.59375000204836681 ) ) ;
#14586 = CARTESIAN_POINT ( 'NONE',  ( -10.81189881249999907, -6.242252689847864744, -68.15625000204839523 ) ) ;
#14587 = CARTESIAN_POINT ( 'NONE',  ( 9.999999999999996447, -5.773502691896262640, -155.5000000040968189 ) ) ;
#14588 = CARTESIAN_POINT ( 'NONE',  ( -5.000000000000003553, -8.660254037844383745, -130.0000000000000000 ) ) ;
#14589 = CARTESIAN_POINT ( 'NONE',  ( 10.81189881249999729, 6.242252689847867408, -154.4062500020483810 ) ) ;
#14590 = CARTESIAN_POINT ( 'NONE',  ( 5.405949406249992428, -9.363379034771808662, -165.2812500020484094 ) ) ;
#14591 = AXIS2_PLACEMENT_3D ( 'NONE', #20227, #6647, #10296 ) ;
#14592 = FACE_BOUND ( 'NONE', #23078, .T. ) ;
#14593 = CARTESIAN_POINT ( 'NONE',  ( -5.405949406249996869, 9.363379034771805109, -98.34375000204838102 ) ) ;
#14594 = CARTESIAN_POINT ( 'NONE',  ( 9.999999999999742428, 5.773502691896404748, -120.7500000040967905 ) ) ;
#14595 = CARTESIAN_POINT ( 'NONE',  ( -10.00000000000000000, -5.773502691896251982, -73.12499999999995737 ) ) ;
#14596 = CARTESIAN_POINT ( 'NONE',  ( 7.644554776091147741E-16, 12.48450537969573659, -192.9687500020483810 ) ) ;
#14597 = CARTESIAN_POINT ( 'NONE',  ( 4.999999999999992006, -8.660254037844389075, -82.12500000409676204 ) ) ;
#14598 = EDGE_CURVE ( 'NONE', #28673, #22153, #20988, .T. ) ;
#14599 = CARTESIAN_POINT ( 'NONE',  ( -4.999999999999996447, 8.660254037844387298, -25.87500000409675849 ) ) ;
#14600 = CARTESIAN_POINT ( 'NONE',  ( -10.81189881249999907, -6.242252689847864744, -98.15625000204839523 ) ) ;
#14601 = CARTESIAN_POINT ( 'NONE',  ( -10.81189881249999729, -6.242252689847864744, -77.15625000204836681 ) ) ;
#14602 = ADVANCED_FACE ( 'NONE', ( #23772 ), #18135, .T. ) ;
#14603 = CARTESIAN_POINT ( 'NONE',  ( -9.999999999999998224, 5.773502691896259087, -76.75000000409676204 ) ) ;
#14604 = CARTESIAN_POINT ( 'NONE',  ( -4.999999999999996447, 8.660254037844387298, -112.8750000040967763 ) ) ;
#14605 = CARTESIAN_POINT ( 'NONE',  ( 7.644554776091147741E-16, 12.48450537969573659, -36.96875000204835260 ) ) ;
#14606 = ORIENTED_EDGE ( 'NONE', *, *, #9588, .T. ) ;
#14607 = CARTESIAN_POINT ( 'NONE',  ( 10.81189881249999729, 0.000000000000000000, -198.0312500020484094 ) ) ;
#14608 = EDGE_CURVE ( 'NONE', #4966, #12865, #10584, .T. ) ;
#14609 = CARTESIAN_POINT ( 'NONE',  ( -10.81189881249999907, -6.242252689847864744, -24.65625000204838102 ) ) ;
#14610 = CARTESIAN_POINT ( 'NONE',  ( 7.644554776091147741E-16, 12.48450537969573659, -9.968750002048363257 ) ) ;
#14611 = CARTESIAN_POINT ( 'NONE',  ( -9.999999999999998224, 1.224646799147353059E-15, -142.2500000000000000 ) ) ;
#14612 = CARTESIAN_POINT ( 'NONE',  ( 4.999999999999992006, -8.660254037844389075, -4.125000004096768258 ) ) ;
#14613 = CARTESIAN_POINT ( 'NONE',  ( -10.81189881249999729, 6.242252689847871849, -131.4062500020484094 ) ) ;
#14614 = VECTOR ( 'NONE', #24587, 1000.000000000000000 ) ;
#14615 = CARTESIAN_POINT ( 'NONE',  ( 4.999999999999992006, -8.660254037844389075, -183.7500000000000000 ) ) ;
#14616 = FACE_OUTER_BOUND ( 'NONE', #26190, .T. ) ;
#14618 = ORIENTED_EDGE ( 'NONE', *, *, #15617, .T. ) ;
#14617 = CARTESIAN_POINT ( 'NONE',  ( -10.81189881249999729, 6.242252689847871849, -107.4062500020483810 ) ) ;
#14619 = CARTESIAN_POINT ( 'NONE',  ( 9.999999999999998224, 0.000000000000000000, -40.99999999999997868 ) ) ;
#14620 = ORIENTED_EDGE ( 'NONE', *, *, #16955, .T. ) ;
#14621 =( BOUNDED_CURVE ( )  B_SPLINE_CURVE ( 2, ( #36984, #11066, #23625, #30314, #26639, #13657, #20359 ),
 .UNSPECIFIED., .F., .F. ) 
 B_SPLINE_CURVE_WITH_KNOTS ( ( 3, 2, 2, 3 ),
 ( 0.2313432835820896372, 0.2325870646766169947, 0.2338308457711443245, 0.2350746268656717097 ),
 .UNSPECIFIED. ) 
 CURVE ( )  GEOMETRIC_REPRESENTATION_ITEM ( )  RATIONAL_B_SPLINE_CURVE ( ( 0.9999999999999910072, 0.8660254037844477004, 1.000000000000000000, 0.8660254037844387076, 1.000000000000000000, 0.8660254037844327124, 1.000000000000005995 ) ) 
 REPRESENTATION_ITEM ( '' )  );
#14622 = EDGE_LOOP ( 'NONE', ( #29136, #22710, #40357, #4111 ) ) ;
#14623 = ADVANCED_FACE ( 'NONE', ( #38005 ), #35268, .T. ) ;
#14624 = CARTESIAN_POINT ( 'NONE',  ( -5.405949406249996869, 9.363379034771805109, -35.53125000204837391 ) ) ;
#14625 = PERSON_AND_ORGANIZATION ( #11915, #17965 ) ;
#14626 = VECTOR ( 'NONE', #10199, 1000.000000000000000 ) ;
#14627 = CARTESIAN_POINT ( 'NONE',  ( 10.81189881249999907, 6.242252689847868297, -91.21875000204838102 ) ) ;
#14628 = CARTESIAN_POINT ( 'NONE',  ( 4.607092693325971489, 9.672354888048561250, -99.99999999999998579 ) ) ;
#14629 = CARTESIAN_POINT ( 'NONE',  ( 5.000000000000000000, 8.660254037844385522, -170.1250000040968189 ) ) ;
#14630 = CARTESIAN_POINT ( 'NONE',  ( 5.405949406249992428, -9.363379034771808662, -168.2812500020484094 ) ) ;
#14631 = CARTESIAN_POINT ( 'NONE',  ( -9.999999999999998224, 1.224646799147353059E-15, -173.7500000000000284 ) ) ;
#14632 = CARTESIAN_POINT ( 'NONE',  ( -10.81189881249999729, 1.324075727343319199E-15, -123.5937500020483952 ) ) ;
#14633 = CARTESIAN_POINT ( 'NONE',  ( 10.81189881249999907, 6.242252689847868297, -85.21875000204836681 ) ) ;
#14634 = CARTESIAN_POINT ( 'NONE',  ( -10.81189881249999729, 6.242252689847871849, -2.406250002048375247 ) ) ;
#14635 = CARTESIAN_POINT ( 'NONE',  ( 5.405949406249992428, -9.363379034771808662, -198.0937500020484094 ) ) ;
#14636 = CARTESIAN_POINT ( 'NONE',  ( 5.405949406249992428, -9.363379034771808662, -88.78125000204838102 ) ) ;
#14637 = CARTESIAN_POINT ( 'NONE',  ( -9.999999999999998224, 1.224646799147353059E-15, -177.1250000040968189 ) ) ;
#14638 = CARTESIAN_POINT ( 'NONE',  ( 7.644554776091147741E-16, 12.48450537969573659, -107.4687500020483668 ) ) ;
#14639 = CARTESIAN_POINT ( 'NONE',  ( -5.405949406250003975, -9.363379034771801557, -167.0312500020484094 ) ) ;
#14640 = CARTESIAN_POINT ( 'NONE',  ( -9.999999999999998224, 1.224646799147353059E-15, -28.62500000409676204 ) ) ;
#14641 = CARTESIAN_POINT ( 'NONE',  ( 10.81189881249999729, 0.000000000000000000, -171.0312500020484094 ) ) ;
#14642 = CARTESIAN_POINT ( 'NONE',  ( -2.293366432827344421E-15, -12.48450537969573659, -184.9062500020484094 ) ) ;
#14643 = CARTESIAN_POINT ( 'NONE',  ( 7.644554776091147741E-16, 12.48450537969573659, -51.96875000204836681 ) ) ;
#14644 = CARTESIAN_POINT ( 'NONE',  ( -4.999999999999996447, 8.660254037844387298, -175.8750000040967905 ) ) ;
#14645 = CARTESIAN_POINT ( 'NONE',  ( 10.81189881249999551, -6.242252689847874514, -12.15625000204835793 ) ) ;
#14646 = CARTESIAN_POINT ( 'NONE',  ( -10.81189881249999729, 1.324075727343319199E-15, -24.59375000204835970 ) ) ;
#14647 = CARTESIAN_POINT ( 'NONE',  ( -9.999999999999998224, 1.224646799147353059E-15, -153.1250000040967905 ) ) ;
#14648 = CARTESIAN_POINT ( 'NONE',  ( 10.81189881249999907, 6.242252689847868297, -118.2187500020483810 ) ) ;
#14649 = CARTESIAN_POINT ( 'NONE',  ( 9.999999999999996447, -5.773502691896262640, -96.62500000000000000 ) ) ;
#14650 = CARTESIAN_POINT ( 'NONE',  ( -10.81189881249999729, 1.324075727343319199E-15, -29.28125000204837036 ) ) ;
#14651 = CARTESIAN_POINT ( 'NONE',  ( 5.000000000000000000, 8.660254037844385522, -108.6250000040967763 ) ) ;
#14652 = CARTESIAN_POINT ( 'NONE',  ( -5.000000000000003553, -8.660254037844383745, -190.3750000040967905 ) ) ;
#14653 = CARTESIAN_POINT ( 'NONE',  ( 9.999999999999998224, 0.000000000000000000, -52.99999999999996447 ) ) ;
#14654 = CARTESIAN_POINT ( 'NONE',  ( -10.81189881249999729, 1.324075727343319199E-15, -120.7812500020483952 ) ) ;
#14655 = CARTESIAN_POINT ( 'NONE',  ( -10.81189881249999729, 1.324075727343319199E-15, -99.78125000204839523 ) ) ;
#14656 = ORIENTED_EDGE ( 'NONE', *, *, #2732, .F. ) ;
#14657 = CARTESIAN_POINT ( 'NONE',  ( -10.00000000000000000, -5.773502691896251982, -103.5000000040967763 ) ) ;
#14658 = CARTESIAN_POINT ( 'NONE',  ( -5.000000000000003553, -8.660254037844383745, -166.3750000040967905 ) ) ;
#14659 = CARTESIAN_POINT ( 'NONE',  ( 10.81189881249999907, 6.242252689847868297, -166.4062500020483810 ) ) ;
#14660 = CARTESIAN_POINT ( 'NONE',  ( 10.81189881249999551, -6.242252689847874514, -56.96875000204838102 ) ) ;
#14661 = EDGE_LOOP ( 'NONE', ( #6194, #9270 ) ) ;
#14662 = CARTESIAN_POINT ( 'NONE',  ( -10.00000000000000000, -5.773502691896251982, -28.12499999999998934 ) ) ;
#14663 = CARTESIAN_POINT ( 'NONE',  ( 10.81189881249999729, 0.000000000000000000, -24.03125000204836681 ) ) ;
#14664 = CARTESIAN_POINT ( 'NONE',  ( 9.999999999999998224, 0.000000000000000000, -159.5000000000000000 ) ) ;
#14665 = DIRECTION ( 'NONE',  ( 1.000000000000000000, 0.000000000000000000, 0.000000000000000000 ) ) ;
#14666 = CARTESIAN_POINT ( 'NONE',  ( 9.999999999999998224, 0.000000000000000000, -27.87500000409676204 ) ) ;
#14667 =( BOUNDED_CURVE ( )  B_SPLINE_CURVE ( 2, ( #26900, #29727, #16314, #40056, #29942, #23246, #29510 ),
 .UNSPECIFIED., .F., .F. ) 
 B_SPLINE_CURVE_WITH_KNOTS ( ( 3, 2, 2, 3 ),
 ( 0.4141791044776120256, 0.4154228855721394109, 0.4166666666666667962, 0.4179104477611941260 ),
 .UNSPECIFIED. ) 
 CURVE ( )  GEOMETRIC_REPRESENTATION_ITEM ( )  RATIONAL_B_SPLINE_CURVE ( ( 0.9999999999999880096, 0.8660254037844506980, 1.000000000000000000, 0.8660254037844387076, 1.000000000000000000, 0.8660254037844267172, 1.000000000000011990 ) ) 
 REPRESENTATION_ITEM ( '' )  );
#14668 = CARTESIAN_POINT ( 'NONE',  ( 9.999999999999998224, 0.000000000000000000, -22.99999999999996447 ) ) ;
#14669 = EDGE_CURVE ( 'NONE', #11871, #18780, #35627, .T. ) ;
#14670 = CARTESIAN_POINT ( 'NONE',  ( 10.81189881249999551, -6.242252689847874514, -130.6562500020484094 ) ) ;
#14671 = CARTESIAN_POINT ( 'NONE',  ( 1.490774595143464776, 10.17940913545393578, 1.249419088690773332E-14 ) ) ;
#14672 = CARTESIAN_POINT ( 'NONE',  ( 9.999999999999998224, 0.000000000000000000, -200.0000000000000000 ) ) ;
#14673 = VERTEX_POINT ( 'NONE', #8869 ) ;
#14674 =( BOUNDED_CURVE ( )  B_SPLINE_CURVE ( 2, ( #26953, #39898, #3878, #4083, #12916, #439, #23086 ),
 .UNSPECIFIED., .F., .F. ) 
 B_SPLINE_CURVE_WITH_KNOTS ( ( 3, 2, 2, 3 ),
 ( 0.7313432835820897759, 0.7325870646766171612, 0.7338308457711446575, 0.7350746268656719318 ),
 .UNSPECIFIED. ) 
 CURVE ( )  GEOMETRIC_REPRESENTATION_ITEM ( )  RATIONAL_B_SPLINE_CURVE ( ( 0.9999999999999761302, 0.8660254037844625774, 1.000000000000000000, 0.8660254037844387076, 1.000000000000000000, 0.8660254037844028474, 1.000000000000035971 ) ) 
 REPRESENTATION_ITEM ( '' )  );
#14675 = CARTESIAN_POINT ( 'NONE',  ( 10.81189881249999729, 0.000000000000000000, -60.03125000204836681 ) ) ;
#14677 = VERTEX_POINT ( 'NONE', #25700 ) ;
#14676 = VERTEX_POINT ( 'NONE', #22031 ) ;
#14678 = CARTESIAN_POINT ( 'NONE',  ( -9.999999999999998224, 1.224646799147353059E-15, -126.1250000040967620 ) ) ;
#14679 = CARTESIAN_POINT ( 'NONE',  ( 10.81189881249999729, 0.000000000000000000, -157.3437500020483810 ) ) ;
#14680 = CARTESIAN_POINT ( 'NONE',  ( -10.81189881249999729, 1.324075727343319199E-15, -189.7812500020484094 ) ) ;
#14681 = CARTESIAN_POINT ( 'NONE',  ( -10.81189881249999907, -6.242252689847864744, -12.46875000204837391 ) ) ;
#14682 = DIRECTION ( 'NONE',  ( -0.000000000000000000, -0.000000000000000000, 1.000000000000000000 ) ) ;
#14683 = CARTESIAN_POINT ( 'NONE',  ( 10.81189881249999551, -6.242252689847874514, -151.4687500020484094 ) ) ;
#14684 = CARTESIAN_POINT ( 'NONE',  ( 10.81189881249999551, -6.242252689847874514, -131.9687500020483810 ) ) ;
#14685 = CARTESIAN_POINT ( 'NONE',  ( -10.81189881249999729, 6.242252689847871849, -110.4062500020483810 ) ) ;
#14686 = CARTESIAN_POINT ( 'NONE',  ( 10.81189881249999551, -6.242252689847874514, -113.9687500020483810 ) ) ;
#14687 = CARTESIAN_POINT ( 'NONE',  ( 10.81189881249999729, 0.000000000000000000, -127.5312500020483952 ) ) ;
#14688 = CARTESIAN_POINT ( 'NONE',  ( 7.644554776091147741E-16, 12.48450537969573659, -3.968750002048366810 ) ) ;
#14689 = CARTESIAN_POINT ( 'NONE',  ( 10.81189881249999729, 0.000000000000000000, -131.8437500020484094 ) ) ;
#14690 = CARTESIAN_POINT ( 'NONE',  ( 4.999999999999992006, -8.660254037844389075, -54.74999999999996447 ) ) ;
#14691 = FACE_OUTER_BOUND ( 'NONE', #4375, .T. ) ;
#14692 = CARTESIAN_POINT ( 'NONE',  ( 7.070501591499377789E-16, 11.54700538379251284, -148.6250000000000000 ) ) ;
#14693 = CARTESIAN_POINT ( 'NONE',  ( -5.000000000000003553, -8.660254037844383745, -20.49999999999996447 ) ) ;
#14694 = CARTESIAN_POINT ( 'NONE',  ( -10.81189881249999729, 6.242252689847871849, -72.71875000204836681 ) ) ;
#14695 = CARTESIAN_POINT ( 'NONE',  ( -5.405949406250003975, -9.363379034771801557, -66.34375000204836681 ) ) ;
#14696 = CARTESIAN_POINT ( 'NONE',  ( -9.999999999999998224, 1.224646799147353059E-15, -136.2499999999999716 ) ) ;
#14697 = CARTESIAN_POINT ( 'NONE',  ( 10.81189881249999551, -6.242252689847874514, -31.65625000204834905 ) ) ;
#14698 = CARTESIAN_POINT ( 'NONE',  ( -2.293366432827344421E-15, -12.48450537969573659, -42.21875000204835970 ) ) ;
#14699 = CYLINDRICAL_SURFACE ( 'NONE', #30932, 9.999999999999998224 ) ;
#14700 = CARTESIAN_POINT ( 'NONE',  ( -5.405949406250003975, -9.363379034771801557, -154.8437500020483810 ) ) ;
#14701 = CARTESIAN_POINT ( 'NONE',  ( 5.000000000000000000, 8.660254037844385522, -123.2500000000000000 ) ) ;
#14702 = CARTESIAN_POINT ( 'NONE',  ( -10.81189881249999729, 1.324075727343319199E-15, -129.7812500020483810 ) ) ;
#14703 = CARTESIAN_POINT ( 'NONE',  ( 10.00000000000000000, 5.773502691896255534, -73.87499999999995737 ) ) ;
#14704 = CARTESIAN_POINT ( 'NONE',  ( 5.405949406249999534, 9.363379034771803333, -10.28125000204835260 ) ) ;
#14705 = ORIENTED_EDGE ( 'NONE', *, *, #20946, .F. ) ;
#14706 = CARTESIAN_POINT ( 'NONE',  ( 7.644554776091147741E-16, 12.48450537969573659, -100.1562500020483952 ) ) ;
#14707 = CARTESIAN_POINT ( 'NONE',  ( 7.070501591499377789E-16, 11.54700538379251284, -125.0000000040967763 ) ) ;
#14708 = DIRECTION ( 'NONE',  ( -0.000000000000000000, -0.000000000000000000, 1.000000000000000000 ) ) ;
#14709 = CARTESIAN_POINT ( 'NONE',  ( -10.81189881249999907, -6.242252689847864744, -85.96875000204836681 ) ) ;
#14710 = CARTESIAN_POINT ( 'NONE',  ( 9.999999999999998224, 0.000000000000000000, -36.87500000409676915 ) ) ;
#14711 = CARTESIAN_POINT ( 'NONE',  ( 9.999999999999479527, 5.773502691896553074, -75.37499999999998579 ) ) ;
#14712 = CARTESIAN_POINT ( 'NONE',  ( -5.405949406249996869, 9.363379034771805109, -43.03125000204838102 ) ) ;
#14713 = DIRECTION ( 'NONE',  ( 1.000000000000000000, 0.000000000000000000, 0.000000000000000000 ) ) ;
#14714 = CARTESIAN_POINT ( 'NONE',  ( 5.405949406249999534, 9.363379034771803333, -155.7812500020484094 ) ) ;
#14715 = CARTESIAN_POINT ( 'NONE',  ( -2.293366432827344421E-15, -12.48450537969573659, -130.7187500020483810 ) ) ;
#14716 = CARTESIAN_POINT ( 'NONE',  ( 9.999999999999998224, 0.000000000000000000, -95.37500000409677625 ) ) ;
#14717 = EDGE_LOOP ( 'NONE', ( #26203, #12443, #20383, #7049 ) ) ;
#14718 = CARTESIAN_POINT ( 'NONE',  ( 7.070501591499376803E-16, 11.54700538379251284, -177.1250000000000000 ) ) ;
#14719 = ORIENTED_EDGE ( 'NONE', *, *, #17580, .T. ) ;
#14720 = ORIENTED_EDGE ( 'NONE', *, *, #38855, .F. ) ;
#14721 = EDGE_LOOP ( 'NONE', ( #40551, #10567, #18398, #25327 ) ) ;
#14722 = CARTESIAN_POINT ( 'NONE',  ( -9.999999999999998224, 1.224646799147353059E-15, -200.0000000000000000 ) ) ;
#14723 = CARTESIAN_POINT ( 'NONE',  ( -10.81189881249999729, 6.242252689847871849, -189.7187500020484379 ) ) ;
#14724 = CARTESIAN_POINT ( 'NONE',  ( -10.81189881249999729, 1.324075727343319199E-15, -36.59375000204836681 ) ) ;
#14725 = CARTESIAN_POINT ( 'NONE',  ( -5.599846275199223733, -8.529742854289207088, 2.111525036386693496E-16 ) ) ;
#14726 = DIRECTION ( 'NONE',  ( -0.000000000000000000, -0.000000000000000000, 1.000000000000000000 ) ) ;
#14727 = CARTESIAN_POINT ( 'NONE',  ( 5.405949406249999534, 9.363379034771803333, -175.0937500020484094 ) ) ;
#14728 = CARTESIAN_POINT ( 'NONE',  ( 7.644554776091147741E-16, 12.48450537969573659, -156.9687500020484094 ) ) ;
#14729 =( BOUNDED_CURVE ( )  B_SPLINE_CURVE ( 2, ( #38136, #31460, #25205, #17838, #8152, #34703, #38346 ),
 .UNSPECIFIED., .F., .F. ) 
 B_SPLINE_CURVE_WITH_KNOTS ( ( 3, 2, 2, 3 ),
 ( 0.2798507462686568026, 0.2810945273631841879, 0.2823383084577115731, 0.2835820895522389029 ),
 .UNSPECIFIED. ) 
 CURVE ( )  GEOMETRIC_REPRESENTATION_ITEM ( )  RATIONAL_B_SPLINE_CURVE ( ( 0.9999999999999880096, 0.8660254037844506980, 1.000000000000000000, 0.8660254037844387076, 1.000000000000000000, 0.8660254037844267172, 1.000000000000011990 ) ) 
 REPRESENTATION_ITEM ( '' )  );
#14730 = CARTESIAN_POINT ( 'NONE',  ( -9.999999999999998224, 1.224646799147353059E-15, -33.12500000409676915 ) ) ;
#14731 = CARTESIAN_POINT ( 'NONE',  ( 10.81189881249999729, 0.000000000000000000, -140.8437500020483810 ) ) ;
#14732 = CARTESIAN_POINT ( 'NONE',  ( -10.81189881249999907, -6.242252689847864744, -152.1562500020484094 ) ) ;
#14733 = CARTESIAN_POINT ( 'NONE',  ( -10.81189881249999729, -6.242252689847864744, -153.4687500020484094 ) ) ;
#14734 = CARTESIAN_POINT ( 'NONE',  ( 5.000000000000000000, 8.660254037844385522, -126.6250000040967620 ) ) ;
#14735 = CYLINDRICAL_SURFACE ( 'NONE', #27525, 9.999999999999998224 ) ;
#14736 = CARTESIAN_POINT ( 'NONE',  ( -2.121150477449813534E-15, -11.54700538379251284, -170.3750000000000284 ) ) ;
#14737 = CARTESIAN_POINT ( 'NONE',  ( 5.405949406249999534, 9.363379034771803333, -92.59375000204838102 ) ) ;
#14738 = CARTESIAN_POINT ( 'NONE',  ( 9.999999999999548805, 5.773502691896515771, -180.7500000040967905 ) ) ;
#14739 = CARTESIAN_POINT ( 'NONE',  ( -5.405949406249996869, 9.363379034771805109, -58.03125000204836681 ) ) ;
#14740 = DIRECTION ( 'NONE',  ( 1.000000000000000000, 0.000000000000000000, 0.000000000000000000 ) ) ;
#14741 = CARTESIAN_POINT ( 'NONE',  ( -5.405949406250003975, -9.363379034771801557, -180.3437500020483810 ) ) ;
#14742 = CARTESIAN_POINT ( 'NONE',  ( -2.293366432827344421E-15, -12.48450537969573659, -111.4062500020483952 ) ) ;
#14743 = CARTESIAN_POINT ( 'NONE',  ( -5.405949406249996869, 9.363379034771805109, -152.5312500020484094 ) ) ;
#14744 = DIRECTION ( 'NONE',  ( -1.000000000000000000, 0.000000000000000000, 0.000000000000000000 ) ) ;
#14745 = CARTESIAN_POINT ( 'NONE',  ( 10.81189881249999551, -6.242252689847874514, -42.15625000204836681 ) ) ;
#14746 = CARTESIAN_POINT ( 'NONE',  ( -9.999999999999998224, 1.224646799147353059E-15, -132.1250000040967620 ) ) ;
#14747 = CARTESIAN_POINT ( 'NONE',  ( -9.999999999999998224, 5.773502691896259087, -95.87499999999998579 ) ) ;
#14748 = VERTEX_POINT ( 'NONE', #5839 ) ;
#14749 = CARTESIAN_POINT ( 'NONE',  ( 10.81189881249999729, 0.000000000000000000, -124.5312500020483952 ) ) ;
#14750 = CARTESIAN_POINT ( 'NONE',  ( 10.00000000000000000, 5.773502691896255534, -150.7500000040967905 ) ) ;
#14751 = CARTESIAN_POINT ( 'NONE',  ( 0.000000000000000000, 0.000000000000000000, -99.99999999999998579 ) ) ;
#14752 = CARTESIAN_POINT ( 'NONE',  ( 10.81189881249999551, -6.242252689847874514, -181.6562500020484379 ) ) ;
#14753 = EDGE_LOOP ( 'NONE', ( #18977, #16892, #103, #21378 ) ) ;
#14754 = CARTESIAN_POINT ( 'NONE',  ( -10.81189881249999729, 1.324075727343319199E-15, -173.0937500020484094 ) ) ;
#14755 = CARTESIAN_POINT ( 'NONE',  ( -9.999999999999998224, 5.773502691896259087, -54.25000000409677625 ) ) ;
#14756 = DIRECTION ( 'NONE',  ( -0.000000000000000000, -0.000000000000000000, 1.000000000000000000 ) ) ;
#14757 = CARTESIAN_POINT ( 'NONE',  ( -10.00000000000076916, 5.773502691895813221, -135.2500000040967905 ) ) ;
#14758 = CARTESIAN_POINT ( 'NONE',  ( -10.81189881249999729, 1.324075727343319199E-15, -71.28125000204838102 ) ) ;
#14759 = CARTESIAN_POINT ( 'NONE',  ( -5.405949406249996869, 9.363379034771805109, -50.53125000204835970 ) ) ;
#14760 = CARTESIAN_POINT ( 'NONE',  ( 7.070501591499377789E-16, 11.54700538379251284, -45.50000000409676915 ) ) ;
#14761 = CARTESIAN_POINT ( 'NONE',  ( 10.81189881249999907, 6.242252689847868297, -1.218750002048352155 ) ) ;
#14762 = CARTESIAN_POINT ( 'NONE',  ( 5.405949406249999534, 9.363379034771803333, -175.2812500020484094 ) ) ;
#14763 = CARTESIAN_POINT ( 'NONE',  ( -9.999999999999998224, 1.224646799147353059E-15, -200.0000000000000000 ) ) ;
#14764 = CARTESIAN_POINT ( 'NONE',  ( 9.999999999999998224, 0.000000000000000000, -149.0000000000000000 ) ) ;
#14765 = ORIENTED_EDGE ( 'NONE', *, *, #23660, .T. ) ;
#14766 = CARTESIAN_POINT ( 'NONE',  ( -10.00000000000154188, 5.773502691895366468, -16.75000000409671586 ) ) ;
#14767 = CARTESIAN_POINT ( 'NONE',  ( 60.00000000000000711, 7.347880794884119933E-15, -223.0000000000000000 ) ) ;
#14768 = CARTESIAN_POINT ( 'NONE',  ( 0.000000000000000000, 0.000000000000000000, -200.0000000000000000 ) ) ;
#14770 = ORIENTED_EDGE ( 'NONE', *, *, #8798, .F. ) ;
#14769 = CARTESIAN_POINT ( 'NONE',  ( -10.81189881249999729, 1.324075727343319199E-15, -83.28125000204838102 ) ) ;
#14771 = LINE ( 'NONE', #31424, #31062 ) ;
#14773 = ORIENTED_EDGE ( 'NONE', *, *, #10123, .F. ) ;
#14772 = LINE ( 'NONE', #34240, #29609 ) ;
#14774 = ORIENTED_EDGE ( 'NONE', *, *, #32403, .T. ) ;
#14775 =( BOUNDED_CURVE ( )  B_SPLINE_CURVE ( 2, ( #2486, #41949, #5291, #18444, #15614, #12381, #12802 ),
 .UNSPECIFIED., .F., .F. ) 
 B_SPLINE_CURVE_WITH_KNOTS ( ( 3, 2, 2, 3 ),
 ( 0.1082089552238805485, 0.1094527363184079616, 0.1106965174129353746, 0.1119402985074627876 ),
 .UNSPECIFIED. ) 
 CURVE ( )  GEOMETRIC_REPRESENTATION_ITEM ( )  RATIONAL_B_SPLINE_CURVE ( ( 1.000000000000004441, 0.8660254037844343777, 1.000000000000000000, 0.8660254037844387076, 1.000000000000000000, 0.8660254037844282715, 1.000000000000010436 ) ) 
 REPRESENTATION_ITEM ( '' )  );
#14776 = CARTESIAN_POINT ( 'NONE',  ( 5.405949406249999534, 9.363379034771803333, -40.09375000204837391 ) ) ;
#14777 = DIRECTION ( 'NONE',  ( -0.000000000000000000, -0.000000000000000000, 1.000000000000000000 ) ) ;
#14778 = CARTESIAN_POINT ( 'NONE',  ( 5.405949406249999534, 9.363379034771803333, -13.28125000204835615 ) ) ;
#14780 = ORIENTED_EDGE ( 'NONE', *, *, #27800, .F. ) ;
#14779 = CARTESIAN_POINT ( 'NONE',  ( -10.81189881249999907, -6.242252689847864744, -66.46875000204838102 ) ) ;
#14781 = EDGE_CURVE ( 'NONE', #41753, #32304, #31761, .T. ) ;
#14782 = CARTESIAN_POINT ( 'NONE',  ( -5.000000000000003553, -8.660254037844383745, -36.99999999999997868 ) ) ;
#14783 = CARTESIAN_POINT ( 'NONE',  ( 10.81189881249999907, 6.242252689847868297, -187.2187500020484094 ) ) ;
#14784 = CARTESIAN_POINT ( 'NONE',  ( 10.81189881249999907, 6.242252689847868297, -166.2187500020484094 ) ) ;
#14785 = CARTESIAN_POINT ( 'NONE',  ( -10.81189881249999729, 1.324075727343319199E-15, -176.0937500020484094 ) ) ;
#14786 = CARTESIAN_POINT ( 'NONE',  ( -9.999999999999998224, 1.224646799147353059E-15, -131.7499999999999716 ) ) ;
#14787 = VECTOR ( 'NONE', #38554, 1000.000000000000000 ) ;
#14788 = DIRECTION ( 'NONE',  ( -0.000000000000000000, -0.000000000000000000, 1.000000000000000000 ) ) ;
#14789 = DIRECTION ( 'NONE',  ( 1.000000000000000000, 0.000000000000000000, 0.000000000000000000 ) ) ;
#14790 = CARTESIAN_POINT ( 'NONE',  ( 7.070501591499377789E-16, 11.54700538379251284, -192.1250000000000000 ) ) ;
#14791 = CARTESIAN_POINT ( 'NONE',  ( 10.81189881249999907, 6.242252689847868297, -112.2187500020483810 ) ) ;
#14792 = DIRECTION ( 'NONE',  ( -0.000000000000000000, -1.000000000000000000, -0.000000000000000000 ) ) ;
#14793 = CARTESIAN_POINT ( 'NONE',  ( -2.293366432827344421E-15, -12.48450537969573659, -79.90625000204839523 ) ) ;
#14794 = CARTESIAN_POINT ( 'NONE',  ( 10.81189881249999729, 6.242252689847867408, -88.21875000204838102 ) ) ;
#14795 = CARTESIAN_POINT ( 'NONE',  ( -5.405949406249996869, 9.363379034771805109, -62.34375000204836681 ) ) ;
#14796 = CARTESIAN_POINT ( 'NONE',  ( 5.405949406249999534, 9.363379034771803333, -68.78125000204838102 ) ) ;
#14797 = CARTESIAN_POINT ( 'NONE',  ( 7.070501591499377789E-16, 11.54700538379251284, -150.5000000040968189 ) ) ;
#14798 = CARTESIAN_POINT ( 'NONE',  ( 10.00000000000000000, 5.773502691896255534, -127.8749999999999858 ) ) ;
#14799 = CARTESIAN_POINT ( 'NONE',  ( -5.405949406250003975, -9.363379034771801557, -152.0312500020484094 ) ) ;
#14800 = CARTESIAN_POINT ( 'NONE',  ( -5.405949406249996869, 9.363379034771805109, -167.5312500020484094 ) ) ;
#14801 = CARTESIAN_POINT ( 'NONE',  ( -10.00000000000051337, 5.773502691895962435, -97.75000000409676204 ) ) ;
#14802 = CYLINDRICAL_SURFACE ( 'NONE', #10275, 9.999999999999998224 ) ;
#14803 = CARTESIAN_POINT ( 'NONE',  ( 5.405949406249992428, -9.363379034771808662, -100.5937500020483810 ) ) ;
#14804 = CARTESIAN_POINT ( 'NONE',  ( 9.999999999999998224, 0.000000000000000000, -10.99999999999995381 ) ) ;
#14805 = CARTESIAN_POINT ( 'NONE',  ( 9.999999999999998224, 0.000000000000000000, -72.49999999999998579 ) ) ;
#14806 = CARTESIAN_POINT ( 'NONE',  ( 5.405949406249992428, -9.363379034771808662, -195.0937500020484094 ) ) ;
#14807 = CARTESIAN_POINT ( 'NONE',  ( 7.070501591499377789E-16, 11.54700538379251284, -78.50000000409677625 ) ) ;
#14808 = CARTESIAN_POINT ( 'NONE',  ( -8.660253955908514101, -5.000000141917089636, -180.0000000000000284 ) ) ;
#14809 = CARTESIAN_POINT ( 'NONE',  ( 10.81189881249999907, 6.242252689847868297, -94.40625000204836681 ) ) ;
#14810 = VECTOR ( 'NONE', #3160, 1000.000000000000000 ) ;
#14811 = CARTESIAN_POINT ( 'NONE',  ( 5.405949406249992428, -9.363379034771808662, -75.28125000204838102 ) ) ;
#14812 = CARTESIAN_POINT ( 'NONE',  ( -9.999999999999998224, 5.773502691896259087, -67.75000000409677625 ) ) ;
#14813 = CARTESIAN_POINT ( 'NONE',  ( 7.070501591499376803E-16, 11.54700538379251284, -135.1250000000000000 ) ) ;
#14814 = CARTESIAN_POINT ( 'NONE',  ( 10.81189881249999729, 0.000000000000000000, -28.34375000204836326 ) ) ;
#14815 = ORIENTED_EDGE ( 'NONE', *, *, #36380, .F. ) ;
#14816 = CARTESIAN_POINT ( 'NONE',  ( -9.999999999999998224, 5.773502691896259087, -1.374999999999974465 ) ) ;
#14817 = CARTESIAN_POINT ( 'NONE',  ( 10.81189881249999907, 6.242252689847868297, -22.40625000204838102 ) ) ;
#14818 = CARTESIAN_POINT ( 'NONE',  ( -5.405949406249996869, 9.363379034771805109, -12.84375000204834905 ) ) ;
#14819 = CARTESIAN_POINT ( 'NONE',  ( 10.00000000000000000, 5.773502691896255534, -5.250000004096754935 ) ) ;
#14820 = FACE_OUTER_BOUND ( 'NONE', #2940, .T. ) ;
#14821 = CARTESIAN_POINT ( 'NONE',  ( 5.405949406249992428, -9.363379034771808662, -129.2812500020483810 ) ) ;
#14822 = CARTESIAN_POINT ( 'NONE',  ( -9.999999999999998224, 1.224646799147353059E-15, -184.2500000000000000 ) ) ;
#14823 = DIRECTION ( 'NONE',  ( 1.000000000000000000, 0.000000000000000000, 0.000000000000000000 ) ) ;
#14825 = ORIENTED_EDGE ( 'NONE', *, *, #12742, .F. ) ;
#14824 = CARTESIAN_POINT ( 'NONE',  ( 5.405949406249999534, 9.363379034771803333, -112.2812500020483952 ) ) ;
#14826 = DIRECTION ( 'NONE',  ( 1.000000000000000000, 0.000000000000000000, 0.000000000000000000 ) ) ;
#14827 = ORIENTED_EDGE ( 'NONE', *, *, #11385, .T. ) ;
#14828 = ORIENTED_EDGE ( 'NONE', *, *, #5361, .T. ) ;
#14829 = CARTESIAN_POINT ( 'NONE',  ( 10.81189881249999729, 0.000000000000000000, -34.53125000204837391 ) ) ;
#14830 = PERSON_AND_ORGANIZATION ( #11915, #17965 ) ;
#14831 = CARTESIAN_POINT ( 'NONE',  ( -2.293366432827344421E-15, -12.48450537969573659, -87.21875000204838102 ) ) ;
#14832 = CARTESIAN_POINT ( 'NONE',  ( 9.999999999999998224, 0.000000000000000000, -90.87500000409677625 ) ) ;
#14833 = EDGE_CURVE ( 'NONE', #3489, #9539, #13535, .T. ) ;
#14834 = CARTESIAN_POINT ( 'NONE',  ( -5.000000000000003553, -8.660254037844383745, -108.9999999999999858 ) ) ;
#14835 = EDGE_CURVE ( 'NONE', #38736, #13374, #35414, .T. ) ;
#14836 = VECTOR ( 'NONE', #15421, 1000.000000000000000 ) ;
#14837 = ADVANCED_FACE ( 'NONE', ( #2190 ), #38850, .T. ) ;
#14838 = DIRECTION ( 'NONE',  ( -0.000000000000000000, -0.000000000000000000, -1.000000000000000000 ) ) ;
#14839 = CARTESIAN_POINT ( 'NONE',  ( -5.405949406250003975, -9.363379034771801557, -168.5312500020484094 ) ) ;
#14840 = CARTESIAN_POINT ( 'NONE',  ( 4.999999999999992006, -8.660254037844389075, -68.24999999999997158 ) ) ;
#14841 = CARTESIAN_POINT ( 'NONE',  ( -10.81189881249999729, 1.324075727343319199E-15, -126.5937500020483668 ) ) ;
#14842 = AXIS2_PLACEMENT_3D ( 'NONE', #8748, #41314, #38095 ) ;
#14843 = PRODUCT_RELATED_PRODUCT_CATEGORY ( 'detail', '', ( #18390 ) ) ;
#14844 = CARTESIAN_POINT ( 'NONE',  ( -5.405949406249996869, 9.363379034771805109, -87.84375000204836681 ) ) ;
#14845 = CARTESIAN_POINT ( 'NONE',  ( 10.81189881249999729, 6.242252689847867408, -4.406250002048352599 ) ) ;
#14846 = CARTESIAN_POINT ( 'NONE',  ( -2.293366432827344421E-15, -12.48450537969573659, -192.2187500020484379 ) ) ;
#14847 = CARTESIAN_POINT ( 'NONE',  ( -5.405949406250003975, -9.363379034771801557, -92.03125000204838102 ) ) ;
#14848 = CARTESIAN_POINT ( 'NONE',  ( 9.999999999999998224, 0.000000000000000000, -180.8750000040967905 ) ) ;
#14849 = CARTESIAN_POINT ( 'NONE',  ( 10.81189881249999551, -6.242252689847874514, -166.6562500020484094 ) ) ;
#14850 = CARTESIAN_POINT ( 'NONE',  ( 5.000000000000000000, 8.660254037844385522, -103.7500000000000000 ) ) ;
#14851 = CARTESIAN_POINT ( 'NONE',  ( -10.81189881249999729, -6.242252689847864744, -174.6562500020484094 ) ) ;
#14852 = CARTESIAN_POINT ( 'NONE',  ( 10.81189881249999551, -6.242252689847874514, -187.6562500020484379 ) ) ;
#14853 = CARTESIAN_POINT ( 'NONE',  ( -5.405949406249996869, 9.363379034771805109, -51.84375000204835260 ) ) ;
#14854 = CARTESIAN_POINT ( 'NONE',  ( 10.00000000000000000, 5.773502691896255534, -161.2500000040967905 ) ) ;
#14855 = CARTESIAN_POINT ( 'NONE',  ( 7.644554776091147741E-16, 12.48450537969573659, -8.656250002048372139 ) ) ;
#14856 = CARTESIAN_POINT ( 'NONE',  ( -10.81189881249999729, 6.242252689847871849, -14.21875000204836326 ) ) ;
#14857 = CARTESIAN_POINT ( 'NONE',  ( -5.000000000000003553, -8.660254037844383745, -152.8750000040967905 ) ) ;
#14858 = CARTESIAN_POINT ( 'NONE',  ( -5.405949406249996869, 9.363379034771805109, -123.8437500020483952 ) ) ;
#14859 = CARTESIAN_POINT ( 'NONE',  ( -10.00000000000000000, -5.773502691896251982, -98.62499999999998579 ) ) ;
#14860 = CARTESIAN_POINT ( 'NONE',  ( -5.405949406249996869, 9.363379034771805109, -23.53125000204836681 ) ) ;
#14861 = CARTESIAN_POINT ( 'NONE',  ( -4.999999999999996447, 8.660254037844387298, -103.8750000040967763 ) ) ;
#14862 = CARTESIAN_POINT ( 'NONE',  ( -2.121150477449813534E-15, -11.54700538379251284, -136.2500000040967905 ) ) ;
#14863 = CARTESIAN_POINT ( 'NONE',  ( 10.00000000000000000, 5.773502691896255534, -49.87499999999997158 ) ) ;
#14864 = CARTESIAN_POINT ( 'NONE',  ( 5.405949406249999534, 9.363379034771803333, -113.7812500020483952 ) ) ;
#14865 = CARTESIAN_POINT ( 'NONE',  ( 10.81189881249999729, 0.000000000000000000, -96.03125000204838102 ) ) ;
#14866 = EDGE_LOOP ( 'NONE', ( #1912, #18831 ) ) ;
#14867 = CARTESIAN_POINT ( 'NONE',  ( -10.00000000000000000, -5.773502691896251982, -91.50000000409677625 ) ) ;
#14868 = DIRECTION ( 'NONE',  ( 0.000000000000000000, 0.000000000000000000, -1.000000000000000000 ) ) ;
#14869 = CARTESIAN_POINT ( 'NONE',  ( -10.81189881249999907, -6.242252689847864744, -159.6562500020484094 ) ) ;
#14870 = CARTESIAN_POINT ( 'NONE',  ( 5.405949406249999534, 9.363379034771803333, -52.09375000204835260 ) ) ;
#14872 = EDGE_CURVE ( 'NONE', #22602, #23620, #12088, .T. ) ;
#14871 = VERTEX_POINT ( 'NONE', #34780 ) ;
#14873 = CARTESIAN_POINT ( 'NONE',  ( -9.999999999999998224, 1.224646799147353059E-15, -28.24999999999996803 ) ) ;
#14874 = CARTESIAN_POINT ( 'NONE',  ( -2.293366432827344421E-15, -12.48450537969573659, -24.40625000204838457 ) ) ;
#14875 = CARTESIAN_POINT ( 'NONE',  ( -9.999999999999998224, 1.224646799147353059E-15, -163.2500000000000000 ) ) ;
#14876 = CARTESIAN_POINT ( 'NONE',  ( 9.999999999999998224, 0.000000000000000000, -19.99999999999996092 ) ) ;
#14877 =( BOUNDED_CURVE ( )  B_SPLINE_CURVE ( 2, ( #32431, #19662, #2856, #6305, #32850, #42113, #6722 ),
 .UNSPECIFIED., .F., .F. ) 
 B_SPLINE_CURVE_WITH_KNOTS ( ( 3, 2, 2, 3 ),
 ( 0.1641791044776119424, 0.1654228855721392999, 0.1666666666666666574, 0.1679104477611940427 ),
 .UNSPECIFIED. ) 
 CURVE ( )  GEOMETRIC_REPRESENTATION_ITEM ( )  RATIONAL_B_SPLINE_CURVE ( ( 1.000000000000000000, 0.8660254037844387076, 1.000000000000000000, 0.8660254037844387076, 1.000000000000000000, 0.8660254037844387076, 1.000000000000000000 ) ) 
 REPRESENTATION_ITEM ( '' )  );
#14878 = CARTESIAN_POINT ( 'NONE',  ( 5.000000000000000000, 8.660254037844385522, -29.12500000409676204 ) ) ;
#14879 = AXIS2_PLACEMENT_3D ( 'NONE', #21281, #30796, #1231 ) ;
#14880 = CARTESIAN_POINT ( 'NONE',  ( 0.000000000000000000, 0.000000000000000000, -99.99999999999998579 ) ) ;
#14881 = CARTESIAN_POINT ( 'NONE',  ( 10.81189881249999907, 6.242252689847868297, -136.4062500020484094 ) ) ;
#14882 = CARTESIAN_POINT ( 'NONE',  ( 10.31059247562686210, 3.150086566999095616, 3.656666817559539767E-15 ) ) ;
#14883 = EDGE_CURVE ( 'NONE', #22659, #23066, #19598, .T. ) ;
#14884 = CARTESIAN_POINT ( 'NONE',  ( -2.121150477449813534E-15, -11.54700538379251284, -68.75000000409679046 ) ) ;
#14885 = ORIENTED_EDGE ( 'NONE', *, *, #23304, .F. ) ;
#14886 = CARTESIAN_POINT ( 'NONE',  ( -10.81189881249999729, 1.324075727343319199E-15, -62.28125000204837391 ) ) ;
#14887 = APPROVAL_STATUS ( 'not_yet_approved' ) ;
#14889 = VERTEX_POINT ( 'NONE', #42075 ) ;
#14888 = ORIENTED_EDGE ( 'NONE', *, *, #34117, .F. ) ;
#14890 = CARTESIAN_POINT ( 'NONE',  ( 10.00000000000051159, -5.773502691895965988, -120.6250000000000000 ) ) ;
#14891 = CARTESIAN_POINT ( 'NONE',  ( -9.999999999999998224, 1.224646799147353059E-15, -144.1250000040967905 ) ) ;
#14892 = CARTESIAN_POINT ( 'NONE',  ( 10.81189881249999907, 6.242252689847868297, -160.2187500020483810 ) ) ;
#14893 = CARTESIAN_POINT ( 'NONE',  ( 5.405949406249999534, 9.363379034771803333, -190.2812500020484094 ) ) ;
#14894 = CARTESIAN_POINT ( 'NONE',  ( 10.81189881249999907, 6.242252689847868297, -7.218750002048349934 ) ) ;
#14895 = CARTESIAN_POINT ( 'NONE',  ( -17.32050807568889539, 1.110223024625133663E-15, 49.99999999999998579 ) ) ;
#14896 = CARTESIAN_POINT ( 'NONE',  ( 7.644554776091147741E-16, 12.48450537969573659, -150.9687500020484094 ) ) ;
#14897 = CARTESIAN_POINT ( 'NONE',  ( 10.81189881249999551, -6.242252689847874514, -103.6562500020483668 ) ) ;
#14898 = CARTESIAN_POINT ( 'NONE',  ( 10.81189881249999907, 6.242252689847868297, -107.7187500020483810 ) ) ;
#14899 = CARTESIAN_POINT ( 'NONE',  ( 9.999999999999998224, 0.000000000000000000, -129.8750000040967905 ) ) ;
#14900 = CARTESIAN_POINT ( 'NONE',  ( -10.81189881249999729, 1.324075727343319199E-15, -117.7812500020483952 ) ) ;
#14901 = CARTESIAN_POINT ( 'NONE',  ( 7.644554776091147741E-16, 12.48450537969573659, -0.9687500020483524876 ) ) ;
#14902 = CARTESIAN_POINT ( 'NONE',  ( -10.81189881249999729, 1.324075727343319199E-15, -128.0937500020483810 ) ) ;
#14903 = CARTESIAN_POINT ( 'NONE',  ( 7.644554776091147741E-16, 12.48450537969573659, -193.1562500020484094 ) ) ;
#14904 = CARTESIAN_POINT ( 'NONE',  ( 9.999999999999996447, -5.773502691896262640, -147.6250000000000000 ) ) ;
#14905 = CARTESIAN_POINT ( 'NONE',  ( -5.000000000000003553, -8.660254037844383745, -12.99999999999995559 ) ) ;
#14906 = EDGE_CURVE ( 'NONE', #39524, #9909, #28457, .T. ) ;
#14907 = CARTESIAN_POINT ( 'NONE',  ( 10.81189881249999551, -6.242252689847874514, -79.46875000204836681 ) ) ;
#14908 = CARTESIAN_POINT ( 'NONE',  ( 10.81189881249999551, -6.242252689847874514, -59.96875000204837391 ) ) ;
#14909 = CARTESIAN_POINT ( 'NONE',  ( -5.000000000000003553, -8.660254037844383745, -190.3750000040967905 ) ) ;
#14910 = CARTESIAN_POINT ( 'NONE',  ( -5.405949406249996869, 9.363379034771805109, -32.53125000204837391 ) ) ;
#14911 = CARTESIAN_POINT ( 'NONE',  ( 5.405949406249992428, -9.363379034771808662, -36.09375000204836681 ) ) ;
#14912 = CARTESIAN_POINT ( 'NONE',  ( 0.000000000000000000, 0.000000000000000000, -200.0000000000000000 ) ) ;
#14913 = CARTESIAN_POINT ( 'NONE',  ( -2.293366432827344421E-15, -12.48450537969573659, -144.2187500020483810 ) ) ;
#14914 = CARTESIAN_POINT ( 'NONE',  ( 5.000000000000000000, 8.660254037844385522, -124.7500000000000000 ) ) ;
#14915 = DIRECTION ( 'NONE',  ( -0.000000000000000000, -0.000000000000000000, -1.000000000000000000 ) ) ;
#14916 = CARTESIAN_POINT ( 'NONE',  ( 10.00000000000000000, 5.773502691896255534, -75.37499999999998579 ) ) ;
#14917 = CARTESIAN_POINT ( 'NONE',  ( -2.293366432827344421E-15, -12.48450537969573659, -13.90625000204836503 ) ) ;
#14918 = ORIENTED_EDGE ( 'NONE', *, *, #40401, .T. ) ;
#14919 =( BOUNDED_CURVE ( )  B_SPLINE_CURVE ( 2, ( #32812, #35840, #39484, #23307, #13352, #16161, #35633 ),
 .UNSPECIFIED., .F., .F. ) 
 B_SPLINE_CURVE_WITH_KNOTS ( ( 3, 2, 2, 3 ),
 ( 0.4104477611940299253, 0.4116915422885572551, 0.4129353233830846959, 0.4141791044776120256 ),
 .UNSPECIFIED. ) 
 CURVE ( )  GEOMETRIC_REPRESENTATION_ITEM ( )  RATIONAL_B_SPLINE_CURVE ( ( 0.9999999999999940048, 0.8660254037844447028, 1.000000000000000000, 0.8660254037844387076, 1.000000000000000000, 0.8660254037844267172, 1.000000000000011990 ) ) 
 REPRESENTATION_ITEM ( '' )  );
#14920 = CARTESIAN_POINT ( 'NONE',  ( -2.121150477449813534E-15, -11.54700538379251284, -164.3749999999999716 ) ) ;
#14921 = CARTESIAN_POINT ( 'NONE',  ( -10.00000000000000000, -5.773502691896251982, -121.5000000040967905 ) ) ;
#14922 = CARTESIAN_POINT ( 'NONE',  ( 10.00000000000102318, -5.773502691895667560, -56.50000000409674783 ) ) ;
#14923 = CARTESIAN_POINT ( 'NONE',  ( -5.405949406249996869, 9.363379034771805109, -75.84375000204838102 ) ) ;
#14924 = CARTESIAN_POINT ( 'NONE',  ( 10.00000000000000000, 5.773502691896255534, -36.75000000409675494 ) ) ;
#14925 = CARTESIAN_POINT ( 'NONE',  ( 0.000000000000000000, 0.000000000000000000, -200.0000000000000000 ) ) ;
#14926 = CARTESIAN_POINT ( 'NONE',  ( 5.405949406249999534, 9.363379034771803333, -41.78125000204838102 ) ) ;
#14927 =( BOUNDED_CURVE ( )  B_SPLINE_CURVE ( 2, ( #224, #13346, #23299, #36457, #6891, #16793, #29993 ),
 .UNSPECIFIED., .F., .F. ) 
 B_SPLINE_CURVE_WITH_KNOTS ( ( 3, 2, 2, 3 ),
 ( 0.4365671641791046276, 0.4378109452736320129, 0.4390547263681593981, 0.4402985074626867279 ),
 .UNSPECIFIED. ) 
 CURVE ( )  GEOMETRIC_REPRESENTATION_ITEM ( )  RATIONAL_B_SPLINE_CURVE ( ( 0.9999999999999820144, 0.8660254037844566932, 1.000000000000000000, 0.8660254037844387076, 1.000000000000000000, 0.8660254037844207220, 1.000000000000017986 ) ) 
 REPRESENTATION_ITEM ( '' )  );
#14928 = CARTESIAN_POINT ( 'NONE',  ( 10.00000000000051159, -5.773502691895965988, -99.62499999999997158 ) ) ;
#14929 = CARTESIAN_POINT ( 'NONE',  ( -5.405949406250003975, -9.363379034771801557, -149.0312500020483810 ) ) ;
#14930 = CARTESIAN_POINT ( 'NONE',  ( -10.81189881249999729, 6.242252689847871849, -129.7187500020483810 ) ) ;
#14931 = CARTESIAN_POINT ( 'NONE',  ( -9.999999999999998224, 1.224646799147353059E-15, -3.125000004096767370 ) ) ;
#14932 = CARTESIAN_POINT ( 'NONE',  ( -2.121150477449813534E-15, -11.54700538379251284, -120.8749999999999858 ) ) ;
#14933 = ORIENTED_EDGE ( 'NONE', *, *, #15138, .F. ) ;
#14934 = CC_DESIGN_SECURITY_CLASSIFICATION ( #25992, ( #42696 ) ) ;
#14935 = EDGE_LOOP ( 'NONE', ( #23547, #29452, #16609, #37237 ) ) ;
#14936 = ORIENTED_EDGE ( 'NONE', *, *, #1835, .F. ) ;
#14937 = CARTESIAN_POINT ( 'NONE',  ( -9.999999999999998224, 1.224646799147353059E-15, -145.6250000040967905 ) ) ;
#14938 = CARTESIAN_POINT ( 'NONE',  ( -10.81189881249999729, 6.242252689847871849, -182.2187500020484379 ) ) ;
#14939 = CARTESIAN_POINT ( 'NONE',  ( -5.405949406249996869, 9.363379034771805109, -39.84375000204837391 ) ) ;
#14940 = CARTESIAN_POINT ( 'NONE',  ( 9.999999999999998224, 0.000000000000000000, -108.4999999999999858 ) ) ;
#14941 = CARTESIAN_POINT ( 'NONE',  ( -10.81189881249999729, -6.242252689847864744, -172.9687500020483526 ) ) ;
#14942 = CARTESIAN_POINT ( 'NONE',  ( -10.81189881249999729, 1.324075727343319199E-15, -156.5937500020483810 ) ) ;
#14943 = CARTESIAN_POINT ( 'NONE',  ( 4.999999999999992006, -8.660254037844389075, -122.6250000040967905 ) ) ;
#14944 = CARTESIAN_POINT ( 'NONE',  ( -10.81189881249999729, 1.324075727343319199E-15, -134.0937500020483810 ) ) ;
#14945 = CARTESIAN_POINT ( 'NONE',  ( 10.81189881249999551, -6.242252689847874514, -141.1562500020484094 ) ) ;
#14946 = CARTESIAN_POINT ( 'NONE',  ( 10.81189881249999551, -6.242252689847874514, -154.4687500020484094 ) ) ;
#14947 = CARTESIAN_POINT ( 'NONE',  ( -2.121150477449813534E-15, -11.54700538379251284, -152.3749999999999716 ) ) ;
#14948 = CARTESIAN_POINT ( 'NONE',  ( -9.999999999999998224, 1.224646799147353059E-15, -169.2500000000000000 ) ) ;
#14949 = CARTESIAN_POINT ( 'NONE',  ( 9.999999999999998224, 0.000000000000000000, -168.5000000000000000 ) ) ;
#14950 = ADVANCED_FACE ( 'NONE', ( #15102 ), #28089, .F. ) ;
#14951 = CARTESIAN_POINT ( 'NONE',  ( -5.405949406250003975, -9.363379034771801557, -84.34375000204836681 ) ) ;
#14952 = CARTESIAN_POINT ( 'NONE',  ( -9.999999999999998224, 1.224646799147353059E-15, -136.2499999999999716 ) ) ;
#14953 = CARTESIAN_POINT ( 'NONE',  ( -10.81189881249999729, 1.324075727343319199E-15, -62.28125000204837391 ) ) ;
#14954 = DIRECTION ( 'NONE',  ( -0.000000000000000000, -0.000000000000000000, 1.000000000000000000 ) ) ;
#14955 = CARTESIAN_POINT ( 'NONE',  ( 10.81189881249999729, 0.000000000000000000, -167.8437500020484094 ) ) ;
#14956 = CARTESIAN_POINT ( 'NONE',  ( -5.405949406249996869, 9.363379034771805109, -110.5312500020483810 ) ) ;
#14957 = CARTESIAN_POINT ( 'NONE',  ( 10.81189881249999729, 0.000000000000000000, -156.0312500020484094 ) ) ;
#14958 = DIRECTION ( 'NONE',  ( 0.5000000000000007772, -0.8660254037844381525, -0.000000000000000000 ) ) ;
#14959 = CARTESIAN_POINT ( 'NONE',  ( -10.81189881249999729, 1.324075727343319199E-15, -42.78125000204838102 ) ) ;
#14960 = CARTESIAN_POINT ( 'NONE',  ( 9.999999999999996447, -5.773502691896262640, -131.5000000040967905 ) ) ;
#14961 = CARTESIAN_POINT ( 'NONE',  ( -5.000000000000003553, -8.660254037844383745, -98.49999999999998579 ) ) ;
#14962 = ORIENTED_EDGE ( 'NONE', *, *, #8533, .T. ) ;
#14963 = CARTESIAN_POINT ( 'NONE',  ( 10.81189881249999551, -6.242252689847874514, -129.1562500020483810 ) ) ;
#14964 = CARTESIAN_POINT ( 'NONE',  ( 5.000000000000000000, 8.660254037844385522, -150.6250000040967905 ) ) ;
#14965 = CYLINDRICAL_SURFACE ( 'NONE', #3622, 9.999999999999998224 ) ;
#14966 = CARTESIAN_POINT ( 'NONE',  ( -10.81189881249999729, 1.324075727343319199E-15, -177.7812500020484094 ) ) ;
#14967 = EDGE_LOOP ( 'NONE', ( #1528, #12908, #41541, #29064 ) ) ;
#14968 = CARTESIAN_POINT ( 'NONE',  ( -5.405949406250003975, -9.363379034771801557, -171.3437500020484094 ) ) ;
#14969 = CARTESIAN_POINT ( 'NONE',  ( -4.999999999999996447, 8.660254037844387298, -58.87500000409676204 ) ) ;
#14970 = CARTESIAN_POINT ( 'NONE',  ( 0.000000000000000000, 0.000000000000000000, -200.0000000000000000 ) ) ;
#14971 = CARTESIAN_POINT ( 'NONE',  ( -4.999999999999996447, 8.660254037844387298, -130.5000000000000000 ) ) ;
#14972 = CARTESIAN_POINT ( 'NONE',  ( 10.81189881249999551, -6.242252689847874514, -67.65625000204838102 ) ) ;
#14973 = EDGE_CURVE ( 'NONE', #15207, #28849, #37506, .T. ) ;
#14974 = CARTESIAN_POINT ( 'NONE',  ( -10.00000000000000000, -5.773502691896251982, -40.50000000409675494 ) ) ;
#14975 = CARTESIAN_POINT ( 'NONE',  ( -10.81189881249999907, -6.242252689847864744, -1.968750002048352599 ) ) ;
#14976 = CARTESIAN_POINT ( 'NONE',  ( 7.070501591499376803E-16, 11.54700538379251284, -147.5000000040967905 ) ) ;
#14977 = CARTESIAN_POINT ( 'NONE',  ( -2.293366432827344421E-15, -12.48450537969573659, -165.4062500020483810 ) ) ;
#14978 = VECTOR ( 'NONE', #30062, 1000.000000000000000 ) ;
#14979 = FACE_OUTER_BOUND ( 'NONE', #38107, .T. ) ;
#14980 = CARTESIAN_POINT ( 'NONE',  ( -9.999999999999479527, -5.773502691896549521, -82.12499999999997158 ) ) ;
#14981 = VERTEX_POINT ( 'NONE', #29784 ) ;
#14982 = LINE ( 'NONE', #31211, #5645 ) ;
#14983 = CARTESIAN_POINT ( 'NONE',  ( 4.999999999999992006, -8.660254037844389075, -153.7500000000000000 ) ) ;
#14984 = CARTESIAN_POINT ( 'NONE',  ( 5.000000000000000000, 8.660254037844385522, -195.6250000040967905 ) ) ;
#14986 = EDGE_LOOP ( 'NONE', ( #29593, #5684, #30939, #23031 ) ) ;
#14985 = CARTESIAN_POINT ( 'NONE',  ( -5.405949406249996869, 9.363379034771805109, -77.53125000204838102 ) ) ;
#14987 = CARTESIAN_POINT ( 'NONE',  ( 0.000000000000000000, 0.000000000000000000, 0.000000000000000000 ) ) ;
#14989 = VERTEX_POINT ( 'NONE', #39478 ) ;
#14988 = CARTESIAN_POINT ( 'NONE',  ( 4.999999999999992006, -8.660254037844389075, -69.74999999999997158 ) ) ;
#14990 =( BOUNDED_CURVE ( )  B_SPLINE_CURVE ( 2, ( #6916, #3690, #12942, #39079, #13370, #22688, #32625 ),
 .UNSPECIFIED., .F., .F. ) 
 B_SPLINE_CURVE_WITH_KNOTS ( ( 3, 2, 2, 3 ),
 ( 0.4402985074626867279, 0.4415422885572141132, 0.4427860696517414429, 0.4440298507462688282 ),
 .UNSPECIFIED. ) 
 CURVE ( )  GEOMETRIC_REPRESENTATION_ITEM ( )  RATIONAL_B_SPLINE_CURVE ( ( 0.9999999999999820144, 0.8660254037844566932, 1.000000000000000000, 0.8660254037844387076, 1.000000000000000000, 0.8660254037844207220, 1.000000000000017986 ) ) 
 REPRESENTATION_ITEM ( '' )  );
#14991 = ORIENTED_EDGE ( 'NONE', *, *, #5559, .T. ) ;
#14992 = CARTESIAN_POINT ( 'NONE',  ( -5.405949406250003975, -9.363379034771801557, -37.84375000204837391 ) ) ;
#14993 = CARTESIAN_POINT ( 'NONE',  ( -10.81189881249999907, -6.242252689847864744, -3.656250002048349046 ) ) ;
#14995 = ORIENTED_EDGE ( 'NONE', *, *, #20645, .F. ) ;
#14994 = CARTESIAN_POINT ( 'NONE',  ( 7.644554776091147741E-16, 12.48450537969573659, -59.46875000204837391 ) ) ;
#14996 = CARTESIAN_POINT ( 'NONE',  ( 7.070501591499376803E-16, 11.54700538379251284, -112.6249999999999858 ) ) ;
#14997 = ADVANCED_FACE ( 'NONE', ( #39687 ), #20045, .T. ) ;
#14998 = CARTESIAN_POINT ( 'NONE',  ( 4.999999999999992006, -8.660254037844389075, -36.74999999999997868 ) ) ;
#14999 = CARTESIAN_POINT ( 'NONE',  ( -2.293366432827344421E-15, -12.48450537969573659, -178.7187500020484094 ) ) ;
#15000 = CARTESIAN_POINT ( 'NONE',  ( -5.405949406250003975, -9.363379034771801557, -163.8437500020484094 ) ) ;
#15002 = EDGE_CURVE ( 'NONE', #30921, #20035, #13779, .T. ) ;
#15001 = CARTESIAN_POINT ( 'NONE',  ( 9.999999999999998224, 0.000000000000000000, -200.0000000000000000 ) ) ;
#15003 = DIRECTION ( 'NONE',  ( 1.000000000000000000, 0.000000000000000000, 0.000000000000000000 ) ) ;
#15004 = CARTESIAN_POINT ( 'NONE',  ( -5.000000000000003553, -8.660254037844383745, -191.8750000040967905 ) ) ;
#15005 = CARTESIAN_POINT ( 'NONE',  ( 5.000000000000000000, 8.660254037844385522, -192.2500000000000000 ) ) ;
#15006 = CARTESIAN_POINT ( 'NONE',  ( -10.81189881249999729, 1.324075727343319199E-15, -104.0937500020483810 ) ) ;
#15007 = DIRECTION ( 'NONE',  ( 0.000000000000000000, 0.000000000000000000, 1.000000000000000000 ) ) ;
#15008 = CARTESIAN_POINT ( 'NONE',  ( 10.81189881249999551, -6.242252689847874514, -85.65625000204838102 ) ) ;
#15009 = CARTESIAN_POINT ( 'NONE',  ( -2.293366432827344421E-15, -12.48450537969573659, -91.71875000204838102 ) ) ;
#15010 = VECTOR ( 'NONE', #8400, 1000.000000000000000 ) ;
#15011 = CARTESIAN_POINT ( 'NONE',  ( -5.405949406249996869, 9.363379034771805109, -65.53125000204838102 ) ) ;
#15012 = CARTESIAN_POINT ( 'NONE',  ( 9.999999999999998224, 0.000000000000000000, -153.8750000040967905 ) ) ;
#15013 = CARTESIAN_POINT ( 'NONE',  ( -9.999999999999998224, 5.773502691896259087, -127.3750000000000000 ) ) ;
#15014 = CARTESIAN_POINT ( 'NONE',  ( 10.81189881249999729, 6.242252689847867408, -146.9062500020484379 ) ) ;
#15015 = CARTESIAN_POINT ( 'NONE',  ( 10.81189881249999551, -6.242252689847874514, -163.6562500020484094 ) ) ;
#15016 = DIRECTION ( 'NONE',  ( -1.000000000000000000, -4.506943796211477094E-16, 0.000000000000000000 ) ) ;
#15017 = CARTESIAN_POINT ( 'NONE',  ( -9.999999999999612754, -5.773502691896474914, -182.6249999999999716 ) ) ;
#15018 = CARTESIAN_POINT ( 'NONE',  ( -10.81189881249999729, 1.324075727343319199E-15, -101.0937500020483810 ) ) ;
#15019 = ORIENTED_EDGE ( 'NONE', *, *, #37085, .F. ) ;
#15020 = CARTESIAN_POINT ( 'NONE',  ( 9.999999999999996447, -5.773502691896262640, -66.62499999999998579 ) ) ;
#15021 = CARTESIAN_POINT ( 'NONE',  ( 10.81189881249999729, 0.000000000000000000, -199.3437500020484094 ) ) ;
#15022 = CARTESIAN_POINT ( 'NONE',  ( -4.999999999999996447, 8.660254037844387298, -85.87500000409677625 ) ) ;
#15023 = CARTESIAN_POINT ( 'NONE',  ( 1.257163379650654722, -10.41811935602516392, -180.0000000000000568 ) ) ;
#15024 = CARTESIAN_POINT ( 'NONE',  ( -5.405949406250003975, -9.363379034771801557, -89.03125000204838102 ) ) ;
#15025 = CARTESIAN_POINT ( 'NONE',  ( 5.405949406249999534, 9.363379034771803333, -73.28125000204838102 ) ) ;
#15026 = CARTESIAN_POINT ( 'NONE',  ( 5.000000000000000000, 8.660254037844385522, -68.12500000409677625 ) ) ;
#15027 = LINE ( 'NONE', #38142, #5723 ) ;
#15028 = CARTESIAN_POINT ( 'NONE',  ( 5.405949406249992428, -9.363379034771808662, -24.09375000204835970 ) ) ;
#15029 = VERTEX_POINT ( 'NONE', #23301 ) ;
#15030 = CARTESIAN_POINT ( 'NONE',  ( -9.999999999999998224, 5.773502691896259087, -4.374999999999956479 ) ) ;
#15031 = CARTESIAN_POINT ( 'NONE',  ( -10.81189881249999907, -6.242252689847864744, -21.65625000204838102 ) ) ;
#15032 = ADVANCED_FACE ( 'NONE', ( #13130 ), #33016, .T. ) ;
#15033 = CARTESIAN_POINT ( 'NONE',  ( -10.81189881249999729, 6.242252689847871849, -2.218750002048358372 ) ) ;
#15034 = CARTESIAN_POINT ( 'NONE',  ( -60.00000000000000711, 7.347880794884119933E-15, -240.0000000000000000 ) ) ;
#15035 = CARTESIAN_POINT ( 'NONE',  ( 5.405949406249992428, -9.363379034771808662, -142.5937500020483810 ) ) ;
#15036 = CARTESIAN_POINT ( 'NONE',  ( 9.999999999999998224, 0.000000000000000000, -107.3750000040967763 ) ) ;
#15037 = CARTESIAN_POINT ( 'NONE',  ( 5.000000000000000000, 8.660254037844385522, -152.1250000040967905 ) ) ;
#15038 =( BOUNDED_CURVE ( )  B_SPLINE_CURVE ( 2, ( #36727, #7166, #10813, #33512, #17073, #13829, #7594 ),
 .UNSPECIFIED., .F., .F. ) 
 B_SPLINE_CURVE_WITH_KNOTS ( ( 3, 2, 2, 3 ),
 ( 0.6716417910447763928, 0.6728855721393036671, 0.6741293532338310523, 0.6753731343283584376 ),
 .UNSPECIFIED. ) 
 CURVE ( )  GEOMETRIC_REPRESENTATION_ITEM ( )  RATIONAL_B_SPLINE_CURVE ( ( 0.9999999999999761302, 0.8660254037844625774, 1.000000000000000000, 0.8660254037844387076, 1.000000000000000000, 0.8660254037844148378, 1.000000000000023981 ) ) 
 REPRESENTATION_ITEM ( '' )  );
#15039 = CARTESIAN_POINT ( 'NONE',  ( -9.999999999999998224, 5.773502691896259087, -182.8750000000000000 ) ) ;
#15040 = CARTESIAN_POINT ( 'NONE',  ( 0.000000000000000000, 0.000000000000000000, -223.0000000000000000 ) ) ;
#15042 = VERTEX_POINT ( 'NONE', #36667 ) ;
#15041 = CARTESIAN_POINT ( 'NONE',  ( -10.81189881249999907, -6.242252689847864744, -98.15625000204839523 ) ) ;
#15043 = DIRECTION ( 'NONE',  ( -0.000000000000000000, -0.000000000000000000, 1.000000000000000000 ) ) ;
#15044 = AXIS2_PLACEMENT_3D ( 'NONE', #3346, #20365, #23413 ) ;
#15045 = VERTEX_POINT ( 'NONE', #12917 ) ;
#15046 = ORIENTED_EDGE ( 'NONE', *, *, #24107, .T. ) ;
#15047 = CARTESIAN_POINT ( 'NONE',  ( -10.81189881249999729, 6.242252689847871849, -41.40625000204836681 ) ) ;
#15048 = COORDINATED_UNIVERSAL_TIME_OFFSET ( 6, 0, .AHEAD. ) ;
#15049 = CARTESIAN_POINT ( 'NONE',  ( 5.405949406249999534, 9.363379034771803333, -83.59375000204836681 ) ) ;
#15050 = CARTESIAN_POINT ( 'NONE',  ( 0.000000000000000000, 0.000000000000000000, -200.0000000000000000 ) ) ;
#15051 = CARTESIAN_POINT ( 'NONE',  ( 8.850157141833594920, 5.572544619961112389, -99.99999999999998579 ) ) ;
#15052 = CARTESIAN_POINT ( 'NONE',  ( -99.99999999999994316, -20.00000000000000355, -160.0000000000000000 ) ) ;
#15053 = CARTESIAN_POINT ( 'NONE',  ( -5.405949406249996869, 9.363379034771805109, -163.0312500020484094 ) ) ;
#15054 = CARTESIAN_POINT ( 'NONE',  ( 10.00000000000051159, -5.773502691895965988, -77.12499999999997158 ) ) ;
#15055 = CARTESIAN_POINT ( 'NONE',  ( 10.81189881249999551, -6.242252689847874514, -115.4687500020483810 ) ) ;
#15056 = CARTESIAN_POINT ( 'NONE',  ( -5.405949406249996869, 9.363379034771805109, -84.84375000204836681 ) ) ;
#15057 = CARTESIAN_POINT ( 'NONE',  ( 5.405949406249999534, 9.363379034771803333, -1.281250002048373027 ) ) ;
#15058 = CARTESIAN_POINT ( 'NONE',  ( -10.81189881249999729, 6.242252689847871849, -191.2187500020484663 ) ) ;
#15059 = CARTESIAN_POINT ( 'NONE',  ( -10.81189881249999729, 1.324075727343319199E-15, -93.78125000204838102 ) ) ;
#15060 = CARTESIAN_POINT ( 'NONE',  ( 10.00000000000000000, 5.773502691896255534, -174.7500000040968189 ) ) ;
#15061 = CARTESIAN_POINT ( 'NONE',  ( 5.405949406249992428, -9.363379034771808662, -166.7812500020484094 ) ) ;
#15062 = CARTESIAN_POINT ( 'NONE',  ( 7.644554776091147741E-16, 12.48450537969573659, -175.1562500020484094 ) ) ;
#15063 = CARTESIAN_POINT ( 'NONE',  ( -5.405949406249996869, 9.363379034771805109, -191.5312500020484094 ) ) ;
#15064 = CARTESIAN_POINT ( 'NONE',  ( 5.405949406249999534, 9.363379034771803333, -44.59375000204837391 ) ) ;
#15065 = CARTESIAN_POINT ( 'NONE',  ( 9.999999999999998224, 0.000000000000000000, -164.3750000040967905 ) ) ;
#15066 = CARTESIAN_POINT ( 'NONE',  ( 7.644554776091147741E-16, 12.48450537969573659, -5.656250002048358816 ) ) ;
#15067 = CARTESIAN_POINT ( 'NONE',  ( -10.81189881249999729, 6.242252689847871849, -15.71875000204836503 ) ) ;
#15068 = CARTESIAN_POINT ( 'NONE',  ( -10.81189881249999907, -6.242252689847864744, -121.9687500020483952 ) ) ;
#15069 = CARTESIAN_POINT ( 'NONE',  ( -4.999999999999996447, 8.660254037844387298, -88.49999999999998579 ) ) ;
#15070 = CARTESIAN_POINT ( 'NONE',  ( -10.81189881249999729, 1.324075727343319199E-15, -17.28125000204835970 ) ) ;
#15071 = CARTESIAN_POINT ( 'NONE',  ( -9.999999999999998224, 1.224646799147353059E-15, -102.1250000040967905 ) ) ;
#15072 = AXIS2_PLACEMENT_3D ( 'NONE', #12677, #35384, #18962 ) ;
#15073 = CARTESIAN_POINT ( 'NONE',  ( -10.00000000000051337, 5.773502691895962435, -82.37499999999997158 ) ) ;
#15074 = CARTESIAN_POINT ( 'NONE',  ( 9.999999999999998224, 0.000000000000000000, -49.99999999999998579 ) ) ;
#15075 = CARTESIAN_POINT ( 'NONE',  ( 5.405949406249992428, -9.363379034771808662, -120.2812500020483952 ) ) ;
#15076 = CARTESIAN_POINT ( 'NONE',  ( 5.405949406249999534, 9.363379034771803333, -103.2812500020483952 ) ) ;
#15077 = VERTEX_POINT ( 'NONE', #10330 ) ;
#15078 = CARTESIAN_POINT ( 'NONE',  ( 5.000000000000000000, 8.660254037844385522, -89.12500000409677625 ) ) ;
#15079 = DIRECTION ( 'NONE',  ( -0.000000000000000000, -0.000000000000000000, 1.000000000000000000 ) ) ;
#15080 = CARTESIAN_POINT ( 'NONE',  ( -5.405949406250003975, -9.363379034771801557, -159.5312500020484094 ) ) ;
#15081 = CARTESIAN_POINT ( 'NONE',  ( 10.81189881249999729, 0.000000000000000000, -50.84375000204835260 ) ) ;
#15082 = EDGE_LOOP ( 'NONE', ( #882, #34327, #4230, #25792 ) ) ;
#15083 = CARTESIAN_POINT ( 'NONE',  ( -4.999999999999996447, 8.660254037844387298, -23.99999999999996447 ) ) ;
#15084 = EDGE_CURVE ( 'NONE', #3910, #34292, #41906, .T. ) ;
#15085 = AXIS2_PLACEMENT_3D ( 'NONE', #30176, #11146, #14370 ) ;
#15086 = EDGE_CURVE ( 'NONE', #23116, #40511, #32854, .T. ) ;
#15087 = CARTESIAN_POINT ( 'NONE',  ( 7.644554776091147741E-16, 12.48450537969573659, -29.65625000204835970 ) ) ;
#15088 = CARTESIAN_POINT ( 'NONE',  ( 10.00000000000000000, 5.773502691896255534, -159.3750000000000000 ) ) ;
#15089 = CARTESIAN_POINT ( 'NONE',  ( 4.999999999999992006, -8.660254037844389075, -23.62500000409675849 ) ) ;
#15090 = EDGE_CURVE ( 'NONE', #30784, #15995, #19413, .T. ) ;
#15091 = DIRECTION ( 'NONE',  ( 1.000000000000000000, 0.000000000000000000, 0.000000000000000000 ) ) ;
#15092 = CARTESIAN_POINT ( 'NONE',  ( 10.81189881249999551, -6.242252689847874514, -132.1562500020484094 ) ) ;
#15093 = CARTESIAN_POINT ( 'NONE',  ( -10.00000000000051337, 5.773502691895962435, -46.37499999999995026 ) ) ;
#15094 = CARTESIAN_POINT ( 'NONE',  ( 9.999999999999998224, 0.000000000000000000, -135.5000000000000000 ) ) ;
#15095 = VERTEX_POINT ( 'NONE', #19619 ) ;
#15096 = CARTESIAN_POINT ( 'NONE',  ( 10.81189881249999907, 6.242252689847868297, -62.90625000204838813 ) ) ;
#15097 = APPROVAL_STATUS ( 'not_yet_approved' ) ;
#15099 = ORIENTED_EDGE ( 'NONE', *, *, #6940, .F. ) ;
#15098 = EDGE_LOOP ( 'NONE', ( #2798, #11591, #39506, #13159 ) ) ;
#15100 = EDGE_CURVE ( 'NONE', #5147, #25998, #35970, .T. ) ;
#15101 = DIRECTION ( 'NONE',  ( 0.000000000000000000, -1.000000000000000000, 0.000000000000000000 ) ) ;
#15102 = FACE_OUTER_BOUND ( 'NONE', #40675, .T. ) ;
#15103 = CARTESIAN_POINT ( 'NONE',  ( 5.405949406249992428, -9.363379034771808662, -154.5937500020483810 ) ) ;
#15104 = CARTESIAN_POINT ( 'NONE',  ( 10.81189881249999551, -6.242252689847874514, -189.1562500020484379 ) ) ;
#15105 = CARTESIAN_POINT ( 'NONE',  ( -2.293366432827344421E-15, -12.48450537969573659, -9.218750002048359704 ) ) ;
#15106 = AXIS2_PLACEMENT_3D ( 'NONE', #8955, #22118, #35293 ) ;
#15107 = EDGE_CURVE ( 'NONE', #10156, #36017, #22385, .T. ) ;
#15108 = CARTESIAN_POINT ( 'NONE',  ( 10.81189881249999729, 0.000000000000000000, -137.8437500020484094 ) ) ;
#15109 = CARTESIAN_POINT ( 'NONE',  ( 5.405949406249999534, 9.363379034771803333, -98.78125000204839523 ) ) ;
#15110 = CARTESIAN_POINT ( 'NONE',  ( -10.81189881249999907, -6.242252689847864744, -111.4687500020483810 ) ) ;
#15111 = CARTESIAN_POINT ( 'NONE',  ( 9.999999999999742428, 5.773502691896404748, -187.8750000000000000 ) ) ;
#15112 = CARTESIAN_POINT ( 'NONE',  ( 10.81189881249999907, 6.242252689847868297, -119.9062500020483810 ) ) ;
#15113 = CARTESIAN_POINT ( 'NONE',  ( -10.81189881249999729, 6.242252689847871849, -0.7187500020483512664 ) ) ;
#15114 = CARTESIAN_POINT ( 'NONE',  ( -5.405949406249996869, 9.363379034771805109, -123.8437500020483952 ) ) ;
#15115 = CARTESIAN_POINT ( 'NONE',  ( -2.293366432827344421E-15, -12.48450537969573659, -190.9062500020484094 ) ) ;
#15116 = CARTESIAN_POINT ( 'NONE',  ( 5.000000000000000000, 8.660254037844385522, -179.1250000040968189 ) ) ;
#15117 = CARTESIAN_POINT ( 'NONE',  ( -2.121150477449813534E-15, -11.54700538379251284, -144.8750000000000000 ) ) ;
#15118 = CARTESIAN_POINT ( 'NONE',  ( 5.000000000000000000, 8.660254037844385522, -9.249999999999952038 ) ) ;
#15119 = CARTESIAN_POINT ( 'NONE',  ( -10.81189881249999729, -6.242252689847864744, -76.96875000204838102 ) ) ;
#15120 = CARTESIAN_POINT ( 'NONE',  ( -10.81189881249999907, -6.242252689847864744, -55.96875000204836681 ) ) ;
#15121 = CARTESIAN_POINT ( 'NONE',  ( -4.999999999999996447, 8.660254037844387298, -187.8750000040967905 ) ) ;
#15122 = CARTESIAN_POINT ( 'NONE',  ( 10.81189881249999551, -6.242252689847874514, -22.65625000204837391 ) ) ;
#15123 = CARTESIAN_POINT ( 'NONE',  ( -10.81189881249999907, -6.242252689847864744, -37.96875000204835970 ) ) ;
#15124 = CARTESIAN_POINT ( 'NONE',  ( 7.070501591499376803E-16, 11.54700538379251284, -136.6250000000000000 ) ) ;
#15125 = CARTESIAN_POINT ( 'NONE',  ( -5.405949406249996869, 9.363379034771805109, -149.3437500020483810 ) ) ;
#15126 = CARTESIAN_POINT ( 'NONE',  ( -5.000000000000003553, -8.660254037844383745, -124.0000000000000000 ) ) ;
#15127 =( BOUNDED_CURVE ( )  B_SPLINE_CURVE ( 2, ( #12176, #31637, #11751, #38514, #2070, #9163, #5934 ),
 .UNSPECIFIED., .F., .F. ) 
 B_SPLINE_CURVE_WITH_KNOTS ( ( 3, 2, 2, 3 ),
 ( 0.3731343283582090331, 0.3743781094527363629, 0.3756218905472638037, 0.3768656716417911334 ),
 .UNSPECIFIED. ) 
 CURVE ( )  GEOMETRIC_REPRESENTATION_ITEM ( )  RATIONAL_B_SPLINE_CURVE ( ( 0.9999999999999940048, 0.8660254037844447028, 1.000000000000000000, 0.8660254037844387076, 1.000000000000000000, 0.8660254037844267172, 1.000000000000011990 ) ) 
 REPRESENTATION_ITEM ( '' )  );
#15128 = CARTESIAN_POINT ( 'NONE',  ( 9.999999999999998224, 0.000000000000000000, -137.0000000000000000 ) ) ;
#15129 = CARTESIAN_POINT ( 'NONE',  ( -10.00000000000000000, -5.773502691896251982, -73.12499999999995737 ) ) ;
#15130 = CARTESIAN_POINT ( 'NONE',  ( 10.81189881249999729, 0.000000000000000000, -138.0312500020484094 ) ) ;
#15131 = CARTESIAN_POINT ( 'NONE',  ( -10.81189881249999729, 6.242252689847871849, -11.40625000204835438 ) ) ;
#15132 = ORIENTED_EDGE ( 'NONE', *, *, #32636, .T. ) ;
#15133 = CARTESIAN_POINT ( 'NONE',  ( -5.405949406249996869, 9.363379034771805109, -101.5312500020483952 ) ) ;
#15134 = CARTESIAN_POINT ( 'NONE',  ( 9.999999999999996447, -5.773502691896262640, -113.5000000040967763 ) ) ;
#15135 = DIRECTION ( 'NONE',  ( -0.000000000000000000, -0.000000000000000000, 1.000000000000000000 ) ) ;
#15136 = CARTESIAN_POINT ( 'NONE',  ( 10.81189881249999729, 0.000000000000000000, -77.84375000204838102 ) ) ;
#15137 = CARTESIAN_POINT ( 'NONE',  ( -4.999999999999996447, 8.660254037844387298, -27.37500000409676204 ) ) ;
#15138 = EDGE_CURVE ( 'NONE', #31616, #41954, #17324, .T. ) ;
#15139 = CARTESIAN_POINT ( 'NONE',  ( 7.070501591499376803E-16, 11.54700538379251284, -75.12499999999997158 ) ) ;
#15140 = CARTESIAN_POINT ( 'NONE',  ( -10.81189881249999907, -6.242252689847864744, -45.65625000204837391 ) ) ;
#15141 = ADVANCED_FACE ( 'NONE', ( #1061 ), #34887, .T. ) ;
#15142 = CARTESIAN_POINT ( 'NONE',  ( -79.99999999999992895, 39.99999999999999289, -160.0000000000000000 ) ) ;
#15143 = CARTESIAN_POINT ( 'NONE',  ( 5.405949406249999534, 9.363379034771803333, -142.2812500020483810 ) ) ;
#15144 = AXIS2_PLACEMENT_3D ( 'NONE', #161, #39619, #40455 ) ;
#15145 = EDGE_CURVE ( 'NONE', #34431, #18400, #3612, .T. ) ;
#15146 = CARTESIAN_POINT ( 'NONE',  ( 10.81189881249999729, 0.000000000000000000, -127.3437500020483952 ) ) ;
#15147 = CARTESIAN_POINT ( 'NONE',  ( 5.000000000000000000, 8.660254037844385522, -78.62500000409677625 ) ) ;
#15148 = DIRECTION ( 'NONE',  ( -0.000000000000000000, -0.000000000000000000, -1.000000000000000000 ) ) ;
#15149 = ORIENTED_EDGE ( 'NONE', *, *, #42029, .F. ) ;
#15150 = ORIENTED_EDGE ( 'NONE', *, *, #42537, .T. ) ;
#15151 = ORIENTED_EDGE ( 'NONE', *, *, #23539, .T. ) ;
#15152 = EDGE_CURVE ( 'NONE', #33065, #34698, #40009, .T. ) ;
#15153 = DIRECTION ( 'NONE',  ( -0.000000000000000000, -0.000000000000000000, 1.000000000000000000 ) ) ;
#15154 = CARTESIAN_POINT ( 'NONE',  ( -2.293366432827344421E-15, -12.48450537969573659, -180.2187500020484094 ) ) ;
#15155 = CARTESIAN_POINT ( 'NONE',  ( -5.405949406249996869, 9.363379034771805109, -30.84375000204836326 ) ) ;
#15156 = CARTESIAN_POINT ( 'NONE',  ( -9.999999999999998224, 1.224646799147353059E-15, -60.12500000409676204 ) ) ;
#15157 = CARTESIAN_POINT ( 'NONE',  ( 5.405949406249992428, -9.363379034771808662, -160.5937500020484094 ) ) ;
#15158 = CARTESIAN_POINT ( 'NONE',  ( -2.293366432827344421E-15, -12.48450537969573659, -150.2187500020483810 ) ) ;
#15159 = FACE_OUTER_BOUND ( 'NONE', #34611, .T. ) ;
#15160 = CARTESIAN_POINT ( 'NONE',  ( 5.405949406249999534, 9.363379034771803333, -137.5937500020483810 ) ) ;
#15161 = CARTESIAN_POINT ( 'NONE',  ( 10.81189881249999729, 0.000000000000000000, -141.0312500020483810 ) ) ;
#15162 = CARTESIAN_POINT ( 'NONE',  ( 10.81189881249999729, 6.242252689847867408, -148.2187500020484094 ) ) ;
#15163 = DIRECTION ( 'NONE',  ( -0.000000000000000000, -0.000000000000000000, 1.000000000000000000 ) ) ;
#15164 =( BOUNDED_CURVE ( )  B_SPLINE_CURVE ( 2, ( #17516, #30714, #11689, #14920, #8477, #31574, #9105 ),
 .UNSPECIFIED., .F., .F. ) 
 B_SPLINE_CURVE_WITH_KNOTS ( ( 3, 2, 2, 3 ),
 ( 0.1753731343283582433, 0.1766169154228856009, 0.1778606965174129861, 0.1791044776119403437 ),
 .UNSPECIFIED. ) 
 CURVE ( )  GEOMETRIC_REPRESENTATION_ITEM ( )  RATIONAL_B_SPLINE_CURVE ( ( 0.9999999999999970024, 0.8660254037844417052, 1.000000000000000000, 0.8660254037844387076, 1.000000000000000000, 0.8660254037844327124, 1.000000000000005995 ) ) 
 REPRESENTATION_ITEM ( '' )  );
#15165 = CARTESIAN_POINT ( 'NONE',  ( 9.999999999999676703, 5.773502691896441164, -183.3749999999999432 ) ) ;
#15166 = CARTESIAN_POINT ( 'NONE',  ( 4.999999999999992006, -8.660254037844389075, -168.7500000000000000 ) ) ;
#15167 = AXIS2_PLACEMENT_3D ( 'NONE', #15729, #9065, #36031 ) ;
#15168 = CARTESIAN_POINT ( 'NONE',  ( 10.81189881249999729, 0.000000000000000000, -79.34375000204838102 ) ) ;
#15169 = DIRECTION ( 'NONE',  ( -0.000000000000000000, -0.000000000000000000, -1.000000000000000000 ) ) ;
#15170 = CARTESIAN_POINT ( 'NONE',  ( 10.81189881249999729, 0.000000000000000000, -58.53125000204836681 ) ) ;
#15171 = CARTESIAN_POINT ( 'NONE',  ( 9.999999999999998224, 0.000000000000000000, -149.0000000000000000 ) ) ;
#15172 = CARTESIAN_POINT ( 'NONE',  ( -10.81189881249999729, 6.242252689847871849, -170.2187500020483810 ) ) ;
#15173 = CARTESIAN_POINT ( 'NONE',  ( 10.81189881249999551, -6.242252689847874514, -114.1562500020483952 ) ) ;
#15174 = CARTESIAN_POINT ( 'NONE',  ( 7.644554776091147741E-16, 12.48450537969573659, -149.6562500020484094 ) ) ;
#15175 = CARTESIAN_POINT ( 'NONE',  ( 4.999999999999992006, -8.660254037844389075, -29.24999999999997158 ) ) ;
#15176 = CARTESIAN_POINT ( 'NONE',  ( -2.293366432827344421E-15, -12.48450537969573659, -45.40625000204837391 ) ) ;
#15177 = CARTESIAN_POINT ( 'NONE',  ( -9.999999999999998224, 1.224646799147353059E-15, -118.6250000040967905 ) ) ;
#15178 = CARTESIAN_POINT ( 'NONE',  ( 7.070501591499377789E-16, 11.54700538379251284, -102.1250000000000000 ) ) ;
#15179 = EDGE_LOOP ( 'NONE', ( #6031, #4929 ) ) ;
#15180 =( BOUNDED_CURVE ( )  B_SPLINE_CURVE ( 2, ( #36712, #13181, #26164, #33289, #29612, #26374, #16631 ),
 .UNSPECIFIED., .F., .F. ) 
 B_SPLINE_CURVE_WITH_KNOTS ( ( 3, 2, 2, 3 ),
 ( 0.3843283582089552786, 0.3855721393034826638, 0.3868159203980099936, 0.3880597014925373789 ),
 .UNSPECIFIED. ) 
 CURVE ( )  GEOMETRIC_REPRESENTATION_ITEM ( )  RATIONAL_B_SPLINE_CURVE ( ( 0.9999999999999940048, 0.8660254037844447028, 1.000000000000000000, 0.8660254037844387076, 1.000000000000000000, 0.8660254037844327124, 1.000000000000005995 ) ) 
 REPRESENTATION_ITEM ( '' )  );
#15181 = CARTESIAN_POINT ( 'NONE',  ( 10.81189881249999729, 6.242252689847867408, -122.9062500020483810 ) ) ;
#15182 = CARTESIAN_POINT ( 'NONE',  ( 9.999999999999996447, -5.773502691896262640, -143.5000000040967905 ) ) ;
#15183 = CARTESIAN_POINT ( 'NONE',  ( -10.00000000000102496, 5.773502691895664007, -67.75000000409676204 ) ) ;
#15184 = CARTESIAN_POINT ( 'NONE',  ( 10.81189881249999907, 6.242252689847868297, -179.9062500020484094 ) ) ;
#15185 = ORIENTED_EDGE ( 'NONE', *, *, #37263, .T. ) ;
#15186 = CARTESIAN_POINT ( 'NONE',  ( 10.81189881249999907, 6.242252689847868297, -175.2187500020484094 ) ) ;
#15187 = CARTESIAN_POINT ( 'NONE',  ( 9.999999999999998224, 0.000000000000000000, -47.37500000409677625 ) ) ;
#15188 = CARTESIAN_POINT ( 'NONE',  ( -9.999999999999998224, 1.224646799147353059E-15, -10.24999999999995381 ) ) ;
#15189 = CYLINDRICAL_SURFACE ( 'NONE', #20074, 9.999999999999998224 ) ;
#15190 = CARTESIAN_POINT ( 'NONE',  ( -10.81189881249999907, -6.242252689847864744, -66.65625000204839523 ) ) ;
#15191 = CARTESIAN_POINT ( 'NONE',  ( 4.999999999999992006, -8.660254037844389075, -41.62500000409677625 ) ) ;
#15192 = CARTESIAN_POINT ( 'NONE',  ( 10.81189881249999729, 0.000000000000000000, -5.843750002048370362 ) ) ;
#15193 = CARTESIAN_POINT ( 'NONE',  ( 0.000000000000000000, 0.000000000000000000, -200.0000000000000000 ) ) ;
#15194 = CARTESIAN_POINT ( 'NONE',  ( -10.81189881249999729, 1.324075727343319199E-15, -171.7812500020484094 ) ) ;
#15195 = DIRECTION ( 'NONE',  ( 1.000000000000000000, 0.000000000000000000, 0.000000000000000000 ) ) ;
#15196 = CARTESIAN_POINT ( 'NONE',  ( 9.999999999999998224, 0.000000000000000000, -200.0000000000000000 ) ) ;
#15197 = ORIENTED_EDGE ( 'NONE', *, *, #13005, .F. ) ;
#15198 = CARTESIAN_POINT ( 'NONE',  ( -9.999999999999998224, 1.224646799147353059E-15, -159.1250000040967905 ) ) ;
#15199 = CARTESIAN_POINT ( 'NONE',  ( -5.000000000000003553, -8.660254037844383745, -194.5000000000000000 ) ) ;
#15200 = CARTESIAN_POINT ( 'NONE',  ( 0.000000000000000000, 0.000000000000000000, -200.0000000000000000 ) ) ;
#15201 = LOCAL_TIME ( 11, 57, 6.000000000000000000, #11651 ) ;
#15202 = EDGE_CURVE ( 'NONE', #35906, #38687, #16561, .T. ) ;
#15204 = ORIENTED_EDGE ( 'NONE', *, *, #6913, .F. ) ;
#15203 = CARTESIAN_POINT ( 'NONE',  ( 10.81189881249999551, -6.242252689847874514, -78.15625000204838102 ) ) ;
#15206 = ORIENTED_EDGE ( 'NONE', *, *, #27256, .F. ) ;
#15205 = LINE ( 'NONE', #32064, #11659 ) ;
#15207 = VERTEX_POINT ( 'NONE', #26465 ) ;
#15208 = CARTESIAN_POINT ( 'NONE',  ( 5.405949406249992428, -9.363379034771808662, -25.59375000204835970 ) ) ;
#15209 = CARTESIAN_POINT ( 'NONE',  ( 9.999999999999998224, 0.000000000000000000, -144.5000000000000000 ) ) ;
#15210 = CARTESIAN_POINT ( 'NONE',  ( 10.81189881249999729, 0.000000000000000000, -4.531250002048375691 ) ) ;
#15212 = EDGE_LOOP ( 'NONE', ( #10323, #19537, #4497, #36709 ) ) ;
#15211 = CARTESIAN_POINT ( 'NONE',  ( 10.81189881249999907, 6.242252689847868297, -58.21875000204836681 ) ) ;
#15213 = DIRECTION ( 'NONE',  ( -0.000000000000000000, -0.000000000000000000, 1.000000000000000000 ) ) ;
#15214 = CARTESIAN_POINT ( 'NONE',  ( -4.999999999999996447, 8.660254037844387298, -34.49999999999997158 ) ) ;
#15215 = CARTESIAN_POINT ( 'NONE',  ( 10.81189881249999729, 6.242252689847867408, -194.7187500020484094 ) ) ;
#15216 = CARTESIAN_POINT ( 'NONE',  ( -10.81189881249999729, 6.242252689847871849, -176.2187500020483810 ) ) ;
#15217 = CARTESIAN_POINT ( 'NONE',  ( 5.405949406249999534, 9.363379034771803333, -155.5937500020483810 ) ) ;
#15218 = EDGE_CURVE ( 'NONE', #3659, #15095, #37242, .T. ) ;
#15219 = CARTESIAN_POINT ( 'NONE',  ( -5.405949406249996869, 9.363379034771805109, -179.3437500020483810 ) ) ;
#15220 = CARTESIAN_POINT ( 'NONE',  ( 9.999999999999998224, 0.000000000000000000, -41.37500000409677625 ) ) ;
#15221 = CARTESIAN_POINT ( 'NONE',  ( 9.999999999999998224, 0.000000000000000000, -24.49999999999996447 ) ) ;
#15222 = CARTESIAN_POINT ( 'NONE',  ( -10.00000000000000000, -5.773502691896251982, -194.6250000000000284 ) ) ;
#15223 = CARTESIAN_POINT ( 'NONE',  ( 10.81189881249999551, -6.242252689847874514, -106.4687500020483810 ) ) ;
#15224 = CARTESIAN_POINT ( 'NONE',  ( 9.999999999999998224, 0.000000000000000000, -200.0000000000000000 ) ) ;
#15225 = CARTESIAN_POINT ( 'NONE',  ( -5.405949406250003975, -9.363379034771801557, -80.03125000204838102 ) ) ;
#15226 = CARTESIAN_POINT ( 'NONE',  ( -5.405949406249996869, 9.363379034771805109, -89.34375000204838102 ) ) ;
#15227 = CARTESIAN_POINT ( 'NONE',  ( 10.81189881249999729, 0.000000000000000000, -66.03125000204838102 ) ) ;
#15228 = CARTESIAN_POINT ( 'NONE',  ( -5.000000000000003553, -8.660254037844383745, -148.3750000040967905 ) ) ;
#15229 = CARTESIAN_POINT ( 'NONE',  ( -4.999999999999996447, 8.660254037844387298, -126.0000000000000000 ) ) ;
#15230 = AXIS2_PLACEMENT_3D ( 'NONE', #33321, #30081, #3746 ) ;
#15231 = ORIENTED_EDGE ( 'NONE', *, *, #13676, .F. ) ;
#15232 = CARTESIAN_POINT ( 'NONE',  ( -5.405949406249996869, 9.363379034771805109, -149.5312500020483810 ) ) ;
#15233 = CARTESIAN_POINT ( 'NONE',  ( 10.81189881249999551, -6.242252689847874514, -165.1562500020483526 ) ) ;
#15234 = APPROVAL_PERSON_ORGANIZATION ( #17009, #21199, #33864 ) ;
#15235 = CARTESIAN_POINT ( 'NONE',  ( 9.999999999999998224, 1.224646799147353059E-15, -99.99999999999998579 ) ) ;
#15236 = CARTESIAN_POINT ( 'NONE',  ( 10.70731569305653252, 1.500182182591227154, -180.0000000000000284 ) ) ;
#15237 = CARTESIAN_POINT ( 'NONE',  ( 10.81189881249999551, -6.242252689847874514, -101.9687500020483810 ) ) ;
#15238 = EDGE_LOOP ( 'NONE', ( #15424, #36816, #11370, #14620 ) ) ;
#15239 = CARTESIAN_POINT ( 'NONE',  ( 10.00000000000000000, 5.773502691896255534, -66.37499999999998579 ) ) ;
#15240 = CARTESIAN_POINT ( 'NONE',  ( 5.405949406249999534, 9.363379034771803333, 0.2187499979516283055 ) ) ;
#15241 = CARTESIAN_POINT ( 'NONE',  ( -10.00000000000000000, -5.773502691896251982, -82.50000000409677625 ) ) ;
#15242 = CARTESIAN_POINT ( 'NONE',  ( 0.000000000000000000, 0.000000000000000000, -99.99999999999998579 ) ) ;
#15243 = CARTESIAN_POINT ( 'NONE',  ( -5.405949406249996869, 9.363379034771805109, -91.03125000204838102 ) ) ;
#15244 = CARTESIAN_POINT ( 'NONE',  ( -10.81189881249999729, 1.324075727343319199E-15, -78.78125000204838102 ) ) ;
#15245 = CARTESIAN_POINT ( 'NONE',  ( -10.00000000000000000, -5.773502691896251982, -70.50000000409677625 ) ) ;
#15246 = LINE ( 'NONE', #15458, #36238 ) ;
#15247 = CARTESIAN_POINT ( 'NONE',  ( -5.405949406249996869, 9.363379034771805109, -23.34375000204835970 ) ) ;
#15248 = ORIENTED_EDGE ( 'NONE', *, *, #21754, .T. ) ;
#15249 = CARTESIAN_POINT ( 'NONE',  ( 7.644554776091147741E-16, 12.48450537969573659, -193.1562500020484094 ) ) ;
#15250 = CARTESIAN_POINT ( 'NONE',  ( 10.81189881249999907, 6.242252689847868297, -23.90625000204838102 ) ) ;
#15251 = CARTESIAN_POINT ( 'NONE',  ( 7.644554776091147741E-16, 12.48450537969573659, -8.468750002048356151 ) ) ;
#15252 = CARTESIAN_POINT ( 'NONE',  ( 7.070501591499376803E-16, 11.54700538379251284, -160.6250000000000284 ) ) ;
#15253 = CARTESIAN_POINT ( 'NONE',  ( 7.644554776091147741E-16, 12.48450537969573659, -143.4687500020483810 ) ) ;
#15254 =( BOUNDED_CURVE ( )  B_SPLINE_CURVE ( 2, ( #35051, #12354, #21439, #11719, #38272, #25551, #38702 ),
 .UNSPECIFIED., .F., .F. ) 
 B_SPLINE_CURVE_WITH_KNOTS ( ( 3, 2, 2, 3 ),
 ( 0.9328358208955226383, 0.9340796019900500236, 0.9353233830845774088, 0.9365671641791047941 ),
 .UNSPECIFIED. ) 
 CURVE ( )  GEOMETRIC_REPRESENTATION_ITEM ( )  RATIONAL_B_SPLINE_CURVE ( ( 0.9999999999999761302, 0.8660254037844625774, 1.000000000000000000, 0.8660254037844387076, 1.000000000000000000, 0.8660254037844028474, 1.000000000000035971 ) ) 
 REPRESENTATION_ITEM ( '' )  );
#15255 = CARTESIAN_POINT ( 'NONE',  ( 5.000000000000000000, 8.660254037844385522, -192.2500000000000000 ) ) ;
#15256 = DIRECTION ( 'NONE',  ( 0.5000000000000007772, -0.8660254037844381525, 0.000000000000000000 ) ) ;
#15257 = EDGE_CURVE ( 'NONE', #11871, #16838, #10050, .T. ) ;
#15258 = CARTESIAN_POINT ( 'NONE',  ( -9.999999999999998224, 5.773502691896259087, -172.3750000000000000 ) ) ;
#15259 = CARTESIAN_POINT ( 'NONE',  ( -9.999999999999998224, 1.224646799147353059E-15, -119.7500000000000000 ) ) ;
#15261 = ORIENTED_EDGE ( 'NONE', *, *, #31687, .F. ) ;
#15260 = CARTESIAN_POINT ( 'NONE',  ( -10.81189881249999907, -6.242252689847864744, -101.1562500020483952 ) ) ;
#15262 = CARTESIAN_POINT ( 'NONE',  ( -5.000000000000003553, -8.660254037844383745, -161.8750000040967905 ) ) ;
#15263 = ORIENTED_EDGE ( 'NONE', *, *, #39587, .F. ) ;
#15264 = EDGE_LOOP ( 'NONE', ( #15887, #26633, #13180, #5732 ) ) ;
#15265 = AXIS2_PLACEMENT_3D ( 'NONE', #30995, #1422, #17367 ) ;
#15266 = CARTESIAN_POINT ( 'NONE',  ( -10.81189881249999907, -6.242252689847864744, -33.65625000204836681 ) ) ;
#15267 = DATE_AND_TIME ( #30837, #29060 ) ;
#15268 = VERTEX_POINT ( 'NONE', #7901 ) ;
#15269 = CARTESIAN_POINT ( 'NONE',  ( 10.81189881249999551, -6.242252689847874514, -85.46875000204836681 ) ) ;
#15270 = CARTESIAN_POINT ( 'NONE',  ( 9.999999999999998224, 0.000000000000000000, -3.875000004096768258 ) ) ;
#15271 = EDGE_CURVE ( 'NONE', #5984, #24638, #13694, .T. ) ;
#15272 = CARTESIAN_POINT ( 'NONE',  ( 8.891868809992706346, -4.636149425435562854, -99.99999999999998579 ) ) ;
#15273 = CARTESIAN_POINT ( 'NONE',  ( -9.999999999998969713, -5.773502691896847949, -130.5000000040967905 ) ) ;
#15274 = CARTESIAN_POINT ( 'NONE',  ( -5.405949406250003975, -9.363379034771801557, -162.5312500020484094 ) ) ;
#15275 = CARTESIAN_POINT ( 'NONE',  ( -4.999999999999996447, 8.660254037844387298, -13.87500000409674961 ) ) ;
#15276 = AXIS2_PLACEMENT_3D ( 'NONE', #31330, #17270, #13815 ) ;
#15277 = LINE ( 'NONE', #28684, #26034 ) ;
#15278 = CARTESIAN_POINT ( 'NONE',  ( 7.644554776091147741E-16, 12.48450537969573659, -117.9687500020483668 ) ) ;
#15279 = CARTESIAN_POINT ( 'NONE',  ( 5.405949406249992428, -9.363379034771808662, -85.59375000204836681 ) ) ;
#15280 = CARTESIAN_POINT ( 'NONE',  ( 10.81189881249999729, 0.000000000000000000, -194.8437500020484094 ) ) ;
#15281 = CARTESIAN_POINT ( 'NONE',  ( 5.405949406249999534, 9.363379034771803333, -92.78125000204838102 ) ) ;
#15282 = CARTESIAN_POINT ( 'NONE',  ( 7.070501591499377789E-16, 11.54700538379251284, -168.5000000040967905 ) ) ;
#15283 = CARTESIAN_POINT ( 'NONE',  ( 10.81189881249999729, 6.242252689847867408, -170.9062500020484094 ) ) ;
#15284 = CARTESIAN_POINT ( 'NONE',  ( 7.070501591499376803E-16, 11.54700538379251284, -69.12499999999998579 ) ) ;
#15285 = CARTESIAN_POINT ( 'NONE',  ( -10.81189881249999729, 6.242252689847871849, -174.9062500020484094 ) ) ;
#15286 = CARTESIAN_POINT ( 'NONE',  ( -5.405949406249996869, 9.363379034771805109, -187.0312500020484094 ) ) ;
#15287 = CARTESIAN_POINT ( 'NONE',  ( 7.644554776091147741E-16, 12.48450537969573659, -47.46875000204836681 ) ) ;
#15288 = CARTESIAN_POINT ( 'NONE',  ( -10.00000000000000000, -5.773502691896251982, -160.5000000040967905 ) ) ;
#15289 = CARTESIAN_POINT ( 'NONE',  ( 5.405949406249999534, 9.363379034771803333, -4.281250002048375691 ) ) ;
#15290 = CARTESIAN_POINT ( 'NONE',  ( 10.81189881249999551, -6.242252689847874514, -16.46875000204836681 ) ) ;
#15291 = CARTESIAN_POINT ( 'NONE',  ( 0.000000000000000000, 0.000000000000000000, -200.0000000000000000 ) ) ;
#15292 = CARTESIAN_POINT ( 'NONE',  ( -2.293366432827344421E-15, -12.48450537969573659, -121.7187500020483952 ) ) ;
#15293 = CARTESIAN_POINT ( 'NONE',  ( 9.999999999999996447, -5.773502691896262640, -89.12499999999997158 ) ) ;
#15294 = CARTESIAN_POINT ( 'NONE',  ( 10.81189881249999907, 6.242252689847868297, -19.40625000204837747 ) ) ;
#15295 = CARTESIAN_POINT ( 'NONE',  ( -10.00000000000000000, -5.773502691896251982, -109.5000000040967905 ) ) ;
#15296 = CARTESIAN_POINT ( 'NONE',  ( -9.999999999999227285, -5.773502691896698735, -136.5000000040967620 ) ) ;
#15297 = CARTESIAN_POINT ( 'NONE',  ( -9.999999999999998224, 5.773502691896259087, -52.37499999999997868 ) ) ;
#15298 = CARTESIAN_POINT ( 'NONE',  ( 10.81189881249999907, 6.242252689847868297, -116.9062500020483952 ) ) ;
#15299 = CARTESIAN_POINT ( 'NONE',  ( -10.81189881249999729, 6.242252689847871849, -98.40625000204838102 ) ) ;
#15300 = ORIENTED_EDGE ( 'NONE', *, *, #10422, .F. ) ;
#15301 =( BOUNDED_CURVE ( )  B_SPLINE_CURVE ( 2, ( #28488, #31299, #21782, #38182, #41180, #7980, #1942 ),
 .UNSPECIFIED., .F., .F. ) 
 B_SPLINE_CURVE_WITH_KNOTS ( ( 3, 2, 2, 3 ),
 ( 0.7238805970149256863, 0.7251243781094530716, 0.7263681592039803459, 0.7276119402985077311 ),
 .UNSPECIFIED. ) 
 CURVE ( )  GEOMETRIC_REPRESENTATION_ITEM ( )  RATIONAL_B_SPLINE_CURVE ( ( 0.9999999999999641398, 0.8660254037844745678, 1.000000000000000000, 0.8660254037844387076, 1.000000000000000000, 0.8660254037844148378, 1.000000000000023981 ) ) 
 REPRESENTATION_ITEM ( '' )  );
#15302 = CARTESIAN_POINT ( 'NONE',  ( -9.999999999999998224, 5.773502691896259087, -91.75000000409677625 ) ) ;
#15303 = CARTESIAN_POINT ( 'NONE',  ( -10.00000000000051337, 5.773502691895962435, -71.87499999999998579 ) ) ;
#15304 = CARTESIAN_POINT ( 'NONE',  ( 10.81189881249999551, -6.242252689847874514, -154.6562500020484379 ) ) ;
#15305 = CARTESIAN_POINT ( 'NONE',  ( 5.405949406249999534, 9.363379034771803333, -53.59375000204835970 ) ) ;
#15306 = VERTEX_POINT ( 'NONE', #36595 ) ;
#15307 = CARTESIAN_POINT ( 'NONE',  ( 9.999999999999998224, 0.000000000000000000, -18.49999999999996092 ) ) ;
#15308 = CARTESIAN_POINT ( 'NONE',  ( -10.81189881249999729, 1.324075727343319199E-15, -27.78125000204837036 ) ) ;
#15309 = CARTESIAN_POINT ( 'NONE',  ( 7.070501591499377789E-16, 11.54700538379251284, -153.1250000000000000 ) ) ;
#15310 = CARTESIAN_POINT ( 'NONE',  ( 10.00000000000000000, 5.773502691896255534, -18.75000000409676915 ) ) ;
#15311 = AXIS2_PLACEMENT_3D ( 'NONE', #37776, #20940, #21590 ) ;
#15312 = CARTESIAN_POINT ( 'NONE',  ( 5.000000000000000000, 8.660254037844385522, -199.7500000000000000 ) ) ;
#15313 = CARTESIAN_POINT ( 'NONE',  ( 10.81189881249999729, 0.000000000000000000, -127.5312500020483952 ) ) ;
#15314 = CARTESIAN_POINT ( 'NONE',  ( -9.999999999999998224, 1.224646799147353059E-15, -22.24999999999996447 ) ) ;
#15315 = CARTESIAN_POINT ( 'NONE',  ( -9.999999999999776179, -5.773502691896382544, -188.6250000000000568 ) ) ;
#15316 = ORIENTED_EDGE ( 'NONE', *, *, #22547, .F. ) ;
#15317 = CARTESIAN_POINT ( 'NONE',  ( -10.81189881249999729, 6.242252689847871849, -57.90625000204838813 ) ) ;
#15318 = APPROVAL_ROLE ( '' ) ;
#15319 = CARTESIAN_POINT ( 'NONE',  ( -5.405949406249996869, 9.363379034771805109, -114.8437500020483810 ) ) ;
#15321 = ORIENTED_EDGE ( 'NONE', *, *, #22014, .T. ) ;
#15320 = ORIENTED_EDGE ( 'NONE', *, *, #3134, .T. ) ;
#15322 = CYLINDRICAL_SURFACE ( 'NONE', #25930, 9.999999999999998224 ) ;
#15323 = CARTESIAN_POINT ( 'NONE',  ( -9.999999999999998224, 0.000000000000000000, -99.99999999999998579 ) ) ;
#15324 = CARTESIAN_POINT ( 'NONE',  ( 10.81189881249999729, 0.000000000000000000, -161.8437500020484094 ) ) ;
#15325 = CARTESIAN_POINT ( 'NONE',  ( 5.405949406249999534, 9.363379034771803333, -191.7812500020484094 ) ) ;
#15326 = CARTESIAN_POINT ( 'NONE',  ( -5.405949406250003975, -9.363379034771801557, -7.843750002048343717 ) ) ;
#15327 = EDGE_CURVE ( 'NONE', #42072, #14017, #18211, .T. ) ;
#15328 = CARTESIAN_POINT ( 'NONE',  ( 10.81189881249999729, 6.242252689847867408, -140.7187500020483810 ) ) ;
#15329 = CARTESIAN_POINT ( 'NONE',  ( -10.81189881249999907, -6.242252689847864744, -109.9687500020483668 ) ) ;
#15330 = CARTESIAN_POINT ( 'NONE',  ( 0.000000000000000000, 0.000000000000000000, -200.0000000000000000 ) ) ;
#15331 = CARTESIAN_POINT ( 'NONE',  ( -10.81189881249999729, 6.242252689847871849, -114.9062500020483952 ) ) ;
#15332 = CARTESIAN_POINT ( 'NONE',  ( -10.81189881249999729, 6.242252689847871849, -2.218750002048357928 ) ) ;
#15333 = CARTESIAN_POINT ( 'NONE',  ( -10.81189881249999729, -6.242252689847864744, -121.9687500020484237 ) ) ;
#15334 = CARTESIAN_POINT ( 'NONE',  ( 10.81189881249999729, 6.242252689847867408, -197.9062500020484379 ) ) ;
#15335 = DIRECTION ( 'NONE',  ( -1.000000000000000000, 0.000000000000000000, 0.000000000000000000 ) ) ;
#15336 = CARTESIAN_POINT ( 'NONE',  ( -5.000000000000003553, -8.660254037844383745, -146.5000000000000000 ) ) ;
#15337 = CARTESIAN_POINT ( 'NONE',  ( -9.999999999999998224, 1.224646799147353059E-15, -10.24999999999995381 ) ) ;
#15338 = CARTESIAN_POINT ( 'NONE',  ( 5.405949406249999534, 9.363379034771803333, -68.59375000204836681 ) ) ;
#15339 = CARTESIAN_POINT ( 'NONE',  ( 5.405949406249999534, 9.363379034771803333, -61.09375000204836681 ) ) ;
#15340 = CARTESIAN_POINT ( 'NONE',  ( 7.070501591499377789E-16, 11.54700538379251284, -186.5000000040967905 ) ) ;
#15341 = CARTESIAN_POINT ( 'NONE',  ( -5.405949406250003975, -9.363379034771801557, -27.53125000204836681 ) ) ;
#15342 = CARTESIAN_POINT ( 'NONE',  ( -5.405949406249996869, 9.363379034771805109, -41.34375000204837391 ) ) ;
#15343 = CARTESIAN_POINT ( 'NONE',  ( -10.81189881249999729, 6.242252689847871849, -149.2187500020484379 ) ) ;
#15344 = CARTESIAN_POINT ( 'NONE',  ( -9.999999999999998224, 5.773502691896259087, -113.8750000000000000 ) ) ;
#15345 = CARTESIAN_POINT ( 'NONE',  ( 5.000000000000000000, 8.660254037844385522, -136.7499999999999716 ) ) ;
#15346 = CARTESIAN_POINT ( 'NONE',  ( 7.070501591499377789E-16, 11.54700538379251284, -75.12500000000000000 ) ) ;
#15347 = CARTESIAN_POINT ( 'NONE',  ( 7.644554776091147741E-16, 12.48450537969573659, -143.6562500020484094 ) ) ;
#15348 = CARTESIAN_POINT ( 'NONE',  ( 5.405949406249992428, -9.363379034771808662, -12.28125000204835438 ) ) ;
#15349 = ORIENTED_EDGE ( 'NONE', *, *, #20048, .T. ) ;
#15350 = CARTESIAN_POINT ( 'NONE',  ( 5.000000000000000000, 8.660254037844385522, -120.6250000040967905 ) ) ;
#15351 = CARTESIAN_POINT ( 'NONE',  ( 5.000000000000000000, 8.660254037844385522, -119.1250000040967905 ) ) ;
#15352 = DIRECTION ( 'NONE',  ( 1.000000000000000000, -1.734723475976807094E-16, 0.000000000000000000 ) ) ;
#15353 = CARTESIAN_POINT ( 'NONE',  ( 10.81189881249999907, 6.242252689847868297, -74.71875000204838102 ) ) ;
#15354 = CARTESIAN_POINT ( 'NONE',  ( -9.999999999999998224, 5.773502691896259087, -50.87499999999998579 ) ) ;
#15355 = CARTESIAN_POINT ( 'NONE',  ( 5.000000000000000000, 8.660254037844385522, -23.12500000409675849 ) ) ;
#15356 = CARTESIAN_POINT ( 'NONE',  ( 9.999999999999998224, 0.000000000000000000, -13.99999999999995737 ) ) ;
#15357 = CARTESIAN_POINT ( 'NONE',  ( 10.81189881249999551, -6.242252689847874514, -40.65625000204835970 ) ) ;
#15358 = CYLINDRICAL_SURFACE ( 'NONE', #17265, 9.999999999999998224 ) ;
#15359 = CARTESIAN_POINT ( 'NONE',  ( 10.81189881249999551, -6.242252689847874514, -145.6562500020484094 ) ) ;
#15360 = CARTESIAN_POINT ( 'NONE',  ( -10.81189881249999729, 1.324075727343319199E-15, -152.2812500020484094 ) ) ;
#15361 = DIRECTION ( 'NONE',  ( 0.000000000000000000, 0.000000000000000000, -1.000000000000000000 ) ) ;
#15362 = CARTESIAN_POINT ( 'NONE',  ( 10.00000000000051159, -5.773502691895965988, -127.0000000040967763 ) ) ;
#15363 = VERTEX_POINT ( 'NONE', #16941 ) ;
#15364 = EDGE_LOOP ( 'NONE', ( #18758, #38403, #38520, #18242 ) ) ;
#15365 = ORIENTED_EDGE ( 'NONE', *, *, #24079, .T. ) ;
#15366 = CARTESIAN_POINT ( 'NONE',  ( 4.999999999999992006, -8.660254037844389075, -100.1250000040967905 ) ) ;
#15367 = CARTESIAN_POINT ( 'NONE',  ( -5.405949406249996869, 9.363379034771805109, -179.3437500020483810 ) ) ;
#15368 = CARTESIAN_POINT ( 'NONE',  ( -5.405949406250003975, -9.363379034771801557, -33.34375000204836681 ) ) ;
#15369 = CARTESIAN_POINT ( 'NONE',  ( 9.999999999999479527, 5.773502691896553074, -118.8749999999999858 ) ) ;
#15370 = ADVANCED_FACE ( 'NONE', ( #10472 ), #16087, .F. ) ;
#15371 = CARTESIAN_POINT ( 'NONE',  ( 7.644554776091147741E-16, 12.48450537969573659, -164.4687500020483810 ) ) ;
#15372 = CARTESIAN_POINT ( 'NONE',  ( -10.81189881249999729, 6.242252689847871849, -149.2187500020484379 ) ) ;
#15373 = CARTESIAN_POINT ( 'NONE',  ( -9.999999999999998224, 1.224646799147353059E-15, -88.62500000409677625 ) ) ;
#15374 = CARTESIAN_POINT ( 'NONE',  ( -10.81189881249999729, 6.242252689847871849, -134.2187500020483810 ) ) ;
#15375 = CARTESIAN_POINT ( 'NONE',  ( 5.405949406249992428, -9.363379034771808662, -138.2812500020483810 ) ) ;
#15377 = EDGE_CURVE ( 'NONE', #32801, #14436, #5627, .T. ) ;
#15376 = CARTESIAN_POINT ( 'NONE',  ( 10.81189881249999729, 6.242252689847867408, -149.7187500020483810 ) ) ;
#15378 = CARTESIAN_POINT ( 'NONE',  ( -9.999999999999998224, 1.224646799147353059E-15, -128.7499999999999716 ) ) ;
#15379 = CARTESIAN_POINT ( 'NONE',  ( 5.000000000000000000, 8.660254037844385522, -183.2500000000000000 ) ) ;
#15380 = CARTESIAN_POINT ( 'NONE',  ( 9.999999999999996447, -5.773502691896262640, -171.6250000000000284 ) ) ;
#15381 = ADVANCED_FACE ( 'NONE', ( #42426 ), #9635, .T. ) ;
#15382 = CARTESIAN_POINT ( 'NONE',  ( 10.81189881249999907, 6.242252689847868297, -83.71875000204836681 ) ) ;
#15383 = DIRECTION ( 'NONE',  ( -0.000000000000000000, -0.000000000000000000, 1.000000000000000000 ) ) ;
#15384 = CARTESIAN_POINT ( 'NONE',  ( 7.644554776091147741E-16, 12.48450537969573659, -53.65625000204838102 ) ) ;
#15385 = CARTESIAN_POINT ( 'NONE',  ( -6.979918204473413823, 8.247283589362350398, -99.99999999999998579 ) ) ;
#15386 = CARTESIAN_POINT ( 'NONE',  ( 10.81189881249999551, -6.242252689847874514, -170.9687500020483810 ) ) ;
#15387 = CARTESIAN_POINT ( 'NONE',  ( -10.00000000000000000, -5.773502691896251982, -136.1250000000000000 ) ) ;
#15388 = CARTESIAN_POINT ( 'NONE',  ( -2.293366432827344421E-15, -12.48450537969573659, -144.4062500020484094 ) ) ;
#15389 = APPROVAL ( #17216, 'UNSPECIFIED' ) ;
#15390 = CARTESIAN_POINT ( 'NONE',  ( 9.999999999999998224, 0.000000000000000000, -69.49999999999997158 ) ) ;
#15391 = CARTESIAN_POINT ( 'NONE',  ( -10.81189881249999907, -6.242252689847864744, -33.65625000204835970 ) ) ;
#15392 = CARTESIAN_POINT ( 'NONE',  ( 4.999999999999992006, -8.660254037844389075, -124.1250000040967905 ) ) ;
#15393 = CARTESIAN_POINT ( 'NONE',  ( -5.000000000000003553, -8.660254037844383745, -101.5000000000000000 ) ) ;
#15394 = VERTEX_POINT ( 'NONE', #21257 ) ;
#15395 = CARTESIAN_POINT ( 'NONE',  ( -5.405949406250003975, -9.363379034771801557, -117.5312500020483952 ) ) ;
#15396 = CARTESIAN_POINT ( 'NONE',  ( -5.000000000000003553, -8.660254037844383745, -140.8750000040967905 ) ) ;
#15397 = CARTESIAN_POINT ( 'NONE',  ( -9.999999999999998224, 1.224646799147353059E-15, -154.6250000040967905 ) ) ;
#15398 = CARTESIAN_POINT ( 'NONE',  ( 10.81189881249999907, 6.242252689847868297, -182.9062500020484094 ) ) ;
#15399 = ORIENTED_EDGE ( 'NONE', *, *, #33696, .F. ) ;
#15400 = CARTESIAN_POINT ( 'NONE',  ( 10.00000000000000000, 5.773502691896255534, -47.25000000409676915 ) ) ;
#15401 = DIRECTION ( 'NONE',  ( 1.000000000000000000, 0.000000000000000000, 0.000000000000000000 ) ) ;
#15402 = CARTESIAN_POINT ( 'NONE',  ( 7.644554776091147741E-16, 12.48450537969573659, -65.65625000204838102 ) ) ;
#15403 = FACE_BOUND ( 'NONE', #12757, .T. ) ;
#15404 = CARTESIAN_POINT ( 'NONE',  ( -2.293366432827344421E-15, -12.48450537969573659, -171.4062500020484379 ) ) ;
#15405 = EDGE_CURVE ( 'NONE', #3969, #8277, #1635, .T. ) ;
#15406 = PLANE ( 'NONE',  #24264 ) ;
#15407 = FACE_OUTER_BOUND ( 'NONE', #30364, .T. ) ;
#15408 = ORIENTED_EDGE ( 'NONE', *, *, #29872, .T. ) ;
#15409 = DIRECTION ( 'NONE',  ( -0.000000000000000000, -0.000000000000000000, 1.000000000000000000 ) ) ;
#15410 = CARTESIAN_POINT ( 'NONE',  ( 0.000000000000000000, 0.000000000000000000, -240.0000000000000000 ) ) ;
#15411 =( BOUNDED_CURVE ( )  B_SPLINE_CURVE ( 2, ( #374, #3813, #35979, #23029, #33390, #40047, #9645 ),
 .UNSPECIFIED., .F., .F. ) 
 B_SPLINE_CURVE_WITH_KNOTS ( ( 3, 2, 2, 3 ),
 ( 0.1902985074626866169, 0.1915422885572139744, 0.1927860696517413319, 0.1940298507462686894 ),
 .UNSPECIFIED. ) 
 CURVE ( )  GEOMETRIC_REPRESENTATION_ITEM ( )  RATIONAL_B_SPLINE_CURVE ( ( 0.9999999999999940048, 0.8660254037844447028, 1.000000000000000000, 0.8660254037844387076, 1.000000000000000000, 0.8660254037844357100, 1.000000000000003109 ) ) 
 REPRESENTATION_ITEM ( '' )  );
#15412 = CARTESIAN_POINT ( 'NONE',  ( 9.999999999998969713, 5.773502691896851502, -27.37499999999996092 ) ) ;
#15414 = ORIENTED_EDGE ( 'NONE', *, *, #11683, .T. ) ;
#15413 = CARTESIAN_POINT ( 'NONE',  ( 10.81189881249999729, 0.000000000000000000, -75.03125000204838102 ) ) ;
#15415 = SHAPE_REPRESENTATION_RELATIONSHIP ( 'NONE' , 'NONE' ,  #12816, #16028 ) ;
#15417 = ORIENTED_EDGE ( 'NONE', *, *, #41370, .T. ) ;
#15416 = CARTESIAN_POINT ( 'NONE',  ( -2.121150477449813534E-15, -11.54700538379251284, -143.3750000000000000 ) ) ;
#15418 = ORIENTED_EDGE ( 'NONE', *, *, #41781, .T. ) ;
#15419 = CARTESIAN_POINT ( 'NONE',  ( -5.405949406250003975, -9.363379034771801557, -30.34375000204836326 ) ) ;
#15421 = DIRECTION ( 'NONE',  ( -0.000000000000000000, -0.000000000000000000, -1.000000000000000000 ) ) ;
#15420 =( BOUNDED_CURVE ( )  B_SPLINE_CURVE ( 2, ( #39294, #29813, #36281, #32837, #33049, #254, #13375 ),
 .UNSPECIFIED., .F., .F. ) 
 B_SPLINE_CURVE_WITH_KNOTS ( ( 3, 2, 2, 3 ),
 ( 0.2835820895522389029, 0.2848258706467662882, 0.2860696517412936180, 0.2873134328358210032 ),
 .UNSPECIFIED. ) 
 CURVE ( )  GEOMETRIC_REPRESENTATION_ITEM ( )  RATIONAL_B_SPLINE_CURVE ( ( 0.9999999999999880096, 0.8660254037844506980, 1.000000000000000000, 0.8660254037844387076, 1.000000000000000000, 0.8660254037844267172, 1.000000000000011990 ) ) 
 REPRESENTATION_ITEM ( '' )  );
#15422 = CARTESIAN_POINT ( 'NONE',  ( -10.81189881249999907, -6.242252689847864744, -9.656250002048379244 ) ) ;
#15424 = ORIENTED_EDGE ( 'NONE', *, *, #19650, .F. ) ;
#15423 = CARTESIAN_POINT ( 'NONE',  ( 5.405949406249999534, 9.363379034771803333, -56.59375000204835970 ) ) ;
#15425 = CARTESIAN_POINT ( 'NONE',  ( 0.000000000000000000, 0.000000000000000000, -180.0000000000000000 ) ) ;
#15426 = CARTESIAN_POINT ( 'NONE',  ( -5.000000000000003553, -8.660254037844383745, -38.49999999999997868 ) ) ;
#15427 = CARTESIAN_POINT ( 'NONE',  ( 7.644554776091147741E-16, 12.48450537969573659, -189.9687500020484094 ) ) ;
#15428 = CARTESIAN_POINT ( 'NONE',  ( 5.405949406249999534, 9.363379034771803333, -181.0937500020483810 ) ) ;
#15429 = CARTESIAN_POINT ( 'NONE',  ( -2.293366432827344421E-15, -12.48450537969573659, -160.7187500020483810 ) ) ;
#15430 = CARTESIAN_POINT ( 'NONE',  ( 5.405949406249992428, -9.363379034771808662, -166.5937500020484094 ) ) ;
#15431 = CARTESIAN_POINT ( 'NONE',  ( 9.999999999999998224, 0.000000000000000000, -165.5000000000000000 ) ) ;
#15432 =( BOUNDED_CURVE ( )  B_SPLINE_CURVE ( 2, ( #18443, #8325, #34653, #11962, #25152, #38300, #8745 ),
 .UNSPECIFIED., .F., .F. ) 
 B_SPLINE_CURVE_WITH_KNOTS ( ( 3, 2, 2, 3 ),
 ( 0.9776119402985076201, 0.9788557213930348944, 0.9800995024875623907, 0.9813432835820897759 ),
 .UNSPECIFIED. ) 
 CURVE ( )  GEOMETRIC_REPRESENTATION_ITEM ( )  RATIONAL_B_SPLINE_CURVE ( ( 0.9999999999999880096, 0.8660254037844506980, 1.000000000000000000, 0.8660254037844387076, 1.000000000000000000, 0.8660254037844148378, 1.000000000000023981 ) ) 
 REPRESENTATION_ITEM ( '' )  );
#15433 = DIRECTION ( 'NONE',  ( -0.000000000000000000, -0.000000000000000000, 1.000000000000000000 ) ) ;
#15434 = CARTESIAN_POINT ( 'NONE',  ( -2.121150477449813534E-15, -11.54700538379251284, -198.8750000000000284 ) ) ;
#15435 = CARTESIAN_POINT ( 'NONE',  ( 7.644554776091147741E-16, 12.48450537969573659, -101.4687500020483668 ) ) ;
#15436 = CARTESIAN_POINT ( 'NONE',  ( -9.999999999999998224, 1.224646799147353059E-15, -73.24999999999998579 ) ) ;
#15437 = CARTESIAN_POINT ( 'NONE',  ( 10.81189881249999551, -6.242252689847874514, -70.65625000204839523 ) ) ;
#15438 = CARTESIAN_POINT ( 'NONE',  ( 5.405949406249999534, 9.363379034771803333, -94.09375000204838102 ) ) ;
#15439 = CARTESIAN_POINT ( 'NONE',  ( -5.405949406250003975, -9.363379034771801557, -68.03125000204838102 ) ) ;
#15440 = CARTESIAN_POINT ( 'NONE',  ( -10.00000000000000000, -5.773502691896251982, -145.5000000040967905 ) ) ;
#15441 = CARTESIAN_POINT ( 'NONE',  ( 10.00000000000000000, 5.773502691896255534, -126.3749999999999858 ) ) ;
#15442 = ORIENTED_EDGE ( 'NONE', *, *, #39183, .F. ) ;
#15443 = CARTESIAN_POINT ( 'NONE',  ( 5.405949406249999534, 9.363379034771803333, -152.7812500020484094 ) ) ;
#15444 = CARTESIAN_POINT ( 'NONE',  ( 10.81189881249999907, 6.242252689847868297, -164.9062500020484094 ) ) ;
#15445 = EDGE_CURVE ( 'NONE', #8390, #35567, #33107, .T. ) ;
#15446 = CARTESIAN_POINT ( 'NONE',  ( -10.00000000000012790, -5.773502691896178263, -175.1250000000000284 ) ) ;
#15447 = CARTESIAN_POINT ( 'NONE',  ( -9.999999999999998224, 1.224646799147353059E-15, -148.2500000000000000 ) ) ;
#15448 = CARTESIAN_POINT ( 'NONE',  ( -10.81189881249999729, 6.242252689847871849, -95.21875000204838102 ) ) ;
#15449 = ORIENTED_EDGE ( 'NONE', *, *, #30112, .T. ) ;
#15450 = CARTESIAN_POINT ( 'NONE',  ( -10.00000000000000000, -5.773502691896251982, -65.62499999999998579 ) ) ;
#15451 = CARTESIAN_POINT ( 'NONE',  ( -2.293366432827344421E-15, -12.48450537969573659, -196.7187500020484094 ) ) ;
#15452 = CARTESIAN_POINT ( 'NONE',  ( 4.999999999999992006, -8.660254037844389075, -77.62500000409677625 ) ) ;
#15453 = CARTESIAN_POINT ( 'NONE',  ( 7.428843778402297815, -7.774210255481911247, -179.9999999999999716 ) ) ;
#15454 = CARTESIAN_POINT ( 'NONE',  ( -2.121150477449813534E-15, -11.54700538379251284, -144.8750000000000000 ) ) ;
#15455 = CARTESIAN_POINT ( 'NONE',  ( -2.293366432827344421E-15, -12.48450537969573659, -91.90625000204838102 ) ) ;
#15456 = CARTESIAN_POINT ( 'NONE',  ( -10.81189881249999729, 6.242252689847871849, -71.40625000204838102 ) ) ;
#15457 = CARTESIAN_POINT ( 'NONE',  ( 7.070501591499377789E-16, 11.54700538379251284, -69.50000000409679046 ) ) ;
#15458 = CARTESIAN_POINT ( 'NONE',  ( 9.999999999999998224, 0.000000000000000000, -200.0000000000000000 ) ) ;
#15459 = CARTESIAN_POINT ( 'NONE',  ( 5.405949406249999534, 9.363379034771803333, -28.09375000204836326 ) ) ;
#15460 = CARTESIAN_POINT ( 'NONE',  ( -9.999999999999998224, 1.224646799147353059E-15, -100.2499999999999858 ) ) ;
#15461 = CARTESIAN_POINT ( 'NONE',  ( 10.81189881249999729, 0.000000000000000000, -190.5312500020484094 ) ) ;
#15462 = CARTESIAN_POINT ( 'NONE',  ( -5.405949406250003975, -9.363379034771801557, -21.53125000204836326 ) ) ;
#15463 = CARTESIAN_POINT ( 'NONE',  ( 10.81189881249999729, 0.000000000000000000, -2.843750002048367698 ) ) ;
#15464 = CARTESIAN_POINT ( 'NONE',  ( -9.999999999999998224, 1.224646799147353059E-15, -63.12500000409676204 ) ) ;
#15465 = CARTESIAN_POINT ( 'NONE',  ( -9.999999999999479527, -5.773502691896549521, -112.5000000040967478 ) ) ;
#15466 = CARTESIAN_POINT ( 'NONE',  ( -9.999999999999998224, 1.224646799147353059E-15, -175.2500000000000284 ) ) ;
#15467 = CARTESIAN_POINT ( 'NONE',  ( -9.999999999999998224, 1.224646799147353059E-15, -1.249999999999973355 ) ) ;
#15469 = ORIENTED_EDGE ( 'NONE', *, *, #2974, .F. ) ;
#15468 = CARTESIAN_POINT ( 'NONE',  ( -10.81189881249999729, 6.242252689847871849, -102.9062500020483810 ) ) ;
#15470 = CARTESIAN_POINT ( 'NONE',  ( -9.999999999999998224, 1.224646799147353059E-15, -162.1250000040967905 ) ) ;
#15471 = ORIENTED_EDGE ( 'NONE', *, *, #39473, .F. ) ;
#15472 = ORIENTED_EDGE ( 'NONE', *, *, #3823, .F. ) ;
#15473 = CARTESIAN_POINT ( 'NONE',  ( 10.81189881249999551, -6.242252689847874514, -33.15625000204835970 ) ) ;
#15474 = CONTEXT_DEPENDENT_SHAPE_REPRESENTATION ( #6071, #41474 ) ;
#15475 = CARTESIAN_POINT ( 'NONE',  ( 10.81189881249999551, -6.242252689847874514, -77.96875000204838102 ) ) ;
#15476 = CARTESIAN_POINT ( 'NONE',  ( -5.000000000000003553, -8.660254037844383745, -173.5000000000000284 ) ) ;
#15477 = CARTESIAN_POINT ( 'NONE',  ( -10.81189881249999907, -6.242252689847864744, -198.4687500020484379 ) ) ;
#15478 = DIRECTION ( 'NONE',  ( 0.000000000000000000, 0.000000000000000000, -1.000000000000000000 ) ) ;
#15479 = CARTESIAN_POINT ( 'NONE',  ( -10.81189881249999729, 1.324075727343319199E-15, -165.7812500020484094 ) ) ;
#15480 = CARTESIAN_POINT ( 'NONE',  ( 7.070501591499377789E-16, 11.54700538379251284, -12.50000000409677092 ) ) ;
#15481 = CARTESIAN_POINT ( 'NONE',  ( -5.000000000000003553, -8.660254037844383745, -86.49999999999998579 ) ) ;
#15482 = CARTESIAN_POINT ( 'NONE',  ( -10.81189881249999729, 1.324075727343319199E-15, -132.5937500020483810 ) ) ;
#15483 = CARTESIAN_POINT ( 'NONE',  ( -10.81189881249999729, 6.242252689847871849, -113.2187500020483810 ) ) ;
#15484 = CARTESIAN_POINT ( 'NONE',  ( 5.405949406249999534, 9.363379034771803333, -85.09375000204836681 ) ) ;
#15485 = CARTESIAN_POINT ( 'NONE',  ( 10.81189881249999907, 6.242252689847868297, -91.40625000204836681 ) ) ;
#15486 = CARTESIAN_POINT ( 'NONE',  ( -4.999999999999996447, 8.660254037844387298, -168.3750000040967905 ) ) ;
#15487 = CARTESIAN_POINT ( 'NONE',  ( 5.405949406249992428, -9.363379034771808662, -174.2812500020484094 ) ) ;
#15488 = CARTESIAN_POINT ( 'NONE',  ( 9.999999999999998224, 0.000000000000000000, -200.0000000000000000 ) ) ;
#15489 = CARTESIAN_POINT ( 'NONE',  ( -10.81189881249999729, 6.242252689847871849, -173.4062500020483810 ) ) ;
#15490 = CARTESIAN_POINT ( 'NONE',  ( 10.81189881249999551, -6.242252689847874514, -189.1562500020484379 ) ) ;
#15491 = CARTESIAN_POINT ( 'NONE',  ( 10.81189881249999551, -6.242252689847874514, -43.46875000204835970 ) ) ;
#15492 = CARTESIAN_POINT ( 'NONE',  ( -9.999999999999998224, 5.773502691896259087, -165.2500000040967905 ) ) ;
#15493 = CARTESIAN_POINT ( 'NONE',  ( 5.000000000000000000, 8.660254037844385522, -86.12500000409677625 ) ) ;
#15494 = CARTESIAN_POINT ( 'NONE',  ( -2.293366432827344421E-15, -12.48450537969573659, -15.21875000204836326 ) ) ;
#15495 = CARTESIAN_POINT ( 'NONE',  ( -10.81189881249999729, 6.242252689847871849, -120.7187500020483952 ) ) ;
#15496 = CARTESIAN_POINT ( 'NONE',  ( 10.00000000000000000, 5.773502691896255534, -85.87499999999997158 ) ) ;
#15497 = CARTESIAN_POINT ( 'NONE',  ( 5.405949406249999534, 9.363379034771803333, -23.78125000204836681 ) ) ;
#15498 = CARTESIAN_POINT ( 'NONE',  ( 7.070501591499377789E-16, 11.54700538379251284, -98.00000000409677625 ) ) ;
#15499 =( BOUNDED_CURVE ( )  B_SPLINE_CURVE ( 2, ( #38018, #34577, #5434, #41451, #22044, #27880, #5007 ),
 .UNSPECIFIED., .F., .F. ) 
 B_SPLINE_CURVE_WITH_KNOTS ( ( 3, 2, 2, 3 ),
 ( 0.1641791044776119424, 0.1654228855721392999, 0.1666666666666666574, 0.1679104477611940427 ),
 .UNSPECIFIED. ) 
 CURVE ( )  GEOMETRIC_REPRESENTATION_ITEM ( )  RATIONAL_B_SPLINE_CURVE ( ( 1.000000000000000000, 0.8660254037844387076, 1.000000000000000000, 0.8660254037844387076, 1.000000000000000000, 0.8660254037844387076, 1.000000000000000000 ) ) 
 REPRESENTATION_ITEM ( '' )  );
#15500 = CARTESIAN_POINT ( 'NONE',  ( 5.000000000000002665, 20.00000000000000000, -235.0000000000000000 ) ) ;
#15501 = CARTESIAN_POINT ( 'NONE',  ( -5.405949406249996869, 9.363379034771805109, -115.0312500020483952 ) ) ;
#15502 = CARTESIAN_POINT ( 'NONE',  ( -10.81189881249999729, -6.242252689847864744, -99.65625000204839523 ) ) ;
#15503 = EDGE_LOOP ( 'NONE', ( #39360, #7610, #8107, #14885 ) ) ;
#15504 = AXIS2_PLACEMENT_3D ( 'NONE', #29324, #3212, #16339 ) ;
#15505 = CARTESIAN_POINT ( 'NONE',  ( -2.121150477449813534E-15, -11.54700538379251284, -94.25000000409677625 ) ) ;
#15506 = CARTESIAN_POINT ( 'NONE',  ( 5.000000000000000000, 8.660254037844385522, -72.24999999999998579 ) ) ;
#15507 = CARTESIAN_POINT ( 'NONE',  ( 5.405949406249999534, 9.363379034771803333, -160.2812500020484094 ) ) ;
#15508 = CARTESIAN_POINT ( 'NONE',  ( -10.81189881249999729, 1.324075727343319199E-15, -50.09375000204835260 ) ) ;
#15509 = VERTEX_POINT ( 'NONE', #34231 ) ;
#15510 = CARTESIAN_POINT ( 'NONE',  ( 9.999999999999998224, 0.000000000000000000, -13.99999999999995737 ) ) ;
#15511 = CARTESIAN_POINT ( 'NONE',  ( -5.405949406249996869, 9.363379034771805109, -25.03125000204836681 ) ) ;
#15512 = CARTESIAN_POINT ( 'NONE',  ( 5.000000000000000000, 8.660254037844385522, -151.7500000000000000 ) ) ;
#15513 = CARTESIAN_POINT ( 'NONE',  ( -2.121150477449813534E-15, -11.54700538379251284, -16.25000000409676559 ) ) ;
#15514 = EDGE_CURVE ( 'NONE', #18936, #6937, #3347, .T. ) ;
#15515 = CARTESIAN_POINT ( 'NONE',  ( 10.00000000000000000, 5.773502691896255534, -198.3750000000000000 ) ) ;
#15517 = ORIENTED_EDGE ( 'NONE', *, *, #11870, .T. ) ;
#15516 = CARTESIAN_POINT ( 'NONE',  ( -5.405949406250003975, -9.363379034771801557, -129.5312500020484094 ) ) ;
#15518 = CARTESIAN_POINT ( 'NONE',  ( -9.999999999999998224, 1.224646799147353059E-15, -13.24999999999995559 ) ) ;
#15519 = AXIS2_PLACEMENT_3D ( 'NONE', #7767, #7120, #17237 ) ;
#15520 = ORIENTED_EDGE ( 'NONE', *, *, #4340, .T. ) ;
#15521 = CARTESIAN_POINT ( 'NONE',  ( 5.405949406249992428, -9.363379034771808662, -52.78125000204836681 ) ) ;
#15522 = PERSON_AND_ORGANIZATION ( #11915, #17965 ) ;
#15523 = CARTESIAN_POINT ( 'NONE',  ( -2.293366432827344421E-15, -12.48450537969573659, -102.2187500020483952 ) ) ;
#15525 = VERTEX_POINT ( 'NONE', #8105 ) ;
#15524 = EDGE_LOOP ( 'NONE', ( #30524, #35778, #18460, #8759 ) ) ;
#15526 = VECTOR ( 'NONE', #36545, 1000.000000000000114 ) ;
#15527 = FACE_OUTER_BOUND ( 'NONE', #22541, .T. ) ;
#15528 = DIRECTION ( 'NONE',  ( 0.000000000000000000, 0.000000000000000000, 1.000000000000000000 ) ) ;
#15529 = CARTESIAN_POINT ( 'NONE',  ( -10.81189881249999729, 1.324075727343319199E-15, -158.0937500020483810 ) ) ;
#15530 = CARTESIAN_POINT ( 'NONE',  ( 5.405949406249992428, -9.363379034771808662, -189.2812500020484094 ) ) ;
#15531 = CARTESIAN_POINT ( 'NONE',  ( -5.405949406250003975, -9.363379034771801557, -9.343750002048345493 ) ) ;
#15532 = DIRECTION ( 'NONE',  ( 0.000000000000000000, 0.000000000000000000, 1.000000000000000000 ) ) ;
#15533 = EDGE_CURVE ( 'NONE', #8915, #10633, #17365, .T. ) ;
#15534 = CARTESIAN_POINT ( 'NONE',  ( -5.405949406250003975, -9.363379034771801557, -139.8437500020484094 ) ) ;
#15535 = CARTESIAN_POINT ( 'NONE',  ( -10.81189881249999729, 1.324075727343319199E-15, -113.0937500020483810 ) ) ;
#15536 = CARTESIAN_POINT ( 'NONE',  ( 5.321294541346989426, -5.321294541346989426, -220.0000000000000000 ) ) ;
#15537 = CARTESIAN_POINT ( 'NONE',  ( -5.405949406249996869, 9.363379034771805109, -119.5312500020483952 ) ) ;
#15538 = CARTESIAN_POINT ( 'NONE',  ( -2.121150477449813534E-15, -11.54700538379251284, -191.7500000040967905 ) ) ;
#15539 = CARTESIAN_POINT ( 'NONE',  ( 7.644554776091147741E-16, 12.48450537969573659, -123.9687500020483952 ) ) ;
#15540 = CARTESIAN_POINT ( 'NONE',  ( -10.81189881249999729, 1.324075727343319199E-15, -192.7812500020484094 ) ) ;
#15541 =( BOUNDED_CURVE ( )  B_SPLINE_CURVE ( 2, ( #35050, #38913, #2258, #18627, #8928, #34837, #15378 ),
 .UNSPECIFIED., .F., .F. ) 
 B_SPLINE_CURVE_WITH_KNOTS ( ( 3, 2, 2, 3 ),
 ( 0.3507462686567164867, 0.3519900497512438720, 0.3532338308457712572, 0.3544776119402986980 ),
 .UNSPECIFIED. ) 
 CURVE ( )  GEOMETRIC_REPRESENTATION_ITEM ( )  RATIONAL_B_SPLINE_CURVE ( ( 0.9999999999999940048, 0.8660254037844447028, 1.000000000000000000, 0.8660254037844387076, 1.000000000000000000, 0.8660254037844207220, 1.000000000000017986 ) ) 
 REPRESENTATION_ITEM ( '' )  );
#15542 = CARTESIAN_POINT ( 'NONE',  ( 60.00000000000000711, 0.000000000000000000, -223.0000000000000000 ) ) ;
#15543 = CARTESIAN_POINT ( 'NONE',  ( 9.999999999999996447, -5.773502691896262640, -140.1250000000000000 ) ) ;
#15544 = CARTESIAN_POINT ( 'NONE',  ( 7.070501591499377789E-16, 11.54700538379251284, -12.12499999999996980 ) ) ;
#15545 = CARTESIAN_POINT ( 'NONE',  ( 5.405949406249999534, 9.363379034771803333, -70.09375000204836681 ) ) ;
#15546 = CARTESIAN_POINT ( 'NONE',  ( -10.81189881249999729, 1.324075727343319199E-15, -54.59375000204835970 ) ) ;
#15547 = CARTESIAN_POINT ( 'NONE',  ( -9.999999999999998224, 1.224646799147353059E-15, -186.1250000040967905 ) ) ;
#15548 = CARTESIAN_POINT ( 'NONE',  ( 5.405949406249999534, 9.363379034771803333, -23.78125000204836681 ) ) ;
#15549 = CARTESIAN_POINT ( 'NONE',  ( 10.81189881249999729, 0.000000000000000000, -40.34375000204837391 ) ) ;
#15550 = CARTESIAN_POINT ( 'NONE',  ( -9.999999999999479527, -5.773502691896549521, -106.1249999999999716 ) ) ;
#15551 = CARTESIAN_POINT ( 'NONE',  ( 10.81189881249999551, -6.242252689847874514, -146.9687500020484094 ) ) ;
#15552 = CARTESIAN_POINT ( 'NONE',  ( 5.000000000000000000, 8.660254037844385522, -112.7499999999999858 ) ) ;
#15553 = LINE ( 'NONE', #12531, #34852 ) ;
#15554 = AXIS2_PLACEMENT_3D ( 'NONE', #25334, #12768, #41916 ) ;
#15555 = CARTESIAN_POINT ( 'NONE',  ( 4.999999999999992006, -8.660254037844389075, -75.74999999999998579 ) ) ;
#15556 = CARTESIAN_POINT ( 'NONE',  ( -10.81189881249999729, 6.242252689847871849, -140.4062500020484094 ) ) ;
#15557 = CARTESIAN_POINT ( 'NONE',  ( 10.81189881249999729, 0.000000000000000000, -10.53125000204835260 ) ) ;
#15558 = ORIENTED_EDGE ( 'NONE', *, *, #26514, .F. ) ;
#15559 = VECTOR ( 'NONE', #27747, 1000.000000000000114 ) ;
#15560 = CARTESIAN_POINT ( 'NONE',  ( -9.999999999999998224, 1.224646799147353059E-15, -121.2500000000000000 ) ) ;
#15561 = CARTESIAN_POINT ( 'NONE',  ( -9.999999999999998224, 1.224646799147353059E-15, -118.6250000040967905 ) ) ;
#15562 = CARTESIAN_POINT ( 'NONE',  ( 9.999999999999998224, 0.000000000000000000, -86.37500000409677625 ) ) ;
#15563 = CARTESIAN_POINT ( 'NONE',  ( -5.405949406249996869, 9.363379034771805109, -77.34375000204838102 ) ) ;
#15564 = CARTESIAN_POINT ( 'NONE',  ( 10.00000000000000000, 5.773502691896255534, -37.87499999999995737 ) ) ;
#15565 = CARTESIAN_POINT ( 'NONE',  ( -9.999999999999998224, 5.773502691896259087, -28.75000000409675138 ) ) ;
#15566 = CARTESIAN_POINT ( 'NONE',  ( 10.81189881249999729, 6.242252689847867408, -53.90625000204838102 ) ) ;
#15567 = CARTESIAN_POINT ( 'NONE',  ( -9.999999999999998224, 1.224646799147353059E-15, -118.6250000040967905 ) ) ;
#15568 = CARTESIAN_POINT ( 'NONE',  ( 7.644554776091147741E-16, 12.48450537969573659, -34.15625000204835970 ) ) ;
#15569 = DIRECTION ( 'NONE',  ( 1.000000000000000000, 0.000000000000000000, 0.000000000000000000 ) ) ;
#15570 = CARTESIAN_POINT ( 'NONE',  ( 5.405949406249999534, 9.363379034771803333, -143.7812500020483810 ) ) ;
#15571 = CARTESIAN_POINT ( 'NONE',  ( 5.405949406249999534, 9.363379034771803333, -149.7812500020483810 ) ) ;
#15572 = EDGE_CURVE ( 'NONE', #33599, #7201, #36630, .T. ) ;
#15573 = DIRECTION ( 'NONE',  ( -0.000000000000000000, -0.000000000000000000, 1.000000000000000000 ) ) ;
#15574 = ORIENTED_EDGE ( 'NONE', *, *, #35571, .F. ) ;
#15575 = EDGE_LOOP ( 'NONE', ( #5352, #24526, #31969, #9580 ) ) ;
#15576 = VERTEX_POINT ( 'NONE', #24088 ) ;
#15577 = VECTOR ( 'NONE', #4936, 1000.000000000000000 ) ;
#15578 = DIRECTION ( 'NONE',  ( 1.000000000000000000, 0.000000000000000000, 0.000000000000000000 ) ) ;
#15579 = CARTESIAN_POINT ( 'NONE',  ( 10.81189881249999907, 6.242252689847868297, -184.2187500020483810 ) ) ;
#15580 = CARTESIAN_POINT ( 'NONE',  ( -5.405949406249996869, 9.363379034771805109, -33.84375000204836681 ) ) ;
#15581 = CARTESIAN_POINT ( 'NONE',  ( 9.999999999999998224, 0.000000000000000000, -109.9999999999999858 ) ) ;
#15582 = CARTESIAN_POINT ( 'NONE',  ( -5.405949406250003975, -9.363379034771801557, -162.3437500020484094 ) ) ;
#15583 = CARTESIAN_POINT ( 'NONE',  ( -5.405949406249996869, 9.363379034771805109, -153.8437500020483810 ) ) ;
#15584 = CARTESIAN_POINT ( 'NONE',  ( -9.999999999999998224, 1.224646799147353059E-15, -200.0000000000000000 ) ) ;
#15585 = CARTESIAN_POINT ( 'NONE',  ( 5.405949406249999534, 9.363379034771803333, -133.0937500020483810 ) ) ;
#15586 = CARTESIAN_POINT ( 'NONE',  ( -10.81189881249999729, 6.242252689847871849, -137.4062500020484094 ) ) ;
#15587 = CARTESIAN_POINT ( 'NONE',  ( 7.644554776091147741E-16, 12.48450537969573659, -17.46875000204836681 ) ) ;
#15588 = CARTESIAN_POINT ( 'NONE',  ( 5.405949406249999534, 9.363379034771803333, -145.0937500020483810 ) ) ;
#15589 = DIRECTION ( 'NONE',  ( -0.000000000000000000, -0.000000000000000000, 1.000000000000000000 ) ) ;
#15590 = CARTESIAN_POINT ( 'NONE',  ( -9.999999999999998224, 1.224646799147353059E-15, -157.2500000000000000 ) ) ;
#15591 = CARTESIAN_POINT ( 'NONE',  ( 7.070501591499377789E-16, 11.54700538379251284, -168.1250000000000000 ) ) ;
#15592 = CARTESIAN_POINT ( 'NONE',  ( 5.405949406249999534, 9.363379034771803333, -85.09375000204836681 ) ) ;
#15593 = CARTESIAN_POINT ( 'NONE',  ( -10.81189881249999729, 1.324075727343319199E-15, -51.78125000204835970 ) ) ;
#15594 = CARTESIAN_POINT ( 'NONE',  ( -10.81189881249999729, 1.324075727343319199E-15, -63.59375000204836681 ) ) ;
#15595 = CARTESIAN_POINT ( 'NONE',  ( 80.00000000000002842, 19.99999999999999289, -160.0000000000000000 ) ) ;
#15596 = CARTESIAN_POINT ( 'NONE',  ( -10.81189881249999907, -6.242252689847864744, -169.9687500020484094 ) ) ;
#15597 = CARTESIAN_POINT ( 'NONE',  ( 10.00000000000000000, 5.773502691896255534, -136.8750000000000000 ) ) ;
#15598 = CARTESIAN_POINT ( 'NONE',  ( -10.81189881249999729, -6.242252689847864744, -143.1562500020484094 ) ) ;
#15599 = CARTESIAN_POINT ( 'NONE',  ( 9.999999999999998224, 0.000000000000000000, -111.8750000040967763 ) ) ;
#15600 = CARTESIAN_POINT ( 'NONE',  ( 10.81189881249999907, 6.242252689847868297, -40.40625000204836681 ) ) ;
#15601 = CARTESIAN_POINT ( 'NONE',  ( 10.00000000000000000, 5.773502691896255534, -120.7500000040967905 ) ) ;
#15602 = CARTESIAN_POINT ( 'NONE',  ( -4.999999999999996447, 8.660254037844387298, -100.4999999999999858 ) ) ;
#15603 = ORIENTED_EDGE ( 'NONE', *, *, #8320, .F. ) ;
#15604 = CARTESIAN_POINT ( 'NONE',  ( 10.81189881249999729, 6.242252689847867408, -119.9062500020483810 ) ) ;
#15605 = CARTESIAN_POINT ( 'NONE',  ( 9.999999999999996447, -5.773502691896262640, -139.0000000040967905 ) ) ;
#15606 = CARTESIAN_POINT ( 'NONE',  ( 5.000000000000000000, 8.660254037844385522, -52.74999999999996447 ) ) ;
#15607 = CARTESIAN_POINT ( 'NONE',  ( -5.405949406250003975, -9.363379034771801557, -170.0312500020484094 ) ) ;
#15608 = CARTESIAN_POINT ( 'NONE',  ( -5.000000000000003553, -8.660254037844383745, -46.37500000409677625 ) ) ;
#15609 = CARTESIAN_POINT ( 'NONE',  ( 10.00000000000051159, -5.773502691895965988, -98.12499999999998579 ) ) ;
#15610 = CARTESIAN_POINT ( 'NONE',  ( -10.81189881249999729, 1.324075727343319199E-15, -63.78125000204837391 ) ) ;
#15611 = CARTESIAN_POINT ( 'NONE',  ( -9.999999999999998224, 1.224646799147353059E-15, -147.1250000040967905 ) ) ;
#15612 = CARTESIAN_POINT ( 'NONE',  ( 10.81189881249999729, 0.000000000000000000, -171.0312500020484094 ) ) ;
#15613 = CARTESIAN_POINT ( 'NONE',  ( -9.999999999999227285, -5.773502691896698735, -106.5000000040967336 ) ) ;
#15615 = EDGE_CURVE ( 'NONE', #16149, #26720, #4010, .T. ) ;
#15614 = CARTESIAN_POINT ( 'NONE',  ( 4.999999999999992006, -8.660254037844389075, -177.7500000000000284 ) ) ;
#15616 = ORIENTED_EDGE ( 'NONE', *, *, #22890, .F. ) ;
#15617 = EDGE_CURVE ( 'NONE', #35866, #13495, #40664, .T. ) ;
#15618 = FACE_OUTER_BOUND ( 'NONE', #37402, .T. ) ;
#15619 = EDGE_CURVE ( 'NONE', #24959, #14677, #995, .T. ) ;
#15621 = ORIENTED_EDGE ( 'NONE', *, *, #41083, .F. ) ;
#15620 = CARTESIAN_POINT ( 'NONE',  ( -10.81189881249999907, -6.242252689847864744, -75.65625000204839523 ) ) ;
#15623 = ORIENTED_EDGE ( 'NONE', *, *, #20097, .T. ) ;
#15622 = CARTESIAN_POINT ( 'NONE',  ( 9.999999999999998224, 0.000000000000000000, -30.49999999999997158 ) ) ;
#15624 = CC_DESIGN_DATE_AND_TIME_ASSIGNMENT ( #20415, #591, ( #25992 ) ) ;
#15625 = ORIENTED_EDGE ( 'NONE', *, *, #31113, .F. ) ;
#15626 = CARTESIAN_POINT ( 'NONE',  ( -10.81189881249999729, 1.324075727343319199E-15, -27.59375000204836326 ) ) ;
#15627 = CARTESIAN_POINT ( 'NONE',  ( -10.81189881249999907, -6.242252689847864744, -2.156250002048373915 ) ) ;
#15629 = ORIENTED_EDGE ( 'NONE', *, *, #18282, .T. ) ;
#15628 = CARTESIAN_POINT ( 'NONE',  ( 10.81189881249999729, 0.000000000000000000, -55.34375000204835970 ) ) ;
#15630 = CARTESIAN_POINT ( 'NONE',  ( 10.00000000000051159, -5.773502691895965988, -109.0000000040967620 ) ) ;
#15631 = CARTESIAN_POINT ( 'NONE',  ( 9.999999999999998224, 0.000000000000000000, -37.99999999999997868 ) ) ;
#15632 = EDGE_CURVE ( 'NONE', #21702, #36795, #7765, .T. ) ;
#15633 = CARTESIAN_POINT ( 'NONE',  ( 10.81189881249999551, -6.242252689847874514, -187.4687500020484094 ) ) ;
#15634 = CARTESIAN_POINT ( 'NONE',  ( 7.644554776091147741E-16, 12.48450537969573659, -174.9687500020484094 ) ) ;
#15635 = CARTESIAN_POINT ( 'NONE',  ( -2.293366432827344421E-15, -12.48450537969573659, -156.2187500020483810 ) ) ;
#15636 = CARTESIAN_POINT ( 'NONE',  ( 5.405949406249999534, 9.363379034771803333, -169.0937500020484094 ) ) ;
#15637 = LINE ( 'NONE', #9394, #38449 ) ;
#15638 = DIRECTION ( 'NONE',  ( -0.000000000000000000, -0.000000000000000000, 1.000000000000000000 ) ) ;
#15639 = ADVANCED_FACE ( 'NONE', ( #33798 ), #17574, .F. ) ;
#15640 = CARTESIAN_POINT ( 'NONE',  ( 7.070501591499377789E-16, 11.54700538379251284, -196.6250000000000284 ) ) ;
#15641 = CARTESIAN_POINT ( 'NONE',  ( -10.81189881249999729, 1.324075727343319199E-15, -102.5937500020483810 ) ) ;
#15642 = CARTESIAN_POINT ( 'NONE',  ( -9.999999999999998224, 1.224646799147353059E-15, -48.12500000409677625 ) ) ;
#15643 = CARTESIAN_POINT ( 'NONE',  ( 5.405949406249992428, -9.363379034771808662, -78.28125000204838102 ) ) ;
#15644 = CARTESIAN_POINT ( 'NONE',  ( -10.81189881249999729, 6.242252689847871849, -95.21875000204838102 ) ) ;
#15645 = EDGE_CURVE ( 'NONE', #14397, #5685, #20828, .T. ) ;
#15646 = CARTESIAN_POINT ( 'NONE',  ( 5.405949406249999534, 9.363379034771803333, -58.28125000204836681 ) ) ;
#15647 = CARTESIAN_POINT ( 'NONE',  ( 10.00000000000000000, 5.773502691896255534, -143.2500000040967905 ) ) ;
#15648 = CARTESIAN_POINT ( 'NONE',  ( -10.00000000000000000, -5.773502691896251982, -121.1250000000000000 ) ) ;
#15649 = ORIENTED_EDGE ( 'NONE', *, *, #31800, .F. ) ;
#15650 = CARTESIAN_POINT ( 'NONE',  ( -5.405949406250003975, -9.363379034771801557, -143.0312500020483810 ) ) ;
#15651 = CARTESIAN_POINT ( 'NONE',  ( 10.81189881249999907, 6.242252689847868297, -155.9062500020484094 ) ) ;
#15652 = CARTESIAN_POINT ( 'NONE',  ( -5.405949406249996869, 9.363379034771805109, -197.5312500020484094 ) ) ;
#15653 = CARTESIAN_POINT ( 'NONE',  ( -9.999999999999998224, 1.224646799147353059E-15, -200.0000000000000000 ) ) ;
#15654 = CARTESIAN_POINT ( 'NONE',  ( 10.81189881249999551, -6.242252689847874514, -91.46875000204838102 ) ) ;
#15655 = ORIENTED_EDGE ( 'NONE', *, *, #18991, .F. ) ;
#15656 = CARTESIAN_POINT ( 'NONE',  ( -9.999999999999998224, 5.773502691896259087, -67.37500000000001421 ) ) ;
#15657 = CARTESIAN_POINT ( 'NONE',  ( -10.81189881249999907, -6.242252689847864744, -184.9687500020484094 ) ) ;
#15658 = CARTESIAN_POINT ( 'NONE',  ( -9.999999999999998224, 1.224646799147353059E-15, -76.62500000409677625 ) ) ;
#15659 = CARTESIAN_POINT ( 'NONE',  ( -10.00000000000025580, 5.773502691896109873, -101.8750000000000000 ) ) ;
#15660 = CARTESIAN_POINT ( 'NONE',  ( 10.00000000000012257, -5.773502691896187144, -160.0000000040968189 ) ) ;
#15661 = CARTESIAN_POINT ( 'NONE',  ( -10.81189881249999729, 1.324075727343319199E-15, -92.28125000204838102 ) ) ;
#15662 = CARTESIAN_POINT ( 'NONE',  ( 10.81189881249999551, -6.242252689847874514, -70.65625000204839523 ) ) ;
#15663 =( BOUNDED_CURVE ( )  B_SPLINE_CURVE ( 2, ( #34929, #41372, #1697, #28021, #41151, #24796, #18290 ),
 .UNSPECIFIED., .F., .F. ) 
 B_SPLINE_CURVE_WITH_KNOTS ( ( 3, 2, 2, 3 ),
 ( 0.8097014925373136052, 0.8109452736318409904, 0.8121890547263682647, 0.8134328358208956500 ),
 .UNSPECIFIED. ) 
 CURVE ( )  GEOMETRIC_REPRESENTATION_ITEM ( )  RATIONAL_B_SPLINE_CURVE ( ( 0.9999999999999761302, 0.8660254037844625774, 1.000000000000000000, 0.8660254037844387076, 1.000000000000000000, 0.8660254037844267172, 1.000000000000011990 ) ) 
 REPRESENTATION_ITEM ( '' )  );
#15664 = CARTESIAN_POINT ( 'NONE',  ( -10.00000000000000000, -5.773502691896251982, -66.00000000409679046 ) ) ;
#15665 = CARTESIAN_POINT ( 'NONE',  ( 9.999999999999998224, 0.000000000000000000, -93.87500000409677625 ) ) ;
#15666 = CARTESIAN_POINT ( 'NONE',  ( 5.405949406249999534, 9.363379034771803333, -22.09375000204835615 ) ) ;
#15667 = CARTESIAN_POINT ( 'NONE',  ( 5.000000000000000000, 8.660254037844385522, -47.12500000409677625 ) ) ;
#15668 = CARTESIAN_POINT ( 'NONE',  ( -5.405949406250003975, -9.363379034771801557, -197.0312500020484094 ) ) ;
#15669 = CARTESIAN_POINT ( 'NONE',  ( 10.81189881249999551, -6.242252689847874514, -19.65625000204837747 ) ) ;
#15670 = CARTESIAN_POINT ( 'NONE',  ( -5.405949406250003975, -9.363379034771801557, -6.343750002048370362 ) ) ;
#15671 = CARTESIAN_POINT ( 'NONE',  ( -9.999999999999998224, 1.224646799147353059E-15, -117.1250000040967905 ) ) ;
#15672 = CARTESIAN_POINT ( 'NONE',  ( -5.000000000000003553, -8.660254037844383745, 0.1249999959032355168 ) ) ;
#15673 = CARTESIAN_POINT ( 'NONE',  ( -9.999999999999998224, 1.224646799147353059E-15, -112.6250000040967763 ) ) ;
#15674 = ADVANCED_FACE ( 'NONE', ( #1208 ), #24308, .F. ) ;
#15675 = CARTESIAN_POINT ( 'NONE',  ( -2.121150477449813534E-15, -11.54700538379251284, -171.8750000000000284 ) ) ;
#15676 = CARTESIAN_POINT ( 'NONE',  ( -2.121150477449813534E-15, -11.54700538379251284, -36.87499999999996447 ) ) ;
#15678 = VERTEX_POINT ( 'NONE', #40879 ) ;
#15677 = CARTESIAN_POINT ( 'NONE',  ( 10.81189881249999907, 6.242252689847868297, -101.9062500020484094 ) ) ;
#15679 = CARTESIAN_POINT ( 'NONE',  ( 10.00000000000000000, 5.773502691896255534, -170.2500000040967905 ) ) ;
#15680 = ORIENTED_EDGE ( 'NONE', *, *, #36507, .F. ) ;
#15681 = ORIENTED_EDGE ( 'NONE', *, *, #7351, .T. ) ;
#15682 = CARTESIAN_POINT ( 'NONE',  ( 5.405949406249999534, 9.363379034771803333, -26.78125000204836681 ) ) ;
#15683 = COORDINATED_UNIVERSAL_TIME_OFFSET ( 6, 0, .AHEAD. ) ;
#15684 = CARTESIAN_POINT ( 'NONE',  ( -2.293366432827344421E-15, -12.48450537969573659, -79.71875000204838102 ) ) ;
#15685 = CARTESIAN_POINT ( 'NONE',  ( 0.000000000000000000, 0.000000000000000000, -200.0000000000000000 ) ) ;
#15686 = APPLICATION_CONTEXT ( 'configuration controlled 3d designs of mechanical parts and assemblies' ) ;
#15687 = CONICAL_SURFACE ( 'NONE', #28110, 60.00000000000000711, 0.7853981633974447263 ) ;
#15688 = AXIS2_PLACEMENT_3D ( 'NONE', #12036, #19364, #25231 ) ;
#15689 = CARTESIAN_POINT ( 'NONE',  ( -9.999999999999998224, 1.224646799147353059E-15, -19.62500000409675494 ) ) ;
#15690 = ADVANCED_FACE ( 'NONE', ( #24734 ), #15406, .T. ) ;
#15691 = CARTESIAN_POINT ( 'NONE',  ( -9.999999999999998224, 1.224646799147353059E-15, -200.0000000000000000 ) ) ;
#15692 = CARTESIAN_POINT ( 'NONE',  ( 5.000000000000000000, 8.660254037844385522, -49.74999999999998579 ) ) ;
#15693 = CARTESIAN_POINT ( 'NONE',  ( -10.81189881249999907, -6.242252689847864744, -158.1562500020484094 ) ) ;
#15694 = CARTESIAN_POINT ( 'NONE',  ( 9.999999999999996447, -5.773502691896262640, -14.50000000409676382 ) ) ;
#15695 = CARTESIAN_POINT ( 'NONE',  ( -2.121150477449813534E-15, -11.54700538379251284, -172.2500000040968189 ) ) ;
#15696 = CARTESIAN_POINT ( 'NONE',  ( -5.405949406250003975, -9.363379034771801557, -132.3437500020484094 ) ) ;
#15697 = CARTESIAN_POINT ( 'NONE',  ( -10.81189881249999729, 6.242252689847871849, -114.7187500020483810 ) ) ;
#15698 = CARTESIAN_POINT ( 'NONE',  ( 10.81189881249999729, 0.000000000000000000, -80.84375000204838102 ) ) ;
#15699 = CARTESIAN_POINT ( 'NONE',  ( 10.81189881249999551, -6.242252689847874514, -84.15625000204838102 ) ) ;
#15700 = CARTESIAN_POINT ( 'NONE',  ( -5.000000000000003553, -8.660254037844383745, -173.8750000040968189 ) ) ;
#15701 = CARTESIAN_POINT ( 'NONE',  ( 9.999999999999998224, 0.000000000000000000, -140.3750000040967905 ) ) ;
#15702 = CARTESIAN_POINT ( 'NONE',  ( -10.81189881249999729, 6.242252689847871849, -170.4062500020484094 ) ) ;
#15703 = CARTESIAN_POINT ( 'NONE',  ( 10.81189881249999907, 6.242252689847868297, -182.9062500020484094 ) ) ;
#15704 = CARTESIAN_POINT ( 'NONE',  ( -10.81189881249999729, 6.242252689847871849, -45.71875000204837391 ) ) ;
#15705 = CARTESIAN_POINT ( 'NONE',  ( 10.00000000000000000, 5.773502691896255534, -162.7500000040967905 ) ) ;
#15706 = CARTESIAN_POINT ( 'NONE',  ( 5.405949406249992428, -9.363379034771808662, -1.781250002048373471 ) ) ;
#15707 = CARTESIAN_POINT ( 'NONE',  ( 7.644554776091147741E-16, 12.48450537969573659, -11.46875000204836148 ) ) ;
#15708 = FACE_OUTER_BOUND ( 'NONE', #3710, .T. ) ;
#15709 = CARTESIAN_POINT ( 'NONE',  ( -10.81189881249999729, 6.242252689847871849, -117.7187500020483952 ) ) ;
#15710 = CARTESIAN_POINT ( 'NONE',  ( -5.000000000000003553, -8.660254037844383745, -92.49999999999998579 ) ) ;
#15711 = CARTESIAN_POINT ( 'NONE',  ( 10.81189881249999729, 0.000000000000000000, -24.03125000204836681 ) ) ;
#15712 = CARTESIAN_POINT ( 'NONE',  ( 10.00000000000000000, 5.773502691896255534, -96.75000000409679046 ) ) ;
#15713 = DIRECTION ( 'NONE',  ( -0.000000000000000000, -0.000000000000000000, 1.000000000000000000 ) ) ;
#15714 = CARTESIAN_POINT ( 'NONE',  ( 10.81189881249999551, -6.242252689847874514, -112.6562500020483810 ) ) ;
#15715 = CARTESIAN_POINT ( 'NONE',  ( 5.405949406249992428, -9.363379034771808662, -93.28125000204838102 ) ) ;
#15716 = VERTEX_POINT ( 'NONE', #25575 ) ;
#15717 = CARTESIAN_POINT ( 'NONE',  ( 5.000000000000000000, 8.660254037844385522, -92.12500000409677625 ) ) ;
#15718 = CARTESIAN_POINT ( 'NONE',  ( -5.000000000000003553, -8.660254037844383745, -99.99999999999998579 ) ) ;
#15719 = CARTESIAN_POINT ( 'NONE',  ( 5.405949406249992428, -9.363379034771808662, -156.2812500020484094 ) ) ;
#15720 = CARTESIAN_POINT ( 'NONE',  ( -5.405949406250003975, -9.363379034771801557, -49.84375000204838102 ) ) ;
#15721 = ORIENTED_EDGE ( 'NONE', *, *, #9304, .T. ) ;
#15722 = CARTESIAN_POINT ( 'NONE',  ( -4.999999999999996447, 8.660254037844387298, -17.99999999999996092 ) ) ;
#15723 = CARTESIAN_POINT ( 'NONE',  ( 10.81189881249999729, 0.000000000000000000, -22.53125000204836326 ) ) ;
#15724 = CARTESIAN_POINT ( 'NONE',  ( -4.999999999999996447, 8.660254037844387298, -151.5000000000000000 ) ) ;
#15725 = CARTESIAN_POINT ( 'NONE',  ( -2.121150477449813534E-15, -11.54700538379251284, -17.75000000409676559 ) ) ;
#15726 = LINE ( 'NONE', #12695, #8438 ) ;
#15728 = EDGE_LOOP ( 'NONE', ( #14050, #42202, #12063, #18338 ) ) ;
#15727 = CARTESIAN_POINT ( 'NONE',  ( -5.405949406250003975, -9.363379034771801557, -128.0312500020484094 ) ) ;
#15729 = CARTESIAN_POINT ( 'NONE',  ( 0.000000000000000000, 0.000000000000000000, 49.99999999999998579 ) ) ;
#15730 = ORIENTED_EDGE ( 'NONE', *, *, #14906, .F. ) ;
#15731 = CARTESIAN_POINT ( 'NONE',  ( -10.81189881249999729, 6.242252689847871849, -53.40625000204837391 ) ) ;
#15732 = DATE_AND_TIME ( #5834, #41454 ) ;
#15733 = EDGE_CURVE ( 'NONE', #19924, #35515, #12160, .T. ) ;
#15734 = CARTESIAN_POINT ( 'NONE',  ( 10.81189881249999907, 6.242252689847868297, -104.7187500020483810 ) ) ;
#15736 = ORIENTED_EDGE ( 'NONE', *, *, #39587, .T. ) ;
#15735 = ORIENTED_EDGE ( 'NONE', *, *, #27427, .T. ) ;
#15737 = CARTESIAN_POINT ( 'NONE',  ( 9.999999999999479527, 5.773502691896553074, -175.8749999999999716 ) ) ;
#15738 = CARTESIAN_POINT ( 'NONE',  ( -9.999999999999998224, 1.224646799147353059E-15, -184.2500000000000000 ) ) ;
#15739 = CARTESIAN_POINT ( 'NONE',  ( -10.81189881249999907, -6.242252689847864744, -151.9687500020484094 ) ) ;
#15740 = CARTESIAN_POINT ( 'NONE',  ( 5.405949406249992428, -9.363379034771808662, -180.2812500020484094 ) ) ;
#15741 = CARTESIAN_POINT ( 'NONE',  ( 10.81189881249999729, 0.000000000000000000, -4.343750002048368586 ) ) ;
#15742 = CARTESIAN_POINT ( 'NONE',  ( -10.00000000000076916, 5.773502691895813221, -139.3750000000000000 ) ) ;
#15743 = CARTESIAN_POINT ( 'NONE',  ( -10.81189881249999729, 6.242252689847871849, -141.7187500020483810 ) ) ;
#15744 =( BOUNDED_CURVE ( )  B_SPLINE_CURVE ( 2, ( #25443, #35155, #25234, #15695, #18522, #5580, #1927 ),
 .UNSPECIFIED., .F., .F. ) 
 B_SPLINE_CURVE_WITH_KNOTS ( ( 3, 2, 2, 3 ),
 ( 0.1305970149253731227, 0.1318407960199005080, 0.1330845771144278378, 0.1343283582089551953 ),
 .UNSPECIFIED. ) 
 CURVE ( )  GEOMETRIC_REPRESENTATION_ITEM ( )  RATIONAL_B_SPLINE_CURVE ( ( 1.000000000000000000, 0.8660254037844387076, 1.000000000000000000, 0.8660254037844387076, 1.000000000000000000, 0.8660254037844417052, 0.9999999999999970024 ) ) 
 REPRESENTATION_ITEM ( '' )  );
#15745 = CARTESIAN_POINT ( 'NONE',  ( -10.81189881249999907, -6.242252689847864744, -112.9687500020483810 ) ) ;
#15746 = CARTESIAN_POINT ( 'NONE',  ( 0.000000000000000000, 0.000000000000000000, -200.0000000000000000 ) ) ;
#15747 = CARTESIAN_POINT ( 'NONE',  ( -5.405949406250003975, -9.363379034771801557, -113.0312500020483952 ) ) ;
#15748 = CARTESIAN_POINT ( 'NONE',  ( -9.999999999999998224, 1.224646799147353059E-15, -192.1250000040967905 ) ) ;
#15750 = ADVANCED_FACE ( 'NONE', ( #31415 ), #41733, .T. ) ;
#15749 = CARTESIAN_POINT ( 'NONE',  ( 7.644554776091147741E-16, 12.48450537969573659, -125.4687500020483952 ) ) ;
#15751 = CARTESIAN_POINT ( 'NONE',  ( 10.81189881249999551, -6.242252689847874514, -193.6562500020484094 ) ) ;
#15752 = CARTESIAN_POINT ( 'NONE',  ( 7.070501591499376803E-16, 11.54700538379251284, -149.0000000040967905 ) ) ;
#15753 = CARTESIAN_POINT ( 'NONE',  ( 10.00000000000000000, 5.773502691896255534, -141.3750000000000000 ) ) ;
#15754 = CARTESIAN_POINT ( 'NONE',  ( 9.999999999999996447, -5.773502691896262640, -11.12499999999996980 ) ) ;
#15755 = CARTESIAN_POINT ( 'NONE',  ( -10.81189881249999729, 6.242252689847871849, -65.21875000204838102 ) ) ;
#15756 = CARTESIAN_POINT ( 'NONE',  ( -10.81189881249999729, 1.324075727343319199E-15, -45.59375000204838102 ) ) ;
#15757 = CARTESIAN_POINT ( 'NONE',  ( -9.999999999999998224, 1.224646799147353059E-15, -189.1250000040967905 ) ) ;
#15758 = CARTESIAN_POINT ( 'NONE',  ( -10.81189881249999729, 1.324075727343319199E-15, -23.28125000204836326 ) ) ;
#15759 = CARTESIAN_POINT ( 'NONE',  ( -5.405949406249996869, 9.363379034771805109, -35.34375000204836681 ) ) ;
#15760 = CARTESIAN_POINT ( 'NONE',  ( 10.00000000000205347, -5.773502691895071592, -8.124999999999923617 ) ) ;
#15761 = CARTESIAN_POINT ( 'NONE',  ( 7.644554776091147741E-16, 12.48450537969573659, -146.4687500020484094 ) ) ;
#15762 = CARTESIAN_POINT ( 'NONE',  ( 5.000000000000000000, 8.660254037844385522, -115.7499999999999858 ) ) ;
#15763 = DIRECTION ( 'NONE',  ( -0.000000000000000000, -0.000000000000000000, 1.000000000000000000 ) ) ;
#15764 = CARTESIAN_POINT ( 'NONE',  ( 7.070501591499377789E-16, 11.54700538379251284, -67.62500000000000000 ) ) ;
#15765 = CARTESIAN_POINT ( 'NONE',  ( -5.405949406250003975, -9.363379034771801557, -143.0312500020483810 ) ) ;
#15766 = CARTESIAN_POINT ( 'NONE',  ( -2.293366432827344421E-15, -12.48450537969573659, -115.9062500020483952 ) ) ;
#15767 = ORIENTED_EDGE ( 'NONE', *, *, #15983, .T. ) ;
#15768 = CARTESIAN_POINT ( 'NONE',  ( 5.000000000000000000, 8.660254037844385522, -121.7500000000000000 ) ) ;
#15769 = CARTESIAN_POINT ( 'NONE',  ( -4.999999999999996447, 8.660254037844387298, -118.8750000040967905 ) ) ;
#15770 = CARTESIAN_POINT ( 'NONE',  ( 9.999999999999998224, 0.000000000000000000, -170.0000000000000000 ) ) ;
#15771 = CARTESIAN_POINT ( 'NONE',  ( -5.405949406250003975, -9.363379034771801557, -70.84375000204836681 ) ) ;
#15772 = CARTESIAN_POINT ( 'NONE',  ( -4.999999999999996447, 8.660254037844387298, -40.49999999999997868 ) ) ;
#15773 = CARTESIAN_POINT ( 'NONE',  ( -2.121150477449813534E-15, -11.54700538379251284, -28.25000000409675138 ) ) ;
#15774 = CARTESIAN_POINT ( 'NONE',  ( 5.405949406249992428, -9.363379034771808662, -54.28125000204836681 ) ) ;
#15775 = CARTESIAN_POINT ( 'NONE',  ( -9.999999999999998224, 1.224646799147353059E-15, -132.1250000040967620 ) ) ;
#15776 = CARTESIAN_POINT ( 'NONE',  ( -5.405949406250003975, -9.363379034771801557, -35.03125000204837391 ) ) ;
#15777 = CARTESIAN_POINT ( 'NONE',  ( -9.999999999999998224, 1.224646799147353059E-15, -139.2499999999999716 ) ) ;
#15778 = CARTESIAN_POINT ( 'NONE',  ( -5.405949406249996869, 9.363379034771805109, -143.5312500020483810 ) ) ;
#15779 = CARTESIAN_POINT ( 'NONE',  ( -10.81189881249999729, 6.242252689847871849, -149.4062500020484094 ) ) ;
#15780 = CARTESIAN_POINT ( 'NONE',  ( -10.00000000000000000, -5.773502691896252870, -165.0000000040967905 ) ) ;
#15781 = EDGE_LOOP ( 'NONE', ( #7135, #20598, #29289, #7101 ) ) ;
#15782 = EDGE_CURVE ( 'NONE', #23886, #36957, #25424, .T. ) ;
#15783 = AXIS2_PLACEMENT_3D ( 'NONE', #4046, #13943, #4261 ) ;
#15784 = ORIENTED_EDGE ( 'NONE', *, *, #20684, .F. ) ;
#15785 = ORIENTED_EDGE ( 'NONE', *, *, #2480, .T. ) ;
#15786 = CARTESIAN_POINT ( 'NONE',  ( 9.999999999999998224, 0.000000000000000000, -176.3750000040967905 ) ) ;
#15787 =( BOUNDED_CURVE ( )  B_SPLINE_CURVE ( 2, ( #34829, #22297, #21431, #31594, #18620, #41491, #32020 ),
 .UNSPECIFIED., .F., .F. ) 
 B_SPLINE_CURVE_WITH_KNOTS ( ( 3, 2, 2, 3 ),
 ( 0.7873134328358211143, 0.7885572139303484995, 0.7898009950248758848, 0.7910447761194031591 ),
 .UNSPECIFIED. ) 
 CURVE ( )  GEOMETRIC_REPRESENTATION_ITEM ( )  RATIONAL_B_SPLINE_CURVE ( ( 0.9999999999999761302, 0.8660254037844625774, 1.000000000000000000, 0.8660254037844387076, 1.000000000000000000, 0.8660254037844148378, 1.000000000000023981 ) ) 
 REPRESENTATION_ITEM ( '' )  );
#15788 = CARTESIAN_POINT ( 'NONE',  ( 7.644554776091147741E-16, 12.48450537969573659, -185.4687500020483810 ) ) ;
#15789 = CIRCLE ( 'NONE', #33719, 42.00000000000001421 ) ;
#15790 = CARTESIAN_POINT ( 'NONE',  ( -5.405949406249996869, 9.363379034771805109, -27.84375000204836326 ) ) ;
#15791 = CARTESIAN_POINT ( 'NONE',  ( -2.121150477449813534E-15, -11.54700538379251284, -130.2500000040967905 ) ) ;
#15792 = CARTESIAN_POINT ( 'NONE',  ( 7.644554776091147741E-16, 12.48450537969573659, -162.9687500020483810 ) ) ;
#15793 = CARTESIAN_POINT ( 'NONE',  ( -10.81189881249999729, 1.324075727343319199E-15, -141.5937500020483810 ) ) ;
#15794 = DIRECTION ( 'NONE',  ( 1.000000000000000000, 0.000000000000000000, 0.000000000000000000 ) ) ;
#15795 = CARTESIAN_POINT ( 'NONE',  ( 10.81189881249999551, -6.242252689847874514, -131.9687500020483810 ) ) ;
#15796 = CARTESIAN_POINT ( 'NONE',  ( 5.405949406249999534, 9.363379034771803333, -143.7812500020483810 ) ) ;
#15797 = CARTESIAN_POINT ( 'NONE',  ( 10.81189881249999907, 6.242252689847868297, -19.21875000204837747 ) ) ;
#15798 = CARTESIAN_POINT ( 'NONE',  ( 5.405949406249999534, 9.363379034771803333, -143.5937500020483810 ) ) ;
#15799 = DIRECTION ( 'NONE',  ( 1.000000000000000000, 0.000000000000000000, 0.000000000000000000 ) ) ;
#15800 = CARTESIAN_POINT ( 'NONE',  ( -10.00000000000102496, 5.773502691895664007, -33.25000000409673362 ) ) ;
#15801 = CARTESIAN_POINT ( 'NONE',  ( -9.999999999999998224, 1.224646799147353059E-15, -163.2500000000000000 ) ) ;
#15802 = CARTESIAN_POINT ( 'NONE',  ( -5.405949406250003975, -9.363379034771801557, -79.84375000204838102 ) ) ;
#15803 = CARTESIAN_POINT ( 'NONE',  ( -10.81189881249999907, -6.242252689847864744, -51.65625000204838102 ) ) ;
#15804 = CARTESIAN_POINT ( 'NONE',  ( -2.293366432827344421E-15, -12.48450537969573659, -64.71875000204838102 ) ) ;
#15805 = CARTESIAN_POINT ( 'NONE',  ( 5.000000000000000000, 8.660254037844385522, -57.24999999999996447 ) ) ;
#15806 = ADVANCED_FACE ( 'NONE', ( #14979 ), #8954, .T. ) ;
#15807 = CARTESIAN_POINT ( 'NONE',  ( 10.81189881249999729, 0.000000000000000000, -173.8437500020484094 ) ) ;
#15808 = CARTESIAN_POINT ( 'NONE',  ( -5.000000000000003553, -8.660254037844383745, -134.5000000000000000 ) ) ;
#15809 = CARTESIAN_POINT ( 'NONE',  ( -2.293366432827344421E-15, -12.48450537969573659, -145.9062500020484094 ) ) ;
#15810 = DIRECTION ( 'NONE',  ( 1.000000000000000000, 0.000000000000000000, 0.000000000000000000 ) ) ;
#15811 = CARTESIAN_POINT ( 'NONE',  ( 10.00000000000000000, 5.773502691896255534, -119.2500000040967905 ) ) ;
#15812 = CARTESIAN_POINT ( 'NONE',  ( 10.00000000000000000, 5.773502691896255534, -88.87499999999998579 ) ) ;
#15813 = ORIENTED_EDGE ( 'NONE', *, *, #39940, .T. ) ;
#15814 = CARTESIAN_POINT ( 'NONE',  ( -5.405949406249996869, 9.363379034771805109, -118.0312500020483952 ) ) ;
#15815 = CARTESIAN_POINT ( 'NONE',  ( -4.999999999999996447, 8.660254037844387298, -136.8750000040967905 ) ) ;
#15816 = CARTESIAN_POINT ( 'NONE',  ( -9.999999999999998224, 1.224646799147353059E-15, -193.6250000040967905 ) ) ;
#15817 = VECTOR ( 'NONE', #8701, 1000.000000000000000 ) ;
#15818 = CARTESIAN_POINT ( 'NONE',  ( -2.293366432827344421E-15, -12.48450537969573659, -171.4062500020484379 ) ) ;
#15819 = CARTESIAN_POINT ( 'NONE',  ( -4.999999999999996447, 8.660254037844387298, -49.87500000409675494 ) ) ;
#15820 = DIRECTION ( 'NONE',  ( -0.000000000000000000, -0.000000000000000000, 1.000000000000000000 ) ) ;
#15821 = CARTESIAN_POINT ( 'NONE',  ( -10.81189881249999907, -6.242252689847864744, -62.15625000204838102 ) ) ;
#15822 = CARTESIAN_POINT ( 'NONE',  ( -10.00000000000154188, 5.773502691895366468, -83.87499999999992895 ) ) ;
#15823 = CARTESIAN_POINT ( 'NONE',  ( -5.405949406249996869, 9.363379034771805109, -172.0312500020484094 ) ) ;
#15824 = CARTESIAN_POINT ( 'NONE',  ( 9.999999999999998224, 0.000000000000000000, -134.3750000040967905 ) ) ;
#15825 = CYLINDRICAL_SURFACE ( 'NONE', #4806, 9.999999999999998224 ) ;
#15826 = ORIENTED_EDGE ( 'NONE', *, *, #42633, .F. ) ;
#15827 = FACE_OUTER_BOUND ( 'NONE', #35717, .T. ) ;
#15828 = CARTESIAN_POINT ( 'NONE',  ( 9.999999999999998224, 0.000000000000000000, -70.99999999999998579 ) ) ;
#15830 = VERTEX_POINT ( 'NONE', #15824 ) ;
#15829 = CARTESIAN_POINT ( 'NONE',  ( -10.81189881249999729, 6.242252689847871849, -77.40625000204838102 ) ) ;
#15831 = EDGE_LOOP ( 'NONE', ( #39761, #3073, #15838 ) ) ;
#15832 = VERTEX_POINT ( 'NONE', #38091 ) ;
#15833 = CARTESIAN_POINT ( 'NONE',  ( 10.81189881249999551, -6.242252689847874514, -28.46875000204837036 ) ) ;
#15834 = CARTESIAN_POINT ( 'NONE',  ( 9.999999999999479527, 5.773502691896553074, -126.7500000040967478 ) ) ;
#15835 = CARTESIAN_POINT ( 'NONE',  ( -10.81189881249999729, 6.242252689847871849, -9.906250002048379244 ) ) ;
#15836 = CIRCLE ( 'NONE', #39980, 5.000000000000002665 ) ;
#15838 = ORIENTED_EDGE ( 'NONE', *, *, #15572, .F. ) ;
#15837 = CARTESIAN_POINT ( 'NONE',  ( -2.293366432827344421E-15, -12.48450537969573659, -58.71875000204836681 ) ) ;
#15839 = CARTESIAN_POINT ( 'NONE',  ( -9.999999999999227285, -5.773502691896698735, -109.5000000040967478 ) ) ;
#15840 = CARTESIAN_POINT ( 'NONE',  ( 10.00000000000000000, 5.773502691896255534, -25.87499999999998224 ) ) ;
#15841 = CARTESIAN_POINT ( 'NONE',  ( -5.405949406249996869, 9.363379034771805109, -186.8437500020483810 ) ) ;
#15842 = CARTESIAN_POINT ( 'NONE',  ( 5.405949406249992428, -9.363379034771808662, -178.5937500020484094 ) ) ;
#15843 = CARTESIAN_POINT ( 'NONE',  ( 5.405949406249999534, 9.363379034771803333, -160.0937500020484094 ) ) ;
#15844 = CARTESIAN_POINT ( 'NONE',  ( 5.405949406249992428, -9.363379034771808662, -172.5937500020484094 ) ) ;
#15845 = CARTESIAN_POINT ( 'NONE',  ( 9.999999999999742428, 5.773502691896404748, -124.8749999999999858 ) ) ;
#15846 = CARTESIAN_POINT ( 'NONE',  ( -9.999999999999998224, 1.224646799147353059E-15, -127.2499999999999716 ) ) ;
#15847 = CARTESIAN_POINT ( 'NONE',  ( -10.00000000000000000, -5.773502691896251982, -185.6250000000000284 ) ) ;
#15848 = CARTESIAN_POINT ( 'NONE',  ( 10.81189881249999729, 0.000000000000000000, -107.8437500020483810 ) ) ;
#15849 = DIRECTION ( 'NONE',  ( 1.000000000000000000, 0.000000000000000000, -0.000000000000000000 ) ) ;
#15850 = CARTESIAN_POINT ( 'NONE',  ( 5.405949406249992428, -9.363379034771808662, -75.28125000204838102 ) ) ;
#15851 = CARTESIAN_POINT ( 'NONE',  ( 4.999999999999992006, -8.660254037844389075, -159.7500000000000000 ) ) ;
#15852 = EDGE_CURVE ( 'NONE', #14676, #19099, #28176, .T. ) ;
#15853 = CARTESIAN_POINT ( 'NONE',  ( -5.405949406249996869, 9.363379034771805109, -84.84375000204836681 ) ) ;
#15854 = EDGE_CURVE ( 'NONE', #5830, #15993, #29830, .T. ) ;
#15855 = CARTESIAN_POINT ( 'NONE',  ( 5.405949406249992428, -9.363379034771808662, -60.28125000204836681 ) ) ;
#15856 = CARTESIAN_POINT ( 'NONE',  ( 9.999999999999998224, 0.000000000000000000, -144.8750000040967905 ) ) ;
#15857 = CARTESIAN_POINT ( 'NONE',  ( -9.999999999999998224, 1.224646799147353059E-15, -124.2500000000000000 ) ) ;
#15858 = ORIENTED_EDGE ( 'NONE', *, *, #35195, .T. ) ;
#15859 = CARTESIAN_POINT ( 'NONE',  ( -2.293366432827344421E-15, -12.48450537969573659, -139.9062500020484094 ) ) ;
#15860 = CARTESIAN_POINT ( 'NONE',  ( 5.405949406249992428, -9.363379034771808662, -154.7812500020484094 ) ) ;
#15861 = CARTESIAN_POINT ( 'NONE',  ( -5.405949406249996869, 9.363379034771805109, -193.0312500020484094 ) ) ;
#15862 = CARTESIAN_POINT ( 'NONE',  ( 5.405949406249999534, 9.363379034771803333, -92.59375000204838102 ) ) ;
#15863 = ORIENTED_EDGE ( 'NONE', *, *, #19093, .T. ) ;
#15864 = CARTESIAN_POINT ( 'NONE',  ( -9.999999999999998224, 5.773502691896259087, -64.37499999999998579 ) ) ;
#15865 = CARTESIAN_POINT ( 'NONE',  ( 10.81189881249999729, 0.000000000000000000, -187.3437500020483810 ) ) ;
#15866 = CARTESIAN_POINT ( 'NONE',  ( 7.070501591499377789E-16, 11.54700538379251284, -72.50000000409676204 ) ) ;
#15867 = DIRECTION ( 'NONE',  ( -0.000000000000000000, -0.000000000000000000, -1.000000000000000000 ) ) ;
#15868 = CARTESIAN_POINT ( 'NONE',  ( -2.293366432827344421E-15, -12.48450537969573659, -87.40625000204838102 ) ) ;
#15869 = CARTESIAN_POINT ( 'NONE',  ( -10.81189881249999729, 6.242252689847871849, -63.90625000204837391 ) ) ;
#15870 = CARTESIAN_POINT ( 'NONE',  ( -10.00000000000000000, -5.773502691896251982, -61.50000000409677625 ) ) ;
#15871 = CARTESIAN_POINT ( 'NONE',  ( -5.405949406249996869, 9.363379034771805109, -14.34375000204834905 ) ) ;
#15872 = VERTEX_POINT ( 'NONE', #5080 ) ;
#15873 = CARTESIAN_POINT ( 'NONE',  ( 7.644554776091147741E-16, 12.48450537969573659, -194.6562500020484094 ) ) ;
#15874 =( GEOMETRIC_REPRESENTATION_CONTEXT ( 3 ) GLOBAL_UNCERTAINTY_ASSIGNED_CONTEXT ( ( #23403 ) ) GLOBAL_UNIT_ASSIGNED_CONTEXT ( ( #11537, #34664, #18234 ) ) REPRESENTATION_CONTEXT ( 'NONE', 'WORKASPACE' ) );
#15875 = CARTESIAN_POINT ( 'NONE',  ( -10.81189881249999729, 6.242252689847871849, -8.406250002048365033 ) ) ;
#15876 = CARTESIAN_POINT ( 'NONE',  ( 10.81189881249999729, 6.242252689847867408, -7.218750002048349934 ) ) ;
#15877 = DIRECTION ( 'NONE',  ( 0.000000000000000000, -1.000000000000000000, 0.000000000000000000 ) ) ;
#15878 = CARTESIAN_POINT ( 'NONE',  ( 9.999999999999998224, 0.000000000000000000, -45.49999999999998579 ) ) ;
#15879 = DIRECTION ( 'NONE',  ( -0.000000000000000000, -0.000000000000000000, 1.000000000000000000 ) ) ;
#15880 = CARTESIAN_POINT ( 'NONE',  ( 9.999999999999996447, -5.773502691896262640, -177.6250000000000000 ) ) ;
#15881 = CARTESIAN_POINT ( 'NONE',  ( -9.999999999999998224, 1.224646799147353059E-15, -166.2500000000000000 ) ) ;
#15883 = ORIENTED_EDGE ( 'NONE', *, *, #4816, .F. ) ;
#15882 = CARTESIAN_POINT ( 'NONE',  ( 5.405949406249992428, -9.363379034771808662, -100.7812500020483952 ) ) ;
#15884 = CARTESIAN_POINT ( 'NONE',  ( -4.999999999999996447, 8.660254037844387298, -37.49999999999997868 ) ) ;
#15885 = EDGE_CURVE ( 'NONE', #18018, #42167, #35878, .T. ) ;
#15886 = ORIENTED_EDGE ( 'NONE', *, *, #23177, .F. ) ;
#15887 = ORIENTED_EDGE ( 'NONE', *, *, #7580, .T. ) ;
#15888 = CARTESIAN_POINT ( 'NONE',  ( 10.81189881249999907, 6.242252689847868297, -31.40625000204834905 ) ) ;
#15889 = APPROVAL_ROLE ( '' ) ;
#15890 = CARTESIAN_POINT ( 'NONE',  ( 5.405949406249992428, -9.363379034771808662, -76.59375000204838102 ) ) ;
#15891 = CARTESIAN_POINT ( 'NONE',  ( 9.999999999999998224, 0.000000000000000000, -180.5000000000000000 ) ) ;
#15892 = DIRECTION ( 'NONE',  ( 0.7071067811865463515, 8.659560562354918067E-17, -0.7071067811865487940 ) ) ;
#15893 = CARTESIAN_POINT ( 'NONE',  ( 10.00000000000025402, -5.773502691896113426, -130.0000000040967905 ) ) ;
#15894 = LINE ( 'NONE', #11447, #30876 ) ;
#15895 = CARTESIAN_POINT ( 'NONE',  ( 10.81189881249999907, 6.242252689847868297, -158.9062500020483810 ) ) ;
#15896 = CARTESIAN_POINT ( 'NONE',  ( -9.999999999999998224, 5.773502691896259087, -15.25000000409676737 ) ) ;
#15897 = FACE_OUTER_BOUND ( 'NONE', #23241, .T. ) ;
#15898 = AXIS2_PLACEMENT_3D ( 'NONE', #28611, #22545, #41745 ) ;
#15899 = CARTESIAN_POINT ( 'NONE',  ( -10.81189881249999729, 6.242252689847871849, -126.7187500020483952 ) ) ;
#15900 = CARTESIAN_POINT ( 'NONE',  ( 10.81189881249999729, 0.000000000000000000, -100.5312500020483952 ) ) ;
#15901 = EDGE_CURVE ( 'NONE', #6715, #13020, #42160, .T. ) ;
#15902 = CARTESIAN_POINT ( 'NONE',  ( 10.81189881249999551, -6.242252689847874514, -104.9687500020483810 ) ) ;
#15903 = CARTESIAN_POINT ( 'NONE',  ( 7.644554776091147741E-16, 12.48450537969573659, -75.96875000204838102 ) ) ;
#15904 = CARTESIAN_POINT ( 'NONE',  ( 5.405949406249999534, 9.363379034771803333, -86.78125000204838102 ) ) ;
#15905 = CARTESIAN_POINT ( 'NONE',  ( -2.121150477449813534E-15, -11.54700538379251284, -166.2500000040968189 ) ) ;
#15906 =( BOUNDED_CURVE ( )  B_SPLINE_CURVE ( 2, ( #18264, #8780, #27781, #21937, #40916, #14801, #35117 ),
 .UNSPECIFIED., .F., .F. ) 
 B_SPLINE_CURVE_WITH_KNOTS ( ( 3, 2, 2, 3 ),
 ( 0.5000000000000001110, 0.5012437810945274963, 0.5024875621890548816, 0.5037313432835821558 ),
 .UNSPECIFIED. ) 
 CURVE ( )  GEOMETRIC_REPRESENTATION_ITEM ( )  RATIONAL_B_SPLINE_CURVE ( ( 0.9999999999999880096, 0.8660254037844506980, 1.000000000000000000, 0.8660254037844387076, 1.000000000000000000, 0.8660254037844267172, 1.000000000000011990 ) ) 
 REPRESENTATION_ITEM ( '' )  );
#15907 = EDGE_CURVE ( 'NONE', #26894, #9613, #15432, .T. ) ;
#15908 = CARTESIAN_POINT ( 'NONE',  ( 0.000000000000000000, 0.000000000000000000, -200.0000000000000000 ) ) ;
#15909 = CARTESIAN_POINT ( 'NONE',  ( 10.81189881249999729, 0.000000000000000000, -168.0312500020484094 ) ) ;
#15910 = CARTESIAN_POINT ( 'NONE',  ( 7.644554776091147741E-16, 12.48450537969573659, -178.1562500020484094 ) ) ;
#15911 = EDGE_CURVE ( 'NONE', #19609, #37214, #36335, .T. ) ;
#15912 = CARTESIAN_POINT ( 'NONE',  ( 9.999999999999996447, -5.773502691896262640, -152.5000000040967905 ) ) ;
#15913 = CARTESIAN_POINT ( 'NONE',  ( -5.405949406249996869, 9.363379034771805109, 0.4687499979516285276 ) ) ;
#15914 = CARTESIAN_POINT ( 'NONE',  ( -10.81189881249999729, 6.242252689847871849, -2.218750002048353043 ) ) ;
#15915 = CARTESIAN_POINT ( 'NONE',  ( -10.00000000000012434, 5.773502691896184480, -162.2500000040967905 ) ) ;
#15916 = CARTESIAN_POINT ( 'NONE',  ( 7.644554776091147741E-16, 12.48450537969573659, -113.4687500020483952 ) ) ;
#15917 = CARTESIAN_POINT ( 'NONE',  ( -4.999999999999996447, 8.660254037844387298, -92.99999999999998579 ) ) ;
#15918 = CARTESIAN_POINT ( 'NONE',  ( 5.405949406249999534, 9.363379034771803333, -11.78125000204835438 ) ) ;
#15919 = CARTESIAN_POINT ( 'NONE',  ( 7.070501591499377789E-16, 11.54700538379251284, -96.50000000409679046 ) ) ;
#15920 = FACE_OUTER_BOUND ( 'NONE', #5623, .T. ) ;
#15921 = PRODUCT_DEFINITION ( 'UNKNOWN', '', #36593, #6283 ) ;
#15922 = CARTESIAN_POINT ( 'NONE',  ( 5.405949406249992428, -9.363379034771808662, -111.2812500020483810 ) ) ;
#15923 = CARTESIAN_POINT ( 'NONE',  ( 10.81189881249999551, -6.242252689847874514, -93.15625000204838102 ) ) ;
#15924 = VERTEX_POINT ( 'NONE', #13642 ) ;
#15925 = CARTESIAN_POINT ( 'NONE',  ( 5.000000000000000000, 8.660254037844385522, -84.62500000409677625 ) ) ;
#15926 = CARTESIAN_POINT ( 'NONE',  ( -9.999999999999998224, 1.224646799147353059E-15, -101.7500000000000000 ) ) ;
#15927 = CARTESIAN_POINT ( 'NONE',  ( 10.81189881249999907, 6.242252689847868297, -38.71875000204835260 ) ) ;
#15928 = ORIENTED_EDGE ( 'NONE', *, *, #31528, .F. ) ;
#15929 = CARTESIAN_POINT ( 'NONE',  ( 10.00000000000000000, 5.773502691896255534, -19.87499999999996803 ) ) ;
#15930 = CARTESIAN_POINT ( 'NONE',  ( 9.999999999999996447, -5.773502691896262640, -155.1250000000000000 ) ) ;
#15931 = EDGE_CURVE ( 'NONE', #32336, #5197, #16884, .T. ) ;
#15932 = CARTESIAN_POINT ( 'NONE',  ( 10.00000000000000000, 5.773502691896255534, -17.25000000409676559 ) ) ;
#15933 = EDGE_CURVE ( 'NONE', #22272, #23552, #16647, .T. ) ;
#15934 = AXIS2_PLACEMENT_3D ( 'NONE', #38085, #40872, #5499 ) ;
#15935 = CC_DESIGN_APPROVAL ( #19346, ( #27668 ) ) ;
#15936 = CARTESIAN_POINT ( 'NONE',  ( -9.999999999999998224, 1.224646799147353059E-15, -194.7500000000000000 ) ) ;
#15938 = ORIENTED_EDGE ( 'NONE', *, *, #4445, .F. ) ;
#15937 = CARTESIAN_POINT ( 'NONE',  ( -5.405949406249996869, 9.363379034771805109, -122.5312500020483952 ) ) ;
#15939 = CARTESIAN_POINT ( 'NONE',  ( -4.999999999999996447, 8.660254037844387298, -64.87500000409676204 ) ) ;
#15940 = ORIENTED_EDGE ( 'NONE', *, *, #39110, .F. ) ;
#15941 = CARTESIAN_POINT ( 'NONE',  ( -2.293366432827344421E-15, -12.48450537969573659, -52.90625000204837391 ) ) ;
#15942 = APPROVAL_STATUS ( 'not_yet_approved' ) ;
#15943 = VECTOR ( 'NONE', #37227, 1000.000000000000000 ) ;
#15944 = CARTESIAN_POINT ( 'NONE',  ( -10.81189881249999907, -6.242252689847864744, -102.4687500020483810 ) ) ;
#15946 = ORIENTED_EDGE ( 'NONE', *, *, #7249, .F. ) ;
#15945 = EDGE_LOOP ( 'NONE', ( #28396, #14233, #4117, #33315 ) ) ;
#15947 = CARTESIAN_POINT ( 'NONE',  ( 10.00000000000051159, -5.773502691895965988, -175.0000000040968189 ) ) ;
#15948 = CARTESIAN_POINT ( 'NONE',  ( -4.999999999999996447, 8.660254037844387298, -32.99999999999997158 ) ) ;
#15949 = CARTESIAN_POINT ( 'NONE',  ( -5.405949406250003975, -9.363379034771801557, -183.5312500020484094 ) ) ;
#15950 = CARTESIAN_POINT ( 'NONE',  ( -10.81189881249999729, 6.242252689847871849, -2.218750002048357928 ) ) ;
#15951 = CARTESIAN_POINT ( 'NONE',  ( -2.121150477449813534E-15, -11.54700538379251284, -132.8750000000000000 ) ) ;
#15952 = CARTESIAN_POINT ( 'NONE',  ( 7.644554776091147741E-16, 12.48450537969573659, -141.9687500020483810 ) ) ;
#15953 = B_SPLINE_CURVE_WITH_KNOTS ( 'NONE', 3,
 ( #23023, #16515, #32534, #42637, #22810, #26051 ),
 .UNSPECIFIED., .F., .F.,
 ( 4, 2, 4 ),
 ( 0.9171367075385271628, 0.9585683537692635259, 1.000000000000000000 ),
 .UNSPECIFIED. ) ;
#15954 = CARTESIAN_POINT ( 'NONE',  ( 10.81189881249999551, -6.242252689847874514, -101.9687500020483810 ) ) ;
#15955 = CARTESIAN_POINT ( 'NONE',  ( 9.999999999999998224, 0.000000000000000000, -147.5000000000000000 ) ) ;
#15956 = CARTESIAN_POINT ( 'NONE',  ( -5.405949406249996869, 9.363379034771805109, -106.0312500020483810 ) ) ;
#15957 = CARTESIAN_POINT ( 'NONE',  ( 9.999999999999996447, -5.773502691896262640, -194.5000000040968189 ) ) ;
#15958 = CARTESIAN_POINT ( 'NONE',  ( -5.405949406250003975, -9.363379034771801557, -123.3437500020483952 ) ) ;
#15959 = VECTOR ( 'NONE', #38648, 1000.000000000000114 ) ;
#15960 = CARTESIAN_POINT ( 'NONE',  ( -5.405949406250003975, -9.363379034771801557, -188.0312500020484094 ) ) ;
#15961 = CARTESIAN_POINT ( 'NONE',  ( -2.121150477449813534E-15, -11.54700538379251284, -95.37500000000000000 ) ) ;
#15962 = CARTESIAN_POINT ( 'NONE',  ( -10.00000000000000000, -5.773502691896251982, -140.6249999999999716 ) ) ;
#15963 = CARTESIAN_POINT ( 'NONE',  ( -2.121150477449813534E-15, -11.54700538379251284, -3.874999999999961808 ) ) ;
#15964 = CARTESIAN_POINT ( 'NONE',  ( -10.81189881249999729, 6.242252689847871849, -66.71875000204838102 ) ) ;
#15965 = CARTESIAN_POINT ( 'NONE',  ( -5.405949406249996869, 9.363379034771805109, -48.84375000204838102 ) ) ;
#15966 = CARTESIAN_POINT ( 'NONE',  ( -4.999999999999996447, 8.660254037844387298, -178.8750000040967905 ) ) ;
#15967 = CARTESIAN_POINT ( 'NONE',  ( 5.405949406249992428, -9.363379034771808662, -27.28125000204836681 ) ) ;
#15968 = CARTESIAN_POINT ( 'NONE',  ( 5.405949406249992428, -9.363379034771808662, -28.59375000204836326 ) ) ;
#15969 = CARTESIAN_POINT ( 'NONE',  ( -5.000000000000003553, -8.660254037844383745, -142.3750000040967905 ) ) ;
#15970 = CARTESIAN_POINT ( 'NONE',  ( 10.81189881249999729, 0.000000000000000000, -140.8437500020483810 ) ) ;
#15971 = CARTESIAN_POINT ( 'NONE',  ( -5.000000000000003553, -8.660254037844383745, -114.9999999999999858 ) ) ;
#15972 = CYLINDRICAL_SURFACE ( 'NONE', #20342, 9.999999999999998224 ) ;
#15973 = CARTESIAN_POINT ( 'NONE',  ( 5.000000000000000000, 8.660254037844385522, -70.74999999999998579 ) ) ;
#15974 = CARTESIAN_POINT ( 'NONE',  ( -10.81189881249999729, 1.324075727343319199E-15, -131.2812500020483810 ) ) ;
#15975 = CARTESIAN_POINT ( 'NONE',  ( -10.81189881249999729, -6.242252689847864744, -117.6562500020483952 ) ) ;
#15976 = ORIENTED_EDGE ( 'NONE', *, *, #28450, .T. ) ;
#15977 = CARTESIAN_POINT ( 'NONE',  ( 9.999999999999998224, 0.000000000000000000, -197.3750000040967905 ) ) ;
#15978 = CARTESIAN_POINT ( 'NONE',  ( 10.00000000000000000, 5.773502691896255534, -114.7500000040967763 ) ) ;
#15979 = CARTESIAN_POINT ( 'NONE',  ( 4.999999999999992006, -8.660254037844389075, -128.2499999999999716 ) ) ;
#15980 = CARTESIAN_POINT ( 'NONE',  ( -5.405949406249996869, 9.363379034771805109, -62.34375000204836681 ) ) ;
#15981 = CARTESIAN_POINT ( 'NONE',  ( -9.999999999999998224, 5.773502691896259087, -44.87499999999997868 ) ) ;
#15982 = AXIS2_PLACEMENT_3D ( 'NONE', #22969, #96, #15091 ) ;
#15983 = EDGE_CURVE ( 'NONE', #437, #22331, #35712, .T. ) ;
#15984 = CARTESIAN_POINT ( 'NONE',  ( -4.999999999999996447, 8.660254037844387298, -25.87500000409675849 ) ) ;
#15985 = CARTESIAN_POINT ( 'NONE',  ( 7.644554776091147741E-16, 12.48450537969573659, -40.15625000204835260 ) ) ;
#15986 = CARTESIAN_POINT ( 'NONE',  ( -9.999999999999998224, 1.224646799147353059E-15, -46.62500000409677625 ) ) ;
#15987 = CARTESIAN_POINT ( 'NONE',  ( 5.405949406249999534, 9.363379034771803333, -32.78125000204837391 ) ) ;
#15988 = DIRECTION ( 'NONE',  ( -0.000000000000000000, -0.000000000000000000, -1.000000000000000000 ) ) ;
#15989 = CARTESIAN_POINT ( 'NONE',  ( 5.405949406249999534, 9.363379034771803333, -133.2812500020483810 ) ) ;
#15990 = CARTESIAN_POINT ( 'NONE',  ( 5.405949406249992428, -9.363379034771808662, -148.7812500020483810 ) ) ;
#15991 = CARTESIAN_POINT ( 'NONE',  ( -2.121150477449813534E-15, -11.54700538379251284, -65.37499999999998579 ) ) ;
#15992 = CARTESIAN_POINT ( 'NONE',  ( -5.000000000000003553, -8.660254037844383745, -124.0000000000000000 ) ) ;
#15993 = VERTEX_POINT ( 'NONE', #13219 ) ;
#15994 = ORIENTED_EDGE ( 'NONE', *, *, #29097, .T. ) ;
#15995 = VERTEX_POINT ( 'NONE', #36125 ) ;
#15996 =( BOUNDED_CURVE ( )  B_SPLINE_CURVE ( 2, ( #34083, #36880, #31283, #30633, #27171, #37739, #40523 ),
 .UNSPECIFIED., .F., .F. ) 
 B_SPLINE_CURVE_WITH_KNOTS ( ( 3, 2, 2, 3 ),
 ( 0.3022388059701494045, 0.3034825870646767343, 0.3047263681592040085, 0.3059701492537313383 ),
 .UNSPECIFIED. ) 
 CURVE ( )  GEOMETRIC_REPRESENTATION_ITEM ( )  RATIONAL_B_SPLINE_CURVE ( ( 0.9999999999999820144, 0.8660254037844566932, 1.000000000000000000, 0.8660254037844387076, 1.000000000000000000, 0.8660254037844387076, 1.000000000000000000 ) ) 
 REPRESENTATION_ITEM ( '' )  );
#15997 = CARTESIAN_POINT ( 'NONE',  ( 10.00000000000000000, 5.773502691896255534, -135.7500000040967905 ) ) ;
#15998 = CARTESIAN_POINT ( 'NONE',  ( 5.405949406249999534, 9.363379034771803333, -172.0937500020484094 ) ) ;
#15999 = CARTESIAN_POINT ( 'NONE',  ( 7.644554776091147741E-16, 12.48450537969573659, -29.46875000204835970 ) ) ;
#16000 = CARTESIAN_POINT ( 'NONE',  ( -2.121150477449813534E-15, -11.54700538379251284, -128.7500000040967905 ) ) ;
#16001 = CARTESIAN_POINT ( 'NONE',  ( 5.405949406249999534, 9.363379034771803333, -161.5937500020484094 ) ) ;
#16002 = CARTESIAN_POINT ( 'NONE',  ( -10.81189881249999729, 1.324075727343319199E-15, -149.0937500020483810 ) ) ;
#16003 = LINE ( 'NONE', #19052, #7280 ) ;
#16004 = CARTESIAN_POINT ( 'NONE',  ( -5.405949406250003975, -9.363379034771801557, -124.8437500020483810 ) ) ;
#16005 = CARTESIAN_POINT ( 'NONE',  ( -5.405949406250003975, -9.363379034771801557, -132.5312500020484094 ) ) ;
#16006 = CARTESIAN_POINT ( 'NONE',  ( 5.405949406249999534, 9.363379034771803333, -17.59375000204835260 ) ) ;
#16007 = CARTESIAN_POINT ( 'NONE',  ( -10.81189881249999729, 6.242252689847871849, -147.7187500020484094 ) ) ;
#16008 = CARTESIAN_POINT ( 'NONE',  ( 0.000000000000000000, 0.000000000000000000, -200.0000000000000000 ) ) ;
#16009 = CARTESIAN_POINT ( 'NONE',  ( 9.999999999999479527, 5.773502691896553074, -44.25000000409674783 ) ) ;
#16010 = CARTESIAN_POINT ( 'NONE',  ( -10.00000000000000000, -5.773502691896251982, -166.1249999999999716 ) ) ;
#16011 = CARTESIAN_POINT ( 'NONE',  ( -5.405949406250003975, -9.363379034771801557, -0.5312500020483723606 ) ) ;
#16012 = CARTESIAN_POINT ( 'NONE',  ( 10.81189881249999551, -6.242252689847874514, -71.96875000204838102 ) ) ;
#16013 = CARTESIAN_POINT ( 'NONE',  ( 7.644554776091147741E-16, 12.48450537969573659, -49.15625000204837391 ) ) ;
#16014 = CARTESIAN_POINT ( 'NONE',  ( -5.405949406250003975, -9.363379034771801557, -63.34375000204836681 ) ) ;
#16015 = CARTESIAN_POINT ( 'NONE',  ( 9.999999999999998224, 1.224646799147353059E-15, -99.99999999999998579 ) ) ;
#16016 = CARTESIAN_POINT ( 'NONE',  ( -10.81189881249999907, -6.242252689847864744, -160.9687500020484094 ) ) ;
#16017 = CARTESIAN_POINT ( 'NONE',  ( -5.000000000000003553, -8.660254037844383745, -140.5000000000000000 ) ) ;
#16018 = CARTESIAN_POINT ( 'NONE',  ( -2.293366432827344421E-15, -12.48450537969573659, -150.4062500020484379 ) ) ;
#16019 = LINE ( 'NONE', #12787, #9614 ) ;
#16020 = CARTESIAN_POINT ( 'NONE',  ( -2.121150477449813534E-15, -11.54700538379251284, -115.2500000040967763 ) ) ;
#16021 = CARTESIAN_POINT ( 'NONE',  ( -10.00000000000000000, -5.773502691896251982, -91.12499999999998579 ) ) ;
#16022 = ORIENTED_EDGE ( 'NONE', *, *, #15002, .F. ) ;
#16023 = CARTESIAN_POINT ( 'NONE',  ( -10.81189881249999729, 1.324075727343319199E-15, -114.7812500020483952 ) ) ;
#16024 = CARTESIAN_POINT ( 'NONE',  ( 9.999999999999998224, 0.000000000000000000, -138.8750000040968189 ) ) ;
#16025 = FACE_OUTER_BOUND ( 'NONE', #21810, .T. ) ;
#16026 = CARTESIAN_POINT ( 'NONE',  ( 7.644554776091147741E-16, 12.48450537969573659, -172.1562500020484094 ) ) ;
#16027 = CARTESIAN_POINT ( 'NONE',  ( -9.999999999999998224, 5.773502691896259087, -51.25000000409676915 ) ) ;
#16028 = ADVANCED_BREP_SHAPE_REPRESENTATION ( '', ( #29947, #39998 ), #11785 ) ;
#16029 = DIRECTION ( 'NONE',  ( 0.4999999999999997224, 0.8660254037844388186, 0.000000000000000000 ) ) ;
#16030 = CARTESIAN_POINT ( 'NONE',  ( -10.81189881249999907, -6.242252689847864744, -63.65625000204838102 ) ) ;
#16031 = CARTESIAN_POINT ( 'NONE',  ( 9.999999999999998224, 0.000000000000000000, -156.5000000000000000 ) ) ;
#16032 = CARTESIAN_POINT ( 'NONE',  ( -10.81189881249999729, 6.242252689847871849, -164.4062500020484094 ) ) ;
#16033 = CARTESIAN_POINT ( 'NONE',  ( 10.81189881249999907, 6.242252689847868297, -140.7187500020483810 ) ) ;
#16034 = CARTESIAN_POINT ( 'NONE',  ( 0.000000000000000000, 0.000000000000000000, -200.0000000000000000 ) ) ;
#16035 = CARTESIAN_POINT ( 'NONE',  ( 9.999999999999998224, 0.000000000000000000, -55.99999999999996447 ) ) ;
#16036 = VERTEX_POINT ( 'NONE', #3535 ) ;
#16037 = FACE_OUTER_BOUND ( 'NONE', #6657, .T. ) ;
#16038 = EDGE_CURVE ( 'NONE', #6564, #5725, #38643, .T. ) ;
#16039 =( BOUNDED_CURVE ( )  B_SPLINE_CURVE ( 2, ( #31798, #34599, #31150, #37608, #2229, #41034, #8051 ),
 .UNSPECIFIED., .F., .F. ) 
 B_SPLINE_CURVE_WITH_KNOTS ( ( 3, 2, 2, 3 ),
 ( 0.3432835820895522860, 0.3445273631840797268, 0.3457711442786070566, 0.3470149253731344974 ),
 .UNSPECIFIED. ) 
 CURVE ( )  GEOMETRIC_REPRESENTATION_ITEM ( )  RATIONAL_B_SPLINE_CURVE ( ( 0.9999999999999940048, 0.8660254037844447028, 1.000000000000000000, 0.8660254037844387076, 1.000000000000000000, 0.8660254037844207220, 1.000000000000017986 ) ) 
 REPRESENTATION_ITEM ( '' )  );
#16041 = VERTEX_POINT ( 'NONE', #19712 ) ;
#16040 = CARTESIAN_POINT ( 'NONE',  ( 10.81189881249999729, 0.000000000000000000, -66.03125000204838102 ) ) ;
#16042 = PERSON_AND_ORGANIZATION_ROLE ( 'classification_officer' ) ;
#16044 = ORIENTED_EDGE ( 'NONE', *, *, #17790, .T. ) ;
#16043 = CARTESIAN_POINT ( 'NONE',  ( -10.81189881249999729, 6.242252689847871849, -119.2187500020483810 ) ) ;
#16045 = VERTEX_POINT ( 'NONE', #13428 ) ;
#16046 = CARTESIAN_POINT ( 'NONE',  ( -10.81189881249999729, -6.242252689847864744, -27.46875000204838102 ) ) ;
#16047 = DIRECTION ( 'NONE',  ( -1.000000000000000000, 0.000000000000000000, 0.000000000000000000 ) ) ;
#16048 = CARTESIAN_POINT ( 'NONE',  ( -10.81189881249999907, -6.242252689847864744, -196.9687500020484379 ) ) ;
#16049 =( BOUNDED_CURVE ( )  B_SPLINE_CURVE ( 2, ( #41138, #8156, #20874, #21304, #34060, #37929, #17624 ),
 .UNSPECIFIED., .F., .F. ) 
 B_SPLINE_CURVE_WITH_KNOTS ( ( 3, 2, 2, 3 ),
 ( 0.6977611940298510396, 0.6990049751243784248, 0.7002487562189056991, 0.7014925373134330844 ),
 .UNSPECIFIED. ) 
 CURVE ( )  GEOMETRIC_REPRESENTATION_ITEM ( )  RATIONAL_B_SPLINE_CURVE ( ( 0.9999999999999641398, 0.8660254037844745678, 1.000000000000000000, 0.8660254037844387076, 1.000000000000000000, 0.8660254037844148378, 1.000000000000023981 ) ) 
 REPRESENTATION_ITEM ( '' )  );
#16050 = CARTESIAN_POINT ( 'NONE',  ( 5.405949406249999534, 9.363379034771803333, -58.09375000204835970 ) ) ;
#16051 = CARTESIAN_POINT ( 'NONE',  ( -9.999999999999998224, 1.224646799147353059E-15, -172.6250000040968189 ) ) ;
#16052 = CARTESIAN_POINT ( 'NONE',  ( 9.999999999999996447, -5.773502691896262640, -30.62499999999995737 ) ) ;
#16053 = CARTESIAN_POINT ( 'NONE',  ( -10.81189881249999729, 6.242252689847871849, -188.2187500020484379 ) ) ;
#16054 = CARTESIAN_POINT ( 'NONE',  ( -10.81189881249999729, 1.324075727343319199E-15, -173.0937500020484094 ) ) ;
#16055 = CARTESIAN_POINT ( 'NONE',  ( 5.405949406249999534, 9.363379034771803333, -148.0937500020483810 ) ) ;
#16056 = CARTESIAN_POINT ( 'NONE',  ( -10.81189881249999729, -6.242252689847864744, -172.9687500020483526 ) ) ;
#16057 = CARTESIAN_POINT ( 'NONE',  ( -2.121150477449813534E-15, -11.54700538379251284, -75.87500000000000000 ) ) ;
#16058 = CARTESIAN_POINT ( 'NONE',  ( 9.999999999999998224, 0.000000000000000000, -176.3750000040967905 ) ) ;
#16059 = CARTESIAN_POINT ( 'NONE',  ( 9.999999999999996447, -5.773502691896262640, -188.1250000000000284 ) ) ;
#16060 = CARTESIAN_POINT ( 'NONE',  ( -5.405949406250003975, -9.363379034771801557, -94.84375000204838102 ) ) ;
#16061 = CARTESIAN_POINT ( 'NONE',  ( 9.999999999999998224, 0.000000000000000000, -18.49999999999996092 ) ) ;
#16062 = CARTESIAN_POINT ( 'NONE',  ( -5.405949406249996869, 9.363379034771805109, -73.03125000204838102 ) ) ;
#16063 = CARTESIAN_POINT ( 'NONE',  ( 9.999999999999998224, 0.000000000000000000, -159.5000000000000000 ) ) ;
#16064 = CARTESIAN_POINT ( 'NONE',  ( -2.293366432827344421E-15, -12.48450537969573659, -195.2187500020484094 ) ) ;
#16065 = CARTESIAN_POINT ( 'NONE',  ( -10.81189881249999729, 1.324075727343319199E-15, -87.59375000204836681 ) ) ;
#16066 = CARTESIAN_POINT ( 'NONE',  ( 5.405949406249992428, -9.363379034771808662, -61.78125000204837391 ) ) ;
#16067 = CARTESIAN_POINT ( 'NONE',  ( -4.999999999999996447, 8.660254037844387298, -142.8750000040967905 ) ) ;
#16068 = CARTESIAN_POINT ( 'NONE',  ( -10.00000000000000000, -5.773502691896251982, -112.1249999999999858 ) ) ;
#16069 = ORIENTED_EDGE ( 'NONE', *, *, #6218, .T. ) ;
#16070 = CARTESIAN_POINT ( 'NONE',  ( 7.644554776091147741E-16, 12.48450537969573659, -143.6562500020484094 ) ) ;
#16071 = CARTESIAN_POINT ( 'NONE',  ( 5.405949406249992428, -9.363379034771808662, -153.2812500020484094 ) ) ;
#16072 = CARTESIAN_POINT ( 'NONE',  ( -10.81189881249999729, 6.242252689847871849, -197.4062500020484379 ) ) ;
#16073 = CYLINDRICAL_SURFACE ( 'NONE', #13006, 9.999999999999998224 ) ;
#16074 = CARTESIAN_POINT ( 'NONE',  ( -5.405949406249996869, 9.363379034771805109, -93.84375000204838102 ) ) ;
#16075 = ORIENTED_EDGE ( 'NONE', *, *, #26995, .F. ) ;
#16076 = CARTESIAN_POINT ( 'NONE',  ( -5.000000000000003553, -8.660254037844383745, -59.49999999999997158 ) ) ;
#16077 = CARTESIAN_POINT ( 'NONE',  ( -5.405949406250003975, -9.363379034771801557, -189.3437500020483810 ) ) ;
#16078 = CARTESIAN_POINT ( 'NONE',  ( 4.999999999999992006, -8.660254037844389075, -76.12500000409677625 ) ) ;
#16079 = CYLINDRICAL_SURFACE ( 'NONE', #39457, 9.999999999999998224 ) ;
#16080 = CARTESIAN_POINT ( 'NONE',  ( -2.293366432827344421E-15, -12.48450537969573659, -81.40625000204838102 ) ) ;
#16081 = CARTESIAN_POINT ( 'NONE',  ( -5.405949406249996869, 9.363379034771805109, -65.53125000204838102 ) ) ;
#16082 = CARTESIAN_POINT ( 'NONE',  ( -4.999999999999996447, 8.660254037844387298, -58.87500000409676204 ) ) ;
#16083 = CARTESIAN_POINT ( 'NONE',  ( 10.81189881249999551, -6.242252689847874514, -20.96875000204837036 ) ) ;
#16084 = CARTESIAN_POINT ( 'NONE',  ( -9.999999999999998224, 1.224646799147353059E-15, -156.1250000040967905 ) ) ;
#16085 = CARTESIAN_POINT ( 'NONE',  ( 10.81189881249999551, -6.242252689847874514, -190.6562500020484094 ) ) ;
#16086 = CARTESIAN_POINT ( 'NONE',  ( 10.81189881249999907, 6.242252689847868297, -10.40625000204836859 ) ) ;
#16087 = CYLINDRICAL_SURFACE ( 'NONE', #20088, 9.999999999999998224 ) ;
#16088 = FACE_OUTER_BOUND ( 'NONE', #19393, .T. ) ;
#16089 = CARTESIAN_POINT ( 'NONE',  ( 7.071067811865472841, -7.071067811865472841, -200.0000000000000000 ) ) ;
#16090 = DIRECTION ( 'NONE',  ( -0.000000000000000000, -0.000000000000000000, 1.000000000000000000 ) ) ;
#16091 = CARTESIAN_POINT ( 'NONE',  ( 4.999999999999992006, -8.660254037844389075, -173.2500000000000284 ) ) ;
#16092 = CARTESIAN_POINT ( 'NONE',  ( -4.999999999999996447, 8.660254037844387298, -97.49999999999998579 ) ) ;
#16094 = ORIENTED_EDGE ( 'NONE', *, *, #16994, .F. ) ;
#16093 = CARTESIAN_POINT ( 'NONE',  ( 7.644554776091147741E-16, 12.48450537969573659, -97.15625000204839523 ) ) ;
#16095 = CARTESIAN_POINT ( 'NONE',  ( -2.121150477449813534E-15, -11.54700538379251284, -164.3749999999999716 ) ) ;
#16096 = ADVANCED_FACE ( 'NONE', ( #26625 ), #16457, .T. ) ;
#16097 = ORIENTED_EDGE ( 'NONE', *, *, #11416, .T. ) ;
#16098 = VERTEX_POINT ( 'NONE', #39773 ) ;
#16099 = CARTESIAN_POINT ( 'NONE',  ( -2.293366432827344421E-15, -12.48450537969573659, -37.71875000204836681 ) ) ;
#16100 = CARTESIAN_POINT ( 'NONE',  ( 5.405949406249992428, -9.363379034771808662, -31.78125000204837391 ) ) ;
#16101 = PERSON_AND_ORGANIZATION ( #41262, #13183 ) ;
#16102 = CARTESIAN_POINT ( 'NONE',  ( -5.405949406249996869, 9.363379034771805109, -81.84375000204838102 ) ) ;
#16103 = CARTESIAN_POINT ( 'NONE',  ( -2.293366432827344421E-15, -12.48450537969573659, -190.7187500020484094 ) ) ;
#16104 = CARTESIAN_POINT ( 'NONE',  ( -9.999999999999998224, 1.224646799147353059E-15, -130.6250000040967620 ) ) ;
#16105 = CARTESIAN_POINT ( 'NONE',  ( 9.999999999999998224, 0.000000000000000000, -30.87500000409676559 ) ) ;
#16106 = CARTESIAN_POINT ( 'NONE',  ( 10.81189881249999729, 0.000000000000000000, -154.5312500020484094 ) ) ;
#16107 = CARTESIAN_POINT ( 'NONE',  ( -5.000000000000003553, -8.660254037844383745, -8.875000004096744277 ) ) ;
#16108 = CARTESIAN_POINT ( 'NONE',  ( 10.00000000000025402, -5.773502691896113426, -125.1249999999999574 ) ) ;
#16109 = CARTESIAN_POINT ( 'NONE',  ( -5.405949406249996869, 9.363379034771805109, -132.8437500020484094 ) ) ;
#16110 = CARTESIAN_POINT ( 'NONE',  ( 10.81189881249999551, -6.242252689847874514, -100.6562500020483952 ) ) ;
#16111 = CARTESIAN_POINT ( 'NONE',  ( 5.405949406249992428, -9.363379034771808662, -106.5937500020483810 ) ) ;
#16112 =( BOUNDED_CURVE ( )  B_SPLINE_CURVE ( 2, ( #32041, #12577, #38923, #28156, #9563, #10404, #29856 ),
 .UNSPECIFIED., .F., .F. ) 
 B_SPLINE_CURVE_WITH_KNOTS ( ( 3, 2, 2, 3 ),
 ( 0.8694029850746272103, 0.8706467661691545956, 0.8718905472636818699, 0.8731343283582092551 ),
 .UNSPECIFIED. ) 
 CURVE ( )  GEOMETRIC_REPRESENTATION_ITEM ( )  RATIONAL_B_SPLINE_CURVE ( ( 0.9999999999999641398, 0.8660254037844745678, 1.000000000000000000, 0.8660254037844387076, 1.000000000000000000, 0.8660254037844028474, 1.000000000000035971 ) ) 
 REPRESENTATION_ITEM ( '' )  );
#16113 = CARTESIAN_POINT ( 'NONE',  ( 5.405949406249999534, 9.363379034771803333, -77.59375000204838102 ) ) ;
#16114 = CARTESIAN_POINT ( 'NONE',  ( 10.81189881249999907, 6.242252689847868297, -82.40625000204836681 ) ) ;
#16115 = CARTESIAN_POINT ( 'NONE',  ( -4.999999999999996447, 8.660254037844387298, -171.3750000040968189 ) ) ;
#16116 = DIRECTION ( 'NONE',  ( -0.000000000000000000, -0.000000000000000000, 1.000000000000000000 ) ) ;
#16117 = CARTESIAN_POINT ( 'NONE',  ( -2.293366432827344421E-15, -12.48450537969573659, -169.9062500020484379 ) ) ;
#16118 = CARTESIAN_POINT ( 'NONE',  ( -10.81189881249999729, 1.324075727343319199E-15, -177.7812500020484094 ) ) ;
#16119 = CARTESIAN_POINT ( 'NONE',  ( 5.000000000000000000, 8.660254037844385522, -158.1250000040967905 ) ) ;
#16120 = CARTESIAN_POINT ( 'NONE',  ( -60.00000000000000711, 7.347880794884119933E-15, -223.0000000000000000 ) ) ;
#16121 = CARTESIAN_POINT ( 'NONE',  ( 10.81189881249999729, 0.000000000000000000, -7.343750002048343717 ) ) ;
#16122 = CARTESIAN_POINT ( 'NONE',  ( 5.000000000000000000, 8.660254037844385522, -127.7499999999999716 ) ) ;
#16123 = CARTESIAN_POINT ( 'NONE',  ( -10.81189881249999907, -6.242252689847864744, -117.4687500020483952 ) ) ;
#16124 = CARTESIAN_POINT ( 'NONE',  ( 4.999999999999992006, -8.660254037844389075, -78.74999999999998579 ) ) ;
#16125 = CARTESIAN_POINT ( 'NONE',  ( -5.405949406249996869, 9.363379034771805109, -13.03125000204835615 ) ) ;
#16126 = CARTESIAN_POINT ( 'NONE',  ( -9.999999999999998224, 1.224646799147353059E-15, -99.12500000409677625 ) ) ;
#16127 = FACE_OUTER_BOUND ( 'NONE', #34666, .T. ) ;
#16128 = CARTESIAN_POINT ( 'NONE',  ( 5.405949406249992428, -9.363379034771808662, -108.2812500020483810 ) ) ;
#16129 = CARTESIAN_POINT ( 'NONE',  ( 10.81189881249999551, -6.242252689847874514, -90.15625000204836681 ) ) ;
#16130 = ORIENTED_EDGE ( 'NONE', *, *, #31655, .F. ) ;
#16131 = CARTESIAN_POINT ( 'NONE',  ( -9.999999999999998224, 5.773502691896259087, -87.25000000409676204 ) ) ;
#16132 = DIRECTION ( 'NONE',  ( 1.000000000000000000, 0.000000000000000000, 0.000000000000000000 ) ) ;
#16133 = CARTESIAN_POINT ( 'NONE',  ( 10.81189881249999551, -6.242252689847874514, -38.96875000204835970 ) ) ;
#16134 = ORIENTED_EDGE ( 'NONE', *, *, #27689, .F. ) ;
#16135 = CARTESIAN_POINT ( 'NONE',  ( 9.999999999999996447, -5.773502691896262640, -15.62499999999997691 ) ) ;
#16136 = CARTESIAN_POINT ( 'NONE',  ( -2.121150477449813534E-15, -11.54700538379251284, -152.3750000000000000 ) ) ;
#16137 = CARTESIAN_POINT ( 'NONE',  ( 10.00000000000000000, 5.773502691896255534, -9.750000004096758488 ) ) ;
#16138 = CARTESIAN_POINT ( 'NONE',  ( -10.00000000000000000, -5.773502691896251982, -199.1250000000000284 ) ) ;
#16140 = ORIENTED_EDGE ( 'NONE', *, *, #31434, .T. ) ;
#16139 = CARTESIAN_POINT ( 'NONE',  ( -10.81189881249999729, 6.242252689847871849, -123.9062500020483952 ) ) ;
#16141 = CARTESIAN_POINT ( 'NONE',  ( -9.999999999999742428, -5.773502691896402084, -152.6249999999999716 ) ) ;
#16142 = EDGE_CURVE ( 'NONE', #40023, #5178, #31222, .T. ) ;
#16143 = EDGE_CURVE ( 'NONE', #12803, #15095, #36543, .T. ) ;
#16144 = ORIENTED_EDGE ( 'NONE', *, *, #15632, .F. ) ;
#16145 = EDGE_CURVE ( 'NONE', #14989, #28029, #6984, .T. ) ;
#16146 = CARTESIAN_POINT ( 'NONE',  ( 7.644554776091147741E-16, 12.48450537969573659, -56.65625000204838102 ) ) ;
#16147 = PERSON_AND_ORGANIZATION ( #11915, #17965 ) ;
#16148 = CARTESIAN_POINT ( 'NONE',  ( 5.405949406249999534, 9.363379034771803333, -100.0937500020483810 ) ) ;
#16150 = ORIENTED_EDGE ( 'NONE', *, *, #28811, .T. ) ;
#16149 = VERTEX_POINT ( 'NONE', #38938 ) ;
#16151 = CYLINDRICAL_SURFACE ( 'NONE', #16962, 9.999999999999998224 ) ;
#16152 = CC_DESIGN_DATE_AND_TIME_ASSIGNMENT ( #31917, #32545, ( #138 ) ) ;
#16153 = CARTESIAN_POINT ( 'NONE',  ( -9.999999999999998224, 1.224646799147353059E-15, -200.0000000000000000 ) ) ;
#16154 =( BOUNDED_CURVE ( )  B_SPLINE_CURVE ( 2, ( #28200, #34890, #21708, #41334, #8128, #30794, #1228 ),
 .UNSPECIFIED., .F., .F. ) 
 B_SPLINE_CURVE_WITH_KNOTS ( ( 3, 2, 2, 3 ),
 ( 0.7761194029850747578, 0.7773631840796021431, 0.7786069651741295283, 0.7798507462686569136 ),
 .UNSPECIFIED. ) 
 CURVE ( )  GEOMETRIC_REPRESENTATION_ITEM ( )  RATIONAL_B_SPLINE_CURVE ( ( 0.9999999999999880096, 0.8660254037844506980, 1.000000000000000000, 0.8660254037844387076, 1.000000000000000000, 0.8660254037844148378, 1.000000000000023981 ) ) 
 REPRESENTATION_ITEM ( '' )  );
#16155 = CARTESIAN_POINT ( 'NONE',  ( 10.81189881249999551, -6.242252689847874514, -177.1562500020484094 ) ) ;
#16156 = CARTESIAN_POINT ( 'NONE',  ( -10.81189881249999729, 1.324075727343319199E-15, -0.5937500020483654772 ) ) ;
#16157 = CARTESIAN_POINT ( 'NONE',  ( 10.00000000000051159, -5.773502691895965988, -146.5000000040967620 ) ) ;
#16158 = ADVANCED_FACE ( 'NONE', ( #9369 ), #39148, .T. ) ;
#16159 = CARTESIAN_POINT ( 'NONE',  ( -10.81189881249999729, -6.242252689847864744, -133.9687500020483810 ) ) ;
#16160 = CARTESIAN_POINT ( 'NONE',  ( -10.81189881249999729, 6.242252689847871849, -102.7187500020483810 ) ) ;
#16161 = CARTESIAN_POINT ( 'NONE',  ( -10.00000000000051337, 5.773502691895962435, -115.7500000040967905 ) ) ;
#16162 = CARTESIAN_POINT ( 'NONE',  ( -5.405949406249996869, 9.363379034771805109, -110.5312500020483810 ) ) ;
#16163 = CARTESIAN_POINT ( 'NONE',  ( -10.00000000000000000, -5.773502691896251982, -193.5000000040967905 ) ) ;
#16164 = CARTESIAN_POINT ( 'NONE',  ( -10.81189881249999729, -6.242252689847864744, -112.9687500020483810 ) ) ;
#16165 = CARTESIAN_POINT ( 'NONE',  ( -2.293366432827344421E-15, -12.48450537969573659, -187.9062500020484094 ) ) ;
#16166 = CARTESIAN_POINT ( 'NONE',  ( 4.999999999999992006, -8.660254037844389075, -185.6250000040967905 ) ) ;
#16167 = CARTESIAN_POINT ( 'NONE',  ( 7.070501591499377789E-16, 11.54700538379251284, -141.1250000000000000 ) ) ;
#16168 = CARTESIAN_POINT ( 'NONE',  ( -10.00000000000000000, -5.773502691896251982, -4.124999999999961808 ) ) ;
#16169 = EDGE_CURVE ( 'NONE', #22978, #14748, #31737, .T. ) ;
#16170 = CARTESIAN_POINT ( 'NONE',  ( -10.81189881249999729, -6.242252689847864744, -64.96875000204838102 ) ) ;
#16171 = CARTESIAN_POINT ( 'NONE',  ( 5.405949406249992428, -9.363379034771808662, -49.59375000204838102 ) ) ;
#16172 = CARTESIAN_POINT ( 'NONE',  ( -10.00000000000000000, -5.773502691896251982, -180.0000000040967905 ) ) ;
#16173 = CARTESIAN_POINT ( 'NONE',  ( 10.81189881249999907, 6.242252689847868297, -19.40625000204837747 ) ) ;
#16174 = CARTESIAN_POINT ( 'NONE',  ( 10.81189881249999551, -6.242252689847874514, -28.46875000204837391 ) ) ;
#16175 = CARTESIAN_POINT ( 'NONE',  ( 9.999999999999998224, 0.000000000000000000, -7.999999999999952038 ) ) ;
#16176 = CARTESIAN_POINT ( 'NONE',  ( -10.81189881249999907, -6.242252689847864744, -135.4687500020483810 ) ) ;
#16177 = CARTESIAN_POINT ( 'NONE',  ( 9.999999999999996447, -5.773502691896262640, -116.1250000000000000 ) ) ;
#16178 = CARTESIAN_POINT ( 'NONE',  ( -4.999999999999996447, 8.660254037844387298, -64.49999999999997158 ) ) ;
#16179 = CARTESIAN_POINT ( 'NONE',  ( -10.81189881249999729, 6.242252689847871849, -135.9062500020484094 ) ) ;
#16180 = CARTESIAN_POINT ( 'NONE',  ( 7.644554776091147741E-16, 12.48450537969573659, -115.1562500020483952 ) ) ;
#16181 = ORIENTED_EDGE ( 'NONE', *, *, #11440, .T. ) ;
#16182 = CYLINDRICAL_SURFACE ( 'NONE', #8651, 9.999999999999998224 ) ;
#16183 = CARTESIAN_POINT ( 'NONE',  ( -4.999999999999996447, 8.660254037844387298, -108.3750000040967763 ) ) ;
#16184 = CARTESIAN_POINT ( 'NONE',  ( 4.999999999999992006, -8.660254037844389075, -86.62500000409677625 ) ) ;
#16185 = CARTESIAN_POINT ( 'NONE',  ( -5.405949406250003975, -9.363379034771801557, -69.34375000204836681 ) ) ;
#16186 = ORIENTED_EDGE ( 'NONE', *, *, #17764, .F. ) ;
#16187 = CARTESIAN_POINT ( 'NONE',  ( 7.070501591499377789E-16, 11.54700538379251284, -45.12499999999997158 ) ) ;
#16188 = CARTESIAN_POINT ( 'NONE',  ( 9.999999999999996447, -5.773502691896262640, -17.50000000409676204 ) ) ;
#16189 = CARTESIAN_POINT ( 'NONE',  ( -2.293366432827344421E-15, -12.48450537969573659, -40.90625000204836681 ) ) ;
#16190 = ADVANCED_FACE ( 'NONE', ( #26201 ), #9790, .T. ) ;
#16191 = CARTESIAN_POINT ( 'NONE',  ( 5.000000000000000000, 8.660254037844385522, -16.74999999999996092 ) ) ;
#16192 = CARTESIAN_POINT ( 'NONE',  ( -10.00000000000000000, -5.773502691896251982, -37.50000000409675494 ) ) ;
#16193 = CARTESIAN_POINT ( 'NONE',  ( -5.405949406249996869, 9.363379034771805109, -38.53125000204838102 ) ) ;
#16194 = CARTESIAN_POINT ( 'NONE',  ( -9.999999999999998224, 1.224646799147353059E-15, -200.0000000000000000 ) ) ;
#16195 = CARTESIAN_POINT ( 'NONE',  ( 10.81189881249999729, 0.000000000000000000, -139.5312500020484094 ) ) ;
#16196 = CARTESIAN_POINT ( 'NONE',  ( 5.405949406249992428, -9.363379034771808662, -147.2812500020483810 ) ) ;
#16197 = CARTESIAN_POINT ( 'NONE',  ( -9.999999999999998224, 1.224646799147353059E-15, -150.1250000040967905 ) ) ;
#16198 = ORIENTED_EDGE ( 'NONE', *, *, #40574, .F. ) ;
#16199 = VERTEX_POINT ( 'NONE', #11222 ) ;
#16200 = ORIENTED_EDGE ( 'NONE', *, *, #18037, .T. ) ;
#16201 = CARTESIAN_POINT ( 'NONE',  ( -9.999999999999998224, 0.000000000000000000, -99.99999999999998579 ) ) ;
#16202 = CARTESIAN_POINT ( 'NONE',  ( 5.405949406249999534, 9.363379034771803333, -176.5937500020484094 ) ) ;
#16204 = EDGE_CURVE ( 'NONE', #38561, #6885, #18468, .T. ) ;
#16203 = CARTESIAN_POINT ( 'NONE',  ( 5.405949406249999534, 9.363379034771803333, -26.59375000204835970 ) ) ;
#16205 = CARTESIAN_POINT ( 'NONE',  ( -2.275517850991317657E-15, -20.00000000000000000, -235.0000000000000000 ) ) ;
#16206 = CARTESIAN_POINT ( 'NONE',  ( 10.81189881249999729, 0.000000000000000000, -154.3437500020483810 ) ) ;
#16207 = CARTESIAN_POINT ( 'NONE',  ( -10.81189881249999729, 1.324075727343319199E-15, -146.0937500020483810 ) ) ;
#16208 = CARTESIAN_POINT ( 'NONE',  ( 10.00000000000012790, 5.773502691896179151, -173.2500000040967905 ) ) ;
#16209 = CARTESIAN_POINT ( 'NONE',  ( -10.81189881249999729, 1.324075727343319199E-15, -129.5937500020483810 ) ) ;
#16210 = AXIS2_PLACEMENT_3D ( 'NONE', #13822, #17067, #33296 ) ;
#16211 = CARTESIAN_POINT ( 'NONE',  ( -5.405949406249996869, 9.363379034771805109, -133.0312500020484094 ) ) ;
#16212 = CARTESIAN_POINT ( 'NONE',  ( 7.644554776091147741E-16, 12.48450537969573659, -14.46875000204836859 ) ) ;
#16213 = CARTESIAN_POINT ( 'NONE',  ( -10.81189881249999729, 1.324075727343319199E-15, -135.5937500020483810 ) ) ;
#16214 = DIRECTION ( 'NONE',  ( -0.000000000000000000, -0.000000000000000000, 1.000000000000000000 ) ) ;
#16215 = VECTOR ( 'NONE', #15988, 1000.000000000000000 ) ;
#16216 = CARTESIAN_POINT ( 'NONE',  ( -2.121150477449813534E-15, -11.54700538379251284, -102.8749999999999858 ) ) ;
#16217 = CARTESIAN_POINT ( 'NONE',  ( -5.000000000000003553, -8.660254037844383745, -160.0000000000000000 ) ) ;
#16218 = CARTESIAN_POINT ( 'NONE',  ( -5.000000000000003553, -8.660254037844383745, -167.8750000040967905 ) ) ;
#16219 = CARTESIAN_POINT ( 'NONE',  ( -5.405949406250003975, -9.363379034771801557, -72.34375000204836681 ) ) ;
#16220 = CARTESIAN_POINT ( 'NONE',  ( -5.405949406250003975, -9.363379034771801557, -47.03125000204838813 ) ) ;
#16221 = CARTESIAN_POINT ( 'NONE',  ( 10.81189881249999551, -6.242252689847874514, -56.96875000204838102 ) ) ;
#16222 = LINE ( 'NONE', #29422, #19882 ) ;
#16223 = CARTESIAN_POINT ( 'NONE',  ( 7.644554776091147741E-16, 12.48450537969573659, -164.4687500020483810 ) ) ;
#16224 = CARTESIAN_POINT ( 'NONE',  ( -2.121150477449813534E-15, -11.54700538379251284, -137.3750000000000000 ) ) ;
#16225 = VECTOR ( 'NONE', #4983, 1000.000000000000000 ) ;
#16226 = CARTESIAN_POINT ( 'NONE',  ( -5.405949406250003975, -9.363379034771801557, -135.5312500020484094 ) ) ;
#16227 = CARTESIAN_POINT ( 'NONE',  ( -9.999999999999998224, 1.224646799147353059E-15, -173.7500000000000284 ) ) ;
#16228 = CARTESIAN_POINT ( 'NONE',  ( 9.999999999999998224, 0.000000000000000000, -117.8750000040967905 ) ) ;
#16229 = CARTESIAN_POINT ( 'NONE',  ( -9.999999999999998224, 5.773502691896259087, -88.37499999999998579 ) ) ;
#16230 = ORIENTED_EDGE ( 'NONE', *, *, #37696, .F. ) ;
#16231 = CARTESIAN_POINT ( 'NONE',  ( 7.644554776091147741E-16, 12.48450537969573659, -119.6562500020484094 ) ) ;
#16232 = CARTESIAN_POINT ( 'NONE',  ( -2.121150477449813534E-15, -11.54700538379251284, -134.7500000040967905 ) ) ;
#16233 = CARTESIAN_POINT ( 'NONE',  ( -9.999999999999998224, 1.224646799147353059E-15, -176.7500000000000284 ) ) ;
#16234 = CARTESIAN_POINT ( 'NONE',  ( 7.644554776091147741E-16, 12.48450537969573659, -175.1562500020484094 ) ) ;
#16235 = CARTESIAN_POINT ( 'NONE',  ( -2.121150477449813534E-15, -11.54700538379251284, -43.25000000409675494 ) ) ;
#16236 = CARTESIAN_POINT ( 'NONE',  ( -9.999999999999998224, 1.224646799147353059E-15, -48.12500000409677625 ) ) ;
#16237 = CARTESIAN_POINT ( 'NONE',  ( -10.81189881249999729, 6.242252689847871849, -60.90625000204837391 ) ) ;
#16238 = DIRECTION ( 'NONE',  ( 1.000000000000000000, 1.502314598737160017E-16, 0.000000000000000000 ) ) ;
#16239 = CARTESIAN_POINT ( 'NONE',  ( -10.81189881249999729, 1.324075727343319199E-15, -162.7812500020484094 ) ) ;
#16240 = CARTESIAN_POINT ( 'NONE',  ( 7.644554776091147741E-16, 12.48450537969573659, -146.4687500020484094 ) ) ;
#16241 = CARTESIAN_POINT ( 'NONE',  ( -4.999999999999996447, 8.660254037844387298, -166.8750000040967905 ) ) ;
#16242 = DIRECTION ( 'NONE',  ( -0.000000000000000000, -0.000000000000000000, -1.000000000000000000 ) ) ;
#16243 = ORIENTED_EDGE ( 'NONE', *, *, #38620, .T. ) ;
#16244 =( BOUNDED_CURVE ( )  B_SPLINE_CURVE ( 2, ( #17571, #20394, #4220, #33586, #17150, #21039, #18003 ),
 .UNSPECIFIED., .F., .F. ) 
 B_SPLINE_CURVE_WITH_KNOTS ( ( 3, 2, 2, 3 ),
 ( 0.8171641791044778058, 0.8184079601990051911, 0.8196517412935324653, 0.8208955223880598506 ),
 .UNSPECIFIED. ) 
 CURVE ( )  GEOMETRIC_REPRESENTATION_ITEM ( )  RATIONAL_B_SPLINE_CURVE ( ( 0.9999999999999761302, 0.8660254037844625774, 1.000000000000000000, 0.8660254037844387076, 1.000000000000000000, 0.8660254037844267172, 1.000000000000011990 ) ) 
 REPRESENTATION_ITEM ( '' )  );
#16245 = CARTESIAN_POINT ( 'NONE',  ( 7.070501591499376803E-16, 11.54700538379251284, -114.5000000040967905 ) ) ;
#16246 = AXIS2_PLACEMENT_3D ( 'NONE', #3025, #9074, #34993 ) ;
#16248 = ORIENTED_EDGE ( 'NONE', *, *, #2566, .F. ) ;
#16247 = CARTESIAN_POINT ( 'NONE',  ( -2.293366432827344421E-15, -12.48450537969573659, -70.90625000204839523 ) ) ;
#16249 = DATE_TIME_ROLE ( 'classification_date' ) ;
#16251 = ORIENTED_EDGE ( 'NONE', *, *, #35465, .T. ) ;
#16250 = CARTESIAN_POINT ( 'NONE',  ( 7.644554776091147741E-16, 12.48450537969573659, -117.9687500020483668 ) ) ;
#16252 = EDGE_LOOP ( 'NONE', ( #2700, #7411, #32420, #770 ) ) ;
#16253 = CARTESIAN_POINT ( 'NONE',  ( 10.81189881249999729, 0.000000000000000000, -25.34375000204835970 ) ) ;
#16254 = CARTESIAN_POINT ( 'NONE',  ( -2.293366432827344421E-15, -12.48450537969573659, -196.7187500020484094 ) ) ;
#16256 = EDGE_CURVE ( 'NONE', #4172, #35088, #21152, .T. ) ;
#16255 = CARTESIAN_POINT ( 'NONE',  ( 10.81189881249999729, 0.000000000000000000, -47.84375000204838102 ) ) ;
#16257 = CARTESIAN_POINT ( 'NONE',  ( -9.999999999999998224, 1.224646799147353059E-15, -143.7500000000000000 ) ) ;
#16258 = CARTESIAN_POINT ( 'NONE',  ( 10.00000000000000000, 5.773502691896255534, -27.37499999999998224 ) ) ;
#16259 = CARTESIAN_POINT ( 'NONE',  ( -10.81189881249999729, 6.242252689847871849, -186.7187500020484379 ) ) ;
#16260 = CARTESIAN_POINT ( 'NONE',  ( -10.81189881249999729, 6.242252689847871849, -165.7187500020483810 ) ) ;
#16261 = CARTESIAN_POINT ( 'NONE',  ( -2.293366432827344421E-15, -12.48450537969573659, -147.2187500020484094 ) ) ;
#16262 = CARTESIAN_POINT ( 'NONE',  ( 10.81189881249999729, 0.000000000000000000, -169.3437500020484094 ) ) ;
#16263 = CYLINDRICAL_SURFACE ( 'NONE', #8172, 9.999999999999998224 ) ;
#16264 = CARTESIAN_POINT ( 'NONE',  ( -9.999999999999872102, -5.773502691896326589, -162.0000000040967620 ) ) ;
#16265 = CARTESIAN_POINT ( 'NONE',  ( -9.999999999999998224, 5.773502691896259087, -187.3750000000000000 ) ) ;
#16266 = CARTESIAN_POINT ( 'NONE',  ( -5.405949406249996869, 9.363379034771805109, -96.84375000204838102 ) ) ;
#16267 = CARTESIAN_POINT ( 'NONE',  ( 7.070501591499376803E-16, 11.54700538379251284, -18.12499999999997513 ) ) ;
#16268 = CARTESIAN_POINT ( 'NONE',  ( -5.405949406249996869, 9.363379034771805109, -77.53125000204838102 ) ) ;
#16269 = CARTESIAN_POINT ( 'NONE',  ( 9.999999999999479527, 5.773502691896553074, -96.75000000409676204 ) ) ;
#16270 = CARTESIAN_POINT ( 'NONE',  ( 10.81189881249999551, -6.242252689847874514, -182.9687500020484094 ) ) ;
#16271 = CARTESIAN_POINT ( 'NONE',  ( -10.81189881249999729, 6.242252689847871849, -159.9062500020483810 ) ) ;
#16272 = CARTESIAN_POINT ( 'NONE',  ( 10.81189881249999907, 6.242252689847868297, -62.90625000204838813 ) ) ;
#16273 = CARTESIAN_POINT ( 'NONE',  ( -5.000000000000003553, -8.660254037844383745, -139.3750000040968189 ) ) ;
#16274 = CARTESIAN_POINT ( 'NONE',  ( 4.999999999999992006, -8.660254037844389075, -111.7499999999999858 ) ) ;
#16275 = ADVANCED_FACE ( 'NONE', ( #27640 ), #2248, .T. ) ;
#16276 = ORIENTED_EDGE ( 'NONE', *, *, #17483, .T. ) ;
#16277 = CARTESIAN_POINT ( 'NONE',  ( 10.81189881249999729, 0.000000000000000000, -139.5312500020484094 ) ) ;
#16278 = SECURITY_CLASSIFICATION ( '', '', #33181 ) ;
#16279 = CARTESIAN_POINT ( 'NONE',  ( -10.81189881249999907, -6.242252689847864744, -156.6562500020483810 ) ) ;
#16280 = CARTESIAN_POINT ( 'NONE',  ( -5.405949406250003975, -9.363379034771801557, -198.5312500020484094 ) ) ;
#16281 = CARTESIAN_POINT ( 'NONE',  ( -9.999999999999998224, 1.224646799147353059E-15, -127.2499999999999716 ) ) ;
#16282 = CARTESIAN_POINT ( 'NONE',  ( -10.81189881249999907, -6.242252689847864744, -87.46875000204838102 ) ) ;
#16283 = ORIENTED_EDGE ( 'NONE', *, *, #12451, .F. ) ;
#16284 = CARTESIAN_POINT ( 'NONE',  ( 9.999999999999996447, -5.773502691896262640, -56.12499999999997868 ) ) ;
#16285 = CARTESIAN_POINT ( 'NONE',  ( -10.81189881249999907, -6.242252689847864744, -186.4687500020484094 ) ) ;
#16286 = CARTESIAN_POINT ( 'NONE',  ( -9.999999999999998224, 1.224646799147353059E-15, -75.12500000409677625 ) ) ;
#16287 = CARTESIAN_POINT ( 'NONE',  ( -10.00000000000012434, 5.773502691896184480, -164.8749999999999716 ) ) ;
#16288 = CARTESIAN_POINT ( 'NONE',  ( -9.999999999999742428, -5.773502691896402084, -160.5000000040968189 ) ) ;
#16289 = CARTESIAN_POINT ( 'NONE',  ( -5.405949406249996869, 9.363379034771805109, -83.53125000204838102 ) ) ;
#16290 = CARTESIAN_POINT ( 'NONE',  ( 7.644554776091147741E-16, 12.48450537969573659, -71.65625000204836681 ) ) ;
#16291 =( BOUNDED_CURVE ( )  B_SPLINE_CURVE ( 2, ( #23343, #19872, #39516, #33057, #39725, #3483, #40348 ),
 .UNSPECIFIED., .F., .F. ) 
 B_SPLINE_CURVE_WITH_KNOTS ( ( 3, 2, 2, 3 ),
 ( 0.9813432835820897759, 0.9825870646766171612, 0.9838308457711445465, 0.9850746268656718208 ),
 .UNSPECIFIED. ) 
 CURVE ( )  GEOMETRIC_REPRESENTATION_ITEM ( )  RATIONAL_B_SPLINE_CURVE ( ( 0.9999999999999761302, 0.8660254037844625774, 1.000000000000000000, 0.8660254037844387076, 1.000000000000000000, 0.8660254037844148378, 1.000000000000023981 ) ) 
 REPRESENTATION_ITEM ( '' )  );
#16292 = CARTESIAN_POINT ( 'NONE',  ( 5.000000000000000000, 8.660254037844385522, -62.12500000409676204 ) ) ;
#16293 = CARTESIAN_POINT ( 'NONE',  ( -2.293366432827344421E-15, -12.48450537969573659, -21.21875000204837036 ) ) ;
#16294 = DIRECTION ( 'NONE',  ( 1.000000000000000000, 0.000000000000000000, 0.000000000000000000 ) ) ;
#16295 = CARTESIAN_POINT ( 'NONE',  ( -5.405949406250003975, -9.363379034771801557, -186.5312500020484094 ) ) ;
#16296 = CARTESIAN_POINT ( 'NONE',  ( -5.405949406249996869, 9.363379034771805109, -13.03125000204835615 ) ) ;
#16297 = CARTESIAN_POINT ( 'NONE',  ( 10.81189881249999729, 6.242252689847867408, -1.218750002048353709 ) ) ;
#16298 = CARTESIAN_POINT ( 'NONE',  ( -9.999999999999479527, -5.773502691896549521, -148.5000000040967336 ) ) ;
#16299 = CARTESIAN_POINT ( 'NONE',  ( 4.999999999999992006, -8.660254037844389075, -62.62500000409676204 ) ) ;
#16300 = CARTESIAN_POINT ( 'NONE',  ( -9.999999999999998224, 0.8726646254783168022, 0.000000000000000000 ) ) ;
#16301 =( BOUNDED_CURVE ( )  B_SPLINE_CURVE ( 2, ( #15373, #20312, #3500, #496, #6323, #10176, #36513 ),
 .UNSPECIFIED., .F., .F. ) 
 B_SPLINE_CURVE_WITH_KNOTS ( ( 3, 2, 2, 3 ),
 ( 0.5485074626865672487, 0.5497512437810946340, 0.5509950248756221303, 0.5522388059701495155 ),
 .UNSPECIFIED. ) 
 CURVE ( )  GEOMETRIC_REPRESENTATION_ITEM ( )  RATIONAL_B_SPLINE_CURVE ( ( 0.9999999999999880096, 0.8660254037844506980, 1.000000000000000000, 0.8660254037844387076, 1.000000000000000000, 0.8660254037844148378, 1.000000000000023981 ) ) 
 REPRESENTATION_ITEM ( '' )  );
#16302 = CARTESIAN_POINT ( 'NONE',  ( 10.00000000000000000, 5.773502691896255534, -169.8750000000000000 ) ) ;
#16303 = CARTESIAN_POINT ( 'NONE',  ( -9.999999999999998224, 1.224646799147353059E-15, -200.0000000000000000 ) ) ;
#16305 = ORIENTED_EDGE ( 'NONE', *, *, #13997, .F. ) ;
#16304 = CARTESIAN_POINT ( 'NONE',  ( 10.81189881249999907, 6.242252689847868297, -95.90625000204839523 ) ) ;
#16306 = CARTESIAN_POINT ( 'NONE',  ( 10.00000000000044764, -5.773502691896004180, -181.0000000040967620 ) ) ;
#16308 = ORIENTED_EDGE ( 'NONE', *, *, #15377, .T. ) ;
#16307 = CARTESIAN_POINT ( 'NONE',  ( 5.405949406249992428, -9.363379034771808662, -100.5937500020483810 ) ) ;
#16309 = ORIENTED_EDGE ( 'NONE', *, *, #12760, .T. ) ;
#16310 = EDGE_CURVE ( 'NONE', #28672, #30453, #37561, .T. ) ;
#16311 = CARTESIAN_POINT ( 'NONE',  ( -10.81189881249999729, 1.324075727343319199E-15, -33.59375000204836681 ) ) ;
#16312 = CARTESIAN_POINT ( 'NONE',  ( -5.405949406250003975, -9.363379034771801557, -21.53125000204836326 ) ) ;
#16313 = CARTESIAN_POINT ( 'NONE',  ( 10.81189881249999551, -6.242252689847874514, -82.46875000204836681 ) ) ;
#16314 = CARTESIAN_POINT ( 'NONE',  ( -5.000000000000003553, -8.660254037844383745, -115.3750000040967905 ) ) ;
#16315 = CARTESIAN_POINT ( 'NONE',  ( -10.81189881249999729, 1.324075727343319199E-15, -194.0937500020484094 ) ) ;
#16316 = CARTESIAN_POINT ( 'NONE',  ( 0.000000000000000000, 0.000000000000000000, -200.0000000000000000 ) ) ;
#16317 = CARTESIAN_POINT ( 'NONE',  ( -9.999999999999998224, 0.000000000000000000, -99.99999999999998579 ) ) ;
#16318 = CARTESIAN_POINT ( 'NONE',  ( -5.405949406249996869, 9.363379034771805109, -158.5312500020484094 ) ) ;
#16319 = CARTESIAN_POINT ( 'NONE',  ( -5.000000000000003553, -8.660254037844383745, -1.375000004096765815 ) ) ;
#16320 = DIRECTION ( 'NONE',  ( -1.000000000000000000, -1.502314598737160017E-16, 0.000000000000000000 ) ) ;
#16321 = CARTESIAN_POINT ( 'NONE',  ( -5.405949406250003975, -9.363379034771801557, -121.8437500020483952 ) ) ;
#16322 = CARTESIAN_POINT ( 'NONE',  ( 5.405949406249999534, 9.363379034771803333, -101.7812500020483952 ) ) ;
#16323 = CARTESIAN_POINT ( 'NONE',  ( -10.81189881249999729, -6.242252689847864744, -106.9687500020483810 ) ) ;
#16324 = CARTESIAN_POINT ( 'NONE',  ( -10.81189881249999729, 1.324075727343319199E-15, -75.59375000204838102 ) ) ;
#16325 = CARTESIAN_POINT ( 'NONE',  ( -5.405949406250003975, -9.363379034771801557, -84.53125000204838102 ) ) ;
#16326 = CARTESIAN_POINT ( 'NONE',  ( 9.999999999999996447, -5.773502691896262640, -164.5000000040967905 ) ) ;
#16327 = CARTESIAN_POINT ( 'NONE',  ( -9.999999999999998224, 1.224646799147353059E-15, -81.12500000409677625 ) ) ;
#16328 = CARTESIAN_POINT ( 'NONE',  ( -5.405949406250003975, -9.363379034771801557, -170.0312500020484094 ) ) ;
#16329 = CARTESIAN_POINT ( 'NONE',  ( -5.405949406249996869, 9.363379034771805109, -176.5312500020483810 ) ) ;
#16330 = CARTESIAN_POINT ( 'NONE',  ( -4.999999999999996447, 8.660254037844387298, -153.3750000040967905 ) ) ;
#16331 = DIRECTION ( 'NONE',  ( 1.000000000000000000, 0.000000000000000000, 0.000000000000000000 ) ) ;
#16332 = CARTESIAN_POINT ( 'NONE',  ( 10.81189881249999551, -6.242252689847874514, -5.968750002048355263 ) ) ;
#16333 = CARTESIAN_POINT ( 'NONE',  ( 9.999999999999998224, 0.000000000000000000, -126.5000000000000000 ) ) ;
#16334 = CARTESIAN_POINT ( 'NONE',  ( -10.81189881249999907, -6.242252689847864744, -115.9687500020483810 ) ) ;
#16335 = EDGE_CURVE ( 'NONE', #7903, #24042, #330, .T. ) ;
#16336 = CARTESIAN_POINT ( 'NONE',  ( -4.999999999999996447, 8.660254037844387298, -82.49999999999998579 ) ) ;
#16337 = CARTESIAN_POINT ( 'NONE',  ( 5.405949406249999534, 9.363379034771803333, -13.28125000204835615 ) ) ;
#16338 = CARTESIAN_POINT ( 'NONE',  ( -9.999999999999998224, 1.224646799147353059E-15, -94.62500000409677625 ) ) ;
#16339 = DIRECTION ( 'NONE',  ( 1.000000000000000000, 0.000000000000000000, 0.000000000000000000 ) ) ;
#16340 = CARTESIAN_POINT ( 'NONE',  ( -10.81189881249999729, 1.324075727343319199E-15, -111.7812500020483810 ) ) ;
#16341 = CARTESIAN_POINT ( 'NONE',  ( 5.405949406249999534, 9.363379034771803333, -88.28125000204838102 ) ) ;
#16342 = ORIENTED_EDGE ( 'NONE', *, *, #31063, .T. ) ;
#16343 = CARTESIAN_POINT ( 'NONE',  ( 7.070501591499377789E-16, 11.54700538379251284, -87.50000000409677625 ) ) ;
#16344 = CARTESIAN_POINT ( 'NONE',  ( -5.405949406249996869, 9.363379034771805109, -41.34375000204837391 ) ) ;
#16345 = ORIENTED_EDGE ( 'NONE', *, *, #8806, .F. ) ;
#16346 = CARTESIAN_POINT ( 'NONE',  ( -5.000000000000003553, -8.660254037844383745, -11.49999999999995381 ) ) ;
#16347 = CARTESIAN_POINT ( 'NONE',  ( -4.999999999999996447, 8.660254037844387298, -148.5000000000000000 ) ) ;
#16348 = CARTESIAN_POINT ( 'NONE',  ( -10.00000000000000000, -5.773502691896251982, -15.00000000409676559 ) ) ;
#16349 = CARTESIAN_POINT ( 'NONE',  ( -10.00000000000000000, -5.773502691896251982, -191.6250000000000284 ) ) ;
#16351 = ORIENTED_EDGE ( 'NONE', *, *, #36721, .F. ) ;
#16350 = CARTESIAN_POINT ( 'NONE',  ( 5.405949406249992428, -9.363379034771808662, -114.2812500020483952 ) ) ;
#16352 = VECTOR ( 'NONE', #9865, 1000.000000000000000 ) ;
#16353 = CARTESIAN_POINT ( 'NONE',  ( -10.00000000000102496, 5.773502691895664007, -36.25000000409672651 ) ) ;
#16354 = VECTOR ( 'NONE', #11492, 1000.000000000000114 ) ;
#16355 = ORIENTED_EDGE ( 'NONE', *, *, #40022, .F. ) ;
#16356 = CARTESIAN_POINT ( 'NONE',  ( 5.405949406249992428, -9.363379034771808662, -42.28125000204838102 ) ) ;
#16357 = DATE_AND_TIME ( #9070, #11103 ) ;
#16358 = CARTESIAN_POINT ( 'NONE',  ( -5.405949406250003975, -9.363379034771801557, -99.34375000204838102 ) ) ;
#16359 = CARTESIAN_POINT ( 'NONE',  ( -2.293366432827344421E-15, -12.48450537969573659, -123.4062500020483952 ) ) ;
#16360 = ORIENTED_EDGE ( 'NONE', *, *, #2495, .F. ) ;
#16361 =( BOUNDED_CURVE ( )  B_SPLINE_CURVE ( 2, ( #28705, #15296, #37759, #14862, #2162, #5174, #5391 ),
 .UNSPECIFIED., .F., .F. ) 
 B_SPLINE_CURVE_WITH_KNOTS ( ( 3, 2, 2, 3 ),
 ( 0.3097014925373136052, 0.3109452736318408794, 0.3121890547263682092, 0.3134328358208955390 ),
 .UNSPECIFIED. ) 
 CURVE ( )  GEOMETRIC_REPRESENTATION_ITEM ( )  RATIONAL_B_SPLINE_CURVE ( ( 0.9999999999999820144, 0.8660254037844566932, 1.000000000000000000, 0.8660254037844387076, 1.000000000000000000, 0.8660254037844387076, 1.000000000000000000 ) ) 
 REPRESENTATION_ITEM ( '' )  );
#16362 = CARTESIAN_POINT ( 'NONE',  ( -8.659811548901195977, -5.000849327365069819, 0.000000000000000000 ) ) ;
#16363 = CARTESIAN_POINT ( 'NONE',  ( -5.000000000000003553, -8.660254037844383745, -125.8750000040967905 ) ) ;
#16364 = CARTESIAN_POINT ( 'NONE',  ( 5.405949406249992428, -9.363379034771808662, -178.7812500020484094 ) ) ;
#16365 = LINE ( 'NONE', #33820, #34429 ) ;
#16366 = DIRECTION ( 'NONE',  ( 0.000000000000000000, 0.000000000000000000, 1.000000000000000000 ) ) ;
#16367 = CARTESIAN_POINT ( 'NONE',  ( -10.81189881249999729, 6.242252689847871849, -131.2187500020483810 ) ) ;
#16368 = CARTESIAN_POINT ( 'NONE',  ( -2.293366432827344421E-15, -12.48450537969573659, -105.2187500020483952 ) ) ;
#16369 = LINE ( 'NONE', #22456, #35947 ) ;
#16370 = CARTESIAN_POINT ( 'NONE',  ( -5.405949406249996869, 9.363379034771805109, -109.0312500020483810 ) ) ;
#16371 = CARTESIAN_POINT ( 'NONE',  ( 7.070501591499377789E-16, 11.54700538379251284, -194.0000000040967905 ) ) ;
#16372 = CARTESIAN_POINT ( 'NONE',  ( 10.81189881249999551, -6.242252689847874514, -112.4687500020483810 ) ) ;
#16373 = CARTESIAN_POINT ( 'NONE',  ( -2.293366432827344421E-15, -12.48450537969573659, -184.9062500020484094 ) ) ;
#16374 = CARTESIAN_POINT ( 'NONE',  ( -9.999999999999742428, -5.773502691896402084, -186.0000000040967905 ) ) ;
#16375 = DIRECTION ( 'NONE',  ( -0.000000000000000000, -0.000000000000000000, 1.000000000000000000 ) ) ;
#16376 = CARTESIAN_POINT ( 'NONE',  ( 10.00000000000000000, 5.773502691896255534, -139.8750000000000000 ) ) ;
#16377 = CARTESIAN_POINT ( 'NONE',  ( 9.999999999999998224, 0.000000000000000000, -7.999999999999952038 ) ) ;
#16378 = CARTESIAN_POINT ( 'NONE',  ( -10.81189881249999729, -6.242252689847864744, -60.46875000204836681 ) ) ;
#16379 = CARTESIAN_POINT ( 'NONE',  ( -5.405949406250003975, -9.363379034771801557, -52.84375000204835970 ) ) ;
#16380 = CARTESIAN_POINT ( 'NONE',  ( 9.999999999999998224, 0.000000000000000000, -179.3750000040967905 ) ) ;
#16381 = CARTESIAN_POINT ( 'NONE',  ( 5.405949406249992428, -9.363379034771808662, -18.28125000204835970 ) ) ;
#16382 = VECTOR ( 'NONE', #19783, 1000.000000000000000 ) ;
#16383 = CARTESIAN_POINT ( 'NONE',  ( 10.81189881249999729, 0.000000000000000000, -31.34375000204836681 ) ) ;
#16384 = CARTESIAN_POINT ( 'NONE',  ( 9.999999999999998224, 0.000000000000000000, -141.8750000040967905 ) ) ;
#16385 = CARTESIAN_POINT ( 'NONE',  ( -5.405949406250003975, -9.363379034771801557, -139.8437500020484094 ) ) ;
#16386 = ADVANCED_FACE ( 'NONE', ( #7191 ), #34125, .T. ) ;
#16387 = CARTESIAN_POINT ( 'NONE',  ( -5.000000000000003553, -8.660254037844383745, -103.0000000000000000 ) ) ;
#16388 = CARTESIAN_POINT ( 'NONE',  ( -10.81189881249999729, 6.242252689847871849, -35.40625000204835970 ) ) ;
#16389 = FACE_OUTER_BOUND ( 'NONE', #15098, .T. ) ;
#16390 = EDGE_CURVE ( 'NONE', #5036, #10156, #26791, .T. ) ;
#16391 = CARTESIAN_POINT ( 'NONE',  ( -2.121150477449813534E-15, -11.54700538379251284, -65.37499999999998579 ) ) ;
#16392 = CARTESIAN_POINT ( 'NONE',  ( -2.293366432827344421E-15, -12.48450537969573659, -135.4062500020483810 ) ) ;
#16393 = CARTESIAN_POINT ( 'NONE',  ( -10.81189881249999729, 6.242252689847871849, -116.4062500020483952 ) ) ;
#16394 = ORIENTED_EDGE ( 'NONE', *, *, #18829, .F. ) ;
#16395 = CARTESIAN_POINT ( 'NONE',  ( 5.000000000000000000, 8.660254037844385522, -160.7500000000000000 ) ) ;
#16396 = CARTESIAN_POINT ( 'NONE',  ( -10.00000000000000000, -5.773502691896251982, -111.0000000040967763 ) ) ;
#16397 = CARTESIAN_POINT ( 'NONE',  ( 4.999999999999992006, -8.660254037844389075, -107.2499999999999858 ) ) ;
#16398 = CARTESIAN_POINT ( 'NONE',  ( 7.644554776091147741E-16, 12.48450537969573659, -69.96875000204838102 ) ) ;
#16399 = ORIENTED_EDGE ( 'NONE', *, *, #24629, .T. ) ;
#16400 = CARTESIAN_POINT ( 'NONE',  ( 5.000000000000000000, 8.660254037844385522, -33.24999999999997158 ) ) ;
#16401 = CARTESIAN_POINT ( 'NONE',  ( -9.999999999999998224, 1.224646799147353059E-15, -19.62500000409675494 ) ) ;
#16402 = CARTESIAN_POINT ( 'NONE',  ( -10.81189881249999729, 6.242252689847871849, -41.40625000204836681 ) ) ;
#16403 = LINE ( 'NONE', #23761, #37298 ) ;
#16404 = CARTESIAN_POINT ( 'NONE',  ( 9.999999999999998224, 0.000000000000000000, -32.37500000409676204 ) ) ;
#16405 = CYLINDRICAL_SURFACE ( 'NONE', #23148, 9.999999999999998224 ) ;
#16406 = CARTESIAN_POINT ( 'NONE',  ( 10.81189881249999907, 6.242252689847868297, -136.4062500020484094 ) ) ;
#16407 = CARTESIAN_POINT ( 'NONE',  ( -5.405949406249996869, 9.363379034771805109, -142.0312500020483810 ) ) ;
#16408 = ADVANCED_FACE ( 'NONE', ( #17686 ), #34769, .F. ) ;
#16409 = CARTESIAN_POINT ( 'NONE',  ( 9.999999999999479527, 5.773502691896553074, -122.2500000040967763 ) ) ;
#16410 = ORIENTED_EDGE ( 'NONE', *, *, #1916, .F. ) ;
#16411 =( BOUNDED_CURVE ( )  B_SPLINE_CURVE ( 2, ( #14479, #39754, #10189, #36524, #26817, #10399, #23589 ),
 .UNSPECIFIED., .F., .F. ) 
 B_SPLINE_CURVE_WITH_KNOTS ( ( 3, 2, 2, 3 ),
 ( 0.4216417910447762818, 0.4228855721393036671, 0.4241293532338309413, 0.4253731343283583266 ),
 .UNSPECIFIED. ) 
 CURVE ( )  GEOMETRIC_REPRESENTATION_ITEM ( )  RATIONAL_B_SPLINE_CURVE ( ( 0.9999999999999820144, 0.8660254037844566932, 1.000000000000000000, 0.8660254037844387076, 1.000000000000000000, 0.8660254037844267172, 1.000000000000011990 ) ) 
 REPRESENTATION_ITEM ( '' )  );
#16412 = EDGE_LOOP ( 'NONE', ( #38947, #9891, #378, #22159 ) ) ;
#16413 = ADVANCED_FACE ( 'NONE', ( #18124 ), #31319, .F. ) ;
#16414 = ORIENTED_EDGE ( 'NONE', *, *, #35988, .T. ) ;
#16415 = EDGE_CURVE ( 'NONE', #33809, #1539, #8017, .T. ) ;
#16416 = VECTOR ( 'NONE', #3142, 1000.000000000000000 ) ;
#16417 = CARTESIAN_POINT ( 'NONE',  ( 7.644554776091147741E-16, 12.48450537969573659, -171.9687500020483810 ) ) ;
#16418 = CARTESIAN_POINT ( 'NONE',  ( 10.81189881249999729, 0.000000000000000000, -26.84375000204835970 ) ) ;
#16419 = DIRECTION ( 'NONE',  ( -0.000000000000000000, -0.000000000000000000, 1.000000000000000000 ) ) ;
#16420 = CARTESIAN_POINT ( 'NONE',  ( -2.293366432827344421E-15, -12.48450537969573659, -153.2187500020483810 ) ) ;
#16421 = CARTESIAN_POINT ( 'NONE',  ( 7.644554776091147741E-16, 12.48450537969573659, -147.9687500020484094 ) ) ;
#16422 = CARTESIAN_POINT ( 'NONE',  ( 9.999999999999998224, 0.000000000000000000, -115.9999999999999858 ) ) ;
#16423 = CARTESIAN_POINT ( 'NONE',  ( -10.81189881249999729, 6.242252689847871849, -123.7187500020483952 ) ) ;
#16424 = CARTESIAN_POINT ( 'NONE',  ( 10.81189881249999907, 6.242252689847868297, -131.9062500020484094 ) ) ;
#16425 = CARTESIAN_POINT ( 'NONE',  ( -2.293366432827344421E-15, -12.48450537969573659, -19.71875000204837747 ) ) ;
#16426 = CARTESIAN_POINT ( 'NONE',  ( 7.644554776091147741E-16, 12.48450537969573659, -138.9687500020483810 ) ) ;
#16427 = CARTESIAN_POINT ( 'NONE',  ( 9.999999999999998224, 0.000000000000000000, -129.5000000000000000 ) ) ;
#16428 = CARTESIAN_POINT ( 'NONE',  ( -5.000000000000003553, -8.660254037844383745, -103.0000000000000000 ) ) ;
#16429 = CARTESIAN_POINT ( 'NONE',  ( -9.999999999999998224, 1.224646799147353059E-15, -161.7500000000000000 ) ) ;
#16430 = CARTESIAN_POINT ( 'NONE',  ( 10.81189881249999907, 6.242252689847868297, -1.406250002048359260 ) ) ;
#16431 = CARTESIAN_POINT ( 'NONE',  ( 10.81189881249999907, 6.242252689847868297, -74.71875000204838102 ) ) ;
#16432 = CARTESIAN_POINT ( 'NONE',  ( -10.81189881249999729, 6.242252689847871849, -44.40625000204836681 ) ) ;
#16433 = CARTESIAN_POINT ( 'NONE',  ( -10.81189881249999729, 6.242252689847871849, -57.71875000204837391 ) ) ;
#16434 = CARTESIAN_POINT ( 'NONE',  ( -9.999999999999998224, 1.224646799147353059E-15, -200.0000000000000000 ) ) ;
#16435 = CARTESIAN_POINT ( 'NONE',  ( 10.81189881249999729, 0.000000000000000000, -160.3437500020484094 ) ) ;
#16436 = EDGE_CURVE ( 'NONE', #28405, #1650, #34982, .T. ) ;
#16437 = CARTESIAN_POINT ( 'NONE',  ( 7.070501591499377789E-16, 11.54700538379251284, -132.1250000000000000 ) ) ;
#16438 = CARTESIAN_POINT ( 'NONE',  ( 5.405949406249999534, 9.363379034771803333, -142.2812500020483810 ) ) ;
#16439 = DIRECTION ( 'NONE',  ( -0.000000000000000000, -0.000000000000000000, 1.000000000000000000 ) ) ;
#16440 = CARTESIAN_POINT ( 'NONE',  ( 7.070501591499377789E-16, 11.54700538379251284, -114.5000000040967905 ) ) ;
#16441 = CARTESIAN_POINT ( 'NONE',  ( -2.121150477449813534E-15, -11.54700538379251284, -93.87499999999997158 ) ) ;
#16442 = EDGE_CURVE ( 'NONE', #16950, #12651, #39986, .T. ) ;
#16443 = ORIENTED_EDGE ( 'NONE', *, *, #22506, .F. ) ;
#16444 = CARTESIAN_POINT ( 'NONE',  ( 10.81189881249999729, 0.000000000000000000, -111.0312500020483810 ) ) ;
#16445 = CARTESIAN_POINT ( 'NONE',  ( 9.999999999999996447, -5.773502691896262640, -131.5000000040967905 ) ) ;
#16446 = CARTESIAN_POINT ( 'NONE',  ( 9.999999999998969713, 5.773502691896851502, -39.37499999999995026 ) ) ;
#16447 = EDGE_CURVE ( 'NONE', #19819, #22601, #15726, .T. ) ;
#16448 = CARTESIAN_POINT ( 'NONE',  ( -10.81189881249999729, 1.324075727343319199E-15, -170.2812500020484094 ) ) ;
#16449 = CARTESIAN_POINT ( 'NONE',  ( -9.999999999999998224, 5.773502691896259087, -40.75000000409676204 ) ) ;
#16450 = CIRCLE ( 'NONE', #39881, 24.99999999999999645 ) ;
#16451 = CARTESIAN_POINT ( 'NONE',  ( 9.999999999999998224, 0.000000000000000000, -48.87500000409678336 ) ) ;
#16452 = CARTESIAN_POINT ( 'NONE',  ( 10.81189881249999907, 6.242252689847868297, -61.40625000204838102 ) ) ;
#16453 = CARTESIAN_POINT ( 'NONE',  ( 80.00000000000002842, 39.99999999999999289, -170.0000000000000000 ) ) ;
#16454 = CARTESIAN_POINT ( 'NONE',  ( -5.405949406250003975, -9.363379034771801557, -161.0312500020484094 ) ) ;
#16455 = VECTOR ( 'NONE', #34680, 1000.000000000000000 ) ;
#16456 = CARTESIAN_POINT ( 'NONE',  ( 5.405949406249992428, -9.363379034771808662, -147.0937500020483810 ) ) ;
#16457 = CYLINDRICAL_SURFACE ( 'NONE', #4979, 9.999999999999998224 ) ;
#16458 = LINE ( 'NONE', #19923, #30323 ) ;
#16459 = ORIENTED_EDGE ( 'NONE', *, *, #26285, .F. ) ;
#16460 = CARTESIAN_POINT ( 'NONE',  ( 9.999999999999998224, 0.000000000000000000, -28.99999999999997158 ) ) ;
#16461 = ADVANCED_FACE ( 'NONE', ( #39044 ), #29134, .T. ) ;
#16462 = AXIS2_PLACEMENT_3D ( 'NONE', #235, #35638, #19843 ) ;
#16464 = VERTEX_POINT ( 'NONE', #25890 ) ;
#16463 = CARTESIAN_POINT ( 'NONE',  ( 10.81189881249999907, 6.242252689847868297, -67.40625000204839523 ) ) ;
#16465 = SHAPE_DEFINITION_REPRESENTATION ( #28039, #21658 ) ;
#16467 = ORIENTED_EDGE ( 'NONE', *, *, #22649, .T. ) ;
#16466 = CARTESIAN_POINT ( 'NONE',  ( -10.81189881249999729, 1.324075727343319199E-15, -119.0937500020483810 ) ) ;
#16468 = ORIENTED_EDGE ( 'NONE', *, *, #37813, .F. ) ;
#16469 = CARTESIAN_POINT ( 'NONE',  ( 7.644554776091147741E-16, 12.48450537969573659, -23.46875000204836326 ) ) ;
#16470 = CARTESIAN_POINT ( 'NONE',  ( 5.405949406249992428, -9.363379034771808662, -0.2812500020483721386 ) ) ;
#16471 = CARTESIAN_POINT ( 'NONE',  ( 10.81189881249999729, 0.000000000000000000, -46.34375000204838102 ) ) ;
#16472 = DIRECTION ( 'NONE',  ( -0.000000000000000000, -0.000000000000000000, 1.000000000000000000 ) ) ;
#16473 = CARTESIAN_POINT ( 'NONE',  ( -4.999999999999996447, 8.660254037844387298, -29.99999999999997158 ) ) ;
#16474 = CARTESIAN_POINT ( 'NONE',  ( 10.81189881249999729, 6.242252689847867408, -182.7187500020484094 ) ) ;
#16475 = CARTESIAN_POINT ( 'NONE',  ( 5.405949406249999534, 9.363379034771803333, -169.0937500020484094 ) ) ;
#16476 = CARTESIAN_POINT ( 'NONE',  ( 10.81189881249999729, 0.000000000000000000, -148.3437500020483810 ) ) ;
#16477 = CARTESIAN_POINT ( 'NONE',  ( -2.293366432827344421E-15, -12.48450537969573659, -165.2187500020483810 ) ) ;
#16478 = CARTESIAN_POINT ( 'NONE',  ( 7.070501591499376803E-16, 11.54700538379251284, -123.5000000040967905 ) ) ;
#16479 = CARTESIAN_POINT ( 'NONE',  ( -9.999999999999998224, 1.224646799147353059E-15, -193.6250000040967905 ) ) ;
#16480 = CARTESIAN_POINT ( 'NONE',  ( -2.121150477449813534E-15, -11.54700538379251284, -188.3750000000000284 ) ) ;
#16481 = VECTOR ( 'NONE', #23505, 1000.000000000000000 ) ;
#16482 = CARTESIAN_POINT ( 'NONE',  ( -10.81189881249999729, 6.242252689847871849, -93.71875000204838102 ) ) ;
#16483 = CARTESIAN_POINT ( 'NONE',  ( 7.070501591499376803E-16, 11.54700538379251284, -198.5000000040968189 ) ) ;
#16484 = CARTESIAN_POINT ( 'NONE',  ( 10.81189881249999907, 6.242252689847868297, -65.90625000204839523 ) ) ;
#16485 = DIRECTION ( 'NONE',  ( -0.000000000000000000, -0.000000000000000000, -1.000000000000000000 ) ) ;
#16486 = CARTESIAN_POINT ( 'NONE',  ( 7.644554776091147741E-16, 12.48450537969573659, -189.9687500020484094 ) ) ;
#16487 = CARTESIAN_POINT ( 'NONE',  ( -5.405949406249996869, 9.363379034771805109, -166.0312500020484094 ) ) ;
#16488 = CARTESIAN_POINT ( 'NONE',  ( 10.81189881249999729, 0.000000000000000000, -64.53125000204836681 ) ) ;
#16489 = CARTESIAN_POINT ( 'NONE',  ( 9.999999999999996447, -5.773502691896262640, -137.5000000040967905 ) ) ;
#16490 = CARTESIAN_POINT ( 'NONE',  ( 9.999999999999996447, -5.773502691896262640, -114.6249999999999858 ) ) ;
#16491 = ORIENTED_EDGE ( 'NONE', *, *, #29746, .F. ) ;
#16492 = AXIS2_PLACEMENT_3D ( 'NONE', #37859, #39859, #399 ) ;
#16493 = CARTESIAN_POINT ( 'NONE',  ( 7.644554776091147741E-16, 12.48450537969573659, -145.1562500020484094 ) ) ;
#16494 = CARTESIAN_POINT ( 'NONE',  ( 10.81189881249999907, 6.242252689847868297, -152.9062500020483810 ) ) ;
#16495 = CARTESIAN_POINT ( 'NONE',  ( 10.81189881249999729, 0.000000000000000000, -196.5312500020484094 ) ) ;
#16496 = DIRECTION ( 'NONE',  ( -0.000000000000000000, -0.000000000000000000, -1.000000000000000000 ) ) ;
#16497 = CARTESIAN_POINT ( 'NONE',  ( 5.405949406249992428, -9.363379034771808662, -93.09375000204838102 ) ) ;
#16498 = VERTEX_POINT ( 'NONE', #35188 ) ;
#16499 = CARTESIAN_POINT ( 'NONE',  ( 10.00000000000000000, 5.773502691896255534, -58.87499999999998579 ) ) ;
#16500 = CARTESIAN_POINT ( 'NONE',  ( -10.81189881249999729, 6.242252689847871849, -186.7187500020483810 ) ) ;
#16501 = CARTESIAN_POINT ( 'NONE',  ( 9.999999999999998224, 0.000000000000000000, -69.87500000409677625 ) ) ;
#16502 = LINE ( 'NONE', #32522, #26548 ) ;
#16503 =( BOUNDED_CURVE ( )  B_SPLINE_CURVE ( 2, ( #5928, #21896, #11746, #38508, #32260, #28174, #21468 ),
 .UNSPECIFIED., .F., .F. ) 
 B_SPLINE_CURVE_WITH_KNOTS ( ( 3, 2, 2, 3 ),
 ( 0.9402985074626868389, 0.9415422885572141132, 0.9427860696517416095, 0.9440298507462689948 ),
 .UNSPECIFIED. ) 
 CURVE ( )  GEOMETRIC_REPRESENTATION_ITEM ( )  RATIONAL_B_SPLINE_CURVE ( ( 0.9999999999999761302, 0.8660254037844625774, 1.000000000000000000, 0.8660254037844387076, 1.000000000000000000, 0.8660254037844028474, 1.000000000000035971 ) ) 
 REPRESENTATION_ITEM ( '' )  );
#16504 = CARTESIAN_POINT ( 'NONE',  ( 25.00000000000000000, 3.061616997868383043E-15, -160.0000000000000000 ) ) ;
#16505 = CARTESIAN_POINT ( 'NONE',  ( -10.81189881249999907, -6.242252689847864744, -87.65625000204836681 ) ) ;
#16506 = CARTESIAN_POINT ( 'NONE',  ( 10.81189881249999551, -6.242252689847874514, -61.65625000204838813 ) ) ;
#16507 = CARTESIAN_POINT ( 'NONE',  ( -9.999999999999998224, 5.773502691896259087, -58.75000000409677625 ) ) ;
#16508 = CARTESIAN_POINT ( 'NONE',  ( -5.405949406250003975, -9.363379034771801557, -18.34375000204835260 ) ) ;
#16509 = FACE_OUTER_BOUND ( 'NONE', #32855, .T. ) ;
#16510 = CARTESIAN_POINT ( 'NONE',  ( -10.81189881249999729, 1.324075727343319199E-15, -183.7812500020484094 ) ) ;
#16511 = EDGE_CURVE ( 'NONE', #41044, #12598, #4727, .T. ) ;
#16512 = CARTESIAN_POINT ( 'NONE',  ( -10.81189881249999729, 1.324075727343319199E-15, -14.28125000204835615 ) ) ;
#16513 = CARTESIAN_POINT ( 'NONE',  ( 0.000000000000000000, 0.000000000000000000, -200.0000000000000000 ) ) ;
#16514 = CARTESIAN_POINT ( 'NONE',  ( 10.00000000000025402, -5.773502691896113426, -117.6250000000000142 ) ) ;
#16515 = CARTESIAN_POINT ( 'NONE',  ( -9.106632906167126507, -4.221636404539722776, 0.000000000000000000 ) ) ;
#16516 = CARTESIAN_POINT ( 'NONE',  ( -7.688134889256605042, 6.454000733898044295, 0.000000000000000000 ) ) ;
#16517 = CARTESIAN_POINT ( 'NONE',  ( 10.00000000000000000, 5.773502691896255534, -168.3750000000000000 ) ) ;
#16518 = CARTESIAN_POINT ( 'NONE',  ( 9.999999999999998224, 0.000000000000000000, -159.5000000000000000 ) ) ;
#16519 = CIRCLE ( 'NONE', #30358, 9.750000000000001776 ) ;
#16521 = ORIENTED_EDGE ( 'NONE', *, *, #25421, .T. ) ;
#16520 = CARTESIAN_POINT ( 'NONE',  ( 10.81189881249999907, 6.242252689847868297, -92.90625000204839523 ) ) ;
#16522 = CARTESIAN_POINT ( 'NONE',  ( 4.999999999999992006, -8.660254037844389075, -162.7500000000000000 ) ) ;
#16524 = ORIENTED_EDGE ( 'NONE', *, *, #12285, .F. ) ;
#16523 = CARTESIAN_POINT ( 'NONE',  ( 0.000000000000000000, 0.000000000000000000, -200.0000000000000000 ) ) ;
#16525 = ORIENTED_EDGE ( 'NONE', *, *, #31200, .T. ) ;
#16526 = CARTESIAN_POINT ( 'NONE',  ( -10.81189881249999729, 1.324075727343319199E-15, -30.59375000204836326 ) ) ;
#16527 = CARTESIAN_POINT ( 'NONE',  ( -5.405949406249996869, 9.363379034771805109, -25.03125000204836681 ) ) ;
#16528 = DATE_AND_TIME ( #42019, #11485 ) ;
#16529 = CARTESIAN_POINT ( 'NONE',  ( -10.81189881249999907, -6.242252689847864744, -73.96875000204836681 ) ) ;
#16530 = CARTESIAN_POINT ( 'NONE',  ( 7.070501591499376803E-16, 11.54700538379251284, -105.1249999999999858 ) ) ;
#16531 = CARTESIAN_POINT ( 'NONE',  ( 10.81189881249999907, 6.242252689847868297, -196.2187500020484094 ) ) ;
#16532 = CARTESIAN_POINT ( 'NONE',  ( -5.405949406250003975, -9.363379034771801557, -147.3437500020483810 ) ) ;
#16533 = LINE ( 'NONE', #6426, #5407 ) ;
#16534 = PLANE ( 'NONE',  #32965 ) ;
#16535 = CARTESIAN_POINT ( 'NONE',  ( -10.81189881249999729, 1.324075727343319199E-15, -146.2812500020483810 ) ) ;
#16536 = CARTESIAN_POINT ( 'NONE',  ( 7.070501591499377789E-16, 11.54700538379251284, -0.5000000040967461645 ) ) ;
#16537 = CARTESIAN_POINT ( 'NONE',  ( 7.070501591499376803E-16, 11.54700538379251284, -121.6249999999999858 ) ) ;
#16538 = CARTESIAN_POINT ( 'NONE',  ( -10.81189881249999729, 6.242252689847871849, -117.7187500020483952 ) ) ;
#16539 = CARTESIAN_POINT ( 'NONE',  ( -10.81189881249999729, 6.242252689847871849, -95.40625000204838102 ) ) ;
#16540 = CARTESIAN_POINT ( 'NONE',  ( 5.405949406249992428, -9.363379034771808662, -105.0937500020483810 ) ) ;
#16541 = CARTESIAN_POINT ( 'NONE',  ( 10.81189881249999907, 6.242252689847868297, -77.71875000204838102 ) ) ;
#16542 = CARTESIAN_POINT ( 'NONE',  ( 10.81189881249999729, 0.000000000000000000, -84.03125000204838102 ) ) ;
#16543 = CARTESIAN_POINT ( 'NONE',  ( 9.999999999999998224, 0.000000000000000000, -162.8750000040967905 ) ) ;
#16544 =( BOUNDED_CURVE ( )  B_SPLINE_CURVE ( 2, ( #16061, #38538, #28842, #16267, #31879, #26019, #22146 ),
 .UNSPECIFIED., .F., .F. ) 
 B_SPLINE_CURVE_WITH_KNOTS ( ( 3, 2, 2, 3 ),
 ( 0.9029850746268659467, 0.9042288557213932210, 0.9054726368159207173, 0.9067164179104481025 ),
 .UNSPECIFIED. ) 
 CURVE ( )  GEOMETRIC_REPRESENTATION_ITEM ( )  RATIONAL_B_SPLINE_CURVE ( ( 0.9999999999999761302, 0.8660254037844625774, 1.000000000000000000, 0.8660254037844387076, 1.000000000000000000, 0.8660254037844028474, 1.000000000000035971 ) ) 
 REPRESENTATION_ITEM ( '' )  );
#16545 = CARTESIAN_POINT ( 'NONE',  ( 0.000000000000000000, 0.000000000000000000, -200.0000000000000000 ) ) ;
#16546 = CARTESIAN_POINT ( 'NONE',  ( -10.81189881249999729, 6.242252689847871849, -162.9062500020483810 ) ) ;
#16547 = CARTESIAN_POINT ( 'NONE',  ( -10.81189881249999729, 6.242252689847871849, -182.4062500020483810 ) ) ;
#16548 = AXIS2_PLACEMENT_3D ( 'NONE', #33008, #6884, #33230 ) ;
#16549 = CARTESIAN_POINT ( 'NONE',  ( 4.999999999999992006, -8.660254037844389075, -154.1250000040967905 ) ) ;
#16550 = CARTESIAN_POINT ( 'NONE',  ( -2.121150477449813534E-15, -11.54700538379251284, -189.8750000000000284 ) ) ;
#16551 = CARTESIAN_POINT ( 'NONE',  ( 5.405949406249992428, -9.363379034771808662, -4.593750002048368586 ) ) ;
#16552 = CARTESIAN_POINT ( 'NONE',  ( -2.121150477449813534E-15, -11.54700538379251284, -108.8749999999999858 ) ) ;
#16553 = CARTESIAN_POINT ( 'NONE',  ( 5.405949406249992428, -9.363379034771808662, -114.0937500020483810 ) ) ;
#16554 = CARTESIAN_POINT ( 'NONE',  ( 4.999999999999992006, -8.660254037844389075, -81.74999999999998579 ) ) ;
#16555 = CARTESIAN_POINT ( 'NONE',  ( -10.81189881249999907, -6.242252689847864744, -12.65625000204837036 ) ) ;
#16556 = CARTESIAN_POINT ( 'NONE',  ( 4.999999999999992006, -8.660254037844389075, -86.62500000409677625 ) ) ;
#16557 = CARTESIAN_POINT ( 'NONE',  ( -9.999999999999998224, 0.000000000000000000, -99.99999999999998579 ) ) ;
#16558 = CARTESIAN_POINT ( 'NONE',  ( 10.81189881249999551, -6.242252689847874514, -111.1562500020483952 ) ) ;
#16559 = CARTESIAN_POINT ( 'NONE',  ( -5.405949406249996869, 9.363379034771805109, -88.03125000204838102 ) ) ;
#16560 = ORIENTED_EDGE ( 'NONE', *, *, #22628, .T. ) ;
#16561 =( BOUNDED_CURVE ( )  B_SPLINE_CURVE ( 2, ( #19764, #26049, #22807, #39827, #29282, #7247, #10260 ),
 .UNSPECIFIED., .F., .F. ) 
 B_SPLINE_CURVE_WITH_KNOTS ( ( 3, 2, 2, 3 ),
 ( 0.5970149253731344974, 0.5982587064676618827, 0.5995024875621891569, 0.6007462686567165422 ),
 .UNSPECIFIED. ) 
 CURVE ( )  GEOMETRIC_REPRESENTATION_ITEM ( )  RATIONAL_B_SPLINE_CURVE ( ( 0.9999999999999761302, 0.8660254037844625774, 1.000000000000000000, 0.8660254037844387076, 1.000000000000000000, 0.8660254037844267172, 1.000000000000011990 ) ) 
 REPRESENTATION_ITEM ( '' )  );
#16562 = CARTESIAN_POINT ( 'NONE',  ( -2.121150477449813534E-15, -11.54700538379251284, -83.75000000409677625 ) ) ;
#16563 = CARTESIAN_POINT ( 'NONE',  ( 10.00000000000051159, -5.773502691895965988, -140.5000000040967620 ) ) ;
#16564 = CARTESIAN_POINT ( 'NONE',  ( 10.81189881249999729, 0.000000000000000000, -40.34375000204837391 ) ) ;
#16565 = ORIENTED_EDGE ( 'NONE', *, *, #17901, .F. ) ;
#16566 = CARTESIAN_POINT ( 'NONE',  ( -2.121150477449813534E-15, -11.54700538379251284, -9.874999999999982236 ) ) ;
#16567 = CARTESIAN_POINT ( 'NONE',  ( -9.999999999999998224, 1.224646799147353059E-15, -142.2500000000000000 ) ) ;
#16568 = DIRECTION ( 'NONE',  ( -0.000000000000000000, -0.000000000000000000, 1.000000000000000000 ) ) ;
#16569 = CARTESIAN_POINT ( 'NONE',  ( 7.070501591499377789E-16, 11.54700538379251284, -15.50000000409676382 ) ) ;
#16570 = CARTESIAN_POINT ( 'NONE',  ( 5.000000000000000000, 8.660254037844385522, -189.2500000000000000 ) ) ;
#16572 = ORIENTED_EDGE ( 'NONE', *, *, #20226, .T. ) ;
#16571 = CARTESIAN_POINT ( 'NONE',  ( -10.81189881249999907, -6.242252689847864744, -116.1562500020483952 ) ) ;
#16573 = CARTESIAN_POINT ( 'NONE',  ( -4.999999999999996447, 8.660254037844387298, -13.49999999999995737 ) ) ;
#16574 = ADVANCED_FACE ( 'NONE', ( #12284 ), #22641, .F. ) ;
#16575 = EDGE_LOOP ( 'NONE', ( #25482, #41835, #24745, #16305 ) ) ;
#16576 = CARTESIAN_POINT ( 'NONE',  ( -10.81189881249999729, 6.242252689847871849, -48.90625000204836681 ) ) ;
#16577 = CALENDAR_DATE ( 2026, 28, 9 ) ;
#16578 = CARTESIAN_POINT ( 'NONE',  ( -10.81189881249999907, -6.242252689847864744, -96.46875000204838102 ) ) ;
#16579 = CARTESIAN_POINT ( 'NONE',  ( -2.293366432827344421E-15, -12.48450537969573659, -120.4062500020483952 ) ) ;
#16580 = ORIENTED_EDGE ( 'NONE', *, *, #38580, .F. ) ;
#16581 = DIRECTION ( 'NONE',  ( -0.000000000000000000, -0.000000000000000000, 1.000000000000000000 ) ) ;
#16582 = CARTESIAN_POINT ( 'NONE',  ( 9.999999999999998224, 0.000000000000000000, -128.3750000040967905 ) ) ;
#16583 = CARTESIAN_POINT ( 'NONE',  ( 10.81189881249999729, 0.000000000000000000, -178.5312500020483810 ) ) ;
#16584 = CYLINDRICAL_SURFACE ( 'NONE', #39018, 9.999999999999998224 ) ;
#16585 = CARTESIAN_POINT ( 'NONE',  ( -10.81189881249999729, -6.242252689847864744, -132.4687500020483810 ) ) ;
#16586 = CARTESIAN_POINT ( 'NONE',  ( -5.405949406249996869, 9.363379034771805109, -104.3437500020483810 ) ) ;
#16587 = CARTESIAN_POINT ( 'NONE',  ( 4.999999999999992006, -8.660254037844389075, -158.2500000000000000 ) ) ;
#16588 = CARTESIAN_POINT ( 'NONE',  ( 7.644554776091147741E-16, 12.48450537969573659, -112.1562500020483810 ) ) ;
#16589 = CARTESIAN_POINT ( 'NONE',  ( 7.070501591499377789E-16, 11.54700538379251284, -186.5000000040967905 ) ) ;
#16590 = CARTESIAN_POINT ( 'NONE',  ( -5.405949406249996869, 9.363379034771805109, -114.8437500020483810 ) ) ;
#16591 = CARTESIAN_POINT ( 'NONE',  ( -10.81189881249999729, 1.324075727343319199E-15, -186.7812500020484094 ) ) ;
#16592 = CARTESIAN_POINT ( 'NONE',  ( -9.999999999999998224, 1.224646799147353059E-15, -6.125000004096770034 ) ) ;
#16593 = DIRECTION ( 'NONE',  ( 1.000000000000000000, 0.000000000000000000, 0.000000000000000000 ) ) ;
#16594 = CARTESIAN_POINT ( 'NONE',  ( 5.000000000000000000, 8.660254037844385522, -135.2499999999999716 ) ) ;
#16595 = CARTESIAN_POINT ( 'NONE',  ( -4.999999999999996447, 8.660254037844387298, -1.499999999999973577 ) ) ;
#16596 = CARTESIAN_POINT ( 'NONE',  ( -10.81189881249999729, -6.242252689847864744, -63.46875000204838102 ) ) ;
#16597 = CARTESIAN_POINT ( 'NONE',  ( 7.644554776091147741E-16, 12.48450537969573659, -45.96875000204837391 ) ) ;
#16598 = CARTESIAN_POINT ( 'NONE',  ( 5.000000000000000000, 8.660254037844385522, -182.1250000040967905 ) ) ;
#16599 = CARTESIAN_POINT ( 'NONE',  ( -5.405949406249996869, 9.363379034771805109, -19.03125000204835970 ) ) ;
#16600 = CARTESIAN_POINT ( 'NONE',  ( -10.81189881249999729, 1.324075727343319199E-15, -32.09375000204836681 ) ) ;
#16601 = CARTESIAN_POINT ( 'NONE',  ( 9.999999999999998224, 0.000000000000000000, -92.37500000409677625 ) ) ;
#16602 = CARTESIAN_POINT ( 'NONE',  ( 7.644554776091147741E-16, 12.48450537969573659, -137.4687500020483810 ) ) ;
#16603 = CARTESIAN_POINT ( 'NONE',  ( -9.999999999999998224, 1.224646799147353059E-15, -109.2499999999999858 ) ) ;
#16604 = CARTESIAN_POINT ( 'NONE',  ( 10.81189881249999907, 6.242252689847868297, -35.90625000204835970 ) ) ;
#16605 = CARTESIAN_POINT ( 'NONE',  ( 5.000000000000000000, 8.660254037844385522, -163.7500000000000000 ) ) ;
#16606 = CARTESIAN_POINT ( 'NONE',  ( 9.999999999999996447, -5.773502691896262640, -66.62499999999998579 ) ) ;
#16607 = CARTESIAN_POINT ( 'NONE',  ( -2.293366432827344421E-15, -12.48450537969573659, -129.4062500020483810 ) ) ;
#16608 = CARTESIAN_POINT ( 'NONE',  ( -10.81189881249999729, -6.242252689847864744, -119.1562500020484237 ) ) ;
#16609 = ORIENTED_EDGE ( 'NONE', *, *, #2895, .T. ) ;
#16610 = AXIS2_PLACEMENT_3D ( 'NONE', #24461, #17732, #25103 ) ;
#16611 = CARTESIAN_POINT ( 'NONE',  ( 10.00000000000102318, -5.773502691895667560, -6.624999999999941380 ) ) ;
#16612 = CARTESIAN_POINT ( 'NONE',  ( 10.00000000000000000, 5.773502691896255534, -111.7500000040967763 ) ) ;
#16613 = CARTESIAN_POINT ( 'NONE',  ( -10.81189881249999729, 1.324075727343319199E-15, -69.59375000204836681 ) ) ;
#16614 = ORIENTED_EDGE ( 'NONE', *, *, #5437, .F. ) ;
#16615 = CARTESIAN_POINT ( 'NONE',  ( 9.999999999999996447, -5.773502691896262640, -35.12499999999996447 ) ) ;
#16616 = CC_DESIGN_SECURITY_CLASSIFICATION ( #33910, ( #28392 ) ) ;
#16617 = CARTESIAN_POINT ( 'NONE',  ( 9.999999999999996447, -5.773502691896262640, -20.50000000409677625 ) ) ;
#16618 = CARTESIAN_POINT ( 'NONE',  ( 5.405949406249992428, -9.363379034771808662, -43.78125000204838102 ) ) ;
#16619 = DIRECTION ( 'NONE',  ( -0.000000000000000000, -0.000000000000000000, 1.000000000000000000 ) ) ;
#16620 = CARTESIAN_POINT ( 'NONE',  ( 9.999999999999996447, -5.773502691896262640, -38.50000000409676204 ) ) ;
#16621 = CARTESIAN_POINT ( 'NONE',  ( 9.999999999999998224, 0.000000000000000000, -156.8750000040967905 ) ) ;
#16622 = VECTOR ( 'NONE', #34014, 1000.000000000000000 ) ;
#16623 = CARTESIAN_POINT ( 'NONE',  ( 10.81189881249999729, 0.000000000000000000, -145.5312500020483810 ) ) ;
#16624 =( BOUNDED_CURVE ( )  B_SPLINE_CURVE ( 2, ( #5905, #42136, #2035, #24704, #37850, #8293, #12146 ),
 .UNSPECIFIED., .F., .F. ) 
 B_SPLINE_CURVE_WITH_KNOTS ( ( 3, 2, 2, 3 ),
 ( 0.6417910447761195902, 0.6430348258706469755, 0.6442786069651742498, 0.6455223880597016350 ),
 .UNSPECIFIED. ) 
 CURVE ( )  GEOMETRIC_REPRESENTATION_ITEM ( )  RATIONAL_B_SPLINE_CURVE ( ( 0.9999999999999761302, 0.8660254037844625774, 1.000000000000000000, 0.8660254037844387076, 1.000000000000000000, 0.8660254037844267172, 1.000000000000011990 ) ) 
 REPRESENTATION_ITEM ( '' )  );
#16625 = CARTESIAN_POINT ( 'NONE',  ( -9.999999999998969713, -5.773502691896847949, -16.12499999999995737 ) ) ;
#16626 = ORIENTED_EDGE ( 'NONE', *, *, #631, .T. ) ;
#16627 = EDGE_LOOP ( 'NONE', ( #39522, #16992, #19829, #15938 ) ) ;
#16628 = EDGE_CURVE ( 'NONE', #6595, #12803, #19842, .T. ) ;
#16629 = VERTEX_POINT ( 'NONE', #32769 ) ;
#16630 = ADVANCED_FACE ( 'NONE', ( #29317 ), #36424, .F. ) ;
#16631 = CARTESIAN_POINT ( 'NONE',  ( 9.999999999999998224, 0.000000000000000000, -120.8750000040967905 ) ) ;
#16632 = CARTESIAN_POINT ( 'NONE',  ( 5.405949406249992428, -9.363379034771808662, -175.5937500020484094 ) ) ;
#16633 = ORGANIZATION ( 'NAUO-ORG3', 'UNSPECIFIED', 'UNSPECIFIED' ) ;
#16634 = CARTESIAN_POINT ( 'NONE',  ( -10.81189881249999729, 1.324075727343319199E-15, -21.59375000204835615 ) ) ;
#16635 = CARTESIAN_POINT ( 'NONE',  ( 5.000000000000000000, 8.660254037844385522, -144.6250000040967905 ) ) ;
#16636 = CARTESIAN_POINT ( 'NONE',  ( -10.81189881249999729, -6.242252689847864744, -156.4687500020484094 ) ) ;
#16637 = CARTESIAN_POINT ( 'NONE',  ( -2.293366432827344421E-15, -12.48450537969573659, -145.7187500020484094 ) ) ;
#16638 = CARTESIAN_POINT ( 'NONE',  ( 7.070501591499376803E-16, 11.54700538379251284, -67.62500000000000000 ) ) ;
#16639 = CARTESIAN_POINT ( 'NONE',  ( -10.81189881249999907, -6.242252689847864744, -123.4687500020483810 ) ) ;
#16640 = CARTESIAN_POINT ( 'NONE',  ( -5.405949406249996869, 9.363379034771805109, -134.5312500020484094 ) ) ;
#16641 = CARTESIAN_POINT ( 'NONE',  ( 7.644554776091147741E-16, 12.48450537969573659, -6.968750002048349046 ) ) ;
#16642 = CARTESIAN_POINT ( 'NONE',  ( 10.81189881249999729, 6.242252689847867408, -140.7187500020483810 ) ) ;
#16643 = CYLINDRICAL_SURFACE ( 'NONE', #2653, 9.999999999999998224 ) ;
#16644 = DIRECTION ( 'NONE',  ( -0.000000000000000000, -0.000000000000000000, 1.000000000000000000 ) ) ;
#16645 = CARTESIAN_POINT ( 'NONE',  ( -5.000000000000003553, -8.660254037844383745, -161.5000000000000000 ) ) ;
#16646 = CARTESIAN_POINT ( 'NONE',  ( 9.999999999999998224, 0.000000000000000000, -100.9999999999999858 ) ) ;
#16647 = CIRCLE ( 'NONE', #12542, 10.00000000000000178 ) ;
#16648 = CARTESIAN_POINT ( 'NONE',  ( -2.293366432827344421E-15, -12.48450537969573659, -73.71875000204835260 ) ) ;
#16649 = CARTESIAN_POINT ( 'NONE',  ( 7.644554776091147741E-16, 12.48450537969573659, -46.15625000204837391 ) ) ;
#16650 = CARTESIAN_POINT ( 'NONE',  ( 10.81189881249999729, 0.000000000000000000, -52.34375000204835260 ) ) ;
#16651 = CARTESIAN_POINT ( 'NONE',  ( 9.999999999999998224, 0.000000000000000000, -57.49999999999996447 ) ) ;
#16652 = CARTESIAN_POINT ( 'NONE',  ( -2.293366432827344421E-15, -12.48450537969573659, -162.2187500020483810 ) ) ;
#16653 = CARTESIAN_POINT ( 'NONE',  ( -10.00000000000000000, -5.773502691896251982, -127.1249999999999858 ) ) ;
#16654 = CARTESIAN_POINT ( 'NONE',  ( 7.644554776091147741E-16, 12.48450537969573659, -136.1562500020484094 ) ) ;
#16655 = CARTESIAN_POINT ( 'NONE',  ( -9.999999999999479527, -5.773502691896549521, -151.1250000000000000 ) ) ;
#16656 = CARTESIAN_POINT ( 'NONE',  ( -9.999999999999998224, 5.773502691896259087, -117.2500000040967763 ) ) ;
#16657 = CARTESIAN_POINT ( 'NONE',  ( 4.999999999999992006, -8.660254037844389075, -90.74999999999998579 ) ) ;
#16658 = ORIENTED_EDGE ( 'NONE', *, *, #39473, .T. ) ;
#16659 = CARTESIAN_POINT ( 'NONE',  ( -2.293366432827344421E-15, -12.48450537969573659, -114.4062500020483952 ) ) ;
#16660 = CARTESIAN_POINT ( 'NONE',  ( 4.999999999999992006, -8.660254037844389075, -130.1250000040967620 ) ) ;
#16661 = CARTESIAN_POINT ( 'NONE',  ( 9.999999999999998224, 0.000000000000000000, -200.0000000000000000 ) ) ;
#16662 = CARTESIAN_POINT ( 'NONE',  ( 10.81189881249999907, 6.242252689847868297, -167.9062500020484094 ) ) ;
#16663 = CARTESIAN_POINT ( 'NONE',  ( -2.121150477449813534E-15, -11.54700538379251284, -41.75000000409675494 ) ) ;
#16664 = DIRECTION ( 'NONE',  ( 1.000000000000000000, 0.000000000000000000, 0.000000000000000000 ) ) ;
#16665 = CARTESIAN_POINT ( 'NONE',  ( -10.81189881249999907, -6.242252689847864744, -51.65625000204837391 ) ) ;
#16666 = AXIS2_PLACEMENT_3D ( 'NONE', #10487, #23676, #32751 ) ;
#16667 =( BOUNDED_CURVE ( )  B_SPLINE_CURVE ( 2, ( #14041, #1134, #6964, #7174, #11038, #27237, #20326 ),
 .UNSPECIFIED., .F., .F. ) 
 B_SPLINE_CURVE_WITH_KNOTS ( ( 3, 2, 2, 3 ),
 ( 0.06716417910447768091, 0.06840796019900503844, 0.06965174129353240984, 0.07089552238805976736 ),
 .UNSPECIFIED. ) 
 CURVE ( )  GEOMETRIC_REPRESENTATION_ITEM ( )  RATIONAL_B_SPLINE_CURVE ( ( 0.9999999999999924505, 0.8660254037844461461, 1.000000000000000000, 0.8660254037844387076, 1.000000000000000000, 0.8660254037844312691, 1.000000000000007550 ) ) 
 REPRESENTATION_ITEM ( '' )  );
#16668 = CARTESIAN_POINT ( 'NONE',  ( 10.40594940624999865, 0.000000000000000000, -199.7656250010242047 ) ) ;
#16669 = CARTESIAN_POINT ( 'NONE',  ( 5.405949406249999534, 9.363379034771803333, -161.7812500020484094 ) ) ;
#16670 = CARTESIAN_POINT ( 'NONE',  ( -10.81189881249999729, 1.324075727343319199E-15, -138.5937500020483810 ) ) ;
#16671 = CARTESIAN_POINT ( 'NONE',  ( 9.999999999999998224, 0.000000000000000000, -200.0000000000000000 ) ) ;
#16672 = CARTESIAN_POINT ( 'NONE',  ( -9.999999999999998224, 1.224646799147353059E-15, -149.7500000000000000 ) ) ;
#16673 = ORIENTED_EDGE ( 'NONE', *, *, #40653, .F. ) ;
#16674 = CARTESIAN_POINT ( 'NONE',  ( -4.999999999999996447, 8.660254037844387298, -189.3750000040967905 ) ) ;
#16675 = AXIS2_PLACEMENT_3D ( 'NONE', #17729, #15135, #1792 ) ;
#16677 = ORIENTED_EDGE ( 'NONE', *, *, #15933, .F. ) ;
#16676 = CARTESIAN_POINT ( 'NONE',  ( -2.293366432827344421E-15, -12.48450537969573659, -72.40625000204836681 ) ) ;
#16678 = MECHANICAL_CONTEXT ( 'NONE', #13467, 'mechanical' ) ;
#16679 = ADVANCED_FACE ( 'NONE', ( #26083 ), #39650, .F. ) ;
#16681 = ORIENTED_EDGE ( 'NONE', *, *, #6386, .T. ) ;
#16680 = CARTESIAN_POINT ( 'NONE',  ( -5.405949406250003975, -9.363379034771801557, -120.3437500020483952 ) ) ;
#16682 = ORIENTED_EDGE ( 'NONE', *, *, #11456, .T. ) ;
#16683 = EDGE_CURVE ( 'NONE', #18938, #40615, #33204, .T. ) ;
#16684 = CARTESIAN_POINT ( 'NONE',  ( 10.81189881249999729, 0.000000000000000000, -19.34375000204835260 ) ) ;
#16685 = CARTESIAN_POINT ( 'NONE',  ( 10.81189881249999907, 6.242252689847868297, -196.2187500020484094 ) ) ;
#16686 = CARTESIAN_POINT ( 'NONE',  ( -2.293366432827344421E-15, -12.48450537969573659, -43.71875000204835970 ) ) ;
#16687 = CARTESIAN_POINT ( 'NONE',  ( 0.000000000000000000, 0.000000000000000000, -200.0000000000000000 ) ) ;
#16688 = CARTESIAN_POINT ( 'NONE',  ( 0.000000000000000000, 0.000000000000000000, -200.0000000000000000 ) ) ;
#16689 = CARTESIAN_POINT ( 'NONE',  ( 10.81189881249999551, -6.242252689847874514, -179.9687500020484094 ) ) ;
#16690 = CARTESIAN_POINT ( 'NONE',  ( 5.405949406249992428, -9.363379034771808662, -172.5937500020484094 ) ) ;
#16691 = CC_DESIGN_PERSON_AND_ORGANIZATION_ASSIGNMENT ( #39894, #10325, ( #24384 ) ) ;
#16692 = CARTESIAN_POINT ( 'NONE',  ( -10.81189881249999729, 1.324075727343319199E-15, -153.5937500020483810 ) ) ;
#16693 = CARTESIAN_POINT ( 'NONE',  ( 10.81189881249999729, 6.242252689847867408, -164.7187500020483810 ) ) ;
#16694 = DIRECTION ( 'NONE',  ( -0.000000000000000000, -0.000000000000000000, 1.000000000000000000 ) ) ;
#16695 = CARTESIAN_POINT ( 'NONE',  ( 0.000000000000000000, 0.000000000000000000, -200.0000000000000000 ) ) ;
#16696 = CARTESIAN_POINT ( 'NONE',  ( -10.00000000000000000, -5.773502691896251982, -184.1250000000000284 ) ) ;
#16697 = CARTESIAN_POINT ( 'NONE',  ( -10.81189881249999907, -6.242252689847864744, -100.9687500020483810 ) ) ;
#16698 = LINE ( 'NONE', #36994, #23800 ) ;
#16699 = CARTESIAN_POINT ( 'NONE',  ( -5.405949406249996869, 9.363379034771805109, -65.53125000204838102 ) ) ;
#16700 = CARTESIAN_POINT ( 'NONE',  ( 0.000000000000000000, 0.000000000000000000, -99.99999999999998579 ) ) ;
#16701 = CARTESIAN_POINT ( 'NONE',  ( -5.405949406249996869, 9.363379034771805109, -186.8437500020483810 ) ) ;
#16702 = CARTESIAN_POINT ( 'NONE',  ( 10.81189881249999907, 6.242252689847868297, -119.9062500020483810 ) ) ;
#16703 = CARTESIAN_POINT ( 'NONE',  ( 7.644554776091147741E-16, 12.48450537969573659, -166.1562500020483810 ) ) ;
#16704 = CARTESIAN_POINT ( 'NONE',  ( 5.405949406249999534, 9.363379034771803333, -50.78125000204835970 ) ) ;
#16705 = CARTESIAN_POINT ( 'NONE',  ( -10.00000000000000000, -5.773502691896251982, -139.5000000040967905 ) ) ;
#16706 = CARTESIAN_POINT ( 'NONE',  ( 9.999999999999996447, -5.773502691896262640, -113.1250000000000000 ) ) ;
#16707 = ORIENTED_EDGE ( 'NONE', *, *, #21426, .F. ) ;
#16708 = CARTESIAN_POINT ( 'NONE',  ( 7.644554776091147741E-16, 12.48450537969573659, -131.6562500020483810 ) ) ;
#16709 = CARTESIAN_POINT ( 'NONE',  ( 10.81189881249999907, 6.242252689847868297, -151.4062500020484094 ) ) ;
#16710 = ADVANCED_FACE ( 'NONE', ( #3205 ), #9672, .F. ) ;
#16711 = VECTOR ( 'NONE', #39246, 1000.000000000000000 ) ;
#16712 = CARTESIAN_POINT ( 'NONE',  ( 5.405949406249992428, -9.363379034771808662, -190.7812500020484094 ) ) ;
#16713 = CARTESIAN_POINT ( 'NONE',  ( -10.00000000000102496, 5.773502691895664007, -130.7500000040967620 ) ) ;
#16714 = CARTESIAN_POINT ( 'NONE',  ( 10.81189881249999729, 0.000000000000000000, -85.34375000204836681 ) ) ;
#16715 = ORIENTED_EDGE ( 'NONE', *, *, #18180, .F. ) ;
#16716 = CARTESIAN_POINT ( 'NONE',  ( -10.00000000000000000, -5.773502691896251982, -61.12499999999998579 ) ) ;
#16717 = CARTESIAN_POINT ( 'NONE',  ( -5.405949406249996869, 9.363379034771805109, -183.8437500020483810 ) ) ;
#16718 = CARTESIAN_POINT ( 'NONE',  ( -10.00000000000000000, -5.773502691896251982, -69.00000000409677625 ) ) ;
#16719 = CARTESIAN_POINT ( 'NONE',  ( 0.000000000000000000, 0.000000000000000000, -200.0000000000000000 ) ) ;
#16720 = DIRECTION ( 'NONE',  ( -1.000000000000000000, 0.000000000000000000, 0.000000000000000000 ) ) ;
#16721 = CARTESIAN_POINT ( 'NONE',  ( 5.405949406249999534, 9.363379034771803333, -76.28125000204838102 ) ) ;
#16722 = CARTESIAN_POINT ( 'NONE',  ( -5.405949406249996869, 9.363379034771805109, -58.03125000204836681 ) ) ;
#16723 = CARTESIAN_POINT ( 'NONE',  ( 9.999999999999996447, -5.773502691896262640, -58.00000000409677625 ) ) ;
#16724 = CARTESIAN_POINT ( 'NONE',  ( 5.405949406249992428, -9.363379034771808662, -9.093750002048345493 ) ) ;
#16725 = CARTESIAN_POINT ( 'NONE',  ( 9.999999999999994671, -5.773502691896262640, -137.5000000040967905 ) ) ;
#16726 = CARTESIAN_POINT ( 'NONE',  ( 10.81189881249999551, -6.242252689847874514, -187.6562500020484379 ) ) ;
#16727 = CARTESIAN_POINT ( 'NONE',  ( -10.81189881249999907, -6.242252689847864744, -14.15625000204837036 ) ) ;
#16728 = DIRECTION ( 'NONE',  ( -1.000000000000000000, 0.000000000000000000, 0.000000000000000000 ) ) ;
#16729 = DIRECTION ( 'NONE',  ( 1.000000000000000000, 0.000000000000000000, 0.000000000000000000 ) ) ;
#16730 = CARTESIAN_POINT ( 'NONE',  ( -9.096586351904823786, 4.244250262519885020, 0.000000000000000000 ) ) ;
#16731 = CARTESIAN_POINT ( 'NONE',  ( 5.000000000000000000, 8.660254037844385522, -168.2500000000000000 ) ) ;
#16732 = CARTESIAN_POINT ( 'NONE',  ( -2.121150477449813534E-15, -11.54700538379251284, -169.2500000040968189 ) ) ;
#16734 = VERTEX_POINT ( 'NONE', #16120 ) ;
#16733 = CARTESIAN_POINT ( 'NONE',  ( -10.81189881249999907, -6.242252689847864744, -93.65625000204840944 ) ) ;
#16735 = CARTESIAN_POINT ( 'NONE',  ( -9.999999999999998224, 1.224646799147353059E-15, -163.2500000000000000 ) ) ;
#16737 = ORIENTED_EDGE ( 'NONE', *, *, #3279, .T. ) ;
#16736 = CARTESIAN_POINT ( 'NONE',  ( 0.000000000000000000, 0.000000000000000000, -200.0000000000000000 ) ) ;
#16738 = VERTEX_POINT ( 'NONE', #32984 ) ;
#16739 = CARTESIAN_POINT ( 'NONE',  ( 5.405949406249992428, -9.363379034771808662, -33.09375000204836681 ) ) ;
#16740 = CARTESIAN_POINT ( 'NONE',  ( -10.81189881249999907, -6.242252689847864744, -18.65625000204837036 ) ) ;
#16741 = PERSON_AND_ORGANIZATION ( #1703, #37688 ) ;
#16742 = CARTESIAN_POINT ( 'NONE',  ( -5.405949406249996869, 9.363379034771805109, -72.84375000204838102 ) ) ;
#16743 = CARTESIAN_POINT ( 'NONE',  ( -5.405949406250003975, -9.363379034771801557, -193.8437500020484094 ) ) ;
#16744 = CARTESIAN_POINT ( 'NONE',  ( 5.405949406249992428, -9.363379034771808662, -151.5937500020483810 ) ) ;
#16745 = CARTESIAN_POINT ( 'NONE',  ( -9.999999999999998224, 1.224646799147353059E-15, -98.74999999999998579 ) ) ;
#16746 = PLANE ( 'NONE',  #3291 ) ;
#16747 = CARTESIAN_POINT ( 'NONE',  ( -5.405949406250003975, -9.363379034771801557, -152.0312500020484094 ) ) ;
#16748 = CARTESIAN_POINT ( 'NONE',  ( -5.000000000000003553, -8.660254037844383745, -4.375000004096768258 ) ) ;
#16749 = CARTESIAN_POINT ( 'NONE',  ( -9.999999999999227285, -5.773502691896698735, -103.5000000040967336 ) ) ;
#16750 = EDGE_CURVE ( 'NONE', #5023, #33176, #16762, .T. ) ;
#16751 = CARTESIAN_POINT ( 'NONE',  ( -10.81189881249999907, -6.242252689847864744, -121.9687500020483952 ) ) ;
#16752 = DIRECTION ( 'NONE',  ( -1.000000000000000000, 0.000000000000000000, 0.000000000000000000 ) ) ;
#16753 = CARTESIAN_POINT ( 'NONE',  ( 7.644554776091147741E-16, 12.48450537969573659, -91.15625000204838102 ) ) ;
#16754 = CARTESIAN_POINT ( 'NONE',  ( 7.644554776091147741E-16, 12.48450537969573659, -107.4687500020483668 ) ) ;
#16755 =( BOUNDED_CURVE ( )  B_SPLINE_CURVE ( 2, ( #20343, #31152, #7841, #14495, #20989, #27050, #34176 ),
 .UNSPECIFIED., .F., .F. ) 
 B_SPLINE_CURVE_WITH_KNOTS ( ( 3, 2, 2, 3 ),
 ( 0.7873134328358211143, 0.7885572139303484995, 0.7898009950248758848, 0.7910447761194031591 ),
 .UNSPECIFIED. ) 
 CURVE ( )  GEOMETRIC_REPRESENTATION_ITEM ( )  RATIONAL_B_SPLINE_CURVE ( ( 0.9999999999999761302, 0.8660254037844625774, 1.000000000000000000, 0.8660254037844387076, 1.000000000000000000, 0.8660254037844148378, 1.000000000000023981 ) ) 
 REPRESENTATION_ITEM ( '' )  );
#16756 = CARTESIAN_POINT ( 'NONE',  ( 10.81189881249999907, 6.242252689847868297, -68.71875000204838102 ) ) ;
#16757 = CARTESIAN_POINT ( 'NONE',  ( 10.81189881249999907, 6.242252689847868297, -74.90625000204839523 ) ) ;
#16758 = CARTESIAN_POINT ( 'NONE',  ( 4.999999999999992006, -8.660254037844389075, -164.6250000040967905 ) ) ;
#16759 = CARTESIAN_POINT ( 'NONE',  ( -9.999999999999998224, 1.224646799147353059E-15, -200.0000000000000000 ) ) ;
#16760 = CARTESIAN_POINT ( 'NONE',  ( 10.81189881249999729, 0.000000000000000000, -162.0312500020484094 ) ) ;
#16761 = CARTESIAN_POINT ( 'NONE',  ( 10.81189881249999729, 0.000000000000000000, -169.5312500020484094 ) ) ;
#16762 = LINE ( 'NONE', #9881, #18733 ) ;
#16763 = CARTESIAN_POINT ( 'NONE',  ( -10.81189881249999729, 1.324075727343319199E-15, -2.093750002048366810 ) ) ;
#16764 = CARTESIAN_POINT ( 'NONE',  ( -25.00000000000000000, 0.000000000000000000, -160.0000000000000000 ) ) ;
#16765 = CARTESIAN_POINT ( 'NONE',  ( 5.405949406249999534, 9.363379034771803333, -104.5937500020483810 ) ) ;
#16766 = CARTESIAN_POINT ( 'NONE',  ( 5.000000000000000000, 8.660254037844385522, -78.24999999999998579 ) ) ;
#16767 = CARTESIAN_POINT ( 'NONE',  ( 10.81189881249999551, -6.242252689847874514, -9.156250002048365033 ) ) ;
#16768 = CARTESIAN_POINT ( 'NONE',  ( 4.999999999999992006, -8.660254037844389075, -89.62500000409677625 ) ) ;
#16769 = CARTESIAN_POINT ( 'NONE',  ( -2.121150477449813534E-15, -11.54700538379251284, -133.2500000040967905 ) ) ;
#16770 = CARTESIAN_POINT ( 'NONE',  ( 7.644554776091147741E-16, 12.48450537969573659, -112.1562500020483810 ) ) ;
#16771 = CARTESIAN_POINT ( 'NONE',  ( -5.405949406250003975, -9.363379034771801557, -84.53125000204838102 ) ) ;
#16772 = VERTEX_POINT ( 'NONE', #23483 ) ;
#16773 = CARTESIAN_POINT ( 'NONE',  ( 10.00000000000000000, 5.773502691896255534, -86.25000000409677625 ) ) ;
#16774 = CARTESIAN_POINT ( 'NONE',  ( 9.999999999998969713, 5.773502691896851502, -48.37499999999995026 ) ) ;
#16775 = CARTESIAN_POINT ( 'NONE',  ( 10.81189881249999551, -6.242252689847874514, -41.96875000204836681 ) ) ;
#16776 = VERTEX_POINT ( 'NONE', #12889 ) ;
#16777 = CARTESIAN_POINT ( 'NONE',  ( -4.999999999999996447, 8.660254037844387298, -7.499999999999978684 ) ) ;
#16778 = CARTESIAN_POINT ( 'NONE',  ( -10.00000000000000000, -5.773502691896251982, -143.6250000000000000 ) ) ;
#16779 = LINE ( 'NONE', #838, #31723 ) ;
#16780 = CARTESIAN_POINT ( 'NONE',  ( 7.070501591499377789E-16, 11.54700538379251284, -14.00000000409676382 ) ) ;
#16781 = CARTESIAN_POINT ( 'NONE',  ( -10.00000000000000000, -5.773502691896251982, -194.6250000000000284 ) ) ;
#16782 = FACE_OUTER_BOUND ( 'NONE', #28647, .T. ) ;
#16784 = ORIENTED_EDGE ( 'NONE', *, *, #8063, .T. ) ;
#16783 = CARTESIAN_POINT ( 'NONE',  ( 10.81189881249999907, 6.242252689847868297, -119.9062500020483810 ) ) ;
#16785 = CARTESIAN_POINT ( 'NONE',  ( 5.000000000000000000, 8.660254037844385522, -23.12500000409675849 ) ) ;
#16786 = VERTEX_POINT ( 'NONE', #29962 ) ;
#16787 =( BOUNDED_CURVE ( )  B_SPLINE_CURVE ( 2, ( #6829, #30361, #29934, #10269, #26684, #26057, #30145 ),
 .UNSPECIFIED., .F., .F. ) 
 B_SPLINE_CURVE_WITH_KNOTS ( ( 3, 2, 2, 3 ),
 ( 0.4552238805970150737, 0.4564676616915424590, 0.4577114427860698442, 0.4589552238805971740 ),
 .UNSPECIFIED. ) 
 CURVE ( )  GEOMETRIC_REPRESENTATION_ITEM ( )  RATIONAL_B_SPLINE_CURVE ( ( 0.9999999999999820144, 0.8660254037844566932, 1.000000000000000000, 0.8660254037844387076, 1.000000000000000000, 0.8660254037844207220, 1.000000000000017986 ) ) 
 REPRESENTATION_ITEM ( '' )  );
#16788 = CARTESIAN_POINT ( 'NONE',  ( 10.81189881249999551, -6.242252689847874514, -46.65625000204835970 ) ) ;
#16789 = DATE_AND_TIME ( #40307, #30462 ) ;
#16790 = CARTESIAN_POINT ( 'NONE',  ( -10.81189881249999729, 1.324075727343319199E-15, -98.09375000204838102 ) ) ;
#16791 = CARTESIAN_POINT ( 'NONE',  ( 10.81189881249999551, -6.242252689847874514, -126.1562500020483810 ) ) ;
#16792 = ORIENTED_EDGE ( 'NONE', *, *, #6099, .F. ) ;
#16793 = CARTESIAN_POINT ( 'NONE',  ( 10.00000000000076916, -5.773502691895816774, -111.6249999999999716 ) ) ;
#16794 = CARTESIAN_POINT ( 'NONE',  ( -10.00000000000076916, 5.773502691895813221, -127.7500000040967763 ) ) ;
#16795 =( BOUNDED_CURVE ( )  B_SPLINE_CURVE ( 2, ( #12425, #26455, #6189, #39606, #19130, #23222, #9626 ),
 .UNSPECIFIED., .F., .F. ) 
 B_SPLINE_CURVE_WITH_KNOTS ( ( 3, 2, 2, 3 ),
 ( 0.2910447761194031036, 0.2922885572139304333, 0.2935323383084578186, 0.2947761194029852039 ),
 .UNSPECIFIED. ) 
 CURVE ( )  GEOMETRIC_REPRESENTATION_ITEM ( )  RATIONAL_B_SPLINE_CURVE ( ( 0.9999999999999880096, 0.8660254037844506980, 1.000000000000000000, 0.8660254037844387076, 1.000000000000000000, 0.8660254037844267172, 1.000000000000011990 ) ) 
 REPRESENTATION_ITEM ( '' )  );
#16796 = CARTESIAN_POINT ( 'NONE',  ( 10.81189881249999729, 0.000000000000000000, -172.5312500020484094 ) ) ;
#16797 = CARTESIAN_POINT ( 'NONE',  ( 7.070501591499376803E-16, 11.54700538379251284, -155.0000000040968189 ) ) ;
#16798 = CARTESIAN_POINT ( 'NONE',  ( -5.405949406250003975, -9.363379034771801557, -129.3437500020484094 ) ) ;
#16799 = CARTESIAN_POINT ( 'NONE',  ( 5.405949406249999534, 9.363379034771803333, -97.09375000204838102 ) ) ;
#16800 = CARTESIAN_POINT ( 'NONE',  ( -9.999999999999998224, 1.224646799147353059E-15, -106.2499999999999858 ) ) ;
#16801 = CARTESIAN_POINT ( 'NONE',  ( -5.405949406249996869, 9.363379034771805109, -112.0312500020483810 ) ) ;
#16802 = CARTESIAN_POINT ( 'NONE',  ( 5.000000000000000000, 8.660254037844385522, -185.1250000040967905 ) ) ;
#16803 = CARTESIAN_POINT ( 'NONE',  ( 5.405949406249992428, -9.363379034771808662, -115.5937500020483810 ) ) ;
#16804 = CARTESIAN_POINT ( 'NONE',  ( -5.405949406249996869, 9.363379034771805109, -182.5312500020484094 ) ) ;
#16805 =( BOUNDED_CURVE ( )  B_SPLINE_CURVE ( 2, ( #27946, #35068, #5495, #18645, #31839, #13729, #40076 ),
 .UNSPECIFIED., .F., .F. ) 
 B_SPLINE_CURVE_WITH_KNOTS ( ( 3, 2, 2, 3 ),
 ( 0.07462686567164185381, 0.07587064676616922521, 0.07711442786069658273, 0.07835820895522395413 ),
 .UNSPECIFIED. ) 
 CURVE ( )  GEOMETRIC_REPRESENTATION_ITEM ( )  RATIONAL_B_SPLINE_CURVE ( ( 0.9999999999999925615, 0.8660254037844461461, 1.000000000000000000, 0.8660254037844387076, 1.000000000000000000, 0.8660254037844312691, 1.000000000000007550 ) ) 
 REPRESENTATION_ITEM ( '' )  );
#16806 = DIRECTION ( 'NONE',  ( 1.000000000000000000, 0.000000000000000000, 0.000000000000000000 ) ) ;
#16807 = CARTESIAN_POINT ( 'NONE',  ( 10.00000000000051159, -5.773502691895965988, -114.6249999999999574 ) ) ;
#16808 = CARTESIAN_POINT ( 'NONE',  ( -10.00000000000000000, -5.773502691896251982, -1.124999999999959366 ) ) ;
#16809 = CARTESIAN_POINT ( 'NONE',  ( -5.405949406249996869, 9.363379034771805109, -56.34375000204835970 ) ) ;
#16810 = CARTESIAN_POINT ( 'NONE',  ( -5.405949406250003975, -9.363379034771801557, -40.84375000204837391 ) ) ;
#16811 = CARTESIAN_POINT ( 'NONE',  ( 7.070501591499377789E-16, 11.54700538379251284, -182.0000000040968189 ) ) ;
#16812 = CARTESIAN_POINT ( 'NONE',  ( 5.405949406249999534, 9.363379034771803333, -22.28125000204836326 ) ) ;
#16813 = CARTESIAN_POINT ( 'NONE',  ( 5.405949406249992428, -9.363379034771808662, -31.59375000204836681 ) ) ;
#16814 = CARTESIAN_POINT ( 'NONE',  ( 9.999999999999998224, 0.000000000000000000, -182.3750000040967905 ) ) ;
#16815 = CARTESIAN_POINT ( 'NONE',  ( -10.81189881249999729, 1.324075727343319199E-15, -138.5937500020483810 ) ) ;
#16816 = CARTESIAN_POINT ( 'NONE',  ( 9.999999999999996447, -5.773502691896262640, -108.6249999999999858 ) ) ;
#16817 = CARTESIAN_POINT ( 'NONE',  ( -10.81189881249999907, -6.242252689847864744, -35.15625000204835970 ) ) ;
#16818 = CARTESIAN_POINT ( 'NONE',  ( 9.999999999999998224, 0.000000000000000000, -191.0000000000000000 ) ) ;
#16819 = CARTESIAN_POINT ( 'NONE',  ( -2.121150477449813534E-15, -11.54700538379251284, -57.87499999999997868 ) ) ;
#16820 = CARTESIAN_POINT ( 'NONE',  ( -2.293366432827344421E-15, -12.48450537969573659, -133.9062500020483810 ) ) ;
#16821 = CARTESIAN_POINT ( 'NONE',  ( 5.405949406249992428, -9.363379034771808662, -105.2812500020483810 ) ) ;
#16822 = EDGE_CURVE ( 'NONE', #3816, #3490, #40507, .T. ) ;
#16823 = ORIENTED_EDGE ( 'NONE', *, *, #34660, .F. ) ;
#16824 = LINE ( 'NONE', #6502, #32762 ) ;
#16825 = CARTESIAN_POINT ( 'NONE',  ( -9.999999999999998224, 1.224646799147353059E-15, -106.6250000040967763 ) ) ;
#16826 = CARTESIAN_POINT ( 'NONE',  ( -2.121150477449813534E-15, -11.54700538379251284, -107.3749999999999858 ) ) ;
#16827 = CARTESIAN_POINT ( 'NONE',  ( -10.81189881249999729, 1.324075727343319199E-15, -68.09375000204836681 ) ) ;
#16828 = EDGE_LOOP ( 'NONE', ( #25784, #9309, #24496, #13862, #19722, #21642, #19437, #30424, #5886, #9382, #12552, #9358, #24802, #4018, #3443, #26686, #20410, #6309, #10688, #33218, #8635, #25951, #31090, #16414, #17909, #37003, #39001, #18664, #11158, #29009, #25773, #7233, #11813, #35037, #42271, #11111, #25939, #33965, #35570, #6726, #27861, #40613, #36066, #40768, #13388, #7941, #38424, #40291, #26683, #15150, #27976, #30886, #2441, #34884, #31915, #9330, #29719, #40996, #5466, #19811, #12864, #12862, #17101, #24751, #17781, #19442, #31541, #10782, #38080, #29401, #29430, #28349, #31156, #31892, #3436, #29400, #21940, #4127, #29088, #33735, #17044, #9192, #29037, #42052, #34663, #6870, #34560, #37891, #7833, #4865, #36924, #30712, #37035, #29451, #19193, #38207, #5090, #16251, #15248, #3491, #35750, #3522, #6049, #8793, #6467, #39133, #9051, #1320, #13917, #10166, #28184, #10272, #37513, #15414, #21473, #28429, #21594, #34655, #42, #37081, #19611, #11635, #20462, #11442, #23977, #10111, #35334, #18992, #9166, #8426, #13119, #3645, #10002, #1219, #8862, #8060, #11001, #21207, #9477, #37293, #24579, #3438, #4851, #5869, #40728, #2005, #2397, #35569, #24427, #38944, #15132, #14179, #25222, #2607, #21725, #30119, #17805, #31527, #24414, #10239, #20463, #12685, #26111, #41322, #27693, #6152, #42015, #13263, #23427, #8046, #37946, #29028, #39260, #2809, #17528, #11484, #20378, #26476, #41840, #32276, #16243, #20352, #3327, #5245, #12843, #29125, #20565, #3331, #40620, #27971, #42586, #17321, #5822, #5995, #25536, #35623, #34931, #22793, #28134, #29238, #30021, #13649, #21239, #30341, #36969, #37355, #20200, #21273, #15185, #7193, #16682, #34642, #28348, #27257, #18210, #4551, #42171, #2863, #29976, #21211, #9747, #4988, #33478, #26354, #1218, #16737, #18064, #30834, #19602, #21483, #20302, #25013, #4443, #31373, #11091, #10268, #23237, #9064, #26952, #34723, #40885, #25175, #34826, #8732, #8705, #39715, #36857, #34510, #10328, #23132, #679, #18865, #8703, #26790, #2273, #37281, #40049, #8551, #25144, #21141, #25747, #5419, #14276, #10063, #6311, #23599, #37931, #42647, #29610, #24314 ) ) ;
#16829 = CARTESIAN_POINT ( 'NONE',  ( 5.000000000000000000, 8.660254037844385522, -36.24999999999997868 ) ) ;
#16830 = CARTESIAN_POINT ( 'NONE',  ( -2.121150477449813534E-15, -11.54700538379251284, -16.25000000409675849 ) ) ;
#16831 = CARTESIAN_POINT ( 'NONE',  ( -10.81189881249999729, -6.242252689847864744, -45.65625000204837391 ) ) ;
#16832 = CARTESIAN_POINT ( 'NONE',  ( -4.999999999999996447, 8.660254037844387298, -124.8750000040967763 ) ) ;
#16833 = CARTESIAN_POINT ( 'NONE',  ( 10.00000000000000000, 5.773502691896255534, -32.25000000409675494 ) ) ;
#16834 = CARTESIAN_POINT ( 'NONE',  ( -10.00000000000076916, 5.773502691895813221, -133.3749999999999716 ) ) ;
#16835 = CARTESIAN_POINT ( 'NONE',  ( 7.644554776091147741E-16, 12.48450537969573659, -142.1562500020483810 ) ) ;
#16836 = CARTESIAN_POINT ( 'NONE',  ( 10.00000000000154010, -5.773502691895370020, -15.62499999999993960 ) ) ;
#16837 = ORIENTED_EDGE ( 'NONE', *, *, #23459, .F. ) ;
#16838 = VERTEX_POINT ( 'NONE', #22845 ) ;
#16839 = ADVANCED_FACE ( 'NONE', ( #36007 ), #39862, .T. ) ;
#16840 = ORIENTED_EDGE ( 'NONE', *, *, #11687, .T. ) ;
#16841 = CARTESIAN_POINT ( 'NONE',  ( 7.070501591499376803E-16, 11.54700538379251284, -108.1249999999999858 ) ) ;
#16842 = CARTESIAN_POINT ( 'NONE',  ( 9.999999999999998224, 0.000000000000000000, -200.0000000000000000 ) ) ;
#16843 = CARTESIAN_POINT ( 'NONE',  ( -10.81189881249999729, 1.324075727343319199E-15, -171.5937500020484094 ) ) ;
#16844 = VECTOR ( 'NONE', #29755, 1000.000000000000000 ) ;
#16845 = CARTESIAN_POINT ( 'NONE',  ( -10.81189881249999729, 6.242252689847871849, -192.9062500020484094 ) ) ;
#16846 = CARTESIAN_POINT ( 'NONE',  ( 10.81189881249999551, -6.242252689847874514, -23.96875000204836681 ) ) ;
#16847 = CARTESIAN_POINT ( 'NONE',  ( 9.999999999999998224, 0.000000000000000000, -155.0000000000000000 ) ) ;
#16848 = CARTESIAN_POINT ( 'NONE',  ( -8.660254037844442365, -15.00000000000010658, 49.99999999999998579 ) ) ;
#16849 = CARTESIAN_POINT ( 'NONE',  ( -10.81189881249999729, 6.242252689847871849, -152.2187500020483810 ) ) ;
#16850 = CARTESIAN_POINT ( 'NONE',  ( 10.81189881249999551, -6.242252689847874514, -133.4687500020483810 ) ) ;
#16851 = CARTESIAN_POINT ( 'NONE',  ( -4.999999999999996447, 8.660254037844387298, -172.8750000040968189 ) ) ;
#16852 = CARTESIAN_POINT ( 'NONE',  ( -10.81189881249999907, -6.242252689847864744, -129.4687500020483810 ) ) ;
#16853 = CARTESIAN_POINT ( 'NONE',  ( 10.81189881249999729, 0.000000000000000000, -132.0312500020484094 ) ) ;
#16854 = CARTESIAN_POINT ( 'NONE',  ( 5.405949406249999534, 9.363379034771803333, -11.59375000204834727 ) ) ;
#16855 = CARTESIAN_POINT ( 'NONE',  ( -5.405949406250003975, -9.363379034771801557, -139.8437500020484094 ) ) ;
#16856 = CARTESIAN_POINT ( 'NONE',  ( -9.999999999999227285, -5.773502691896698735, -130.1249999999999716 ) ) ;
#16857 = DIRECTION ( 'NONE',  ( 1.000000000000000000, 0.000000000000000000, 0.000000000000000000 ) ) ;
#16858 = CARTESIAN_POINT ( 'NONE',  ( 7.070501591499377789E-16, 11.54700538379251284, -156.1250000000000000 ) ) ;
#16859 = CARTESIAN_POINT ( 'NONE',  ( -4.999999999999996447, 8.660254037844387298, -55.87500000409676204 ) ) ;
#16860 = CARTESIAN_POINT ( 'NONE',  ( 10.81189881249999729, 0.000000000000000000, -86.84375000204836681 ) ) ;
#16861 = CARTESIAN_POINT ( 'NONE',  ( -10.81189881249999729, 6.242252689847871849, -74.21875000204836681 ) ) ;
#16862 = CARTESIAN_POINT ( 'NONE',  ( -10.81189881249999729, 6.242252689847871849, -39.90625000204835970 ) ) ;
#16863 = CARTESIAN_POINT ( 'NONE',  ( 5.405949406249999534, 9.363379034771803333, -55.09375000204835970 ) ) ;
#16864 = CARTESIAN_POINT ( 'NONE',  ( -5.000000000000003553, -8.660254037844383745, -139.3750000040968189 ) ) ;
#16865 = CARTESIAN_POINT ( 'NONE',  ( -10.81189881249999907, -6.242252689847864744, -163.9687500020484094 ) ) ;
#16866 = CARTESIAN_POINT ( 'NONE',  ( 5.000000000000000000, 8.660254037844385522, -132.2499999999999716 ) ) ;
#16867 = CARTESIAN_POINT ( 'NONE',  ( 10.81189881249999729, 6.242252689847867408, -136.4062500020484094 ) ) ;
#16868 = DIRECTION ( 'NONE',  ( -0.000000000000000000, -1.000000000000000000, -0.000000000000000000 ) ) ;
#16869 = CARTESIAN_POINT ( 'NONE',  ( 4.999999999999992006, -8.660254037844389075, -81.74999999999998579 ) ) ;
#16870 = ORIENTED_EDGE ( 'NONE', *, *, #27900, .T. ) ;
#16871 = CARTESIAN_POINT ( 'NONE',  ( 10.81189881249999551, -6.242252689847874514, -108.1562500020483810 ) ) ;
#16872 = CARTESIAN_POINT ( 'NONE',  ( 10.00000000000000000, 5.773502691896255534, -129.7500000040967905 ) ) ;
#16873 = CARTESIAN_POINT ( 'NONE',  ( -35.00000000000000711, 0.000000000000000000, -169.9999999999999716 ) ) ;
#16874 = CARTESIAN_POINT ( 'NONE',  ( 7.644554776091147741E-16, 12.48450537969573659, -167.6562500020483810 ) ) ;
#16875 = CARTESIAN_POINT ( 'NONE',  ( -9.999999999999998224, 1.224646799147353059E-15, -43.62500000409677625 ) ) ;
#16876 = EDGE_CURVE ( 'NONE', #42482, #23937, #26361, .T. ) ;
#16877 =( BOUNDED_CURVE ( )  B_SPLINE_CURVE ( 2, ( #37194, #24484, #27072, #1388, #4403, #1175, #27712 ),
 .UNSPECIFIED., .F., .F. ) 
 B_SPLINE_CURVE_WITH_KNOTS ( ( 3, 2, 2, 3 ),
 ( 0.2947761194029852039, 0.2960199004975125336, 0.2972636815920398634, 0.2985074626865671932 ),
 .UNSPECIFIED. ) 
 CURVE ( )  GEOMETRIC_REPRESENTATION_ITEM ( )  RATIONAL_B_SPLINE_CURVE ( ( 0.9999999999999880096, 0.8660254037844506980, 1.000000000000000000, 0.8660254037844387076, 1.000000000000000000, 0.8660254037844327124, 1.000000000000005995 ) ) 
 REPRESENTATION_ITEM ( '' )  );
#16878 = FACE_OUTER_BOUND ( 'NONE', #7352, .T. ) ;
#16879 = CARTESIAN_POINT ( 'NONE',  ( -10.81189881249999729, 1.324075727343319199E-15, -54.78125000204836681 ) ) ;
#16880 = VECTOR ( 'NONE', #14915, 1000.000000000000000 ) ;
#16881 = CARTESIAN_POINT ( 'NONE',  ( 7.070501591499376803E-16, 11.54700538379251284, -73.62499999999997158 ) ) ;
#16882 = CARTESIAN_POINT ( 'NONE',  ( 10.81189881249999907, 6.242252689847868297, -158.9062500020483810 ) ) ;
#16883 = CARTESIAN_POINT ( 'NONE',  ( 7.644554776091147741E-16, 12.48450537969573659, -137.4687500020483810 ) ) ;
#16884 = LINE ( 'NONE', #16671, #11145 ) ;
#16885 = CARTESIAN_POINT ( 'NONE',  ( -5.000000000000003553, -8.660254037844383745, -115.3750000040967905 ) ) ;
#16886 = EDGE_LOOP ( 'NONE', ( #33178, #39310, #41583, #11536 ) ) ;
#16887 = CARTESIAN_POINT ( 'NONE',  ( 9.999999999999998224, 0.000000000000000000, -131.3750000040967905 ) ) ;
#16889 = ORIENTED_EDGE ( 'NONE', *, *, #8533, .F. ) ;
#16888 = CARTESIAN_POINT ( 'NONE',  ( -2.293366432827344421E-15, -12.48450537969573659, -66.40625000204838102 ) ) ;
#16890 = PERSON_AND_ORGANIZATION ( #11915, #17965 ) ;
#16892 = ORIENTED_EDGE ( 'NONE', *, *, #19616, .T. ) ;
#16891 = CARTESIAN_POINT ( 'NONE',  ( -2.293366432827344421E-15, -12.48450537969573659, -115.7187500020483952 ) ) ;
#16893 = AXIS2_PLACEMENT_3D ( 'NONE', #25601, #26229, #15849 ) ;
#16894 = CARTESIAN_POINT ( 'NONE',  ( -10.81189881249999729, 6.242252689847871849, -23.21875000204835970 ) ) ;
#16895 = CARTESIAN_POINT ( 'NONE',  ( 7.644554776091147741E-16, 12.48450537969573659, 0.3437499979516377424 ) ) ;
#16896 = CARTESIAN_POINT ( 'NONE',  ( -5.405949406249996869, 9.363379034771805109, -47.34375000204838102 ) ) ;
#16897 = FACE_OUTER_BOUND ( 'NONE', #2171, .T. ) ;
#16898 = CARTESIAN_POINT ( 'NONE',  ( 9.999999999999998224, 0.000000000000000000, -192.8750000040967905 ) ) ;
#16899 = CARTESIAN_POINT ( 'NONE',  ( -10.81189881249999729, 6.242252689847871849, -180.7187500020484379 ) ) ;
#16900 = AXIS2_PLACEMENT_3D ( 'NONE', #9744, #22925, #17266 ) ;
#16901 = CARTESIAN_POINT ( 'NONE',  ( 5.405949406249999534, 9.363379034771803333, -170.5937500020484094 ) ) ;
#16902 = CARTESIAN_POINT ( 'NONE',  ( -10.81189881249999907, -6.242252689847864744, -148.9687500020484094 ) ) ;
#16903 = CARTESIAN_POINT ( 'NONE',  ( -10.81189881249999729, 6.242252689847871849, -165.7187500020483810 ) ) ;
#16904 = LINE ( 'NONE', #23195, #36406 ) ;
#16905 = CARTESIAN_POINT ( 'NONE',  ( 5.000000000000000000, 8.660254037844385522, -193.7500000000000000 ) ) ;
#16906 = CARTESIAN_POINT ( 'NONE',  ( -5.000000000000003553, -8.660254037844383745, -178.0000000000000000 ) ) ;
#16907 = CARTESIAN_POINT ( 'NONE',  ( -2.293366432827344421E-15, -12.48450537969573659, -97.71875000204838102 ) ) ;
#16908 = CARTESIAN_POINT ( 'NONE',  ( -10.00000000000051337, 5.773502691895962435, -151.3750000000000284 ) ) ;
#16909 = CARTESIAN_POINT ( 'NONE',  ( -5.405949406249996869, 9.363379034771805109, -62.53125000204837391 ) ) ;
#16910 = CARTESIAN_POINT ( 'NONE',  ( 9.999999999999479527, 5.773502691896553074, -146.2500000040967905 ) ) ;
#16911 = CARTESIAN_POINT ( 'NONE',  ( -5.405949406250003975, -9.363379034771801557, -183.3437500020483810 ) ) ;
#16912 = CARTESIAN_POINT ( 'NONE',  ( 10.81189881249999907, 6.242252689847868297, -125.9062500020483810 ) ) ;
#16913 = CARTESIAN_POINT ( 'NONE',  ( 10.81189881249999729, 0.000000000000000000, -163.5312500020484094 ) ) ;
#16914 = CARTESIAN_POINT ( 'NONE',  ( -5.405949406249996869, 9.363379034771805109, -52.03125000204835970 ) ) ;
#16915 = CARTESIAN_POINT ( 'NONE',  ( -9.999999999999998224, 1.224646799147353059E-15, -135.1250000040967620 ) ) ;
#16916 = CARTESIAN_POINT ( 'NONE',  ( 5.000000000000000000, 8.660254037844385522, -114.2499999999999858 ) ) ;
#16917 =( BOUNDED_CURVE ( )  B_SPLINE_CURVE ( 2, ( #34248, #7909, #21057, #7475, #20626, #11338, #13924 ),
 .UNSPECIFIED., .F., .F. ) 
 B_SPLINE_CURVE_WITH_KNOTS ( ( 3, 2, 2, 3 ),
 ( 0.5298507462686568026, 0.5310945273631841879, 0.5323383084577115731, 0.5335820895522389584 ),
 .UNSPECIFIED. ) 
 CURVE ( )  GEOMETRIC_REPRESENTATION_ITEM ( )  RATIONAL_B_SPLINE_CURVE ( ( 0.9999999999999880096, 0.8660254037844506980, 1.000000000000000000, 0.8660254037844387076, 1.000000000000000000, 0.8660254037844267172, 1.000000000000011990 ) ) 
 REPRESENTATION_ITEM ( '' )  );
#16918 = VERTEX_POINT ( 'NONE', #32569 ) ;
#16919 = CARTESIAN_POINT ( 'NONE',  ( 10.81189881249999551, -6.242252689847874514, -132.1562500020483810 ) ) ;
#16920 = CARTESIAN_POINT ( 'NONE',  ( -10.81189881249999729, 1.324075727343319199E-15, -144.7812500020483810 ) ) ;
#16921 = CARTESIAN_POINT ( 'NONE',  ( 10.81189881249999551, -6.242252689847874514, -190.6562500020484094 ) ) ;
#16922 = LINE ( 'NONE', #30123, #38536 ) ;
#16923 = CARTESIAN_POINT ( 'NONE',  ( -5.405949406249996869, 9.363379034771805109, -83.34375000204836681 ) ) ;
#16924 = ORIENTED_EDGE ( 'NONE', *, *, #32791, .T. ) ;
#16925 = CARTESIAN_POINT ( 'NONE',  ( 10.00000000000000000, 5.773502691896255534, -54.37499999999997158 ) ) ;
#16926 = CARTESIAN_POINT ( 'NONE',  ( 7.644554776091147741E-16, 12.48450537969573659, -183.9687500020484094 ) ) ;
#16927 = CARTESIAN_POINT ( 'NONE',  ( -2.121150477449813534E-15, -11.54700538379251284, -68.75000000409679046 ) ) ;
#16928 = ADVANCED_FACE ( 'NONE', ( #30175 ), #23055, .T. ) ;
#16929 = CARTESIAN_POINT ( 'NONE',  ( 10.00000000000051159, -5.773502691895965988, -109.0000000040967620 ) ) ;
#16930 = CARTESIAN_POINT ( 'NONE',  ( 4.999999999999992006, -8.660254037844389075, -158.2500000000000000 ) ) ;
#16931 = EDGE_CURVE ( 'NONE', #4387, #36434, #25871, .T. ) ;
#16932 = CARTESIAN_POINT ( 'NONE',  ( 5.405949406249999534, 9.363379034771803333, -74.78125000204838102 ) ) ;
#16933 = VECTOR ( 'NONE', #41787, 1000.000000000000000 ) ;
#16934 = CARTESIAN_POINT ( 'NONE',  ( 10.81189881249999729, 6.242252689847867408, -59.90625000204838813 ) ) ;
#16935 = EDGE_CURVE ( 'NONE', #12287, #23382, #24986, .T. ) ;
#16936 = CARTESIAN_POINT ( 'NONE',  ( -4.999999999999996447, 8.660254037844387298, -54.37500000409675494 ) ) ;
#16937 = CARTESIAN_POINT ( 'NONE',  ( -5.405949406250003975, -9.363379034771801557, -9.343750002048345493 ) ) ;
#16938 = CARTESIAN_POINT ( 'NONE',  ( -5.000000000000003553, -8.660254037844383745, -151.3750000040967905 ) ) ;
#16939 = CARTESIAN_POINT ( 'NONE',  ( 7.644554776091147741E-16, 12.48450537969573659, -182.6562500020484094 ) ) ;
#16940 = CARTESIAN_POINT ( 'NONE',  ( -2.293366432827344421E-15, -12.48450537969573659, -7.906250002048365921 ) ) ;
#16941 = CARTESIAN_POINT ( 'NONE',  ( 9.999999999999998224, 0.000000000000000000, -102.8750000040967763 ) ) ;
#16942 = DIRECTION ( 'NONE',  ( -0.000000000000000000, -0.000000000000000000, 1.000000000000000000 ) ) ;
#16943 = DIRECTION ( 'NONE',  ( -1.000000000000000000, 0.000000000000000000, 0.000000000000000000 ) ) ;
#16944 = DIRECTION ( 'NONE',  ( -0.000000000000000000, -0.000000000000000000, 1.000000000000000000 ) ) ;
#16946 = EDGE_LOOP ( 'NONE', ( #10356, #17428, #21856, #20174 ) ) ;
#16945 = CARTESIAN_POINT ( 'NONE',  ( 10.81189881249999551, -6.242252689847874514, -93.15625000204838102 ) ) ;
#16947 = CARTESIAN_POINT ( 'NONE',  ( 7.070501591499376803E-16, 11.54700538379251284, -24.50000000409676559 ) ) ;
#16948 = EDGE_CURVE ( 'NONE', #4388, #28982, #34503, .T. ) ;
#16950 = VERTEX_POINT ( 'NONE', #21243 ) ;
#16949 = CARTESIAN_POINT ( 'NONE',  ( -5.405949406249996869, 9.363379034771805109, -102.8437500020483810 ) ) ;
#16951 = VERTEX_POINT ( 'NONE', #17779 ) ;
#16952 = CARTESIAN_POINT ( 'NONE',  ( 10.81189881249999907, 6.242252689847868297, -37.21875000204835970 ) ) ;
#16953 = CARTESIAN_POINT ( 'NONE',  ( 10.81189881249999729, 0.000000000000000000, -22.53125000204836326 ) ) ;
#16954 = COORDINATED_UNIVERSAL_TIME_OFFSET ( 6, 0, .AHEAD. ) ;
#16955 = EDGE_CURVE ( 'NONE', #5967, #39187, #9794, .T. ) ;
#16956 = CARTESIAN_POINT ( 'NONE',  ( -5.405949406250003975, -9.363379034771801557, -72.34375000204836681 ) ) ;
#16957 = CARTESIAN_POINT ( 'NONE',  ( -5.000000000000003553, -8.660254037844383745, -17.87500000409675138 ) ) ;
#16958 = CARTESIAN_POINT ( 'NONE',  ( 9.999999999999998224, 0.000000000000000000, -40.99999999999997868 ) ) ;
#16959 = EDGE_CURVE ( 'NONE', #10102, #23552, #34428, .T. ) ;
#16960 = CARTESIAN_POINT ( 'NONE',  ( 10.81189881249999551, -6.242252689847874514, -193.4687500020484094 ) ) ;
#16961 = CARTESIAN_POINT ( 'NONE',  ( 5.405949406249992428, -9.363379034771808662, -148.5937500020483810 ) ) ;
#16962 = AXIS2_PLACEMENT_3D ( 'NONE', #5838, #6051, #29350 ) ;
#16963 = CARTESIAN_POINT ( 'NONE',  ( 4.999999999999992006, -8.660254037844389075, -121.1250000040967905 ) ) ;
#16964 = DIRECTION ( 'NONE',  ( 0.000000000000000000, -0.7071067811865487940, -0.7071067811865463515 ) ) ;
#16965 = CARTESIAN_POINT ( 'NONE',  ( -5.405949406249996869, 9.363379034771805109, -152.5312500020484094 ) ) ;
#16966 = CARTESIAN_POINT ( 'NONE',  ( 10.00000000000000000, 5.773502691896255534, -5.250000004096769146 ) ) ;
#16967 = CARTESIAN_POINT ( 'NONE',  ( 4.999999999999992006, -8.660254037844389075, -125.2500000000000000 ) ) ;
#16968 = CARTESIAN_POINT ( 'NONE',  ( -10.81189881249999729, 1.324075727343319199E-15, -125.0937500020483668 ) ) ;
#16969 = CARTESIAN_POINT ( 'NONE',  ( 7.070501591499376803E-16, 11.54700538379251284, -109.6249999999999858 ) ) ;
#16970 = CARTESIAN_POINT ( 'NONE',  ( 5.405949406249992428, -9.363379034771808662, -88.78125000204838102 ) ) ;
#16971 = CARTESIAN_POINT ( 'NONE',  ( -5.405949406249996869, 9.363379034771805109, -96.84375000204838102 ) ) ;
#16972 = CARTESIAN_POINT ( 'NONE',  ( 10.81189881249999551, -6.242252689847874514, -71.96875000204836681 ) ) ;
#16973 = CARTESIAN_POINT ( 'NONE',  ( 5.405949406249999534, 9.363379034771803333, -79.28125000204838102 ) ) ;
#16974 = CARTESIAN_POINT ( 'NONE',  ( 5.000000000000000000, 8.660254037844385522, -158.1250000040967905 ) ) ;
#16975 = CARTESIAN_POINT ( 'NONE',  ( -2.293366432827344421E-15, -12.48450537969573659, -157.9062500020483810 ) ) ;
#16976 = CARTESIAN_POINT ( 'NONE',  ( 7.644554776091147741E-16, 12.48450537969573659, -172.1562500020484094 ) ) ;
#16977 = DIRECTION ( 'NONE',  ( -1.000000000000000000, 0.000000000000000000, 0.000000000000000000 ) ) ;
#16978 = CARTESIAN_POINT ( 'NONE',  ( -9.999999999999998224, 1.224646799147353059E-15, -37.24999999999997868 ) ) ;
#16979 = CARTESIAN_POINT ( 'NONE',  ( -2.121150477449813534E-15, -11.54700538379251284, -53.75000000409677625 ) ) ;
#16980 = CARTESIAN_POINT ( 'NONE',  ( -10.81189881249999729, 1.324075727343319199E-15, -110.0937500020483810 ) ) ;
#16981 = CARTESIAN_POINT ( 'NONE',  ( 7.070501591499377789E-16, 11.54700538379251284, -84.12499999999997158 ) ) ;
#16982 = CARTESIAN_POINT ( 'NONE',  ( 5.405949406249999534, 9.363379034771803333, -7.281250002048378356 ) ) ;
#16983 = CARTESIAN_POINT ( 'NONE',  ( -10.00000000000000000, -5.773502691896251982, -93.00000000409679046 ) ) ;
#16984 = CARTESIAN_POINT ( 'NONE',  ( -5.000000000000003553, -8.660254037844383745, -95.87500000409677625 ) ) ;
#16985 = CARTESIAN_POINT ( 'NONE',  ( -5.405949406250003975, -9.363379034771801557, -104.0312500020483810 ) ) ;
#16986 = CARTESIAN_POINT ( 'NONE',  ( 5.405949406249999534, 9.363379034771803333, -80.78125000204838102 ) ) ;
#16987 = ORIENTED_EDGE ( 'NONE', *, *, #9860, .F. ) ;
#16988 = EDGE_CURVE ( 'NONE', #24317, #25484, #5277, .T. ) ;
#16989 = CARTESIAN_POINT ( 'NONE',  ( 10.00000000000000000, 5.773502691896255534, -74.25000000409677625 ) ) ;
#16990 = DIRECTION ( 'NONE',  ( -0.000000000000000000, -0.000000000000000000, 1.000000000000000000 ) ) ;
#16991 = CARTESIAN_POINT ( 'NONE',  ( -10.81189881249999729, 1.324075727343319199E-15, -33.59375000204836681 ) ) ;
#16992 = ORIENTED_EDGE ( 'NONE', *, *, #37881, .T. ) ;
#16993 = CARTESIAN_POINT ( 'NONE',  ( 5.000000000000000000, 8.660254037844385522, -9.249999999999952038 ) ) ;
#16994 = EDGE_CURVE ( 'NONE', #24042, #30416, #12405, .T. ) ;
#16995 = CARTESIAN_POINT ( 'NONE',  ( 5.405949406249992428, -9.363379034771808662, -36.28125000204837391 ) ) ;
#16996 = CARTESIAN_POINT ( 'NONE',  ( 10.00000000000000000, 5.773502691896255534, -148.8750000000000000 ) ) ;
#16997 = CARTESIAN_POINT ( 'NONE',  ( 9.999999999999998224, 1.224646799147353059E-15, -99.99999999999998579 ) ) ;
#16998 = CARTESIAN_POINT ( 'NONE',  ( 9.999999999999998224, 0.000000000000000000, -12.87500000409674783 ) ) ;
#16999 = CARTESIAN_POINT ( 'NONE',  ( 9.999999999999996447, -5.773502691896262640, -191.1250000000000000 ) ) ;
#17000 = CYLINDRICAL_SURFACE ( 'NONE', #27546, 9.999999999999998224 ) ;
#17002 = EDGE_LOOP ( 'NONE', ( #38369, #14606, #39248, #37128 ) ) ;
#17001 = CARTESIAN_POINT ( 'NONE',  ( 5.405949406249999534, 9.363379034771803333, -121.2812500020483952 ) ) ;
#17003 = CLOSED_SHELL ( 'NONE', ( #18808, #14623, #29395, #30885, #30210, #10378, #24136, #20403, #42288, #22994, #15381, #23992, #22502, #10590, #3707, #2864, #9066, #2026 ) ) ;
#17004 = DIRECTION ( 'NONE',  ( -0.000000000000000000, -0.000000000000000000, 1.000000000000000000 ) ) ;
#17005 = VERTEX_POINT ( 'NONE', #11306 ) ;
#17006 = ORIENTED_EDGE ( 'NONE', *, *, #19564, .T. ) ;
#17007 = ADVANCED_FACE ( 'NONE', ( #4633 ), #1405, .F. ) ;
#17008 = CARTESIAN_POINT ( 'NONE',  ( -10.81189881249999907, -6.242252689847864744, -47.15625000204836681 ) ) ;
#17009 = PERSON_AND_ORGANIZATION ( #11915, #17965 ) ;
#17010 = CARTESIAN_POINT ( 'NONE',  ( 5.405949406249999534, 9.363379034771803333, -98.59375000204838102 ) ) ;
#17011 = CARTESIAN_POINT ( 'NONE',  ( 5.405949406249992428, -9.363379034771808662, -124.7812500020483952 ) ) ;
#17012 = ORIENTED_EDGE ( 'NONE', *, *, #27056, .T. ) ;
#17013 = CARTESIAN_POINT ( 'NONE',  ( 0.000000000000000000, 0.000000000000000000, -200.0000000000000000 ) ) ;
#17014 = CARTESIAN_POINT ( 'NONE',  ( 10.81189881249999729, 0.000000000000000000, -197.8437500020484094 ) ) ;
#17015 = CARTESIAN_POINT ( 'NONE',  ( 5.405949406249992428, -9.363379034771808662, -171.2812500020484094 ) ) ;
#17016 = DIRECTION ( 'NONE',  ( -0.000000000000000000, -0.000000000000000000, 1.000000000000000000 ) ) ;
#17017 = CARTESIAN_POINT ( 'NONE',  ( 5.405949406249999534, 9.363379034771803333, -136.0937500020483810 ) ) ;
#17018 = CARTESIAN_POINT ( 'NONE',  ( 10.81189881249999729, 0.000000000000000000, -95.84375000204838102 ) ) ;
#17019 = CARTESIAN_POINT ( 'NONE',  ( 5.405949406249999534, 9.363379034771803333, -100.2812500020483952 ) ) ;
#17020 = CARTESIAN_POINT ( 'NONE',  ( 9.999999999999998224, 0.000000000000000000, -189.8750000040967905 ) ) ;
#17021 = CARTESIAN_POINT ( 'NONE',  ( 10.81189881249999729, 6.242252689847867408, -110.7187500020483810 ) ) ;
#17022 = CARTESIAN_POINT ( 'NONE',  ( -10.81189881249999729, 1.324075727343319199E-15, -179.2812500020484094 ) ) ;
#17023 = CARTESIAN_POINT ( 'NONE',  ( -9.999999999999479527, -5.773502691896549521, -105.0000000040967620 ) ) ;
#17024 = CARTESIAN_POINT ( 'NONE',  ( -2.293366432827344421E-15, -12.48450537969573659, -178.9062500020484379 ) ) ;
#17025 = CARTESIAN_POINT ( 'NONE',  ( -2.293366432827344421E-15, -12.48450537969573659, -193.9062500020484094 ) ) ;
#17026 = CARTESIAN_POINT ( 'NONE',  ( 5.405949406249992428, -9.363379034771808662, -60.09375000204835970 ) ) ;
#17027 = CARTESIAN_POINT ( 'NONE',  ( -10.81189881249999729, 1.324075727343319199E-15, -44.09375000204837391 ) ) ;
#17028 = CARTESIAN_POINT ( 'NONE',  ( -4.999999999999996447, 8.660254037844387298, -174.3750000040968189 ) ) ;
#17029 = CARTESIAN_POINT ( 'NONE',  ( 10.81189881249999729, 0.000000000000000000, -16.53125000204835970 ) ) ;
#17030 = CARTESIAN_POINT ( 'NONE',  ( -5.405949406250003975, -9.363379034771801557, -21.34375000204835615 ) ) ;
#17031 = DIRECTION ( 'NONE',  ( -0.000000000000000000, -0.000000000000000000, 1.000000000000000000 ) ) ;
#17032 = CARTESIAN_POINT ( 'NONE',  ( 5.405949406249999534, 9.363379034771803333, -128.5937500020483810 ) ) ;
#17033 = CARTESIAN_POINT ( 'NONE',  ( -5.000000000000003553, -8.660254037844383745, -105.9999999999999858 ) ) ;
#17034 = CARTESIAN_POINT ( 'NONE',  ( -10.81189881249999729, 1.324075727343319199E-15, -24.78125000204836681 ) ) ;
#17035 = CARTESIAN_POINT ( 'NONE',  ( -9.999999999999998224, 1.224646799147353059E-15, -198.1250000040967905 ) ) ;
#17036 = CARTESIAN_POINT ( 'NONE',  ( -5.000000000000003553, -8.660254037844383745, -56.49999999999996447 ) ) ;
#17037 = CARTESIAN_POINT ( 'NONE',  ( 10.81189881249999551, -6.242252689847874514, -124.6562500020483952 ) ) ;
#17038 = CARTESIAN_POINT ( 'NONE',  ( -5.405949406249996869, 9.363379034771805109, -110.5312500020483810 ) ) ;
#17039 = ORIENTED_EDGE ( 'NONE', *, *, #41692, .F. ) ;
#17040 = DIRECTION ( 'NONE',  ( -0.000000000000000000, -0.000000000000000000, 1.000000000000000000 ) ) ;
#17041 = CARTESIAN_POINT ( 'NONE',  ( -2.121150477449813534E-15, -11.54700538379251284, -104.7500000040967763 ) ) ;
#17042 = CARTESIAN_POINT ( 'NONE',  ( -9.999999999999998224, 1.224646799147353059E-15, -107.7499999999999858 ) ) ;
#17043 = CARTESIAN_POINT ( 'NONE',  ( 5.405949406249999534, 9.363379034771803333, -61.09375000204836681 ) ) ;
#17044 = ORIENTED_EDGE ( 'NONE', *, *, #5029, .T. ) ;
#17045 = CARTESIAN_POINT ( 'NONE',  ( 5.000000000000000000, 8.660254037844385522, -31.74999999999997158 ) ) ;
#17046 = CARTESIAN_POINT ( 'NONE',  ( 5.405949406249999534, 9.363379034771803333, -34.28125000204837391 ) ) ;
#17047 = LINE ( 'NONE', #7360, #41424 ) ;
#17048 = CARTESIAN_POINT ( 'NONE',  ( -5.000000000000003553, -8.660254037844383745, -38.87500000409676915 ) ) ;
#17049 =( BOUNDED_CURVE ( )  B_SPLINE_CURVE ( 2, ( #17799, #2071, #27964, #4439, #30779, #11752, #34236 ),
 .UNSPECIFIED., .F., .F. ) 
 B_SPLINE_CURVE_WITH_KNOTS ( ( 3, 2, 2, 3 ),
 ( 0.7910447761194031591, 0.7922885572139305443, 0.7935323383084578186, 0.7947761194029852039 ),
 .UNSPECIFIED. ) 
 CURVE ( )  GEOMETRIC_REPRESENTATION_ITEM ( )  RATIONAL_B_SPLINE_CURVE ( ( 0.9999999999999761302, 0.8660254037844625774, 1.000000000000000000, 0.8660254037844387076, 1.000000000000000000, 0.8660254037844267172, 1.000000000000011990 ) ) 
 REPRESENTATION_ITEM ( '' )  );
#17050 = CARTESIAN_POINT ( 'NONE',  ( -9.999999999999998224, 1.224646799147353059E-15, -130.2499999999999716 ) ) ;
#17051 = EDGE_CURVE ( 'NONE', #4845, #437, #590, .T. ) ;
#17052 = CARTESIAN_POINT ( 'NONE',  ( 10.81189881249999729, 0.000000000000000000, -141.0312500020483810 ) ) ;
#17053 = CARTESIAN_POINT ( 'NONE',  ( 9.999999999999742428, 5.773502691896404748, -129.7500000040967905 ) ) ;
#17054 = ORIENTED_EDGE ( 'NONE', *, *, #41015, .F. ) ;
#17055 =( BOUNDED_CURVE ( )  B_SPLINE_CURVE ( 2, ( #22533, #38724, #25779, #6349, #19705, #35706, #22325 ),
 .UNSPECIFIED., .F., .F. ) 
 B_SPLINE_CURVE_WITH_KNOTS ( ( 3, 2, 2, 3 ),
 ( 0.1977611940298507898, 0.1990049751243781750, 0.2002487562189055326, 0.2014925373134328901 ),
 .UNSPECIFIED. ) 
 CURVE ( )  GEOMETRIC_REPRESENTATION_ITEM ( )  RATIONAL_B_SPLINE_CURVE ( ( 0.9999999999999940048, 0.8660254037844447028, 1.000000000000000000, 0.8660254037844387076, 1.000000000000000000, 0.8660254037844327124, 1.000000000000005995 ) ) 
 REPRESENTATION_ITEM ( '' )  );
#17056 = EDGE_LOOP ( 'NONE', ( #29332, #21029, #23401, #30190 ) ) ;
#17057 = CARTESIAN_POINT ( 'NONE',  ( -5.000000000000003553, -8.660254037844383745, -106.3750000040967763 ) ) ;
#17058 = ADVANCED_FACE ( 'NONE', ( #11518 ), #14965, .T. ) ;
#17059 = DIRECTION ( 'NONE',  ( -0.000000000000000000, -0.000000000000000000, 1.000000000000000000 ) ) ;
#17060 = CARTESIAN_POINT ( 'NONE',  ( 5.405949406249992428, -9.363379034771808662, -165.0937500020484094 ) ) ;
#17061 = CYLINDRICAL_SURFACE ( 'NONE', #26128, 9.999999999999998224 ) ;
#17062 = CARTESIAN_POINT ( 'NONE',  ( 10.81189881249999729, 0.000000000000000000, -23.84375000204835970 ) ) ;
#17063 = CARTESIAN_POINT ( 'NONE',  ( 9.999999999999998224, 0.000000000000000000, -171.5000000000000000 ) ) ;
#17064 = CARTESIAN_POINT ( 'NONE',  ( -10.81189881249999729, 1.324075727343319199E-15, -159.5937500020484094 ) ) ;
#17065 = AXIS2_PLACEMENT_3D ( 'NONE', #323, #6369, #26847 ) ;
#17066 = CARTESIAN_POINT ( 'NONE',  ( 5.405949406249992428, -9.363379034771808662, -139.5937500020483810 ) ) ;
#17067 = DIRECTION ( 'NONE',  ( -0.000000000000000000, -0.000000000000000000, -1.000000000000000000 ) ) ;
#17068 = CARTESIAN_POINT ( 'NONE',  ( 10.81189881249999729, 0.000000000000000000, -118.3437500020483810 ) ) ;
#17069 = CARTESIAN_POINT ( 'NONE',  ( 9.999999999999996447, -5.773502691896262640, -193.0000000040968473 ) ) ;
#17070 = CARTESIAN_POINT ( 'NONE',  ( -2.293366432827344421E-15, -12.48450537969573659, -126.4062500020483952 ) ) ;
#17071 = CARTESIAN_POINT ( 'NONE',  ( 10.81189881249999551, -6.242252689847874514, -13.46875000204836503 ) ) ;
#17072 = CARTESIAN_POINT ( 'NONE',  ( -10.81189881249999729, 1.324075727343319199E-15, -137.0937500020483810 ) ) ;
#17073 = CARTESIAN_POINT ( 'NONE',  ( -4.999999999999996447, 8.660254037844387298, -63.37500000409676204 ) ) ;
#17074 = CARTESIAN_POINT ( 'NONE',  ( -9.999999999999998224, 1.224646799147353059E-15, -4.625000004096769146 ) ) ;
#17075 = CARTESIAN_POINT ( 'NONE',  ( 4.999999999999992006, -8.660254037844389075, -153.7500000000000000 ) ) ;
#17076 = CARTESIAN_POINT ( 'NONE',  ( -9.999999999999998224, 5.773502691896259087, -19.37499999999997868 ) ) ;
#17077 = CARTESIAN_POINT ( 'NONE',  ( -2.293366432827344421E-15, -12.48450537969573659, -85.71875000204838102 ) ) ;
#17078 = CARTESIAN_POINT ( 'NONE',  ( -10.81189881249999729, 6.242252689847871849, -66.71875000204838102 ) ) ;
#17079 = CARTESIAN_POINT ( 'NONE',  ( -10.81189881249999729, 1.324075727343319199E-15, -39.78125000204838102 ) ) ;
#17080 = CARTESIAN_POINT ( 'NONE',  ( -10.81189881249999729, 1.324075727343319199E-15, -56.09375000204835970 ) ) ;
#17081 = CARTESIAN_POINT ( 'NONE',  ( 9.999999999999998224, 0.000000000000000000, -110.3750000040967763 ) ) ;
#17082 = CARTESIAN_POINT ( 'NONE',  ( -5.405949406250003975, -9.363379034771801557, -151.8437500020483810 ) ) ;
#17083 = CARTESIAN_POINT ( 'NONE',  ( -5.000000000000003553, -8.660254037844383745, -133.0000000000000000 ) ) ;
#17084 = CARTESIAN_POINT ( 'NONE',  ( -10.81189881249999729, 6.242252689847871849, -138.9062500020484094 ) ) ;
#17085 = CARTESIAN_POINT ( 'NONE',  ( -4.263623593850985216, 9.091409269767630974, -180.0000000000000000 ) ) ;
#17086 = CARTESIAN_POINT ( 'NONE',  ( 9.999999999999998224, 0.000000000000000000, -84.49999999999997158 ) ) ;
#17087 = CARTESIAN_POINT ( 'NONE',  ( -10.81189881249999729, -6.242252689847864744, -21.65625000204837036 ) ) ;
#17088 = ORIENTED_EDGE ( 'NONE', *, *, #34606, .T. ) ;
#17089 = CARTESIAN_POINT ( 'NONE',  ( 7.644554776091147741E-16, 12.48450537969573659, -110.6562500020483810 ) ) ;
#17090 = CARTESIAN_POINT ( 'NONE',  ( 10.00000000000000000, 5.773502691896255534, -132.7500000040967905 ) ) ;
#17091 = CARTESIAN_POINT ( 'NONE',  ( -9.999999999999678479, -5.773502691896439387, -185.6250000000000000 ) ) ;
#17092 = CARTESIAN_POINT ( 'NONE',  ( -2.121150477449813534E-15, -11.54700538379251284, -38.75000000409676915 ) ) ;
#17093 = CARTESIAN_POINT ( 'NONE',  ( -9.999999999999998224, 1.224646799147353059E-15, -106.2499999999999858 ) ) ;
#17094 = CARTESIAN_POINT ( 'NONE',  ( -2.293366432827344421E-15, -12.48450537969573659, -51.40625000204837391 ) ) ;
#17095 = EDGE_CURVE ( 'NONE', #25691, #38243, #31475, .T. ) ;
#17096 = DIRECTION ( 'NONE',  ( -0.000000000000000000, -0.000000000000000000, -1.000000000000000000 ) ) ;
#17097 = CARTESIAN_POINT ( 'NONE',  ( 10.81189881249999729, 0.000000000000000000, -150.0312500020483810 ) ) ;
#17098 = CARTESIAN_POINT ( 'NONE',  ( 10.81189881249999907, 6.242252689847868297, -133.2187500020483810 ) ) ;
#17099 = CARTESIAN_POINT ( 'NONE',  ( -9.999999999999998224, 1.224646799147353059E-15, -10.62500000409674605 ) ) ;
#17100 = CIRCLE ( 'NONE', #41223, 5.500000000000003553 ) ;
#17101 = ORIENTED_EDGE ( 'NONE', *, *, #13277, .T. ) ;
#17102 = ADVANCED_BREP_SHAPE_REPRESENTATION ( '', ( #29300, #39998 ), #28294 ) ;
#17103 = CARTESIAN_POINT ( 'NONE',  ( 9.999999999999998224, 0.000000000000000000, -200.0000000000000000 ) ) ;
#17105 = EDGE_LOOP ( 'NONE', ( #10875, #14828, #33785, #24097 ) ) ;
#17104 = CARTESIAN_POINT ( 'NONE',  ( -10.81189881249999729, 1.324075727343319199E-15, -63.78125000204837391 ) ) ;
#17106 = PERSON_AND_ORGANIZATION_ROLE ( 'design_owner' ) ;
#17108 = ORIENTED_EDGE ( 'NONE', *, *, #30704, .T. ) ;
#17107 = CARTESIAN_POINT ( 'NONE',  ( 5.405949406249999534, 9.363379034771803333, -112.0937500020483810 ) ) ;
#17109 = EDGE_CURVE ( 'NONE', #6874, #32468, #11951, .T. ) ;
#17110 = CARTESIAN_POINT ( 'NONE',  ( 5.405949406249999534, 9.363379034771803333, -22.09375000204835615 ) ) ;
#17111 = CARTESIAN_POINT ( 'NONE',  ( -10.81189881249999729, 6.242252689847871849, -188.2187500020483810 ) ) ;
#17112 = CARTESIAN_POINT ( 'NONE',  ( -10.81189881249999729, 1.324075727343319199E-15, -47.09375000204838102 ) ) ;
#17113 = CARTESIAN_POINT ( 'NONE',  ( 5.000000000000000000, 8.660254037844385522, -62.12500000409676204 ) ) ;
#17114 = CARTESIAN_POINT ( 'NONE',  ( -9.999999999999479527, -5.773502691896549521, -31.50000000409673717 ) ) ;
#17115 = CARTESIAN_POINT ( 'NONE',  ( -2.293366432827344421E-15, -12.48450537969573659, -181.7187500020484094 ) ) ;
#17116 = CARTESIAN_POINT ( 'NONE',  ( -10.81189881249999729, 1.324075727343319199E-15, -159.5937500020484094 ) ) ;
#17117 = CARTESIAN_POINT ( 'NONE',  ( -5.405949406250003975, -9.363379034771801557, -139.8437500020484094 ) ) ;
#17118 = CARTESIAN_POINT ( 'NONE',  ( -2.293366432827344421E-15, -12.48450537969573659, -159.2187500020483526 ) ) ;
#17119 = CARTESIAN_POINT ( 'NONE',  ( 4.999999999999992006, -8.660254037844389075, -104.6250000040967763 ) ) ;
#17120 = FACE_OUTER_BOUND ( 'NONE', #26107, .T. ) ;
#17121 = CARTESIAN_POINT ( 'NONE',  ( 9.999999999999998224, 0.000000000000000000, -177.5000000000000000 ) ) ;
#17122 = CARTESIAN_POINT ( 'NONE',  ( 10.81189881249999729, 0.000000000000000000, -85.34375000204836681 ) ) ;
#17123 = CARTESIAN_POINT ( 'NONE',  ( -9.999999999999742428, -5.773502691896402084, -101.6249999999999716 ) ) ;
#17124 = CARTESIAN_POINT ( 'NONE',  ( -5.405949406249996869, 9.363379034771805109, -67.03125000204838102 ) ) ;
#17125 = CARTESIAN_POINT ( 'NONE',  ( 9.999999999999998224, 0.000000000000000000, -200.0000000000000000 ) ) ;
#17126 = CARTESIAN_POINT ( 'NONE',  ( -5.405949406249996869, 9.363379034771805109, -188.3437500020483810 ) ) ;
#17127 = CARTESIAN_POINT ( 'NONE',  ( 10.81189881249999907, 6.242252689847868297, -122.9062500020484094 ) ) ;
#17128 = AXIS2_PLACEMENT_3D ( 'NONE', #5169, #18323, #26085 ) ;
#17129 = CARTESIAN_POINT ( 'NONE',  ( 10.81189881249999551, -6.242252689847874514, -165.1562500020483526 ) ) ;
#17130 =( BOUNDED_CURVE ( )  B_SPLINE_CURVE ( 2, ( #38813, #6016, #6230, #32142, #32564, #25452, #38597 ),
 .UNSPECIFIED., .F., .F. ) 
 B_SPLINE_CURVE_WITH_KNOTS ( ( 3, 2, 2, 3 ),
 ( 0.3246268656716419510, 0.3258706467661692807, 0.3271144278606965550, 0.3283582089552238847 ),
 .UNSPECIFIED. ) 
 CURVE ( )  GEOMETRIC_REPRESENTATION_ITEM ( )  RATIONAL_B_SPLINE_CURVE ( ( 0.9999999999999820144, 0.8660254037844566932, 1.000000000000000000, 0.8660254037844387076, 1.000000000000000000, 0.8660254037844387076, 1.000000000000000000 ) ) 
 REPRESENTATION_ITEM ( '' )  );
#17131 = CARTESIAN_POINT ( 'NONE',  ( -10.81189881249999729, 1.324075727343319199E-15, -53.28125000204836681 ) ) ;
#17132 = CARTESIAN_POINT ( 'NONE',  ( -2.121150477449813534E-15, -11.54700538379251284, -137.7500000040967905 ) ) ;
#17133 = CARTESIAN_POINT ( 'NONE',  ( 9.999999999999996447, -5.773502691896262640, -108.6249999999999858 ) ) ;
#17134 = ORIENTED_EDGE ( 'NONE', *, *, #11456, .F. ) ;
#17135 = CARTESIAN_POINT ( 'NONE',  ( 7.644554776091147741E-16, 12.48450537969573659, -133.1562500020483810 ) ) ;
#17136 = CARTESIAN_POINT ( 'NONE',  ( 7.644554776091147741E-16, 12.48450537969573659, -148.1562500020484094 ) ) ;
#17137 = AXIS2_PLACEMENT_3D ( 'NONE', #24345, #8365, #1247 ) ;
#17138 = CARTESIAN_POINT ( 'NONE',  ( -10.81189881249999729, 1.324075727343319199E-15, -189.7812500020484094 ) ) ;
#17139 = CARTESIAN_POINT ( 'NONE',  ( -5.405949406249996869, 9.363379034771805109, -78.84375000204838102 ) ) ;
#17140 = VERTEX_POINT ( 'NONE', #38289 ) ;
#17141 = CARTESIAN_POINT ( 'NONE',  ( -5.000000000000003553, -8.660254037844383745, -50.49999999999998579 ) ) ;
#17142 = CARTESIAN_POINT ( 'NONE',  ( -2.293366432827344421E-15, -12.48450537969573659, -178.7187500020484094 ) ) ;
#17143 = CARTESIAN_POINT ( 'NONE',  ( -10.00000000000000000, -5.773502691896251982, -63.00000000409679757 ) ) ;
#17144 = CARTESIAN_POINT ( 'NONE',  ( -5.000000000000003553, -8.660254037844383745, -110.4999999999999858 ) ) ;
#17145 = CARTESIAN_POINT ( 'NONE',  ( -10.00000000000000000, -5.773502691896252870, -166.1249999999999716 ) ) ;
#17146 = CARTESIAN_POINT ( 'NONE',  ( -5.405949406249996869, 9.363379034771805109, -73.03125000204838102 ) ) ;
#17147 = CARTESIAN_POINT ( 'NONE',  ( -5.405949406249996869, 9.363379034771805109, -62.53125000204837391 ) ) ;
#17148 = CARTESIAN_POINT ( 'NONE',  ( 10.00000000000000000, 5.773502691896255534, -50.25000000409676204 ) ) ;
#17149 = CARTESIAN_POINT ( 'NONE',  ( -2.293366432827344421E-15, -12.48450537969573659, -6.218750002048356151 ) ) ;
#17150 = CARTESIAN_POINT ( 'NONE',  ( 4.999999999999992006, -8.660254037844389075, -35.24999999999997868 ) ) ;
#17151 = CARTESIAN_POINT ( 'NONE',  ( -10.81189881249999907, -6.242252689847864744, -180.6562500020484094 ) ) ;
#17152 = CARTESIAN_POINT ( 'NONE',  ( -5.405949406250003975, -9.363379034771801557, -5.031250002048376579 ) ) ;
#17153 = CARTESIAN_POINT ( 'NONE',  ( 9.999999999999998224, 0.000000000000000000, -147.8750000040967905 ) ) ;
#17154 = CARTESIAN_POINT ( 'NONE',  ( 7.070501591499376803E-16, 11.54700538379251284, -176.0000000040967905 ) ) ;
#17155 = DIRECTION ( 'NONE',  ( -1.000000000000000000, 0.000000000000000000, 0.000000000000000000 ) ) ;
#17156 = CARTESIAN_POINT ( 'NONE',  ( 4.999999999999992006, -8.660254037844389075, -134.6250000040967620 ) ) ;
#17157 = CARTESIAN_POINT ( 'NONE',  ( 0.000000000000000000, 0.000000000000000000, -200.0000000000000000 ) ) ;
#17159 = EDGE_LOOP ( 'NONE', ( #9728, #1272, #18401, #31260 ) ) ;
#17158 = CARTESIAN_POINT ( 'NONE',  ( -10.81189881249999907, -6.242252689847864744, -89.15625000204839523 ) ) ;
#17160 = DIRECTION ( 'NONE',  ( -0.000000000000000000, -0.000000000000000000, 1.000000000000000000 ) ) ;
#17162 = ORIENTED_EDGE ( 'NONE', *, *, #20682, .T. ) ;
#17161 = CARTESIAN_POINT ( 'NONE',  ( 9.999999999999998224, 0.000000000000000000, -162.5000000000000000 ) ) ;
#17163 = ORIENTED_EDGE ( 'NONE', *, *, #18172, .F. ) ;
#17164 = CARTESIAN_POINT ( 'NONE',  ( 5.405949406249999534, 9.363379034771803333, -28.09375000204836326 ) ) ;
#17165 = CARTESIAN_POINT ( 'NONE',  ( 7.644554776091147741E-16, 12.48450537969573659, -19.15625000204837391 ) ) ;
#17166 = VECTOR ( 'NONE', #33112, 1000.000000000000000 ) ;
#17167 = CARTESIAN_POINT ( 'NONE',  ( -10.81189881249999907, -6.242252689847864744, -67.96875000204838102 ) ) ;
#17168 = CARTESIAN_POINT ( 'NONE',  ( 4.999999999999992006, -8.660254037844389075, -122.2500000000000000 ) ) ;
#17169 = EDGE_CURVE ( 'NONE', #11948, #933, #8735, .T. ) ;
#17170 = CARTESIAN_POINT ( 'NONE',  ( -9.999999999999998224, 1.224646799147353059E-15, -46.24999999999998579 ) ) ;
#17171 = CARTESIAN_POINT ( 'NONE',  ( -10.81189881249999729, 1.324075727343319199E-15, -182.0937500020483810 ) ) ;
#17172 = EDGE_CURVE ( 'NONE', #1841, #22659, #16805, .T. ) ;
#17173 =( BOUNDED_CURVE ( )  B_SPLINE_CURVE ( 2, ( #13605, #34941, #41163, #37737, #21550, #21112, #26799 ),
 .UNSPECIFIED., .F., .F. ) 
 B_SPLINE_CURVE_WITH_KNOTS ( ( 3, 2, 2, 3 ),
 ( 0.3805970149253732338, 0.3818407960199006190, 0.3830845771144278933, 0.3843283582089552786 ),
 .UNSPECIFIED. ) 
 CURVE ( )  GEOMETRIC_REPRESENTATION_ITEM ( )  RATIONAL_B_SPLINE_CURVE ( ( 0.9999999999999880096, 0.8660254037844506980, 1.000000000000000000, 0.8660254037844387076, 1.000000000000000000, 0.8660254037844327124, 1.000000000000005995 ) ) 
 REPRESENTATION_ITEM ( '' )  );
#17174 = CARTESIAN_POINT ( 'NONE',  ( 10.81189881249999907, 6.242252689847868297, -2.718750002048360592 ) ) ;
#17175 = CARTESIAN_POINT ( 'NONE',  ( -9.999999999999998224, 1.224646799147353059E-15, -121.6250000040967905 ) ) ;
#17176 = VECTOR ( 'NONE', #42354, 1000.000000000000000 ) ;
#17177 = LINE ( 'NONE', #6427, #16382 ) ;
#17178 = CARTESIAN_POINT ( 'NONE',  ( -9.999999999999998224, 1.224646799147353059E-15, -3.125000004096767370 ) ) ;
#17179 = CARTESIAN_POINT ( 'NONE',  ( -9.999999999999998224, 1.224646799147353059E-15, -126.1250000040967620 ) ) ;
#17180 = CARTESIAN_POINT ( 'NONE',  ( -5.405949406250003975, -9.363379034771801557, -120.3437500020483952 ) ) ;
#17181 = CARTESIAN_POINT ( 'NONE',  ( -4.999999999999996447, 8.660254037844387298, -109.4999999999999858 ) ) ;
#17182 = CARTESIAN_POINT ( 'NONE',  ( 5.405949406249999534, 9.363379034771803333, -86.78125000204838102 ) ) ;
#17183 = CARTESIAN_POINT ( 'NONE',  ( -10.81189881249999729, 1.324075727343319199E-15, -98.09375000204838102 ) ) ;
#17184 = CARTESIAN_POINT ( 'NONE',  ( 5.405949406249992428, -9.363379034771808662, -70.59375000204836681 ) ) ;
#17185 = CARTESIAN_POINT ( 'NONE',  ( -10.81189881249999729, 1.324075727343319199E-15, -74.28125000204838102 ) ) ;
#17186 = CARTESIAN_POINT ( 'NONE',  ( 10.00000000000000000, 5.773502691896255534, -162.7500000040967905 ) ) ;
#17187 = CARTESIAN_POINT ( 'NONE',  ( -10.81189881249999729, -6.242252689847864744, -155.1562500020484663 ) ) ;
#17188 = CARTESIAN_POINT ( 'NONE',  ( 10.81189881249999907, 6.242252689847868297, -175.4062500020484094 ) ) ;
#17189 = CYLINDRICAL_SURFACE ( 'NONE', #33032, 9.999999999999998224 ) ;
#17190 = CARTESIAN_POINT ( 'NONE',  ( 7.070501591499376803E-16, 11.54700538379251284, -108.5000000040967763 ) ) ;
#17191 = CARTESIAN_POINT ( 'NONE',  ( -10.81189881249999907, -6.242252689847864744, -103.9687500020483668 ) ) ;
#17192 = CARTESIAN_POINT ( 'NONE',  ( 5.000000000000000000, 8.660254037844385522, -156.2500000000000000 ) ) ;
#17193 = CARTESIAN_POINT ( 'NONE',  ( -4.999999999999996447, 8.660254037844387298, -70.49999999999998579 ) ) ;
#17194 = CARTESIAN_POINT ( 'NONE',  ( -10.81189881249999907, -6.242252689847864744, -5.156250002048362369 ) ) ;
#17195 = CARTESIAN_POINT ( 'NONE',  ( 10.00000000000000000, 5.773502691896255534, -90.75000000409677625 ) ) ;
#17196 = CARTESIAN_POINT ( 'NONE',  ( 7.644554776091147741E-16, 12.48450537969573659, -101.6562500020483952 ) ) ;
#17197 = CARTESIAN_POINT ( 'NONE',  ( -2.293366432827344421E-15, -12.48450537969573659, -82.90625000204838102 ) ) ;
#17198 = CARTESIAN_POINT ( 'NONE',  ( -2.121150477449813534E-15, -11.54700538379251284, -77.75000000409677625 ) ) ;
#17199 = CARTESIAN_POINT ( 'NONE',  ( -10.00000000000154188, 5.773502691895366468, -20.87499999999993250 ) ) ;
#17200 = CARTESIAN_POINT ( 'NONE',  ( -2.293366432827344421E-15, -12.48450537969573659, -34.71875000204835260 ) ) ;
#17201 = ORIENTED_EDGE ( 'NONE', *, *, #18251, .F. ) ;
#17202 = CARTESIAN_POINT ( 'NONE',  ( 7.070501591499377789E-16, 11.54700538379251284, -7.624999999999972466 ) ) ;
#17203 = CARTESIAN_POINT ( 'NONE',  ( -2.293366432827344421E-15, -12.48450537969573659, -25.90625000204838102 ) ) ;
#17204 = CARTESIAN_POINT ( 'NONE',  ( 4.999999999999992006, -8.660254037844389075, -143.2500000000000000 ) ) ;
#17205 = CARTESIAN_POINT ( 'NONE',  ( 4.999999999999992006, -8.660254037844389075, -14.62500000409674961 ) ) ;
#17206 = CARTESIAN_POINT ( 'NONE',  ( 9.999999999999998224, 0.000000000000000000, -3.875000004096768258 ) ) ;
#17207 = CARTESIAN_POINT ( 'NONE',  ( -2.293366432827344421E-15, -12.48450537969573659, -135.4062500020483810 ) ) ;
#17208 = CARTESIAN_POINT ( 'NONE',  ( -4.999999999999996447, 8.660254037844387298, -193.5000000000000000 ) ) ;
#17209 = CARTESIAN_POINT ( 'NONE',  ( 0.000000000000000000, 0.000000000000000000, -200.0000000000000000 ) ) ;
#17211 = ORIENTED_EDGE ( 'NONE', *, *, #30964, .T. ) ;
#17210 = CARTESIAN_POINT ( 'NONE',  ( 7.644554776091147741E-16, 12.48450537969573659, -121.1562500020483952 ) ) ;
#17212 = FACE_OUTER_BOUND ( 'NONE', #22971, .T. ) ;
#17213 = VERTEX_POINT ( 'NONE', #10507 ) ;
#17214 = ORIENTED_EDGE ( 'NONE', *, *, #28094, .T. ) ;
#17215 = CARTESIAN_POINT ( 'NONE',  ( 7.644554776091147741E-16, 12.48450537969573659, -46.15625000204837391 ) ) ;
#17216 = APPROVAL_STATUS ( 'not_yet_approved' ) ;
#17217 = CARTESIAN_POINT ( 'NONE',  ( 5.405949406249992428, -9.363379034771808662, -96.09375000204838102 ) ) ;
#17218 = CARTESIAN_POINT ( 'NONE',  ( -5.405949406250003975, -9.363379034771801557, -123.5312500020483952 ) ) ;
#17220 = ORIENTED_EDGE ( 'NONE', *, *, #1751, .T. ) ;
#17219 = EDGE_CURVE ( 'NONE', #24467, #36911, #8311, .T. ) ;
#17221 = CARTESIAN_POINT ( 'NONE',  ( -8.667397162551022660, -4.987630568095290151, -0.0003570992120843448142 ) ) ;
#17222 = DIRECTION ( 'NONE',  ( 1.000000000000000000, 0.000000000000000000, 0.000000000000000000 ) ) ;
#17223 = EDGE_CURVE ( 'NONE', #26104, #37116, #17952, .T. ) ;
#17224 = CARTESIAN_POINT ( 'NONE',  ( -10.81189881249999729, 6.242252689847871849, -171.9062500020484094 ) ) ;
#17225 = DIRECTION ( 'NONE',  ( -0.000000000000000000, -0.000000000000000000, 1.000000000000000000 ) ) ;
#17226 = AXIS2_PLACEMENT_3D ( 'NONE', #2695, #29025, #9164 ) ;
#17227 = EDGE_CURVE ( 'NONE', #40108, #41753, #2241, .T. ) ;
#17228 = CARTESIAN_POINT ( 'NONE',  ( -10.81189881249999729, 6.242252689847871849, -125.2187500020483810 ) ) ;
#17229 = CC_DESIGN_PERSON_AND_ORGANIZATION_ASSIGNMENT ( #29876, #26630, ( #14563 ) ) ;
#17230 = CARTESIAN_POINT ( 'NONE',  ( -10.81189881249999729, 1.324075727343319199E-15, -96.59375000204838102 ) ) ;
#17231 = CARTESIAN_POINT ( 'NONE',  ( 5.000000000000000000, 8.660254037844385522, -154.7500000000000000 ) ) ;
#17232 = CARTESIAN_POINT ( 'NONE',  ( -5.405949406250003975, -9.363379034771801557, -101.0312500020483952 ) ) ;
#17233 = CARTESIAN_POINT ( 'NONE',  ( -4.999999999999996447, 8.660254037844387298, -187.8750000040967905 ) ) ;
#17234 = CARTESIAN_POINT ( 'NONE',  ( -5.405949406250003975, -9.363379034771801557, -103.8437500020483810 ) ) ;
#17235 = CARTESIAN_POINT ( 'NONE',  ( -10.81189881249999729, 6.242252689847871849, -177.9062500020484094 ) ) ;
#17236 = CARTESIAN_POINT ( 'NONE',  ( 4.999999999999992006, -8.660254037844389075, -104.6250000040967763 ) ) ;
#17237 = DIRECTION ( 'NONE',  ( -1.000000000000000000, 0.000000000000000000, 0.000000000000000000 ) ) ;
#17238 = CARTESIAN_POINT ( 'NONE',  ( -10.81189881249999729, 1.324075727343319199E-15, -192.7812500020484094 ) ) ;
#17239 = CARTESIAN_POINT ( 'NONE',  ( 5.405949406249999534, 9.363379034771803333, -52.09375000204835260 ) ) ;
#17240 = CARTESIAN_POINT ( 'NONE',  ( -10.81189881249999729, 1.324075727343319199E-15, -42.59375000204837391 ) ) ;
#17241 = CARTESIAN_POINT ( 'NONE',  ( -9.999999999999998224, 1.224646799147353059E-15, -169.6250000040967905 ) ) ;
#17242 = CARTESIAN_POINT ( 'NONE',  ( -2.293366432827344421E-15, -12.48450537969573659, -9.406250002048375691 ) ) ;
#17243 = CARTESIAN_POINT ( 'NONE',  ( -10.81189881249999907, -6.242252689847864744, -22.96875000204837036 ) ) ;
#17244 = CARTESIAN_POINT ( 'NONE',  ( 79.99999999999998579, -40.00000000000001421, -160.0000000000000000 ) ) ;
#17245 = CARTESIAN_POINT ( 'NONE',  ( -10.81189881249999729, 6.242252689847871849, -129.7187500020483810 ) ) ;
#17246 = CARTESIAN_POINT ( 'NONE',  ( -9.999999999999998224, 1.224646799147353059E-15, -103.2500000000000000 ) ) ;
#17247 = CARTESIAN_POINT ( 'NONE',  ( 5.405949406249999534, 9.363379034771803333, -28.28125000204837036 ) ) ;
#17248 = CARTESIAN_POINT ( 'NONE',  ( 9.999999999999998224, 0.000000000000000000, -4.999999999999976907 ) ) ;
#17249 = CARTESIAN_POINT ( 'NONE',  ( -2.121150477449813534E-15, -11.54700538379251284, -56.37499999999997868 ) ) ;
#17250 = CARTESIAN_POINT ( 'NONE',  ( -5.405949406250003975, -9.363379034771801557, -122.0312500020483952 ) ) ;
#17251 = CARTESIAN_POINT ( 'NONE',  ( 5.405949406249999534, 9.363379034771803333, -106.2812500020483810 ) ) ;
#17252 = ORIENTED_EDGE ( 'NONE', *, *, #6863, .T. ) ;
#17253 = CARTESIAN_POINT ( 'NONE',  ( -9.999999999999998224, 1.224646799147353059E-15, -128.7499999999999716 ) ) ;
#17254 = CARTESIAN_POINT ( 'NONE',  ( 10.00000000000000000, 5.773502691896255534, -101.2500000040967905 ) ) ;
#17255 = CARTESIAN_POINT ( 'NONE',  ( 0.000000000000000000, 0.000000000000000000, -200.0000000000000000 ) ) ;
#17256 = CARTESIAN_POINT ( 'NONE',  ( -2.293366432827344421E-15, -12.48450537969573659, -54.21875000204837391 ) ) ;
#17257 = VERTEX_POINT ( 'NONE', #29012 ) ;
#17258 = CARTESIAN_POINT ( 'NONE',  ( -10.00000000000000000, -5.773502691896251982, -32.62499999999995737 ) ) ;
#17259 = CARTESIAN_POINT ( 'NONE',  ( -2.293366432827344421E-15, -12.48450537969573659, -36.40625000204835970 ) ) ;
#17260 = CARTESIAN_POINT ( 'NONE',  ( -9.999999999999479527, -5.773502691896549521, -91.12499999999995737 ) ) ;
#17261 = CARTESIAN_POINT ( 'NONE',  ( 4.999999999999992006, -8.660254037844389075, -28.12500000409676204 ) ) ;
#17262 = CARTESIAN_POINT ( 'NONE',  ( 9.999999999999998224, 0.000000000000000000, -12.49999999999995559 ) ) ;
#17263 = AXIS2_PLACEMENT_3D ( 'NONE', #39888, #26527, #10322 ) ;
#17264 = CARTESIAN_POINT ( 'NONE',  ( -2.293366432827344421E-15, -12.48450537969573659, -139.9062500020484094 ) ) ;
#17265 = AXIS2_PLACEMENT_3D ( 'NONE', #31801, #38042, #14713 ) ;
#17266 = DIRECTION ( 'NONE',  ( 0.000000000000000000, 0.000000000000000000, -1.000000000000000000 ) ) ;
#17267 = VERTEX_POINT ( 'NONE', #6132 ) ;
#17268 = ORIENTED_EDGE ( 'NONE', *, *, #39307, .T. ) ;
#17269 = CARTESIAN_POINT ( 'NONE',  ( -4.999999999999996447, 8.660254037844387298, -113.9999999999999858 ) ) ;
#17270 = DIRECTION ( 'NONE',  ( -1.062296840242595709E-16, 0.7071067811865493491, 0.7071067811865456854 ) ) ;
#17271 = CARTESIAN_POINT ( 'NONE',  ( -2.293366432827344421E-15, -12.48450537969573659, -169.7187500020483810 ) ) ;
#17272 = CARTESIAN_POINT ( 'NONE',  ( -10.81189881249999907, -6.242252689847864744, -195.6562500020484094 ) ) ;
#17273 = CARTESIAN_POINT ( 'NONE',  ( -10.81189881249999729, 6.242252689847871849, -18.71875000204837391 ) ) ;
#17274 = CARTESIAN_POINT ( 'NONE',  ( 10.00000000000025402, -5.773502691896113426, -157.0000000040968189 ) ) ;
#17275 = CARTESIAN_POINT ( 'NONE',  ( -10.81189881249999729, 1.324075727343319199E-15, -144.5937500020483810 ) ) ;
#17276 = CARTESIAN_POINT ( 'NONE',  ( 10.81189881249999729, 0.000000000000000000, -134.8437500020484094 ) ) ;
#17277 = CARTESIAN_POINT ( 'NONE',  ( -5.405949406249996869, 9.363379034771805109, -104.5312500020483810 ) ) ;
#17278 = CARTESIAN_POINT ( 'NONE',  ( -2.293366432827344421E-15, -12.48450537969573659, -118.7187500020483952 ) ) ;
#17279 = CARTESIAN_POINT ( 'NONE',  ( -9.999999999999998224, 1.224646799147353059E-15, -198.1250000040967905 ) ) ;
#17280 = CARTESIAN_POINT ( 'NONE',  ( -5.405949406249996869, 9.363379034771805109, -125.5312500020483952 ) ) ;
#17281 = CARTESIAN_POINT ( 'NONE',  ( -10.81189881249999729, 6.242252689847871849, -9.718750002048363257 ) ) ;
#17282 = CARTESIAN_POINT ( 'NONE',  ( -5.405949406249996869, 9.363379034771805109, -131.3437500020484094 ) ) ;
#17283 = AXIS2_PLACEMENT_3D ( 'NONE', #10575, #36915, #3913 ) ;
#17284 = CARTESIAN_POINT ( 'NONE',  ( -9.999999999999998224, 1.224646799147353059E-15, -162.1250000040967905 ) ) ;
#17285 = CARTESIAN_POINT ( 'NONE',  ( -9.999999999999998224, 1.224646799147353059E-15, -70.62500000409677625 ) ) ;
#17286 = CARTESIAN_POINT ( 'NONE',  ( -2.121150477449813534E-15, -11.54700538379251284, -156.8750000000000000 ) ) ;
#17287 = CARTESIAN_POINT ( 'NONE',  ( -10.00000000000000000, -5.773502691896251982, -20.62499999999997868 ) ) ;
#17288 = APPROVAL_PERSON_ORGANIZATION ( #30627, #38361, #27165 ) ;
#17289 = ADVANCED_FACE ( 'NONE', ( #35909 ), #38721, .T. ) ;
#17290 = CARTESIAN_POINT ( 'NONE',  ( 10.81189881249999729, 6.242252689847867408, -80.71875000204838102 ) ) ;
#17291 = CARTESIAN_POINT ( 'NONE',  ( -5.405949406249996869, 9.363379034771805109, -65.34375000204836681 ) ) ;
#17292 = DIRECTION ( 'NONE',  ( 0.000000000000000000, 0.000000000000000000, -1.000000000000000000 ) ) ;
#17293 = CARTESIAN_POINT ( 'NONE',  ( 10.81189881249999551, -6.242252689847874514, -39.15625000204835260 ) ) ;
#17294 = CARTESIAN_POINT ( 'NONE',  ( 5.405949406249999534, 9.363379034771803333, -47.59375000204838102 ) ) ;
#17295 = CARTESIAN_POINT ( 'NONE',  ( -5.405949406249996869, 9.363379034771805109, -156.8437500020483810 ) ) ;
#17296 = CARTESIAN_POINT ( 'NONE',  ( -2.121150477449813534E-15, -11.54700538379251284, -129.8750000000000000 ) ) ;
#17297 = CARTESIAN_POINT ( 'NONE',  ( 5.405949406249992428, -9.363379034771808662, -132.2812500020483810 ) ) ;
#17298 = CARTESIAN_POINT ( 'NONE',  ( 10.00000000000102318, -5.773502691895667560, -67.00000000409674783 ) ) ;
#17299 = CARTESIAN_POINT ( 'NONE',  ( 7.070501591499377789E-16, 11.54700538379251284, -87.12499999999997158 ) ) ;
#17300 = CARTESIAN_POINT ( 'NONE',  ( -10.81189881249999729, 1.324075727343319199E-15, -21.78125000204836326 ) ) ;
#17301 =( BOUNDED_CURVE ( )  B_SPLINE_CURVE ( 2, ( #14764, #5081, #40665, #21687, #11105, #38092, #1209 ),
 .UNSPECIFIED., .F., .F. ) 
 B_SPLINE_CURVE_WITH_KNOTS ( ( 3, 2, 2, 3 ),
 ( 0.2537313432835822113, 0.2549751243781095411, 0.2562189054726369264, 0.2574626865671643117 ),
 .UNSPECIFIED. ) 
 CURVE ( )  GEOMETRIC_REPRESENTATION_ITEM ( )  RATIONAL_B_SPLINE_CURVE ( ( 0.9999999999999880096, 0.8660254037844506980, 1.000000000000000000, 0.8660254037844387076, 1.000000000000000000, 0.8660254037844267172, 1.000000000000011990 ) ) 
 REPRESENTATION_ITEM ( '' )  );
#17302 = ORIENTED_EDGE ( 'NONE', *, *, #1806, .T. ) ;
#17303 = CARTESIAN_POINT ( 'NONE',  ( 10.81189881249999551, -6.242252689847874514, -114.1562500020483952 ) ) ;
#17304 = CARTESIAN_POINT ( 'NONE',  ( -4.999999999999996447, 8.660254037844387298, -124.8750000040967763 ) ) ;
#17305 = CARTESIAN_POINT ( 'NONE',  ( 4.999999999999992006, -8.660254037844389075, -111.7499999999999858 ) ) ;
#17306 = CARTESIAN_POINT ( 'NONE',  ( -4.999999999999996447, 8.660254037844387298, -37.87500000409676915 ) ) ;
#17307 = PRODUCT_DEFINITION_SHAPE ( 'NONE', 'NONE',  #3281 ) ;
#17308 = DIRECTION ( 'NONE',  ( -0.000000000000000000, -0.000000000000000000, 1.000000000000000000 ) ) ;
#17309 = CARTESIAN_POINT ( 'NONE',  ( -10.81189881249999729, 1.324075727343319199E-15, -56.28125000204836681 ) ) ;
#17310 = CARTESIAN_POINT ( 'NONE',  ( -2.121150477449813534E-15, -11.54700538379251284, -146.3749999999999716 ) ) ;
#17311 = CARTESIAN_POINT ( 'NONE',  ( 10.81189881249999729, 0.000000000000000000, -154.5312500020484094 ) ) ;
#17312 = CARTESIAN_POINT ( 'NONE',  ( 10.81189881249999729, 0.000000000000000000, -131.8437500020484094 ) ) ;
#17313 = CARTESIAN_POINT ( 'NONE',  ( -9.999999999999998224, 1.224646799147353059E-15, -109.2499999999999858 ) ) ;
#17314 = EDGE_LOOP ( 'NONE', ( #3423, #29448, #28610, #4496 ) ) ;
#17315 = DIRECTION ( 'NONE',  ( -0.000000000000000000, -0.000000000000000000, 1.000000000000000000 ) ) ;
#17316 = ORIENTED_EDGE ( 'NONE', *, *, #29405, .T. ) ;
#17317 = CC_DESIGN_SECURITY_CLASSIFICATION ( #27668, ( #24948 ) ) ;
#17318 = VERTEX_POINT ( 'NONE', #22322 ) ;
#17319 = CALENDAR_DATE ( 2026, 28, 9 ) ;
#17321 = ORIENTED_EDGE ( 'NONE', *, *, #38527, .T. ) ;
#17320 = CARTESIAN_POINT ( 'NONE',  ( -2.293366432827344421E-15, -12.48450537969573659, -112.7187500020483952 ) ) ;
#17322 = CARTESIAN_POINT ( 'NONE',  ( -2.121150477449813534E-15, -11.54700538379251284, -145.2500000040967905 ) ) ;
#17323 = CARTESIAN_POINT ( 'NONE',  ( -10.81189881249999729, 6.242252689847871849, -191.2187500020484663 ) ) ;
#17324 = CIRCLE ( 'NONE', #4259, 24.99999999999999645 ) ;
#17325 = CARTESIAN_POINT ( 'NONE',  ( 10.81189881249999907, 6.242252689847868297, -43.21875000204835970 ) ) ;
#17326 = CARTESIAN_POINT ( 'NONE',  ( -9.999999999999998224, 1.224646799147353059E-15, -181.2500000000000284 ) ) ;
#17327 = CARTESIAN_POINT ( 'NONE',  ( 0.000000000000000000, 0.000000000000000000, -99.99999999999998579 ) ) ;
#17328 = CARTESIAN_POINT ( 'NONE',  ( 5.405949406249999534, 9.363379034771803333, -182.5937500020483810 ) ) ;
#17329 = CARTESIAN_POINT ( 'NONE',  ( -2.293366432827344421E-15, -12.48450537969573659, -160.7187500020483810 ) ) ;
#17330 = CARTESIAN_POINT ( 'NONE',  ( -5.000000000000003553, -8.660254037844383745, -65.87500000409676204 ) ) ;
#17331 = CARTESIAN_POINT ( 'NONE',  ( -10.81189881249999729, 6.242252689847871849, -138.7187500020483810 ) ) ;
#17332 = CARTESIAN_POINT ( 'NONE',  ( 7.644554776091147741E-16, 12.48450537969573659, -161.4687500020484094 ) ) ;
#17333 = CARTESIAN_POINT ( 'NONE',  ( -1.040834085586084257E-14, -145.0000000000000000, 22.49999999999999289 ) ) ;
#17334 = DIRECTION ( 'NONE',  ( -0.000000000000000000, -0.000000000000000000, 1.000000000000000000 ) ) ;
#17335 = CARTESIAN_POINT ( 'NONE',  ( -4.999999999999996447, 8.660254037844387298, -177.0000000000000000 ) ) ;
#17336 = CARTESIAN_POINT ( 'NONE',  ( 10.81189881249999729, 0.000000000000000000, -88.34375000204838102 ) ) ;
#17337 = CYLINDRICAL_SURFACE ( 'NONE', #34164, 9.999999999999998224 ) ;
#17338 = CARTESIAN_POINT ( 'NONE',  ( 10.81189881249999907, 6.242252689847868297, -64.40625000204839523 ) ) ;
#17339 = CARTESIAN_POINT ( 'NONE',  ( -10.81189881249999729, 6.242252689847871849, -174.7187500020483810 ) ) ;
#17340 = CARTESIAN_POINT ( 'NONE',  ( 5.405949406249992428, -9.363379034771808662, -123.2812500020483952 ) ) ;
#17341 = CARTESIAN_POINT ( 'NONE',  ( 5.405949406249992428, -9.363379034771808662, -151.7812500020484094 ) ) ;
#17342 = CARTESIAN_POINT ( 'NONE',  ( 10.81189881249999551, -6.242252689847874514, -51.15625000204837391 ) ) ;
#17343 = CARTESIAN_POINT ( 'NONE',  ( 5.000000000000000000, 8.660254037844385522, -126.6250000040967620 ) ) ;
#17344 = CARTESIAN_POINT ( 'NONE',  ( 5.000000000000000000, 8.660254037844385522, -108.2499999999999858 ) ) ;
#17345 = VERTEX_POINT ( 'NONE', #5923 ) ;
#17346 = CARTESIAN_POINT ( 'NONE',  ( -10.81189881249999729, -6.242252689847864744, -135.6562500020484094 ) ) ;
#17347 = CARTESIAN_POINT ( 'NONE',  ( 4.999999999999992006, -8.660254037844389075, -158.6250000040967905 ) ) ;
#17348 = CARTESIAN_POINT ( 'NONE',  ( 10.81189881249999551, -6.242252689847874514, -148.6562500020484094 ) ) ;
#17349 = CARTESIAN_POINT ( 'NONE',  ( -5.405949406249996869, 9.363379034771805109, -187.0312500020484094 ) ) ;
#17350 = CARTESIAN_POINT ( 'NONE',  ( 5.405949406249992428, -9.363379034771808662, -82.59375000204836681 ) ) ;
#17351 = EDGE_LOOP ( 'NONE', ( #27058, #10310, #1429, #4972 ) ) ;
#17352 = CARTESIAN_POINT ( 'NONE',  ( -10.00000000000000000, -5.773502691896251982, -49.12499999999997158 ) ) ;
#17353 = CARTESIAN_POINT ( 'NONE',  ( -2.293366432827344421E-15, -12.48450537969573659, -177.2187500020484094 ) ) ;
#17354 = CARTESIAN_POINT ( 'NONE',  ( 9.999999999999996447, -5.773502691896262640, -56.50000000409677625 ) ) ;
#17355 = CARTESIAN_POINT ( 'NONE',  ( -5.000000000000003553, -8.660254037844383745, -172.0000000000000000 ) ) ;
#17356 = CYLINDRICAL_SURFACE ( 'NONE', #41516, 9.999999999999998224 ) ;
#17357 = CARTESIAN_POINT ( 'NONE',  ( 10.81189881249999551, -6.242252689847874514, -76.65625000204838102 ) ) ;
#17358 = CARTESIAN_POINT ( 'NONE',  ( 10.81189881249999729, 0.000000000000000000, -61.53125000204837391 ) ) ;
#17359 = EDGE_CURVE ( 'NONE', #20251, #27593, #9152, .T. ) ;
#17360 = CARTESIAN_POINT ( 'NONE',  ( 5.000000000000000000, 8.660254037844385522, -54.62500000409675494 ) ) ;
#17361 = CARTESIAN_POINT ( 'NONE',  ( 5.405949406249999534, 9.363379034771803333, -11.59375000204834727 ) ) ;
#17362 = CARTESIAN_POINT ( 'NONE',  ( -1.040834085586084257E-14, -145.0000000000000000, 37.50000000000000711 ) ) ;
#17363 = CARTESIAN_POINT ( 'NONE',  ( -5.405949406249996869, 9.363379034771805109, -175.0312500020484094 ) ) ;
#17364 = CARTESIAN_POINT ( 'NONE',  ( -5.405949406250003975, -9.363379034771801557, -2.031250002048373915 ) ) ;
#17365 = LINE ( 'NONE', #14763, #12500 ) ;
#17366 = CARTESIAN_POINT ( 'NONE',  ( -2.121150477449813534E-15, -11.54700538379251284, -81.87500000000000000 ) ) ;
#17367 = DIRECTION ( 'NONE',  ( -1.000000000000000000, 8.673617379884033500E-16, 0.000000000000000000 ) ) ;
#17368 = CARTESIAN_POINT ( 'NONE',  ( 7.070501591499376803E-16, 11.54700538379251284, -105.5000000040967763 ) ) ;
#17369 = CARTESIAN_POINT ( 'NONE',  ( -5.000000000000003553, -8.660254037844383745, -169.3750000040967905 ) ) ;
#17371 = VERTEX_POINT ( 'NONE', #15816 ) ;
#17370 = CARTESIAN_POINT ( 'NONE',  ( 10.81189881249999551, -6.242252689847874514, -88.65625000204838102 ) ) ;
#17372 = DIRECTION ( 'NONE',  ( 0.000000000000000000, 0.000000000000000000, 1.000000000000000000 ) ) ;
#17374 = VERTEX_POINT ( 'NONE', #16233 ) ;
#17373 = CARTESIAN_POINT ( 'NONE',  ( -2.121150477449813534E-15, -11.54700538379251284, -69.87499999999998579 ) ) ;
#17375 = ORIENTED_EDGE ( 'NONE', *, *, #37933, .F. ) ;
#17376 = VECTOR ( 'NONE', #40443, 1000.000000000000000 ) ;
#17377 = CARTESIAN_POINT ( 'NONE',  ( 5.405949406249999534, 9.363379034771803333, -29.59375000204836326 ) ) ;
#17378 = CARTESIAN_POINT ( 'NONE',  ( -5.405949406250003975, -9.363379034771801557, -15.53125000204835793 ) ) ;
#17379 = CARTESIAN_POINT ( 'NONE',  ( 10.81189881249999907, 6.242252689847868297, -64.21875000204838102 ) ) ;
#17380 = CARTESIAN_POINT ( 'NONE',  ( -5.000000000000003553, -8.660254037844383745, -122.5000000000000000 ) ) ;
#17381 = CARTESIAN_POINT ( 'NONE',  ( -5.000000000000003553, -8.660254037844383745, -42.99999999999998579 ) ) ;
#17382 = CARTESIAN_POINT ( 'NONE',  ( 7.644554776091147741E-16, 12.48450537969573659, -183.9687500020484094 ) ) ;
#17383 =( BOUNDED_CURVE ( )  B_SPLINE_CURVE ( 2, ( #25859, #10285, #7067, #32973, #13302, #36199, #42450 ),
 .UNSPECIFIED., .F., .F. ) 
 B_SPLINE_CURVE_WITH_KNOTS ( ( 3, 2, 2, 3 ),
 ( 0.5932835820895523415, 0.5945273631840797268, 0.5957711442786072231, 0.5970149253731344974 ),
 .UNSPECIFIED. ) 
 CURVE ( )  GEOMETRIC_REPRESENTATION_ITEM ( )  RATIONAL_B_SPLINE_CURVE ( ( 0.9999999999999880096, 0.8660254037844506980, 1.000000000000000000, 0.8660254037844387076, 1.000000000000000000, 0.8660254037844148378, 1.000000000000023981 ) ) 
 REPRESENTATION_ITEM ( '' )  );
#17384 = CARTESIAN_POINT ( 'NONE',  ( 10.81189881249999907, 6.242252689847868297, -167.7187500020483810 ) ) ;
#17385 = CARTESIAN_POINT ( 'NONE',  ( 9.999999999999998224, 0.000000000000000000, -21.87500000409675494 ) ) ;
#17386 = CARTESIAN_POINT ( 'NONE',  ( -9.999999999999998224, 1.224646799147353059E-15, -100.2499999999999858 ) ) ;
#17387 = CARTESIAN_POINT ( 'NONE',  ( -10.00000000000051337, 5.773502691895962435, -146.8749999999999716 ) ) ;
#17388 = CARTESIAN_POINT ( 'NONE',  ( -9.999999999999227285, -5.773502691896698735, -104.6249999999999574 ) ) ;
#17389 = AXIS2_PLACEMENT_3D ( 'NONE', #22480, #35023, #35656 ) ;
#17390 = FACE_OUTER_BOUND ( 'NONE', #39662, .T. ) ;
#17391 = CARTESIAN_POINT ( 'NONE',  ( -2.293366432827344421E-15, -12.48450537969573659, -114.2187500020483668 ) ) ;
#17392 = CARTESIAN_POINT ( 'NONE',  ( -9.999999999999998224, 1.224646799147353059E-15, -54.12500000409675494 ) ) ;
#17393 = CARTESIAN_POINT ( 'NONE',  ( -10.81189881249999729, 1.324075727343319199E-15, -92.28125000204838102 ) ) ;
#17394 = CARTESIAN_POINT ( 'NONE',  ( 5.405949406249992428, -9.363379034771808662, -103.5937500020483668 ) ) ;
#17395 = CARTESIAN_POINT ( 'NONE',  ( 10.81189881249999907, 6.242252689847868297, -67.21875000204838102 ) ) ;
#17396 = CARTESIAN_POINT ( 'NONE',  ( -2.293366432827344421E-15, -12.48450537969573659, -79.90625000204839523 ) ) ;
#17397 = CARTESIAN_POINT ( 'NONE',  ( 10.00000000000000000, 5.773502691896255534, -153.7500000040967905 ) ) ;
#17398 = CARTESIAN_POINT ( 'NONE',  ( 10.00000000000000000, 5.773502691896255534, -130.8750000000000000 ) ) ;
#17399 = CARTESIAN_POINT ( 'NONE',  ( -10.81189881249999729, 1.324075727343319199E-15, -159.7812500020484094 ) ) ;
#17400 = CARTESIAN_POINT ( 'NONE',  ( 5.405949406249992428, -9.363379034771808662, -175.7812500020484094 ) ) ;
#17401 = DIRECTION ( 'NONE',  ( 1.000000000000000000, 0.000000000000000000, 0.000000000000000000 ) ) ;
#17402 = LINE ( 'NONE', #23913, #40118 ) ;
#17403 = CARTESIAN_POINT ( 'NONE',  ( -10.81189881249999729, 1.324075727343319199E-15, -108.5937500020483810 ) ) ;
#17404 = CARTESIAN_POINT ( 'NONE',  ( 9.999999999998969713, 5.773502691896851502, -10.87499999999993072 ) ) ;
#17405 = CARTESIAN_POINT ( 'NONE',  ( -4.999999999999996447, 8.660254037844387298, -76.49999999999998579 ) ) ;
#17406 = CARTESIAN_POINT ( 'NONE',  ( -5.405949406249996869, 9.363379034771805109, -5.531250002048376579 ) ) ;
#17407 = CARTESIAN_POINT ( 'NONE',  ( 7.070501591499377789E-16, 11.54700538379251284, -89.00000000409677625 ) ) ;
#17408 = CARTESIAN_POINT ( 'NONE',  ( 9.999999999999994671, -5.773502691896262640, -168.6250000000000000 ) ) ;
#17409 = CARTESIAN_POINT ( 'NONE',  ( -5.405949406249996869, 9.363379034771805109, -98.53125000204839523 ) ) ;
#17410 = CARTESIAN_POINT ( 'NONE',  ( 7.644554776091147741E-16, 12.48450537969573659, -82.15625000204839523 ) ) ;
#17411 = CARTESIAN_POINT ( 'NONE',  ( 9.999999999999998224, 0.000000000000000000, -72.87500000409677625 ) ) ;
#17412 = CARTESIAN_POINT ( 'NONE',  ( -9.999999999999998224, 1.224646799147353059E-15, -19.24999999999996092 ) ) ;
#17413 = CARTESIAN_POINT ( 'NONE',  ( 10.81189881249999729, 0.000000000000000000, -31.34375000204836681 ) ) ;
#17414 = VERTEX_POINT ( 'NONE', #15397 ) ;
#17415 = CARTESIAN_POINT ( 'NONE',  ( 4.999999999999992006, -8.660254037844389075, -3.749999999999975575 ) ) ;
#17416 = CARTESIAN_POINT ( 'NONE',  ( -2.293366432827344421E-15, -12.48450537969573659, -28.90625000204835615 ) ) ;
#17417 = ADVANCED_FACE ( 'NONE', ( #16025 ), #32048, .T. ) ;
#17418 = CARTESIAN_POINT ( 'NONE',  ( -10.81189881249999729, -6.242252689847864744, -13.96875000204836681 ) ) ;
#17419 = CARTESIAN_POINT ( 'NONE',  ( 9.999999999999998224, 0.000000000000000000, -116.3750000040967905 ) ) ;
#17420 = CARTESIAN_POINT ( 'NONE',  ( -5.000000000000003553, -8.660254037844383745, -7.375000004096743389 ) ) ;
#17421 = CARTESIAN_POINT ( 'NONE',  ( -5.405949406250003975, -9.363379034771801557, -134.0312500020484094 ) ) ;
#17422 = CARTESIAN_POINT ( 'NONE',  ( 9.999999999999996447, -5.773502691896262640, -179.1250000000000284 ) ) ;
#17423 = CARTESIAN_POINT ( 'NONE',  ( -9.999999999999998224, 0.000000000000000000, -99.99999999999998579 ) ) ;
#17425 = ORIENTED_EDGE ( 'NONE', *, *, #20666, .T. ) ;
#17424 = CARTESIAN_POINT ( 'NONE',  ( 10.81189881249999729, 0.000000000000000000, -111.0312500020483810 ) ) ;
#17426 = CARTESIAN_POINT ( 'NONE',  ( -9.999999999999998224, 1.224646799147353059E-15, -194.7500000000000000 ) ) ;
#17427 = ORIENTED_EDGE ( 'NONE', *, *, #21492, .F. ) ;
#17428 = ORIENTED_EDGE ( 'NONE', *, *, #7910, .T. ) ;
#17429 =( BOUNDED_CURVE ( )  B_SPLINE_CURVE ( 2, ( #39746, #16856, #10181, #502, #13617, #23367, #16427 ),
 .UNSPECIFIED., .F., .F. ) 
 B_SPLINE_CURVE_WITH_KNOTS ( ( 3, 2, 2, 3 ),
 ( 0.3470149253731344974, 0.3482587064676618271, 0.3495024875621891569, 0.3507462686567164867 ),
 .UNSPECIFIED. ) 
 CURVE ( )  GEOMETRIC_REPRESENTATION_ITEM ( )  RATIONAL_B_SPLINE_CURVE ( ( 0.9999999999999820144, 0.8660254037844566932, 1.000000000000000000, 0.8660254037844387076, 1.000000000000000000, 0.8660254037844327124, 1.000000000000005995 ) ) 
 REPRESENTATION_ITEM ( '' )  );
#17430 = CARTESIAN_POINT ( 'NONE',  ( 5.405949406249999534, 9.363379034771803333, -35.78125000204837391 ) ) ;
#17431 = PERSON_AND_ORGANIZATION_ROLE ( 'creator' ) ;
#17432 = CARTESIAN_POINT ( 'NONE',  ( 7.644554776091147741E-16, 12.48450537969573659, -92.46875000204838102 ) ) ;
#17433 = DIRECTION ( 'NONE',  ( -0.000000000000000000, -0.000000000000000000, 1.000000000000000000 ) ) ;
#17434 = DIRECTION ( 'NONE',  ( -0.000000000000000000, -0.000000000000000000, 1.000000000000000000 ) ) ;
#17435 =( BOUNDED_CURVE ( )  B_SPLINE_CURVE ( 2, ( #5516, #32068, #21488, #28190, #41750, #24963, #2502 ),
 .UNSPECIFIED., .F., .F. ) 
 B_SPLINE_CURVE_WITH_KNOTS ( ( 3, 2, 2, 3 ),
 ( 0.6194029850746269883, 0.6206467661691543736, 0.6218905472636816478, 0.6231343283582090331 ),
 .UNSPECIFIED. ) 
 CURVE ( )  GEOMETRIC_REPRESENTATION_ITEM ( )  RATIONAL_B_SPLINE_CURVE ( ( 0.9999999999999880096, 0.8660254037844506980, 1.000000000000000000, 0.8660254037844387076, 1.000000000000000000, 0.8660254037844267172, 1.000000000000011990 ) ) 
 REPRESENTATION_ITEM ( '' )  );
#17436 = CARTESIAN_POINT ( 'NONE',  ( 10.81189881249999729, 0.000000000000000000, -174.0312500020484094 ) ) ;
#17437 = CARTESIAN_POINT ( 'NONE',  ( 9.999999999999998224, 0.000000000000000000, -58.99999999999997158 ) ) ;
#17438 = CARTESIAN_POINT ( 'NONE',  ( 5.405949406249992428, -9.363379034771808662, -123.0937500020483952 ) ) ;
#17439 = CARTESIAN_POINT ( 'NONE',  ( 10.81189881249999729, 0.000000000000000000, -92.84375000204838102 ) ) ;
#17440 = CARTESIAN_POINT ( 'NONE',  ( 7.070501591499376803E-16, 11.54700538379251284, -106.6249999999999858 ) ) ;
#17441 = CARTESIAN_POINT ( 'NONE',  ( 10.81189881249999729, 0.000000000000000000, -103.5312500020483810 ) ) ;
#17442 = CARTESIAN_POINT ( 'NONE',  ( 9.999999999999998224, 0.000000000000000000, -183.8750000040967905 ) ) ;
#17443 = CARTESIAN_POINT ( 'NONE',  ( 10.81189881249999729, 6.242252689847867408, -109.2187500020483810 ) ) ;
#17444 = CARTESIAN_POINT ( 'NONE',  ( -10.81189881249999729, 1.324075727343319199E-15, -182.2812500020483810 ) ) ;
#17445 = CARTESIAN_POINT ( 'NONE',  ( -9.999999999999227285, -5.773502691896698735, -107.6249999999999574 ) ) ;
#17446 = CARTESIAN_POINT ( 'NONE',  ( -9.999999999999998224, 1.224646799147353059E-15, -153.1250000040967905 ) ) ;
#17447 = CARTESIAN_POINT ( 'NONE',  ( 10.81189881249999729, 0.000000000000000000, -195.0312500020484094 ) ) ;
#17448 = CARTESIAN_POINT ( 'NONE',  ( 10.81189881249999729, 6.242252689847867408, -50.71875000204835970 ) ) ;
#17449 = CARTESIAN_POINT ( 'NONE',  ( -10.81189881249999729, 6.242252689847871849, -44.21875000204836681 ) ) ;
#17450 = CARTESIAN_POINT ( 'NONE',  ( -4.999999999999996447, 8.660254037844387298, -168.3750000040967905 ) ) ;
#17451 = CARTESIAN_POINT ( 'NONE',  ( -5.405949406249996869, 9.363379034771805109, -10.03125000204835260 ) ) ;
#17452 = CARTESIAN_POINT ( 'NONE',  ( -10.81189881249999907, -6.242252689847864744, -24.46875000204837036 ) ) ;
#17453 = DIRECTION ( 'NONE',  ( -0.000000000000000000, -0.000000000000000000, -1.000000000000000000 ) ) ;
#17454 = CARTESIAN_POINT ( 'NONE',  ( -5.405949406249996869, 9.363379034771805109, -129.8437500020484094 ) ) ;
#17455 = CARTESIAN_POINT ( 'NONE',  ( -2.121150477449813534E-15, -11.54700538379251284, -98.37500000000000000 ) ) ;
#17456 = CARTESIAN_POINT ( 'NONE',  ( 10.81189881249999551, -6.242252689847874514, -27.15625000204838102 ) ) ;
#17457 = CARTESIAN_POINT ( 'NONE',  ( 7.070501591499377789E-16, 11.54700538379251284, -111.5000000040967763 ) ) ;
#17458 = CARTESIAN_POINT ( 'NONE',  ( 9.999999999999742428, 5.773502691896404748, -158.2500000040967905 ) ) ;
#17459 = CARTESIAN_POINT ( 'NONE',  ( 5.000000000000000000, 8.660254037844385522, -61.74999999999997158 ) ) ;
#17460 = CARTESIAN_POINT ( 'NONE',  ( -10.81189881249999907, -6.242252689847864744, -126.6562500020483810 ) ) ;
#17461 = CARTESIAN_POINT ( 'NONE',  ( -5.405949406250003975, -9.363379034771801557, -107.0312500020483810 ) ) ;
#17462 = VERTEX_POINT ( 'NONE', #2477 ) ;
#17463 = CARTESIAN_POINT ( 'NONE',  ( 9.999999999998456346, 5.773502691897149042, -8.250000004096712303 ) ) ;
#17464 = CARTESIAN_POINT ( 'NONE',  ( -2.121150477449813534E-15, -11.54700538379251284, -101.7500000040967763 ) ) ;
#17465 = CARTESIAN_POINT ( 'NONE',  ( 9.999999999999994671, -5.773502691896262640, -166.0000000040967905 ) ) ;
#17466 = CARTESIAN_POINT ( 'NONE',  ( 7.644554776091147741E-16, 12.48450537969573659, -59.46875000204837391 ) ) ;
#17467 = ORIENTED_EDGE ( 'NONE', *, *, #32342, .T. ) ;
#17468 = CARTESIAN_POINT ( 'NONE',  ( -9.999999999999998224, 5.773502691896259087, -28.37499999999997158 ) ) ;
#17469 = EDGE_CURVE ( 'NONE', #32539, #13704, #21240, .T. ) ;
#17470 = CARTESIAN_POINT ( 'NONE',  ( -10.81189881249999729, 6.242252689847871849, -32.40625000204835970 ) ) ;
#17471 = CARTESIAN_POINT ( 'NONE',  ( -4.999999999999996447, 8.660254037844387298, -159.0000000000000000 ) ) ;
#17472 = ADVANCED_FACE ( 'NONE', ( #28594 ), #29221, .T. ) ;
#17473 = CARTESIAN_POINT ( 'NONE',  ( 9.999999999999998224, 0.000000000000000000, -161.0000000000000000 ) ) ;
#17474 = CARTESIAN_POINT ( 'NONE',  ( 10.00000000000000000, 5.773502691896255534, -30.75000000409674783 ) ) ;
#17475 = EDGE_CURVE ( 'NONE', #14562, #10196, #22893, .T. ) ;
#17476 = EDGE_CURVE ( 'NONE', #21320, #1841, #24290, .T. ) ;
#17477 = CARTESIAN_POINT ( 'NONE',  ( 7.644554776091147741E-16, 12.48450537969573659, -136.1562500020483810 ) ) ;
#17478 = CC_DESIGN_PERSON_AND_ORGANIZATION_ASSIGNMENT ( #39627, #10066, ( #27695 ) ) ;
#17479 = FACE_OUTER_BOUND ( 'NONE', #4324, .T. ) ;
#17480 = VERTEX_POINT ( 'NONE', #40188 ) ;
#17482 = EDGE_LOOP ( 'NONE', ( #29831, #10797, #40102, #23183 ) ) ;
#17481 = ORIENTED_EDGE ( 'NONE', *, *, #35143, .T. ) ;
#17483 = EDGE_CURVE ( 'NONE', #41727, #35978, #30078, .T. ) ;
#17484 = CYLINDRICAL_SURFACE ( 'NONE', #32794, 9.999999999999998224 ) ;
#17485 = CARTESIAN_POINT ( 'NONE',  ( -9.999999999999998224, 1.224646799147353059E-15, -134.7499999999999716 ) ) ;
#17486 = CARTESIAN_POINT ( 'NONE',  ( 5.405949406249992428, -9.363379034771808662, -163.5937500020484094 ) ) ;
#17487 = EDGE_CURVE ( 'NONE', #16776, #20876, #27296, .T. ) ;
#17488 = CARTESIAN_POINT ( 'NONE',  ( 7.644554776091147741E-16, 12.48450537969573659, -194.6562500020484094 ) ) ;
#17489 = CARTESIAN_POINT ( 'NONE',  ( 5.405949406249999534, 9.363379034771803333, -17.59375000204835260 ) ) ;
#17490 = EDGE_CURVE ( 'NONE', #26632, #18779, #33530, .T. ) ;
#17491 = CARTESIAN_POINT ( 'NONE',  ( -10.81189881249999729, 1.324075727343319199E-15, -150.5937500020483810 ) ) ;
#17492 = CARTESIAN_POINT ( 'NONE',  ( -5.405949406249996869, 9.363379034771805109, -135.8437500020484094 ) ) ;
#17493 = CARTESIAN_POINT ( 'NONE',  ( -2.293366432827344421E-15, -12.48450537969573659, -108.4062500020483810 ) ) ;
#17494 = CARTESIAN_POINT ( 'NONE',  ( 5.405949406249992428, -9.363379034771808662, -120.0937500020483952 ) ) ;
#17495 = CARTESIAN_POINT ( 'NONE',  ( -5.405949406250003975, -9.363379034771801557, -0.3437500020483652552 ) ) ;
#17496 = CARTESIAN_POINT ( 'NONE',  ( 5.405949406249999534, 9.363379034771803333, -124.2812500020483952 ) ) ;
#17497 = CARTESIAN_POINT ( 'NONE',  ( 5.405949406249999534, 9.363379034771803333, -13.09375000204834905 ) ) ;
#17498 = CARTESIAN_POINT ( 'NONE',  ( -2.293366432827344421E-15, -12.48450537969573659, -127.7187500020483952 ) ) ;
#17499 = CARTESIAN_POINT ( 'NONE',  ( 5.000000000000000000, 8.660254037844385522, -125.1250000040967620 ) ) ;
#17500 = CARTESIAN_POINT ( 'NONE',  ( 10.00000000000000000, 5.773502691896255534, -151.8750000000000000 ) ) ;
#17501 = CARTESIAN_POINT ( 'NONE',  ( 10.00000000000000000, 5.773502691896255534, -19.87499999999997513 ) ) ;
#17502 = CARTESIAN_POINT ( 'NONE',  ( -10.81189881249999729, 1.324075727343319199E-15, -78.59375000204838102 ) ) ;
#17503 = CARTESIAN_POINT ( 'NONE',  ( 10.81189881249999729, 0.000000000000000000, -67.34375000204836681 ) ) ;
#17504 = CARTESIAN_POINT ( 'NONE',  ( -5.000000000000003553, -8.660254037844383745, -167.5000000000000000 ) ) ;
#17505 = CARTESIAN_POINT ( 'NONE',  ( 5.405949406249992428, -9.363379034771808662, -34.78125000204837391 ) ) ;
#17506 = CARTESIAN_POINT ( 'NONE',  ( 10.81189881249999551, -6.242252689847874514, -46.46875000204836681 ) ) ;
#17507 = CARTESIAN_POINT ( 'NONE',  ( 9.999999999999998224, 0.000000000000000000, -200.0000000000000000 ) ) ;
#17508 = CARTESIAN_POINT ( 'NONE',  ( 5.405949406249999534, 9.363379034771803333, -151.0937500020483810 ) ) ;
#17509 = CARTESIAN_POINT ( 'NONE',  ( -9.999999999999998224, 1.224646799147353059E-15, -118.2500000000000000 ) ) ;
#17510 = CARTESIAN_POINT ( 'NONE',  ( -10.81189881249999729, 6.242252689847871849, -132.9062500020483810 ) ) ;
#17511 = EDGE_CURVE ( 'NONE', #24195, #33229, #36960, .T. ) ;
#17512 = CARTESIAN_POINT ( 'NONE',  ( 5.132169924948443374, 9.089318513147352618, -179.9999999999999432 ) ) ;
#17513 = CARTESIAN_POINT ( 'NONE',  ( -10.00000000000000000, -5.773502691896251982, -86.62499999999997158 ) ) ;
#17514 = CARTESIAN_POINT ( 'NONE',  ( -10.81189881249999729, 6.242252689847871849, -20.40625000204838102 ) ) ;
#17515 = ORIENTED_EDGE ( 'NONE', *, *, #11748, .F. ) ;
#17516 = CARTESIAN_POINT ( 'NONE',  ( -9.999999999999998224, 1.224646799147353059E-15, -164.7500000000000000 ) ) ;
#17517 = CARTESIAN_POINT ( 'NONE',  ( 7.070501591499377789E-16, 11.54700538379251284, -123.5000000040967905 ) ) ;
#17518 = CARTESIAN_POINT ( 'NONE',  ( 4.999999999999992006, -8.660254037844389075, -34.12500000409676915 ) ) ;
#17519 = CARTESIAN_POINT ( 'NONE',  ( 9.999999999999998224, 0.000000000000000000, -98.37500000409677625 ) ) ;
#17520 = CARTESIAN_POINT ( 'NONE',  ( 10.81189881249999551, -6.242252689847874514, -51.15625000204837391 ) ) ;
#17521 = CYLINDRICAL_SURFACE ( 'NONE', #7636, 9.999999999999998224 ) ;
#17522 = CARTESIAN_POINT ( 'NONE',  ( -10.81189881249999729, 1.324075727343319199E-15, -156.7812500020484094 ) ) ;
#17523 = CARTESIAN_POINT ( 'NONE',  ( 10.81189881249999551, -6.242252689847874514, -125.9687500020483810 ) ) ;
#17524 = CARTESIAN_POINT ( 'NONE',  ( 9.999999999999998224, 0.000000000000000000, -200.0000000000000000 ) ) ;
#17525 = ORIENTED_EDGE ( 'NONE', *, *, #15901, .F. ) ;
#17526 = CARTESIAN_POINT ( 'NONE',  ( 9.999999999998969713, 5.773502691896851502, -31.87499999999993960 ) ) ;
#17527 = VERTEX_POINT ( 'NONE', #30290 ) ;
#17528 = ORIENTED_EDGE ( 'NONE', *, *, #9990, .T. ) ;
#17530 = ORIENTED_EDGE ( 'NONE', *, *, #9304, .F. ) ;
#17529 = CARTESIAN_POINT ( 'NONE',  ( -10.81189881249999729, 1.324075727343319199E-15, -110.0937500020483810 ) ) ;
#17531 = CARTESIAN_POINT ( 'NONE',  ( 9.999999999998969713, 5.773502691896851502, -103.8750000000000000 ) ) ;
#17532 = CARTESIAN_POINT ( 'NONE',  ( 5.405949406249999534, 9.363379034771803333, -193.0937500020484094 ) ) ;
#17533 = CARTESIAN_POINT ( 'NONE',  ( 10.81189881249999907, 6.242252689847868297, -40.21875000204835970 ) ) ;
#17534 = CARTESIAN_POINT ( 'NONE',  ( -8.239685287916026724, -5.747359526181299749, -1.202135122527665920E-14 ) ) ;
#17535 = CARTESIAN_POINT ( 'NONE',  ( 4.999999999999992006, -8.660254037844389075, -10.12500000409674605 ) ) ;
#17536 = CARTESIAN_POINT ( 'NONE',  ( 10.81189881249999729, 6.242252689847867408, -173.7187500020483810 ) ) ;
#17537 = CARTESIAN_POINT ( 'NONE',  ( -2.293366432827344421E-15, -12.48450537969573659, -157.7187500020484094 ) ) ;
#17538 = CARTESIAN_POINT ( 'NONE',  ( -2.121150477449813534E-15, -11.54700538379251284, -65.75000000409677625 ) ) ;
#17539 = CARTESIAN_POINT ( 'NONE',  ( -10.81189881249999907, -6.242252689847864744, -144.4687500020484094 ) ) ;
#17540 =( BOUNDED_CURVE ( )  B_SPLINE_CURVE ( 2, ( #215, #30199, #26941, #635, #7520, #40098, #20458 ),
 .UNSPECIFIED., .F., .F. ) 
 B_SPLINE_CURVE_WITH_KNOTS ( ( 3, 2, 2, 3 ),
 ( 0.3805970149253732338, 0.3818407960199006190, 0.3830845771144278933, 0.3843283582089552786 ),
 .UNSPECIFIED. ) 
 CURVE ( )  GEOMETRIC_REPRESENTATION_ITEM ( )  RATIONAL_B_SPLINE_CURVE ( ( 0.9999999999999880096, 0.8660254037844506980, 1.000000000000000000, 0.8660254037844387076, 1.000000000000000000, 0.8660254037844327124, 1.000000000000005995 ) ) 
 REPRESENTATION_ITEM ( '' )  );
#17541 = CARTESIAN_POINT ( 'NONE',  ( 7.644554776091147741E-16, 12.48450537969573659, -155.4687500020484094 ) ) ;
#17542 = CARTESIAN_POINT ( 'NONE',  ( -10.00000000000102496, 5.773502691895664007, -35.87499999999993605 ) ) ;
#17543 = CARTESIAN_POINT ( 'NONE',  ( -4.999999999999996447, 8.660254037844387298, -178.5000000000000000 ) ) ;
#17544 = CARTESIAN_POINT ( 'NONE',  ( 10.81189881249999551, -6.242252689847874514, -91.46875000204838102 ) ) ;
#17545 = FACE_OUTER_BOUND ( 'NONE', #10631, .T. ) ;
#17546 = CARTESIAN_POINT ( 'NONE',  ( 7.644554776091147741E-16, 12.48450537969573659, -55.15625000204837391 ) ) ;
#17547 = CARTESIAN_POINT ( 'NONE',  ( -10.00000000000102496, 5.773502691895664007, -87.25000000409674783 ) ) ;
#17548 = CARTESIAN_POINT ( 'NONE',  ( 5.405949406249999534, 9.363379034771803333, -175.0937500020484094 ) ) ;
#17549 = CARTESIAN_POINT ( 'NONE',  ( 7.644554776091147741E-16, 12.48450537969573659, -122.6562500020483952 ) ) ;
#17550 = CARTESIAN_POINT ( 'NONE',  ( 5.405949406249992428, -9.363379034771808662, -157.7812500020484094 ) ) ;
#17551 = CARTESIAN_POINT ( 'NONE',  ( 0.000000000000000000, 0.000000000000000000, -203.0000000000000000 ) ) ;
#17552 = CARTESIAN_POINT ( 'NONE',  ( 5.405949406249999534, 9.363379034771803333, -55.28125000204836681 ) ) ;
#17553 = CARTESIAN_POINT ( 'NONE',  ( 4.999999999999992006, -8.660254037844389075, -128.6250000040967620 ) ) ;
#17554 = CARTESIAN_POINT ( 'NONE',  ( 10.00000000000000000, 5.773502691896255534, -103.8750000000000000 ) ) ;
#17555 = EDGE_LOOP ( 'NONE', ( #33918, #24425, #2587, #20764 ) ) ;
#17556 = AXIS2_PLACEMENT_3D ( 'NONE', #14970, #14756, #18435 ) ;
#17557 = CARTESIAN_POINT ( 'NONE',  ( -2.293366432827344421E-15, -12.48450537969573659, -136.9062500020484094 ) ) ;
#17558 = CARTESIAN_POINT ( 'NONE',  ( 7.070501591499377789E-16, 11.54700538379251284, -147.5000000040968189 ) ) ;
#17559 = CARTESIAN_POINT ( 'NONE',  ( 5.405949406249999534, 9.363379034771803333, -151.2812500020484094 ) ) ;
#17560 = CARTESIAN_POINT ( 'NONE',  ( 10.81189881249999907, 6.242252689847868297, -188.9062500020484379 ) ) ;
#17561 = VERTEX_POINT ( 'NONE', #23602 ) ;
#17562 = CARTESIAN_POINT ( 'NONE',  ( -2.121150477449813534E-15, -11.54700538379251284, -48.87499999999997868 ) ) ;
#17563 = CARTESIAN_POINT ( 'NONE',  ( 5.405949406249999534, 9.363379034771803333, -182.5937500020483810 ) ) ;
#17564 = CARTESIAN_POINT ( 'NONE',  ( 9.999999999999998224, 0.000000000000000000, -54.87500000409675494 ) ) ;
#17565 = CYLINDRICAL_SURFACE ( 'NONE', #31372, 9.999999999999998224 ) ;
#17566 = CARTESIAN_POINT ( 'NONE',  ( 9.999999999999998224, 0.000000000000000000, -179.3750000040967905 ) ) ;
#17567 = CARTESIAN_POINT ( 'NONE',  ( 10.81189881249999729, 0.000000000000000000, -75.03125000204838102 ) ) ;
#17568 = CARTESIAN_POINT ( 'NONE',  ( 5.405949406249999534, 9.363379034771803333, -50.78125000204835970 ) ) ;
#17569 = CARTESIAN_POINT ( 'NONE',  ( 4.999999999999992006, -8.660254037844389075, -53.62500000409675494 ) ) ;
#17570 = CARTESIAN_POINT ( 'NONE',  ( 7.644554776091147741E-16, 12.48450537969573659, -11.46875000204836148 ) ) ;
#17571 = CARTESIAN_POINT ( 'NONE',  ( -9.999999999999998224, 1.224646799147353059E-15, -35.74999999999997868 ) ) ;
#17572 = CARTESIAN_POINT ( 'NONE',  ( 10.81189881249999907, 6.242252689847868297, -175.4062500020484094 ) ) ;
#17573 = CARTESIAN_POINT ( 'NONE',  ( -2.293366432827344421E-15, -12.48450537969573659, -3.406250002048361036 ) ) ;
#17574 = CYLINDRICAL_SURFACE ( 'NONE', #32554, 9.999999999999998224 ) ;
#17575 = CARTESIAN_POINT ( 'NONE',  ( 0.000000000000000000, 0.000000000000000000, -200.0000000000000000 ) ) ;
#17576 = LINE ( 'NONE', #27746, #6313 ) ;
#17577 = CARTESIAN_POINT ( 'NONE',  ( 9.999999999999998224, 1.224646799147353059E-15, -99.99999999999998579 ) ) ;
#17578 = VECTOR ( 'NONE', #9523, 1000.000000000000000 ) ;
#17579 = CARTESIAN_POINT ( 'NONE',  ( 9.999999999999998224, 0.000000000000000000, -186.8750000040967905 ) ) ;
#17580 = EDGE_CURVE ( 'NONE', #19560, #22477, #40258, .T. ) ;
#17582 = VERTEX_POINT ( 'NONE', #729 ) ;
#17581 = CARTESIAN_POINT ( 'NONE',  ( 7.644554776091147741E-16, 12.48450537969573659, -83.65625000204838102 ) ) ;
#17584 = ORIENTED_EDGE ( 'NONE', *, *, #23366, .T. ) ;
#17583 = CARTESIAN_POINT ( 'NONE',  ( -9.999999999999998224, 1.224646799147353059E-15, -80.74999999999998579 ) ) ;
#17585 = AXIS2_PLACEMENT_3D ( 'NONE', #28290, #31537, #2181 ) ;
#17586 = ORIENTED_EDGE ( 'NONE', *, *, #29989, .T. ) ;
#17587 = CARTESIAN_POINT ( 'NONE',  ( 7.644554776091147741E-16, 12.48450537969573659, -38.46875000204835970 ) ) ;
#17588 = CARTESIAN_POINT ( 'NONE',  ( 7.644554776091147741E-16, 12.48450537969573659, -24.96875000204837036 ) ) ;
#17589 = CARTESIAN_POINT ( 'NONE',  ( 5.405949406249992428, -9.363379034771808662, -15.28125000204835793 ) ) ;
#17590 = CARTESIAN_POINT ( 'NONE',  ( 7.644554776091147741E-16, 12.48450537969573659, -65.46875000204836681 ) ) ;
#17591 = CARTESIAN_POINT ( 'NONE',  ( -5.000000000000003553, -8.660254037844383745, -131.5000000000000000 ) ) ;
#17592 = CARTESIAN_POINT ( 'NONE',  ( -5.000000000000003553, -8.660254037844383745, -41.49999999999997868 ) ) ;
#17593 = CARTESIAN_POINT ( 'NONE',  ( 10.81189881249999551, -6.242252689847874514, -181.4687500020484094 ) ) ;
#17594 = CARTESIAN_POINT ( 'NONE',  ( -2.293366432827344421E-15, -12.48450537969573659, -169.7187500020483810 ) ) ;
#17595 = EDGE_CURVE ( 'NONE', #25998, #18722, #39554, .T. ) ;
#17596 = CARTESIAN_POINT ( 'NONE',  ( 10.81189881249999729, 6.242252689847867408, -179.7187500020484094 ) ) ;
#17597 = CARTESIAN_POINT ( 'NONE',  ( -9.999999999999998224, 1.224646799147353059E-15, -199.2500000000000000 ) ) ;
#17598 = FACE_OUTER_BOUND ( 'NONE', #8058, .T. ) ;
#17599 = CARTESIAN_POINT ( 'NONE',  ( 5.000000000000000000, 8.660254037844385522, 0.8749999959032361829 ) ) ;
#17600 = DIRECTION ( 'NONE',  ( 0.000000000000000000, 0.000000000000000000, -1.000000000000000000 ) ) ;
#17601 = CARTESIAN_POINT ( 'NONE',  ( -5.405949406250003975, -9.363379034771801557, -109.8437500020483810 ) ) ;
#17602 = DIRECTION ( 'NONE',  ( -0.000000000000000000, -0.000000000000000000, -1.000000000000000000 ) ) ;
#17603 = CARTESIAN_POINT ( 'NONE',  ( 5.405949406249999534, 9.363379034771803333, -92.78125000204838102 ) ) ;
#17604 = CARTESIAN_POINT ( 'NONE',  ( -5.405949406249996869, 9.363379034771805109, -101.3437500020483810 ) ) ;
#17605 = CARTESIAN_POINT ( 'NONE',  ( 5.405949406249999534, 9.363379034771803333, -70.09375000204836681 ) ) ;
#17606 = CARTESIAN_POINT ( 'NONE',  ( 10.81189881249999551, -6.242252689847874514, -75.15625000204838102 ) ) ;
#17607 = CARTESIAN_POINT ( 'NONE',  ( 7.070501591499377789E-16, 11.54700538379251284, -156.5000000040968189 ) ) ;
#17608 = CARTESIAN_POINT ( 'NONE',  ( -2.121150477449813534E-15, -11.54700538379251284, -132.8750000000000000 ) ) ;
#17609 = AXIS2_PLACEMENT_3D ( 'NONE', #13491, #6412, #16943 ) ;
#17610 = CARTESIAN_POINT ( 'NONE',  ( -5.405949406250003975, -9.363379034771801557, -155.0312500020484094 ) ) ;
#17611 = CARTESIAN_POINT ( 'NONE',  ( 10.81189881249999907, 6.242252689847868297, -172.4062500020484094 ) ) ;
#17612 = CARTESIAN_POINT ( 'NONE',  ( -9.999999999999998224, 1.224646799147353059E-15, -153.1250000040967905 ) ) ;
#17613 = CARTESIAN_POINT ( 'NONE',  ( -2.121150477449813534E-15, -11.54700538379251284, -197.3750000000000000 ) ) ;
#17614 = CARTESIAN_POINT ( 'NONE',  ( -2.293366432827344421E-15, -12.48450537969573659, -109.7187500020483668 ) ) ;
#17615 = CARTESIAN_POINT ( 'NONE',  ( -9.999999999999998224, 1.224646799147353059E-15, -130.6250000040967620 ) ) ;
#17616 = CARTESIAN_POINT ( 'NONE',  ( -2.121150477449813534E-15, -11.54700538379251284, -75.87500000000000000 ) ) ;
#17617 = CARTESIAN_POINT ( 'NONE',  ( -2.293366432827344421E-15, -12.48450537969573659, -1.906250002048359704 ) ) ;
#17618 = CARTESIAN_POINT ( 'NONE',  ( 9.999999999999998224, 0.000000000000000000, -81.87500000409676204 ) ) ;
#17619 = AXIS2_PLACEMENT_3D ( 'NONE', #12299, #32184, #2819 ) ;
#17620 = CARTESIAN_POINT ( 'NONE',  ( 7.070501591499376803E-16, 11.54700538379251284, -115.6249999999999858 ) ) ;
#17621 = CARTESIAN_POINT ( 'NONE',  ( 7.644554776091147741E-16, 12.48450537969573659, -97.15625000204839523 ) ) ;
#17622 = CARTESIAN_POINT ( 'NONE',  ( -10.81189881249999729, -6.242252689847864744, -87.65625000204836681 ) ) ;
#17623 = CARTESIAN_POINT ( 'NONE',  ( 4.999999999999992006, -8.660254037844389075, -76.12500000409677625 ) ) ;
#17624 = CARTESIAN_POINT ( 'NONE',  ( 9.999999999999998224, 0.000000000000000000, -58.99999999999997158 ) ) ;
#17625 = CARTESIAN_POINT ( 'NONE',  ( 10.81189881249999551, -6.242252689847874514, -31.46875000204835260 ) ) ;
#17626 = EDGE_LOOP ( 'NONE', ( #15300, #4125, #34022, #25590 ) ) ;
#17627 = CARTESIAN_POINT ( 'NONE',  ( -4.999999999999996447, 8.660254037844387298, -2.999999999999975131 ) ) ;
#17628 = CARTESIAN_POINT ( 'NONE',  ( -5.405949406249996869, 9.363379034771805109, -26.53125000204836681 ) ) ;
#17629 = CARTESIAN_POINT ( 'NONE',  ( -5.405949406249996869, 9.363379034771805109, -17.34375000204835260 ) ) ;
#17630 = CARTESIAN_POINT ( 'NONE',  ( -2.121150477449813534E-15, -11.54700538379251284, -176.7500000040967620 ) ) ;
#17631 = CARTESIAN_POINT ( 'NONE',  ( -2.121150477449813534E-15, -11.54700538379251284, -7.250000004096756712 ) ) ;
#17632 = CARTESIAN_POINT ( 'NONE',  ( -5.405949406250003975, -9.363379034771801557, -132.5312500020484094 ) ) ;
#17633 = EDGE_CURVE ( 'NONE', #37834, #14232, #25675, .T. ) ;
#17634 = CARTESIAN_POINT ( 'NONE',  ( -10.00000000000000000, -5.773502691896251982, -184.1250000000000284 ) ) ;
#17635 = CARTESIAN_POINT ( 'NONE',  ( 5.000000000000000000, 8.660254037844385522, -120.2500000000000000 ) ) ;
#17637 = EDGE_LOOP ( 'NONE', ( #15736, #11653, #39150, #18295 ) ) ;
#17636 = CARTESIAN_POINT ( 'NONE',  ( 10.81189881249999551, -6.242252689847874514, -111.1562500020483952 ) ) ;
#17638 = CARTESIAN_POINT ( 'NONE',  ( -10.00000000000076916, 5.773502691895813221, -138.2500000040967905 ) ) ;
#17639 = VERTEX_POINT ( 'NONE', #26616 ) ;
#17640 =( BOUNDED_CURVE ( )  B_SPLINE_CURVE ( 2, ( #7574, #23561, #4759, #30469, #13809, #11225, #27208 ),
 .UNSPECIFIED., .F., .F. ) 
 B_SPLINE_CURVE_WITH_KNOTS ( ( 3, 2, 2, 3 ),
 ( 0.3917910447761194792, 0.3930348258706468090, 0.3942786069651742498, 0.3955223880597015795 ),
 .UNSPECIFIED. ) 
 CURVE ( )  GEOMETRIC_REPRESENTATION_ITEM ( )  RATIONAL_B_SPLINE_CURVE ( ( 0.9999999999999940048, 0.8660254037844447028, 1.000000000000000000, 0.8660254037844387076, 1.000000000000000000, 0.8660254037844267172, 1.000000000000011990 ) ) 
 REPRESENTATION_ITEM ( '' )  );
#17641 = VERTEX_POINT ( 'NONE', #24026 ) ;
#17642 = CARTESIAN_POINT ( 'NONE',  ( 5.405949406249999534, 9.363379034771803333, -40.28125000204838102 ) ) ;
#17643 = COORDINATED_UNIVERSAL_TIME_OFFSET ( 6, 0, .AHEAD. ) ;
#17644 = CARTESIAN_POINT ( 'NONE',  ( 7.644554776091147741E-16, 12.48450537969573659, -86.46875000204838102 ) ) ;
#17645 = FACE_OUTER_BOUND ( 'NONE', #41963, .T. ) ;
#17646 = CARTESIAN_POINT ( 'NONE',  ( 9.999999999999998224, 0.000000000000000000, -32.37500000409676204 ) ) ;
#17647 = CARTESIAN_POINT ( 'NONE',  ( -5.405949406249996869, 9.363379034771805109, -176.5312500020483810 ) ) ;
#17648 = ADVANCED_FACE ( 'NONE', ( #37166 ), #32885, .F. ) ;
#17649 = CARTESIAN_POINT ( 'NONE',  ( -5.405949406249996869, 9.363379034771805109, -125.3437500020483952 ) ) ;
#17650 = CARTESIAN_POINT ( 'NONE',  ( -10.81189881249999729, 6.242252689847871849, -93.71875000204838102 ) ) ;
#17651 = CARTESIAN_POINT ( 'NONE',  ( 10.81189881249999729, 0.7537365248293982356, -0.01615656218219799906 ) ) ;
#17652 = CARTESIAN_POINT ( 'NONE',  ( -10.00000000000051337, 5.773502691895962435, -112.7500000040967620 ) ) ;
#17653 = CARTESIAN_POINT ( 'NONE',  ( -10.81189881249999907, -6.242252689847864744, -102.6562500020483952 ) ) ;
#17654 = CARTESIAN_POINT ( 'NONE',  ( 9.999999999999996447, -5.773502691896262640, -176.5000000040968189 ) ) ;
#17655 = CARTESIAN_POINT ( 'NONE',  ( 10.81189881249999729, 0.000000000000000000, -104.8437500020483810 ) ) ;
#17656 = CARTESIAN_POINT ( 'NONE',  ( 10.81189881249999729, 6.242252689847867408, -181.4062500020484379 ) ) ;
#17657 = LINE ( 'NONE', #1289, #17859 ) ;
#17658 = CARTESIAN_POINT ( 'NONE',  ( 9.999999999999479527, 5.773502691896553074, -122.2500000040967763 ) ) ;
#17659 = CARTESIAN_POINT ( 'NONE',  ( 5.405949406249999534, 9.363379034771803333, -194.7812500020484094 ) ) ;
#17660 = CARTESIAN_POINT ( 'NONE',  ( 5.405949406249999534, 9.363379034771803333, -53.59375000204835970 ) ) ;
#17661 = CARTESIAN_POINT ( 'NONE',  ( -10.81189881249999729, 1.324075727343319199E-15, -41.09375000204837391 ) ) ;
#17662 = CARTESIAN_POINT ( 'NONE',  ( 10.00000000000000000, 5.773502691896255534, -174.7500000040968189 ) ) ;
#17663 = CARTESIAN_POINT ( 'NONE',  ( 10.81189881249999551, -6.242252689847874514, -10.65625000204838280 ) ) ;
#17664 = CARTESIAN_POINT ( 'NONE',  ( 10.81189881249999729, 0.000000000000000000, -20.84375000204835615 ) ) ;
#17665 = LINE ( 'NONE', #31727, #8203 ) ;
#17666 = CARTESIAN_POINT ( 'NONE',  ( 10.81189881249999729, 0.000000000000000000, -127.3437500020483952 ) ) ;
#17667 = CARTESIAN_POINT ( 'NONE',  ( 9.999999999999998224, 0.000000000000000000, -96.49999999999998579 ) ) ;
#17668 = CARTESIAN_POINT ( 'NONE',  ( 10.81189881249999551, -6.242252689847874514, -31.65625000204835615 ) ) ;
#17669 = CARTESIAN_POINT ( 'NONE',  ( -2.121150477449813534E-15, -11.54700538379251284, -104.7500000040967763 ) ) ;
#17670 = CARTESIAN_POINT ( 'NONE',  ( -9.999999999999998224, 1.224646799147353059E-15, -61.24999999999997158 ) ) ;
#17671 = CARTESIAN_POINT ( 'NONE',  ( -10.81189881249999729, 6.242252689847871849, -123.9062500020483952 ) ) ;
#17672 = CARTESIAN_POINT ( 'NONE',  ( 5.405949406249999534, 9.363379034771803333, -107.7812500020483810 ) ) ;
#17673 = ORIENTED_EDGE ( 'NONE', *, *, #34120, .F. ) ;
#17674 = FACE_OUTER_BOUND ( 'NONE', #10746, .T. ) ;
#17675 = CARTESIAN_POINT ( 'NONE',  ( 9.999999999999998224, 0.000000000000000000, -98.37500000409677625 ) ) ;
#17676 = CARTESIAN_POINT ( 'NONE',  ( 0.000000000000000000, 0.000000000000000000, -99.99999999999998579 ) ) ;
#17677 = CARTESIAN_POINT ( 'NONE',  ( -10.81189881249999729, 6.242252689847871849, -165.9062500020483810 ) ) ;
#17678 = CARTESIAN_POINT ( 'NONE',  ( -10.81189881249999907, -6.242252689847864744, -58.96875000204838102 ) ) ;
#17679 = VERTEX_POINT ( 'NONE', #13210 ) ;
#17680 = CARTESIAN_POINT ( 'NONE',  ( -5.000000000000003553, -8.660254037844383745, -27.99999999999996803 ) ) ;
#17681 = CARTESIAN_POINT ( 'NONE',  ( -10.81189881249999729, 1.324075727343319199E-15, -38.28125000204838102 ) ) ;
#17682 = CARTESIAN_POINT ( 'NONE',  ( -4.999999999999996447, 8.660254037844387298, -165.0000000000000000 ) ) ;
#17683 = CYLINDRICAL_SURFACE ( 'NONE', #22863, 9.999999999999998224 ) ;
#17684 = CARTESIAN_POINT ( 'NONE',  ( 9.999999999999996447, -5.773502691896262640, -31.00000000409675138 ) ) ;
#17685 =( BOUNDED_CURVE ( )  B_SPLINE_CURVE ( 2, ( #34514, #31487, #1921, #23942, #12034, #39007, #38162 ),
 .UNSPECIFIED., .F., .F. ) 
 B_SPLINE_CURVE_WITH_KNOTS ( ( 3, 2, 2, 3 ),
 ( 0.3507462686567164867, 0.3519900497512438720, 0.3532338308457712572, 0.3544776119402986980 ),
 .UNSPECIFIED. ) 
 CURVE ( )  GEOMETRIC_REPRESENTATION_ITEM ( )  RATIONAL_B_SPLINE_CURVE ( ( 0.9999999999999940048, 0.8660254037844447028, 1.000000000000000000, 0.8660254037844387076, 1.000000000000000000, 0.8660254037844207220, 1.000000000000017986 ) ) 
 REPRESENTATION_ITEM ( '' )  );
#17686 = FACE_OUTER_BOUND ( 'NONE', #25520, .T. ) ;
#17687 = CARTESIAN_POINT ( 'NONE',  ( -5.405949406250003975, -9.363379034771801557, -134.0312500020484094 ) ) ;
#17688 = CARTESIAN_POINT ( 'NONE',  ( 9.794892170062176717, 4.319011525664689266, 3.656666817559538189E-15 ) ) ;
#17689 = CARTESIAN_POINT ( 'NONE',  ( -10.00000000000076916, 5.773502691895813221, -129.2500000040967905 ) ) ;
#17690 = VERTEX_POINT ( 'NONE', #33099 ) ;
#17691 =( BOUNDED_CURVE ( )  B_SPLINE_CURVE ( 2, ( #5093, #12185, #28408, #41960, #22130, #38315, #38523 ),
 .UNSPECIFIED., .F., .F. ) 
 B_SPLINE_CURVE_WITH_KNOTS ( ( 3, 2, 2, 3 ),
 ( 0.7276119402985077311, 0.7288557213930350054, 0.7300995024875623907, 0.7313432835820897759 ),
 .UNSPECIFIED. ) 
 CURVE ( )  GEOMETRIC_REPRESENTATION_ITEM ( )  RATIONAL_B_SPLINE_CURVE ( ( 0.9999999999999761302, 0.8660254037844625774, 1.000000000000000000, 0.8660254037844387076, 1.000000000000000000, 0.8660254037844148378, 1.000000000000023981 ) ) 
 REPRESENTATION_ITEM ( '' )  );
#17693 = ORIENTED_EDGE ( 'NONE', *, *, #35673, .T. ) ;
#17692 = EDGE_LOOP ( 'NONE', ( #12484, #3694, #42433, #18601 ) ) ;
#17694 = CARTESIAN_POINT ( 'NONE',  ( -9.999999999999998224, 1.224646799147353059E-15, -123.1250000040967905 ) ) ;
#17695 = CARTESIAN_POINT ( 'NONE',  ( 10.00000000000154010, -5.773502691895370020, -55.00000000409672651 ) ) ;
#17696 = CARTESIAN_POINT ( 'NONE',  ( -2.293366432827344421E-15, -12.48450537969573659, -168.2187500020483810 ) ) ;
#17697 = CARTESIAN_POINT ( 'NONE',  ( -2.293366432827344421E-15, -12.48450537969573659, -195.4062500020484094 ) ) ;
#17698 = CARTESIAN_POINT ( 'NONE',  ( -5.405949406250003975, -9.363379034771801557, -15.34375000204835082 ) ) ;
#17699 = CARTESIAN_POINT ( 'NONE',  ( -5.000000000000003553, -8.660254037844383745, -157.3750000040967905 ) ) ;
#17700 = EDGE_CURVE ( 'NONE', #18552, #14343, #300, .T. ) ;
#17701 = CARTESIAN_POINT ( 'NONE',  ( 5.405949406249992428, -9.363379034771808662, -145.5937500020483810 ) ) ;
#17702 = CARTESIAN_POINT ( 'NONE',  ( -2.293366432827344421E-15, -12.48450537969573659, -138.2187500020483810 ) ) ;
#17703 = ADVANCED_FACE ( 'NONE', ( #23385 ), #36534, .F. ) ;
#17704 = CARTESIAN_POINT ( 'NONE',  ( -5.405949406250003975, -9.363379034771801557, -107.0312500020483810 ) ) ;
#17705 = CARTESIAN_POINT ( 'NONE',  ( 5.405949406249999534, 9.363379034771803333, -115.0937500020483810 ) ) ;
#17706 = CARTESIAN_POINT ( 'NONE',  ( 9.999999999999998224, 0.000000000000000000, -197.3750000040967905 ) ) ;
#17707 = CARTESIAN_POINT ( 'NONE',  ( -5.405949406249996869, 9.363379034771805109, -122.5312500020483952 ) ) ;
#17708 = CARTESIAN_POINT ( 'NONE',  ( -4.999999999999996447, 8.660254037844387298, -198.3750000040967905 ) ) ;
#17709 = CARTESIAN_POINT ( 'NONE',  ( -10.81189881249999729, -6.242252689847864744, -130.9687500020483810 ) ) ;
#17710 = CARTESIAN_POINT ( 'NONE',  ( -5.000000000000003553, -8.660254037844383745, -54.99999999999996447 ) ) ;
#17711 = CARTESIAN_POINT ( 'NONE',  ( -10.00000000000102496, 5.773502691895664007, -4.750000004096740724 ) ) ;
#17712 = CARTESIAN_POINT ( 'NONE',  ( -5.000000000000003553, -8.660254037844383745, -154.0000000000000000 ) ) ;
#17713 = CARTESIAN_POINT ( 'NONE',  ( 5.000000000000000000, 8.660254037844385522, -22.74999999999996447 ) ) ;
#17714 = CARTESIAN_POINT ( 'NONE',  ( 5.405949406249992428, -9.363379034771808662, -76.59375000204838102 ) ) ;
#17715 = CARTESIAN_POINT ( 'NONE',  ( -10.81189881249999729, 1.324075727343319199E-15, -68.09375000204836681 ) ) ;
#17716 = CARTESIAN_POINT ( 'NONE',  ( -9.999999999998456346, -5.773502691897145489, -19.50000000409673717 ) ) ;
#17717 = CARTESIAN_POINT ( 'NONE',  ( -10.81189881249999729, 6.242252689847871849, -32.40625000204835970 ) ) ;
#17718 = CARTESIAN_POINT ( 'NONE',  ( 10.81189881249999907, 6.242252689847868297, -44.71875000204835970 ) ) ;
#17719 = CARTESIAN_POINT ( 'NONE',  ( 0.000000000000000000, 0.000000000000000000, -200.0000000000000000 ) ) ;
#17720 = CARTESIAN_POINT ( 'NONE',  ( -10.81189881249999729, 1.324075727343319199E-15, -153.5937500020483810 ) ) ;
#17721 = CARTESIAN_POINT ( 'NONE',  ( 4.999999999999992006, -8.660254037844389075, -120.7500000000000000 ) ) ;
#17722 = CARTESIAN_POINT ( 'NONE',  ( 10.81189881249999551, -6.242252689847874514, -132.1562500020483810 ) ) ;
#17723 = DIRECTION ( 'NONE',  ( -1.000000000000000000, 0.000000000000000000, 0.000000000000000000 ) ) ;
#17724 = CARTESIAN_POINT ( 'NONE',  ( -10.00000000000000000, -5.773502691896251982, -80.62499999999998579 ) ) ;
#17725 = CARTESIAN_POINT ( 'NONE',  ( 10.81189881249999729, 0.000000000000000000, -19.53125000204835970 ) ) ;
#17726 = ORIENTED_EDGE ( 'NONE', *, *, #2245, .F. ) ;
#17727 = CARTESIAN_POINT ( 'NONE',  ( -2.293366432827344421E-15, -12.48450537969573659, -102.4062500020484094 ) ) ;
#17728 = CARTESIAN_POINT ( 'NONE',  ( -5.000000000000003553, -8.660254037844383745, -125.8750000040967905 ) ) ;
#17729 = CARTESIAN_POINT ( 'NONE',  ( 0.000000000000000000, 0.000000000000000000, -200.0000000000000000 ) ) ;
#17730 = CARTESIAN_POINT ( 'NONE',  ( -2.121150477449813534E-15, -11.54700538379251284, -32.75000000409674783 ) ) ;
#17731 = ADVANCED_FACE ( 'NONE', ( #11691 ), #11262, .T. ) ;
#17732 = DIRECTION ( 'NONE',  ( 0.000000000000000000, -1.000000000000000000, 0.000000000000000000 ) ) ;
#17733 = CARTESIAN_POINT ( 'NONE',  ( 7.644554776091147741E-16, 12.48450537969573659, -47.65625000204837391 ) ) ;
#17734 = CARTESIAN_POINT ( 'NONE',  ( -5.000000000000003553, -8.660254037844383745, -146.5000000000000000 ) ) ;
#17735 = CARTESIAN_POINT ( 'NONE',  ( -2.293366432827344421E-15, -12.48450537969573659, -154.9062500020483810 ) ) ;
#17736 = CARTESIAN_POINT ( 'NONE',  ( -10.81189881249999907, -6.242252689847864744, -126.4687500020483810 ) ) ;
#17737 = CARTESIAN_POINT ( 'NONE',  ( 5.000000000000000000, 8.660254037844385522, -3.625000004096767814 ) ) ;
#17738 = EDGE_CURVE ( 'NONE', #21791, #8991, #30083, .T. ) ;
#17739 = ORIENTED_EDGE ( 'NONE', *, *, #2344, .F. ) ;
#17740 = CARTESIAN_POINT ( 'NONE',  ( 9.999999999999998224, 0.000000000000000000, -22.99999999999996447 ) ) ;
#17741 = VERTEX_POINT ( 'NONE', #24887 ) ;
#17742 = VERTEX_POINT ( 'NONE', #34170 ) ;
#17743 = AXIS2_PLACEMENT_3D ( 'NONE', #4890, #37474, #7701 ) ;
#17745 = ORIENTED_EDGE ( 'NONE', *, *, #11167, .T. ) ;
#17744 = CARTESIAN_POINT ( 'NONE',  ( 10.81189881249999729, 0.000000000000000000, -112.3437500020483810 ) ) ;
#17746 = VECTOR ( 'NONE', #5691, 1000.000000000000000 ) ;
#17747 = CARTESIAN_POINT ( 'NONE',  ( 9.999999999999742428, 5.773502691896404748, -129.7500000040967905 ) ) ;
#17748 = CARTESIAN_POINT ( 'NONE',  ( 5.405949406249992428, -9.363379034771808662, -192.0937500020484094 ) ) ;
#17749 = CARTESIAN_POINT ( 'NONE',  ( 5.405949406249999534, 9.363379034771803333, -38.59375000204837391 ) ) ;
#17750 = DIRECTION ( 'NONE',  ( -0.000000000000000000, -0.000000000000000000, -1.000000000000000000 ) ) ;
#17751 = CARTESIAN_POINT ( 'NONE',  ( -9.999999999999998224, 1.224646799147353059E-15, -74.74999999999998579 ) ) ;
#17752 = EDGE_CURVE ( 'NONE', #26823, #28777, #1979, .T. ) ;
#17753 = CARTESIAN_POINT ( 'NONE',  ( -10.81189881249999729, 6.242252689847871849, -168.7187500020483810 ) ) ;
#17754 = CARTESIAN_POINT ( 'NONE',  ( 7.644554776091147741E-16, 12.48450537969573659, -164.4687500020483810 ) ) ;
#17755 =( BOUNDED_CURVE ( )  B_SPLINE_CURVE ( 2, ( #32367, #9888, #29122, #25879, #26090, #9253, #9679 ),
 .UNSPECIFIED., .F., .F. ) 
 B_SPLINE_CURVE_WITH_KNOTS ( ( 3, 2, 2, 3 ),
 ( 0.1380597014925373234, 0.1393034825870646809, 0.1405472636815920384, 0.1417910447761193959 ),
 .UNSPECIFIED. ) 
 CURVE ( )  GEOMETRIC_REPRESENTATION_ITEM ( )  RATIONAL_B_SPLINE_CURVE ( ( 1.000000000000000000, 0.8660254037844387076, 1.000000000000000000, 0.8660254037844387076, 1.000000000000000000, 0.8660254037844387076, 1.000000000000000000 ) ) 
 REPRESENTATION_ITEM ( '' )  );
#17756 = DIRECTION ( 'NONE',  ( -0.000000000000000000, -0.000000000000000000, 1.000000000000000000 ) ) ;
#17757 = CARTESIAN_POINT ( 'NONE',  ( 10.81189881249999551, -6.242252689847874514, -139.4687500020483810 ) ) ;
#17758 = CARTESIAN_POINT ( 'NONE',  ( 10.81189881249999907, 6.242252689847868297, -146.9062500020484094 ) ) ;
#17760 = EDGE_CURVE ( 'NONE', #25374, #23494, #38898, .T. ) ;
#17759 = CARTESIAN_POINT ( 'NONE',  ( 10.81189881249999729, 0.000000000000000000, -155.8437500020483810 ) ) ;
#17761 = CARTESIAN_POINT ( 'NONE',  ( 9.999999999999998224, 0.000000000000000000, -189.8750000040967905 ) ) ;
#17762 = CARTESIAN_POINT ( 'NONE',  ( -79.99999999999994316, -40.00000000000000711, -160.0000000000000000 ) ) ;
#17763 = CARTESIAN_POINT ( 'NONE',  ( -9.999999999999998224, 1.224646799147353059E-15, -181.2500000000000284 ) ) ;
#17764 = EDGE_CURVE ( 'NONE', #27810, #7227, #4995, .T. ) ;
#17765 = CARTESIAN_POINT ( 'NONE',  ( 10.81189881249999729, 0.000000000000000000, -86.84375000204836681 ) ) ;
#17766 = CARTESIAN_POINT ( 'NONE',  ( -4.999999999999996447, 8.660254037844387298, -180.3750000040967905 ) ) ;
#17767 = CARTESIAN_POINT ( 'NONE',  ( 10.81189881249999729, 0.000000000000000000, -60.03125000204836681 ) ) ;
#17768 = CARTESIAN_POINT ( 'NONE',  ( -9.999999999999998224, 1.224646799147353059E-15, -97.62500000409677625 ) ) ;
#17769 = CARTESIAN_POINT ( 'NONE',  ( -2.293366432827344421E-15, -12.48450537969573659, -174.2187500020484094 ) ) ;
#17770 = CARTESIAN_POINT ( 'NONE',  ( -10.81189881249999729, 6.242252689847871849, -116.4062500020483810 ) ) ;
#17771 = CARTESIAN_POINT ( 'NONE',  ( -5.405949406250003975, -9.363379034771801557, -153.5312500020484094 ) ) ;
#17772 = FACE_OUTER_BOUND ( 'NONE', #18236, .T. ) ;
#17773 = CARTESIAN_POINT ( 'NONE',  ( 7.644554776091147741E-16, 12.48450537969573659, -41.65625000204837391 ) ) ;
#17774 = CARTESIAN_POINT ( 'NONE',  ( 4.999999999999992006, -8.660254037844389075, -133.1250000040967620 ) ) ;
#17775 = CARTESIAN_POINT ( 'NONE',  ( -9.999999999999998224, 1.224646799147353059E-15, -106.2499999999999858 ) ) ;
#17776 = ORIENTED_EDGE ( 'NONE', *, *, #18083, .F. ) ;
#17777 = CARTESIAN_POINT ( 'NONE',  ( 7.644554776091147741E-16, 12.48450537969573659, -130.1562500020483810 ) ) ;
#17778 = CARTESIAN_POINT ( 'NONE',  ( 9.999999999999996447, -5.773502691896262640, -146.5000000040967905 ) ) ;
#17779 = CARTESIAN_POINT ( 'NONE',  ( -9.999999999999998224, 1.224646799147353059E-15, -160.2500000000000000 ) ) ;
#17780 = CARTESIAN_POINT ( 'NONE',  ( 5.405949406249999534, 9.363379034771803333, -179.7812500020484094 ) ) ;
#17781 = ORIENTED_EDGE ( 'NONE', *, *, #38855, .T. ) ;
#17782 = CARTESIAN_POINT ( 'NONE',  ( 9.999999999999998224, 0.000000000000000000, -51.49999999999996447 ) ) ;
#17783 = CARTESIAN_POINT ( 'NONE',  ( -10.81189881249999907, -6.242252689847864744, -175.9687500020483526 ) ) ;
#17784 = CARTESIAN_POINT ( 'NONE',  ( -9.999999999999998224, 5.773502691896259087, -61.75000000409678336 ) ) ;
#17785 = AXIS2_PLACEMENT_3D ( 'NONE', #21871, #11718, #25760 ) ;
#17786 = CYLINDRICAL_SURFACE ( 'NONE', #17556, 9.999999999999998224 ) ;
#17787 = CARTESIAN_POINT ( 'NONE',  ( 7.070501591499376803E-16, 11.54700538379251284, -171.5000000040967905 ) ) ;
#17788 = CARTESIAN_POINT ( 'NONE',  ( -10.81189881249999907, -6.242252689847864744, -69.65625000204839523 ) ) ;
#17789 = CARTESIAN_POINT ( 'NONE',  ( 5.405949406249992428, -9.363379034771808662, -52.78125000204836681 ) ) ;
#17790 = EDGE_CURVE ( 'NONE', #5420, #23886, #28121, .T. ) ;
#17791 = CARTESIAN_POINT ( 'NONE',  ( 5.000000000000000000, 8.660254037844385522, -50.12500000409675494 ) ) ;
#17792 = CARTESIAN_POINT ( 'NONE',  ( 10.81189881249999551, -6.242252689847874514, -5.968750002048355263 ) ) ;
#17793 = CARTESIAN_POINT ( 'NONE',  ( -2.121150477449813534E-15, -11.54700538379251284, -29.75000000409675494 ) ) ;
#17794 = CARTESIAN_POINT ( 'NONE',  ( -5.405949406250003975, -9.363379034771801557, -179.0312500020483810 ) ) ;
#17795 = CARTESIAN_POINT ( 'NONE',  ( -10.00000000000051337, 5.773502691895962435, -147.2500000040967905 ) ) ;
#17796 = CARTESIAN_POINT ( 'NONE',  ( 7.070501591499376803E-16, 11.54700538379251284, -138.5000000040967905 ) ) ;
#17797 = DIRECTION ( 'NONE',  ( 0.9961946980917455452, 0.000000000000000000, -0.08715574274765837404 ) ) ;
#17798 = CARTESIAN_POINT ( 'NONE',  ( 5.000000000000000000, 8.660254037844385522, -105.6250000040967763 ) ) ;
#17799 = CARTESIAN_POINT ( 'NONE',  ( 9.999999999999998224, 0.000000000000000000, -39.87500000409676915 ) ) ;
#17801 = VERTEX_POINT ( 'NONE', #24675 ) ;
#17800 = CARTESIAN_POINT ( 'NONE',  ( 7.644554776091147741E-16, 12.48450537969573659, -89.65625000204839523 ) ) ;
#17802 = DIRECTION ( 'NONE',  ( -0.000000000000000000, -0.000000000000000000, 1.000000000000000000 ) ) ;
#17804 = ORIENTED_EDGE ( 'NONE', *, *, #31687, .T. ) ;
#17803 = CYLINDRICAL_SURFACE ( 'NONE', #39941, 9.999999999999998224 ) ;
#17805 = ORIENTED_EDGE ( 'NONE', *, *, #12168, .T. ) ;
#17806 =( BOUNDED_CURVE ( )  B_SPLINE_CURVE ( 2, ( #822, #27136, #23057, #615, #23267, #6861, #19799 ),
 .UNSPECIFIED., .F., .F. ) 
 B_SPLINE_CURVE_WITH_KNOTS ( ( 3, 2, 2, 3 ),
 ( 0.2500000000000001110, 0.2512437810945274963, 0.2524875621890548261, 0.2537313432835822113 ),
 .UNSPECIFIED. ) 
 CURVE ( )  GEOMETRIC_REPRESENTATION_ITEM ( )  RATIONAL_B_SPLINE_CURVE ( ( 0.9999999999999880096, 0.8660254037844506980, 1.000000000000000000, 0.8660254037844387076, 1.000000000000000000, 0.8660254037844267172, 1.000000000000011990 ) ) 
 REPRESENTATION_ITEM ( '' )  );
#17807 = CARTESIAN_POINT ( 'NONE',  ( 10.81189881249999551, -6.242252689847874514, -34.46875000204835260 ) ) ;
#17808 = CARTESIAN_POINT ( 'NONE',  ( 10.81189881249999907, 6.242252689847868297, -28.21875000204838457 ) ) ;
#17809 = CARTESIAN_POINT ( 'NONE',  ( 10.81189881249999729, 0.000000000000000000, -16.53125000204835970 ) ) ;
#17810 = CARTESIAN_POINT ( 'NONE',  ( -10.81189881249999907, -6.242252689847864744, -61.96875000204838813 ) ) ;
#17811 = CARTESIAN_POINT ( 'NONE',  ( -9.999999999999998224, 1.224646799147353059E-15, -162.1250000040967905 ) ) ;
#17812 = CARTESIAN_POINT ( 'NONE',  ( 5.000000000000000000, 8.660254037844385522, -46.74999999999998579 ) ) ;
#17813 = VECTOR ( 'NONE', #36736, 1000.000000000000000 ) ;
#17814 = CARTESIAN_POINT ( 'NONE',  ( 5.405949406249999534, 9.363379034771803333, -185.5937500020483810 ) ) ;
#17815 = CARTESIAN_POINT ( 'NONE',  ( 10.81189881249999551, -6.242252689847874514, -161.9687500020484094 ) ) ;
#17816 = CARTESIAN_POINT ( 'NONE',  ( -10.81189881249999729, 6.242252689847871849, -179.2187500020484379 ) ) ;
#17817 = LINE ( 'NONE', #31440, #32266 ) ;
#17818 = CARTESIAN_POINT ( 'NONE',  ( 0.000000000000000000, 0.000000000000000000, -200.0000000000000000 ) ) ;
#17819 = CARTESIAN_POINT ( 'NONE',  ( 4.999999999999992006, -8.660254037844389075, -104.2499999999999858 ) ) ;
#17820 = CARTESIAN_POINT ( 'NONE',  ( -9.999999999999998224, 1.224646799147353059E-15, -200.0000000000000000 ) ) ;
#17821 = CARTESIAN_POINT ( 'NONE',  ( -10.81189881249999729, 6.242252689847871849, -113.2187500020483952 ) ) ;
#17822 = DIRECTION ( 'NONE',  ( 1.000000000000000000, 0.000000000000000000, 0.000000000000000000 ) ) ;
#17823 = CARTESIAN_POINT ( 'NONE',  ( 5.405949406249992428, -9.363379034771808662, -84.28125000204838102 ) ) ;
#17824 = CARTESIAN_POINT ( 'NONE',  ( 10.81189881249999729, 0.000000000000000000, -98.84375000204838102 ) ) ;
#17825 = CARTESIAN_POINT ( 'NONE',  ( 5.405949406249992428, -9.363379034771808662, -63.09375000204836681 ) ) ;
#17826 = CARTESIAN_POINT ( 'NONE',  ( -10.81189881249999907, -6.242252689847864744, -71.15625000204839523 ) ) ;
#17827 = CARTESIAN_POINT ( 'NONE',  ( -2.121150477449813534E-15, -11.54700538379251284, -157.2500000040967620 ) ) ;
#17828 = CARTESIAN_POINT ( 'NONE',  ( 9.999999999999996447, -5.773502691896262640, -129.6250000000000000 ) ) ;
#17829 = CARTESIAN_POINT ( 'NONE',  ( -5.405949406249996869, 9.363379034771805109, -154.0312500020484094 ) ) ;
#17830 = CARTESIAN_POINT ( 'NONE',  ( 10.81189881249999729, 0.000000000000000000, -168.0312500020484094 ) ) ;
#17831 = EDGE_CURVE ( 'NONE', #33370, #31274, #41249, .T. ) ;
#17832 = CARTESIAN_POINT ( 'NONE',  ( 7.644554776091147741E-16, 12.48450537969573659, -0.9687500020483519325 ) ) ;
#17833 = CARTESIAN_POINT ( 'NONE',  ( -5.405949406250003975, -9.363379034771801557, -96.34375000204838102 ) ) ;
#17834 = CARTESIAN_POINT ( 'NONE',  ( 5.000000000000000000, 8.660254037844385522, -10.74999999999995381 ) ) ;
#17835 = CARTESIAN_POINT ( 'NONE',  ( 9.999999999999998224, 0.000000000000000000, -75.49999999999998579 ) ) ;
#17836 = CARTESIAN_POINT ( 'NONE',  ( -10.81189881249999907, -6.242252689847864744, -0.6562500020483587049 ) ) ;
#17837 = CARTESIAN_POINT ( 'NONE',  ( -9.999999999999998224, 1.224646799147353059E-15, -81.12500000409677625 ) ) ;
#17838 = CARTESIAN_POINT ( 'NONE',  ( -2.121150477449813534E-15, -11.54700538379251284, -142.2500000040967905 ) ) ;
#17839 = CARTESIAN_POINT ( 'NONE',  ( -5.405949406250003975, -9.363379034771801557, -101.0312500020483952 ) ) ;
#17840 = CARTESIAN_POINT ( 'NONE',  ( 10.81189881249999729, 6.242252689847867408, -71.90625000204836681 ) ) ;
#17841 = CARTESIAN_POINT ( 'NONE',  ( 10.00000000000000000, 5.773502691896255534, -77.25000000409677625 ) ) ;
#17842 = CARTESIAN_POINT ( 'NONE',  ( 9.999999999998456346, 5.773502691897149042, -21.37499999999993605 ) ) ;
#17843 = CARTESIAN_POINT ( 'NONE',  ( 5.405949406249992428, -9.363379034771808662, -37.59375000204837391 ) ) ;
#17844 = ORIENTED_EDGE ( 'NONE', *, *, #24680, .T. ) ;
#17845 = CARTESIAN_POINT ( 'NONE',  ( -10.81189881249999729, 1.324075727343319199E-15, -198.7812500020484094 ) ) ;
#17846 = CARTESIAN_POINT ( 'NONE',  ( 5.405949406249999534, 9.363379034771803333, -28.28125000204837036 ) ) ;
#17847 = CARTESIAN_POINT ( 'NONE',  ( 5.405949406249992428, -9.363379034771808662, -10.59375000204834727 ) ) ;
#17848 = CARTESIAN_POINT ( 'NONE',  ( 9.999999999999479527, 5.773502691896553074, -142.8749999999999716 ) ) ;
#17849 = CARTESIAN_POINT ( 'NONE',  ( 7.070501591499377789E-16, 11.54700538379251284, -5.000000004096755823 ) ) ;
#17850 = CARTESIAN_POINT ( 'NONE',  ( 5.405949406249999534, 9.363379034771803333, -130.2812500020483810 ) ) ;
#17851 = CARTESIAN_POINT ( 'NONE',  ( 5.000000000000000000, 8.660254037844385522, -183.2500000000000000 ) ) ;
#17852 = CARTESIAN_POINT ( 'NONE',  ( -9.999999999999998224, 1.224646799147353059E-15, -109.2499999999999858 ) ) ;
#17853 = AXIS2_PLACEMENT_3D ( 'NONE', #26031, #39184, #38769 ) ;
#17855 = ORIENTED_EDGE ( 'NONE', *, *, #7199, .T. ) ;
#17854 = CARTESIAN_POINT ( 'NONE',  ( 10.81189881249999729, 0.000000000000000000, -106.5312500020483810 ) ) ;
#17856 = CARTESIAN_POINT ( 'NONE',  ( 9.999999999999998224, 0.000000000000000000, -200.0000000000000000 ) ) ;
#17857 = VERTEX_POINT ( 'NONE', #18386 ) ;
#17858 = EDGE_LOOP ( 'NONE', ( #7445, #35918, #42225, #41594 ) ) ;
#17859 = VECTOR ( 'NONE', #3888, 1000.000000000000114 ) ;
#17860 = CARTESIAN_POINT ( 'NONE',  ( 10.81189881249999907, 6.242252689847868297, -35.90625000204835260 ) ) ;
#17861 = DATE_TIME_ROLE ( 'classification_date' ) ;
#17862 = CARTESIAN_POINT ( 'NONE',  ( -5.405949406249996869, 9.363379034771805109, -84.84375000204836681 ) ) ;
#17863 = CARTESIAN_POINT ( 'NONE',  ( -9.999999999999998224, 1.224646799147353059E-15, -101.7500000000000000 ) ) ;
#17864 = CARTESIAN_POINT ( 'NONE',  ( -4.999999999999996447, 8.660254037844387298, -174.0000000000000284 ) ) ;
#17865 = CARTESIAN_POINT ( 'NONE',  ( -10.00000000000051337, 5.773502691895962435, -105.2500000040967620 ) ) ;
#17866 = CARTESIAN_POINT ( 'NONE',  ( 10.81189881249999729, 0.000000000000000000, -165.0312500020484094 ) ) ;
#17867 = CARTESIAN_POINT ( 'NONE',  ( -5.000000000000003553, -8.660254037844383745, -68.49999999999997158 ) ) ;
#17868 = CARTESIAN_POINT ( 'NONE',  ( 10.81189881249999729, 0.000000000000000000, -127.3437500020483952 ) ) ;
#17869 = CARTESIAN_POINT ( 'NONE',  ( 10.81189881249999551, -6.242252689847874514, -82.46875000204836681 ) ) ;
#17870 = CARTESIAN_POINT ( 'NONE',  ( 10.81189881249999729, 6.242252689847867408, -1.406250002048370584 ) ) ;
#17871 = CARTESIAN_POINT ( 'NONE',  ( 10.81189881249999907, 6.242252689847868297, -196.2187500020484094 ) ) ;
#17872 = CARTESIAN_POINT ( 'NONE',  ( -10.81189881249999907, -6.242252689847864744, -89.15625000204839523 ) ) ;
#17873 = CARTESIAN_POINT ( 'NONE',  ( -2.121150477449813534E-15, -11.54700538379251284, -178.2500000040967620 ) ) ;
#17874 = CARTESIAN_POINT ( 'NONE',  ( -5.405949406249996869, 9.363379034771805109, -104.3437500020483810 ) ) ;
#17875 = CARTESIAN_POINT ( 'NONE',  ( 10.81189881249999729, 6.242252689847867408, -175.4062500020484094 ) ) ;
#17876 = CARTESIAN_POINT ( 'NONE',  ( 10.00000000000102318, -5.773502691895667560, -28.00000000409675494 ) ) ;
#17877 = CARTESIAN_POINT ( 'NONE',  ( 9.999999999999998224, 0.000000000000000000, -182.0000000000000000 ) ) ;
#17878 = CARTESIAN_POINT ( 'NONE',  ( -5.405949406250003975, -9.363379034771801557, -194.0312500020484094 ) ) ;
#17879 = CARTESIAN_POINT ( 'NONE',  ( 10.81189881249999729, 6.242252689847867408, -49.21875000204835970 ) ) ;
#17880 = CARTESIAN_POINT ( 'NONE',  ( -5.000000000000003553, -8.660254037844383745, -169.3750000040967905 ) ) ;
#17881 = CARTESIAN_POINT ( 'NONE',  ( 5.405949406249999534, 9.363379034771803333, -11.78125000204835438 ) ) ;
#17882 = CARTESIAN_POINT ( 'NONE',  ( -5.405949406249996869, 9.363379034771805109, -23.34375000204835970 ) ) ;
#17883 = CARTESIAN_POINT ( 'NONE',  ( -10.81189881249999729, 6.242252689847871849, -128.2187500020483810 ) ) ;
#17884 = CARTESIAN_POINT ( 'NONE',  ( 10.00000000000000000, 5.773502691896255534, -96.37499999999998579 ) ) ;
#17885 = CARTESIAN_POINT ( 'NONE',  ( 5.405949406249999534, 9.363379034771803333, -29.78125000204837036 ) ) ;
#17886 = CARTESIAN_POINT ( 'NONE',  ( 4.999999999999992006, -8.660254037844389075, -109.1250000040967763 ) ) ;
#17887 = CARTESIAN_POINT ( 'NONE',  ( -9.999999999999998224, 1.224646799147353059E-15, -27.12500000409676204 ) ) ;
#17888 = CARTESIAN_POINT ( 'NONE',  ( -9.999999999999998224, 1.224646799147353059E-15, -49.24999999999998579 ) ) ;
#17889 = CARTESIAN_POINT ( 'NONE',  ( 10.81189881249999729, 0.000000000000000000, -121.5312500020483952 ) ) ;
#17890 = CARTESIAN_POINT ( 'NONE',  ( -10.81189881249999729, 6.242252689847871849, -101.4062500020483952 ) ) ;
#17891 = VERTEX_POINT ( 'NONE', #21633 ) ;
#17892 = CARTESIAN_POINT ( 'NONE',  ( -5.000000000000003553, -8.660254037844383745, -97.37500000409677625 ) ) ;
#17893 = CARTESIAN_POINT ( 'NONE',  ( 9.999999999999998224, 0.000000000000000000, -112.9999999999999858 ) ) ;
#17894 = CARTESIAN_POINT ( 'NONE',  ( -5.405949406250003975, -9.363379034771801557, -161.0312500020484094 ) ) ;
#17895 = CARTESIAN_POINT ( 'NONE',  ( -10.81189881249999729, 6.242252689847871849, -56.21875000204837391 ) ) ;
#17896 = VERTEX_POINT ( 'NONE', #34811 ) ;
#17897 = CARTESIAN_POINT ( 'NONE',  ( -4.999999999999996447, 8.660254037844387298, -22.49999999999996447 ) ) ;
#17898 = APPLICATION_CONTEXT ( 'configuration controlled 3d designs of mechanical parts and assemblies' ) ;
#17899 = CARTESIAN_POINT ( 'NONE',  ( -10.81189881249999729, 1.324075727343319199E-15, -32.28125000204837391 ) ) ;
#17900 = CARTESIAN_POINT ( 'NONE',  ( 9.999999999999996447, -5.773502691896262640, -159.6250000000000284 ) ) ;
#17901 = EDGE_CURVE ( 'NONE', #22578, #7470, #9395, .T. ) ;
#17902 = CARTESIAN_POINT ( 'NONE',  ( -5.000000000000003553, -8.660254037844383745, -92.49999999999998579 ) ) ;
#17903 =( BOUNDED_CURVE ( )  B_SPLINE_CURVE ( 2, ( #40454, #10899, #14337, #11107, #28821, #2488, #25159 ),
 .UNSPECIFIED., .F., .F. ) 
 B_SPLINE_CURVE_WITH_KNOTS ( ( 3, 2, 2, 3 ),
 ( 0.1119402985074627876, 0.1131840796019901035, 0.1144278606965174333, 0.1156716417910447492 ),
 .UNSPECIFIED. ) 
 CURVE ( )  GEOMETRIC_REPRESENTATION_ITEM ( )  RATIONAL_B_SPLINE_CURVE ( ( 0.9999999999999894529, 0.8660254037844491437, 1.000000000000000000, 0.8660254037844387076, 1.000000000000000000, 0.8660254037844417052, 0.9999999999999970024 ) ) 
 REPRESENTATION_ITEM ( '' )  );
#17904 = CARTESIAN_POINT ( 'NONE',  ( -9.999999999999998224, 5.773502691896259087, -27.25000000409677625 ) ) ;
#17905 = CARTESIAN_POINT ( 'NONE',  ( -4.999999999999996447, 8.660254037844387298, -168.0000000000000000 ) ) ;
#17906 = CARTESIAN_POINT ( 'NONE',  ( -5.405949406249996869, 9.363379034771805109, -133.0312500020484094 ) ) ;
#17907 = CARTESIAN_POINT ( 'NONE',  ( 9.999999999999998224, 0.000000000000000000, -111.4999999999999858 ) ) ;
#17908 = CYLINDRICAL_SURFACE ( 'NONE', #32802, 9.999999999999998224 ) ;
#17909 = ORIENTED_EDGE ( 'NONE', *, *, #23720, .T. ) ;
#17910 = CARTESIAN_POINT ( 'NONE',  ( 7.644554776091147741E-16, 12.48450537969573659, -64.15625000204838102 ) ) ;
#17911 = VECTOR ( 'NONE', #2549, 1000.000000000000000 ) ;
#17913 = ORIENTED_EDGE ( 'NONE', *, *, #598, .F. ) ;
#17912 = EDGE_LOOP ( 'NONE', ( #35232, #35494, #28919, #22817 ) ) ;
#17914 = CARTESIAN_POINT ( 'NONE',  ( 9.999999999999998224, 0.000000000000000000, -120.5000000000000000 ) ) ;
#17915 = FACE_OUTER_BOUND ( 'NONE', #14099, .T. ) ;
#17916 = CARTESIAN_POINT ( 'NONE',  ( -5.405949406249996869, 9.363379034771805109, -165.8437500020484094 ) ) ;
#17917 = CARTESIAN_POINT ( 'NONE',  ( -5.405949406250003975, -9.363379034771801557, -192.5312500020484094 ) ) ;
#17918 = CARTESIAN_POINT ( 'NONE',  ( 7.644554776091147741E-16, 12.48450537969573659, -14.46875000204836859 ) ) ;
#17919 = CYLINDRICAL_SURFACE ( 'NONE', #11556, 9.999999999999998224 ) ;
#17920 = CARTESIAN_POINT ( 'NONE',  ( 5.405949406249992428, -9.363379034771808662, -151.5937500020483810 ) ) ;
#17921 = CARTESIAN_POINT ( 'NONE',  ( -10.81189881249999729, 6.242252689847871849, -125.2187500020483810 ) ) ;
#17922 = CARTESIAN_POINT ( 'NONE',  ( -5.405949406250003975, -9.363379034771801557, -105.5312500020483810 ) ) ;
#17923 = CARTESIAN_POINT ( 'NONE',  ( -10.81189881249999729, 6.242252689847871849, -114.7187500020483810 ) ) ;
#17924 = CARTESIAN_POINT ( 'NONE',  ( 9.999999999999834799, 5.773502691896347905, -191.2500000040968473 ) ) ;
#17925 = CARTESIAN_POINT ( 'NONE',  ( -10.81189881249999729, 1.324075727343319199E-15, -125.2812500020483668 ) ) ;
#17926 = CARTESIAN_POINT ( 'NONE',  ( -5.405949406249996869, 9.363379034771805109, -2.343750002048366810 ) ) ;
#17927 = CARTESIAN_POINT ( 'NONE',  ( 10.81189881249999729, 6.242252689847867408, -131.7187500020483810 ) ) ;
#17928 = CARTESIAN_POINT ( 'NONE',  ( 7.070501591499376803E-16, 11.54700538379251284, -163.6250000000000284 ) ) ;
#17929 = CARTESIAN_POINT ( 'NONE',  ( 4.999999999999992006, -8.660254037844389075, -178.1250000040968189 ) ) ;
#17930 = CARTESIAN_POINT ( 'NONE',  ( -5.000000000000003553, -8.660254037844383745, -149.5000000000000000 ) ) ;
#17931 = CARTESIAN_POINT ( 'NONE',  ( -2.121150477449813534E-15, -11.54700538379251284, -23.37499999999997868 ) ) ;
#17932 = CARTESIAN_POINT ( 'NONE',  ( -10.81189881249999729, 1.324075727343319199E-15, -77.09375000204838102 ) ) ;
#17933 = CARTESIAN_POINT ( 'NONE',  ( 10.81189881249999907, 6.242252689847868297, -62.71875000204838813 ) ) ;
#17934 = LINE ( 'NONE', #40593, #24288 ) ;
#17935 = CARTESIAN_POINT ( 'NONE',  ( 10.81189881249999729, 0.000000000000000000, -33.03125000204837391 ) ) ;
#17936 = CARTESIAN_POINT ( 'NONE',  ( 10.81189881249999907, 6.242252689847868297, -43.21875000204835970 ) ) ;
#17937 = CYLINDRICAL_SURFACE ( 'NONE', #33701, 9.999999999999998224 ) ;
#17938 = CARTESIAN_POINT ( 'NONE',  ( -10.81189881249999907, -6.242252689847864744, -153.4687500020484094 ) ) ;
#17939 = CARTESIAN_POINT ( 'NONE',  ( 7.070501591499377789E-16, 11.54700538379251284, -124.6249999999999858 ) ) ;
#17940 = CARTESIAN_POINT ( 'NONE',  ( 10.81189881249999551, -6.242252689847874514, -130.6562500020483810 ) ) ;
#17941 = CARTESIAN_POINT ( 'NONE',  ( 7.070501591499376803E-16, 11.54700538379251284, -94.62500000000000000 ) ) ;
#17942 = CARTESIAN_POINT ( 'NONE',  ( -5.000000000000003553, -8.660254037844383745, -75.99999999999998579 ) ) ;
#17943 = CARTESIAN_POINT ( 'NONE',  ( -2.293366432827344421E-15, -12.48450537969573659, -10.90625000204838102 ) ) ;
#17944 = ORIENTED_EDGE ( 'NONE', *, *, #41978, .T. ) ;
#17945 =( BOUNDED_CURVE ( )  B_SPLINE_CURVE ( 2, ( #4365, #30699, #17504, #27815, #40309, #24375, #4501 ),
 .UNSPECIFIED., .F., .F. ) 
 B_SPLINE_CURVE_WITH_KNOTS ( ( 3, 2, 2, 3 ),
 ( 0.1604477611940298698, 0.1616915422885572551, 0.1629353233830845848, 0.1641791044776119424 ),
 .UNSPECIFIED. ) 
 CURVE ( )  GEOMETRIC_REPRESENTATION_ITEM ( )  RATIONAL_B_SPLINE_CURVE ( ( 0.9999999999999970024, 0.8660254037844417052, 1.000000000000000000, 0.8660254037844387076, 1.000000000000000000, 0.8660254037844387076, 1.000000000000000000 ) ) 
 REPRESENTATION_ITEM ( '' )  );
#17946 = CARTESIAN_POINT ( 'NONE',  ( -10.81189881249999729, -6.242252689847864744, -101.1562500020483952 ) ) ;
#17947 = CARTESIAN_POINT ( 'NONE',  ( -4.999999999999996447, 8.660254037844387298, -120.3750000040967905 ) ) ;
#17948 = CARTESIAN_POINT ( 'NONE',  ( 4.999999999999992006, -8.660254037844389075, -56.62500000409676204 ) ) ;
#17949 = CARTESIAN_POINT ( 'NONE',  ( -2.121150477449813534E-15, -11.54700538379251284, -34.25000000409674783 ) ) ;
#17950 = VECTOR ( 'NONE', #40448, 1000.000000000000000 ) ;
#17951 = CARTESIAN_POINT ( 'NONE',  ( 10.81189881249999729, 0.000000000000000000, -43.53125000204838102 ) ) ;
#17952 =( BOUNDED_CURVE ( )  B_SPLINE_CURVE ( 2, ( #41940, #39341, #32676, #5716, #25569, #32255, #42574 ),
 .UNSPECIFIED., .F., .F. ) 
 B_SPLINE_CURVE_WITH_KNOTS ( ( 3, 2, 2, 3 ),
 ( 0.8768656716417913000, 0.8781094527363186852, 0.8793532338308460705, 0.8805970149253734558 ),
 .UNSPECIFIED. ) 
 CURVE ( )  GEOMETRIC_REPRESENTATION_ITEM ( )  RATIONAL_B_SPLINE_CURVE ( ( 0.9999999999999761302, 0.8660254037844625774, 1.000000000000000000, 0.8660254037844387076, 1.000000000000000000, 0.8660254037844028474, 1.000000000000035971 ) ) 
 REPRESENTATION_ITEM ( '' )  );
#17953 = CARTESIAN_POINT ( 'NONE',  ( 9.999999999999998224, 0.000000000000000000, -126.8750000040967905 ) ) ;
#17954 = CARTESIAN_POINT ( 'NONE',  ( 5.405949406249999534, 9.363379034771803333, -151.2812500020484094 ) ) ;
#17955 = CARTESIAN_POINT ( 'NONE',  ( -10.81189881249999729, 1.324075727343319199E-15, -125.0937500020483668 ) ) ;
#17957 = EDGE_CURVE ( 'NONE', #34507, #39040, #27049, .T. ) ;
#17956 = CARTESIAN_POINT ( 'NONE',  ( 9.999999999999998224, 0.000000000000000000, -191.0000000000000000 ) ) ;
#17958 = EDGE_LOOP ( 'NONE', ( #40090, #22527, #38575, #15886 ) ) ;
#17959 = CARTESIAN_POINT ( 'NONE',  ( 0.000000000000000000, 0.000000000000000000, -200.0000000000000000 ) ) ;
#17960 = ORIENTED_EDGE ( 'NONE', *, *, #33366, .T. ) ;
#17961 = ORIENTED_EDGE ( 'NONE', *, *, #41735, .F. ) ;
#17962 = ORIENTED_EDGE ( 'NONE', *, *, #39591, .F. ) ;
#17963 = CARTESIAN_POINT ( 'NONE',  ( 9.999999999999998224, 0.000000000000000000, -189.5000000000000000 ) ) ;
#17964 = CARTESIAN_POINT ( 'NONE',  ( 7.644554776091147741E-16, 12.48450537969573659, -189.9687500020484094 ) ) ;
#17965 = ORGANIZATION ( 'UNSPECIFIED', 'UNSPECIFIED', '' ) ;
#17966 = CARTESIAN_POINT ( 'NONE',  ( 5.405949406249999534, 9.363379034771803333, -37.09375000204836681 ) ) ;
#17967 = CARTESIAN_POINT ( 'NONE',  ( 2.944358404844418686, -10.14388074307273691, -1.167351363741249440E-15 ) ) ;
#17968 = CARTESIAN_POINT ( 'NONE',  ( 9.999999999998456346, 5.773502691897149042, -14.25000000409672651 ) ) ;
#17969 = CARTESIAN_POINT ( 'NONE',  ( -2.293366432827344421E-15, -12.48450537969573659, -171.2187500020483810 ) ) ;
#17970 = CARTESIAN_POINT ( 'NONE',  ( -10.81189881249999729, 1.324075727343319199E-15, -161.0937500020484094 ) ) ;
#17971 = CARTESIAN_POINT ( 'NONE',  ( -23.09401076758503280, 0.000000000000000000, 45.00000000000009237 ) ) ;
#17972 = CARTESIAN_POINT ( 'NONE',  ( -5.405949406250003975, -9.363379034771801557, -141.3437500020483810 ) ) ;
#17973 = CARTESIAN_POINT ( 'NONE',  ( -10.81189881249999729, 6.242252689847871849, -144.9062500020484094 ) ) ;
#17974 = CARTESIAN_POINT ( 'NONE',  ( 7.644554776091147741E-16, 12.48450537969573659, -150.9687500020484094 ) ) ;
#17975 = CARTESIAN_POINT ( 'NONE',  ( 9.999999999999998224, 0.000000000000000000, -93.49999999999998579 ) ) ;
#17976 = CARTESIAN_POINT ( 'NONE',  ( 0.000000000000000000, 0.000000000000000000, -99.99999999999998579 ) ) ;
#17977 = CARTESIAN_POINT ( 'NONE',  ( 4.999999999999992006, -8.660254037844389075, -173.2500000000000284 ) ) ;
#17978 = CARTESIAN_POINT ( 'NONE',  ( 5.405949406249999534, 9.363379034771803333, -91.09375000204838102 ) ) ;
#17979 = DIRECTION ( 'NONE',  ( -0.000000000000000000, -0.000000000000000000, -1.000000000000000000 ) ) ;
#17980 = CARTESIAN_POINT ( 'NONE',  ( -10.81189881249999729, 1.324075727343319199E-15, -54.78125000204836681 ) ) ;
#17981 = CARTESIAN_POINT ( 'NONE',  ( -5.000000000000003553, -8.660254037844383745, -16.37500000409675138 ) ) ;
#17982 = CARTESIAN_POINT ( 'NONE',  ( -10.81189881249999729, 1.324075727343319199E-15, -176.0937500020484094 ) ) ;
#17983 = CARTESIAN_POINT ( 'NONE',  ( 10.81189881249999907, 6.242252689847868297, -112.4062500020483952 ) ) ;
#17984 = CARTESIAN_POINT ( 'NONE',  ( 10.81189881249999551, -6.242252689847874514, -156.1562500020483526 ) ) ;
#17985 = CARTESIAN_POINT ( 'NONE',  ( -9.999999999999998224, 1.224646799147353059E-15, -182.7500000000000000 ) ) ;
#17986 = CARTESIAN_POINT ( 'NONE',  ( -10.81189881249999907, -6.242252689847864744, -41.15625000204836681 ) ) ;
#17987 = CARTESIAN_POINT ( 'NONE',  ( 9.999999999999998224, 0.000000000000000000, -132.8750000040967905 ) ) ;
#17988 = CARTESIAN_POINT ( 'NONE',  ( 10.00000000000000000, 5.773502691896255534, -106.8749999999999716 ) ) ;
#17989 = VERTEX_POINT ( 'NONE', #31791 ) ;
#17990 = CARTESIAN_POINT ( 'NONE',  ( -10.81189881249999729, 6.242252689847871849, -123.9062500020483810 ) ) ;
#17991 = CARTESIAN_POINT ( 'NONE',  ( -9.999999999999998224, 1.224646799147353059E-15, -145.6250000040967905 ) ) ;
#17992 = DIRECTION ( 'NONE',  ( 0.000000000000000000, 0.000000000000000000, 1.000000000000000000 ) ) ;
#17993 = CARTESIAN_POINT ( 'NONE',  ( 5.405949406249992428, -9.363379034771808662, -181.7812500020483810 ) ) ;
#17994 = ORIENTED_EDGE ( 'NONE', *, *, #29405, .F. ) ;
#17995 = CARTESIAN_POINT ( 'NONE',  ( -2.293366432827344421E-15, -12.48450537969573659, -172.7187500020484094 ) ) ;
#17996 = CARTESIAN_POINT ( 'NONE',  ( 4.999999999999992006, -8.660254037844389075, -56.62500000409676204 ) ) ;
#17997 = DIRECTION ( 'NONE',  ( -0.7071067811865451302, 8.659560562354903276E-17, 0.7071067811865500152 ) ) ;
#17998 = CARTESIAN_POINT ( 'NONE',  ( -4.999999999999996447, 8.660254037844387298, -135.3750000040967905 ) ) ;
#17999 = CARTESIAN_POINT ( 'NONE',  ( -10.81189881249999907, -6.242252689847864744, -71.15625000204839523 ) ) ;
#18000 = CARTESIAN_POINT ( 'NONE',  ( 10.81189881249999551, -6.242252689847874514, -54.15625000204837391 ) ) ;
#18001 = CARTESIAN_POINT ( 'NONE',  ( -2.121150477449813534E-15, -11.54700538379251284, -47.75000000409676204 ) ) ;
#18002 = CARTESIAN_POINT ( 'NONE',  ( 5.405949406249999534, 9.363379034771803333, -2.593750002048367254 ) ) ;
#18003 = CARTESIAN_POINT ( 'NONE',  ( 9.999999999999998224, 0.000000000000000000, -34.99999999999997868 ) ) ;
#18004 = CARTESIAN_POINT ( 'NONE',  ( -5.405949406249996869, 9.363379034771805109, -179.5312500020483810 ) ) ;
#18005 = SECURITY_CLASSIFICATION ( '', '', #10960 ) ;
#18006 = ADVANCED_FACE ( 'NONE', ( #35235 ), #19234, .T. ) ;
#18007 = DIRECTION ( 'NONE',  ( -0.000000000000000000, -0.000000000000000000, -1.000000000000000000 ) ) ;
#18009 = EDGE_CURVE ( 'NONE', #22602, #6595, #36121, .T. ) ;
#18008 = DIRECTION ( 'NONE',  ( -0.000000000000000000, -0.000000000000000000, 1.000000000000000000 ) ) ;
#18010 = ORIENTED_EDGE ( 'NONE', *, *, #8704, .F. ) ;
#18011 = CARTESIAN_POINT ( 'NONE',  ( 9.999999999999998224, 0.000000000000000000, -0.4999999999999726885 ) ) ;
#18012 = EDGE_CURVE ( 'NONE', #27414, #36340, #6626, .T. ) ;
#18013 = CARTESIAN_POINT ( 'NONE',  ( -6.964452268037473637, 6.964452268037472749, -201.2186212422413689 ) ) ;
#18014 = ADVANCED_FACE ( 'NONE', ( #2225 ), #25937, .F. ) ;
#18015 = CARTESIAN_POINT ( 'NONE',  ( -9.999999999999998224, 1.224646799147353059E-15, -127.6250000040967620 ) ) ;
#18016 = VECTOR ( 'NONE', #30678, 1000.000000000000000 ) ;
#18018 = VERTEX_POINT ( 'NONE', #9525 ) ;
#18017 = CARTESIAN_POINT ( 'NONE',  ( 10.81189881249999729, 0.000000000000000000, -84.03125000204838102 ) ) ;
#18020 = VERTEX_POINT ( 'NONE', #28550 ) ;
#18019 = CARTESIAN_POINT ( 'NONE',  ( 9.999999999999998224, 0.000000000000000000, -17.37500000409675138 ) ) ;
#18021 =( BOUNDED_CURVE ( )  B_SPLINE_CURVE ( 2, ( #19068, #41512, #12364, #12155, #15175, #21882, #9354 ),
 .UNSPECIFIED., .F., .F. ) 
 B_SPLINE_CURVE_WITH_KNOTS ( ( 3, 2, 2, 3 ),
 ( 0.8470149253731346084, 0.8482587064676619937, 0.8495024875621892679, 0.8507462686567166532 ),
 .UNSPECIFIED. ) 
 CURVE ( )  GEOMETRIC_REPRESENTATION_ITEM ( )  RATIONAL_B_SPLINE_CURVE ( ( 0.9999999999999641398, 0.8660254037844745678, 1.000000000000000000, 0.8660254037844387076, 1.000000000000000000, 0.8660254037844148378, 1.000000000000023981 ) ) 
 REPRESENTATION_ITEM ( '' )  );
#18022 = PRODUCT_RELATED_PRODUCT_CATEGORY ( 'detail', '', ( #10757 ) ) ;
#18023 = VERTEX_POINT ( 'NONE', #22695 ) ;
#18024 = CARTESIAN_POINT ( 'NONE',  ( -10.81189881249999729, 6.242252689847871849, -33.71875000204834549 ) ) ;
#18025 = DIRECTION ( 'NONE',  ( -1.000000000000000000, 0.000000000000000000, 0.000000000000000000 ) ) ;
#18026 = CARTESIAN_POINT ( 'NONE',  ( 7.644554776091147741E-16, 12.48450537969573659, -17.65625000204836681 ) ) ;
#18028 = EDGE_LOOP ( 'NONE', ( #35948, #24849, #14452, #38544 ) ) ;
#18027 = CARTESIAN_POINT ( 'NONE',  ( -5.405949406250003975, -9.363379034771801557, -61.84375000204836681 ) ) ;
#18029 = CARTESIAN_POINT ( 'NONE',  ( 5.000000000000000000, 8.660254037844385522, -28.74999999999997158 ) ) ;
#18030 = CARTESIAN_POINT ( 'NONE',  ( 7.070501591499377789E-16, 11.54700538379251284, -39.12499999999997158 ) ) ;
#18031 = CARTESIAN_POINT ( 'NONE',  ( 10.81189881249999551, -6.242252689847874514, -184.4687500020483810 ) ) ;
#18032 = CARTESIAN_POINT ( 'NONE',  ( -10.81189881249999729, 1.324075727343319199E-15, -168.5937500020484094 ) ) ;
#18033 = CIRCLE ( 'NONE', #29768, 5.500000000000003553 ) ;
#18034 = CARTESIAN_POINT ( 'NONE',  ( 10.81189881249999729, 0.000000000000000000, -179.8437500020483810 ) ) ;
#18035 = CARTESIAN_POINT ( 'NONE',  ( 9.999999999999998224, 0.000000000000000000, -167.3750000040967905 ) ) ;
#18036 = CARTESIAN_POINT ( 'NONE',  ( -4.999999999999996447, 8.660254037844387298, -103.8750000040967763 ) ) ;
#18037 = EDGE_CURVE ( 'NONE', #8964, #35035, #27055, .T. ) ;
#18038 = CARTESIAN_POINT ( 'NONE',  ( 7.070501591499377789E-16, 11.54700538379251284, -195.1250000000000284 ) ) ;
#18039 = CARTESIAN_POINT ( 'NONE',  ( -2.293366432827344421E-15, -12.48450537969573659, -111.2187500020483668 ) ) ;
#18040 = FACE_OUTER_BOUND ( 'NONE', #36544, .T. ) ;
#18041 = CARTESIAN_POINT ( 'NONE',  ( 5.405949406249999534, 9.363379034771803333, -80.78125000204838102 ) ) ;
#18042 = CARTESIAN_POINT ( 'NONE',  ( 10.81189881249999729, 0.000000000000000000, -88.34375000204838102 ) ) ;
#18043 = CARTESIAN_POINT ( 'NONE',  ( -10.81189881249999729, 6.242252689847871849, -59.21875000204837391 ) ) ;
#18044 = CARTESIAN_POINT ( 'NONE',  ( 7.644554776091147741E-16, 12.48450537969573659, -68.65625000204839523 ) ) ;
#18045 = CARTESIAN_POINT ( 'NONE',  ( -5.000000000000003553, -8.660254037844383745, -155.8750000040967905 ) ) ;
#18046 = CARTESIAN_POINT ( 'NONE',  ( 9.999999999999998224, 0.000000000000000000, -128.0000000000000000 ) ) ;
#18047 = CARTESIAN_POINT ( 'NONE',  ( 5.405949406249992428, -9.363379034771808662, -153.2812500020484094 ) ) ;
#18048 = CARTESIAN_POINT ( 'NONE',  ( 5.405949406249992428, -9.363379034771808662, -160.7812500020484094 ) ) ;
#18049 = VECTOR ( 'NONE', #37022, 1000.000000000000000 ) ;
#18050 = CYLINDRICAL_SURFACE ( 'NONE', #42652, 9.999999999999998224 ) ;
#18051 = CARTESIAN_POINT ( 'NONE',  ( 7.070501591499376803E-16, 11.54700538379251284, -172.6249999999999716 ) ) ;
#18052 = CARTESIAN_POINT ( 'NONE',  ( 10.81189881249999551, -6.242252689847874514, -100.4687500020483952 ) ) ;
#18053 = CARTESIAN_POINT ( 'NONE',  ( 9.999999999999479527, 5.773502691896553074, -42.75000000409674072 ) ) ;
#18054 = CARTESIAN_POINT ( 'NONE',  ( 10.00000000000000000, 5.773502691896255534, -72.37499999999997158 ) ) ;
#18055 = CARTESIAN_POINT ( 'NONE',  ( 7.644554776091147741E-16, 12.48450537969573659, -198.9687500020484094 ) ) ;
#18056 = CARTESIAN_POINT ( 'NONE',  ( 9.999999999999998224, 0.000000000000000000, -78.87500000409677625 ) ) ;
#18057 = EDGE_CURVE ( 'NONE', #8228, #12293, #6376, .T. ) ;
#18058 = CARTESIAN_POINT ( 'NONE',  ( 2.519142624249889106, -10.23978606567555083, -180.0000000000000000 ) ) ;
#18059 = CARTESIAN_POINT ( 'NONE',  ( -10.81189881249999729, 6.242252689847871849, -90.90625000204838102 ) ) ;
#18060 = CARTESIAN_POINT ( 'NONE',  ( 7.644554776091147741E-16, 12.48450537969573659, -76.15625000204838102 ) ) ;
#18061 = CARTESIAN_POINT ( 'NONE',  ( -4.999999999999996447, 8.660254037844387298, -69.37500000409677625 ) ) ;
#18062 = CARTESIAN_POINT ( 'NONE',  ( -9.999999999999998224, 1.224646799147353059E-15, -118.2500000000000000 ) ) ;
#18063 = CARTESIAN_POINT ( 'NONE',  ( -10.81189881249999907, -6.242252689847864744, -27.46875000204837391 ) ) ;
#18064 = ORIENTED_EDGE ( 'NONE', *, *, #37845, .T. ) ;
#18065 = CARTESIAN_POINT ( 'NONE',  ( 10.00000000000000000, 5.773502691896255534, -3.374999999999951594 ) ) ;
#18066 = CARTESIAN_POINT ( 'NONE',  ( -10.81189881249999729, 6.242252689847871849, -18.90625000204837391 ) ) ;
#18067 = CARTESIAN_POINT ( 'NONE',  ( -5.405949406249996869, 9.363379034771805109, -14.34375000204834905 ) ) ;
#18068 = CARTESIAN_POINT ( 'NONE',  ( -9.999999999999998224, 1.224646799147353059E-15, -119.7500000000000000 ) ) ;
#18069 = CARTESIAN_POINT ( 'NONE',  ( -9.999999999999998224, 1.224646799147353059E-15, -3.125000004096767370 ) ) ;
#18070 = CARTESIAN_POINT ( 'NONE',  ( -23.09401076758503280, 0.000000000000000000, 0.000000000000000000 ) ) ;
#18071 = CARTESIAN_POINT ( 'NONE',  ( -5.405949406250003975, -9.363379034771801557, -129.5312500020484094 ) ) ;
#18072 = VECTOR ( 'NONE', #32127, 1000.000000000000000 ) ;
#18073 =( BOUNDED_CURVE ( )  B_SPLINE_CURVE ( 2, ( #40541, #4314, #36477, #33892, #36687, #7342, #16601 ),
 .UNSPECIFIED., .F., .F. ) 
 B_SPLINE_CURVE_WITH_KNOTS ( ( 3, 2, 2, 3 ),
 ( 0.5261194029850747578, 0.5273631840796021431, 0.5286069651741294173, 0.5298507462686568026 ),
 .UNSPECIFIED. ) 
 CURVE ( )  GEOMETRIC_REPRESENTATION_ITEM ( )  RATIONAL_B_SPLINE_CURVE ( ( 0.9999999999999880096, 0.8660254037844506980, 1.000000000000000000, 0.8660254037844387076, 1.000000000000000000, 0.8660254037844267172, 1.000000000000011990 ) ) 
 REPRESENTATION_ITEM ( '' )  );
#18074 = CARTESIAN_POINT ( 'NONE',  ( 9.999999999999998224, 0.000000000000000000, -185.0000000000000000 ) ) ;
#18075 = CARTESIAN_POINT ( 'NONE',  ( 9.999999999999998224, 0.000000000000000000, -152.3750000040967905 ) ) ;
#18077 = ORIENTED_EDGE ( 'NONE', *, *, #22874, .F. ) ;
#18076 = CARTESIAN_POINT ( 'NONE',  ( 7.644554776091147741E-16, 12.48450537969573659, -106.1562500020483952 ) ) ;
#18078 = CARTESIAN_POINT ( 'NONE',  ( 5.000000000000000000, 8.660254037844385522, -195.2500000000000000 ) ) ;
#18079 = EDGE_LOOP ( 'NONE', ( #9904, #26028, #12211, #1808 ) ) ;
#18080 = ORIENTED_EDGE ( 'NONE', *, *, #22649, .F. ) ;
#18081 = CARTESIAN_POINT ( 'NONE',  ( 10.81189881249999907, 6.242252689847868297, -40.40625000204836681 ) ) ;
#18082 = DATE_TIME_ROLE ( 'creation_date' ) ;
#18083 = EDGE_CURVE ( 'NONE', #2342, #30674, #10765, .T. ) ;
#18084 = CARTESIAN_POINT ( 'NONE',  ( -10.81189881249999729, 6.242252689847871849, -86.21875000204838102 ) ) ;
#18085 = FACE_OUTER_BOUND ( 'NONE', #8008, .T. ) ;
#18086 = CARTESIAN_POINT ( 'NONE',  ( -9.999999999999998224, 1.224646799147353059E-15, -129.1250000040967620 ) ) ;
#18087 = CARTESIAN_POINT ( 'NONE',  ( -9.999999999999998224, 1.224646799147353059E-15, -169.6250000040967905 ) ) ;
#18088 = CARTESIAN_POINT ( 'NONE',  ( -10.81189881249999729, 6.242252689847871849, -165.9062500020483810 ) ) ;
#18089 = CARTESIAN_POINT ( 'NONE',  ( 9.999999999999998224, 0.000000000000000000, -67.99999999999997158 ) ) ;
#18090 = CARTESIAN_POINT ( 'NONE',  ( -5.405949406250003975, -9.363379034771801557, -123.3437500020483952 ) ) ;
#18091 = CARTESIAN_POINT ( 'NONE',  ( 10.81189881249999907, 6.242252689847868297, -83.71875000204836681 ) ) ;
#18092 = LINE ( 'NONE', #31287, #7478 ) ;
#18093 = CARTESIAN_POINT ( 'NONE',  ( -10.81189881249999907, -6.242252689847864744, -192.4687500020484094 ) ) ;
#18094 = CARTESIAN_POINT ( 'NONE',  ( 10.81189881249999729, 0.000000000000000000, -91.53125000204838102 ) ) ;
#18095 = CARTESIAN_POINT ( 'NONE',  ( -5.000000000000003553, -8.660254037844383745, -178.3750000040967905 ) ) ;
#18096 = CARTESIAN_POINT ( 'NONE',  ( 5.405949406249992428, -9.363379034771808662, -168.2812500020484094 ) ) ;
#18097 = CARTESIAN_POINT ( 'NONE',  ( -2.121150477449813534E-15, -11.54700538379251284, -1.250000004096749384 ) ) ;
#18098 = CARTESIAN_POINT ( 'NONE',  ( 7.644554776091147741E-16, 12.48450537969573659, -178.1562500020484094 ) ) ;
#18099 = CARTESIAN_POINT ( 'NONE',  ( 5.405949406249999534, 9.363379034771803333, -187.2812500020484094 ) ) ;
#18100 = CARTESIAN_POINT ( 'NONE',  ( 10.81189881249999729, 6.242252689847867408, -52.21875000204837391 ) ) ;
#18101 = CARTESIAN_POINT ( 'NONE',  ( -2.121150477449813534E-15, -11.54700538379251284, -161.7500000040967620 ) ) ;
#18102 = CARTESIAN_POINT ( 'NONE',  ( -5.405949406250003975, -9.363379034771801557, -9.531250002048352599 ) ) ;
#18103 = CARTESIAN_POINT ( 'NONE',  ( -2.293366432827344421E-15, -12.48450537969573659, -16.71875000204836681 ) ) ;
#18104 = CARTESIAN_POINT ( 'NONE',  ( -9.999999999999998224, 1.224646799147353059E-15, -159.1250000040967905 ) ) ;
#18105 = CARTESIAN_POINT ( 'NONE',  ( 10.81189881249999729, 0.000000000000000000, -124.3437500020483952 ) ) ;
#18106 = CARTESIAN_POINT ( 'NONE',  ( -2.121150477449813534E-15, -11.54700538379251284, -99.87500000000000000 ) ) ;
#18107 = CARTESIAN_POINT ( 'NONE',  ( -10.81189881249999907, -6.242252689847864744, -21.65625000204838102 ) ) ;
#18108 = CARTESIAN_POINT ( 'NONE',  ( -9.999999999999998224, 5.773502691896259087, -109.7500000040967763 ) ) ;
#18109 = LINE ( 'NONE', #41832, #29328 ) ;
#18110 = CARTESIAN_POINT ( 'NONE',  ( 4.999999999999992006, -8.660254037844389075, -50.24999999999998579 ) ) ;
#18111 = CARTESIAN_POINT ( 'NONE',  ( 10.81189881249999907, 6.242252689847868297, -112.4062500020483952 ) ) ;
#18112 = CARTESIAN_POINT ( 'NONE',  ( 10.81189881249999551, -6.242252689847874514, -100.6562500020483952 ) ) ;
#18113 = ORIENTED_EDGE ( 'NONE', *, *, #21754, .F. ) ;
#18114 = CARTESIAN_POINT ( 'NONE',  ( 4.999999999999992006, -8.660254037844389075, -100.1250000040967905 ) ) ;
#18115 = DIRECTION ( 'NONE',  ( -0.000000000000000000, -0.000000000000000000, 1.000000000000000000 ) ) ;
#18116 = CARTESIAN_POINT ( 'NONE',  ( -10.81189881249999907, -6.242252689847864744, -168.6562500020483810 ) ) ;
#18117 = CARTESIAN_POINT ( 'NONE',  ( -5.405949406250003975, -9.363379034771801557, -46.84375000204838102 ) ) ;
#18118 = ORIENTED_EDGE ( 'NONE', *, *, #21578, .T. ) ;
#18119 = CARTESIAN_POINT ( 'NONE',  ( 9.999999999999996447, -5.773502691896262640, -21.62499999999997158 ) ) ;
#18120 = CARTESIAN_POINT ( 'NONE',  ( 5.405949406249992428, -9.363379034771808662, -25.78125000204836681 ) ) ;
#18121 = CARTESIAN_POINT ( 'NONE',  ( -5.000000000000003553, -8.660254037844383745, -164.5000000000000000 ) ) ;
#18122 = CARTESIAN_POINT ( 'NONE',  ( -2.121150477449813534E-15, -11.54700538379251284, -102.8749999999999858 ) ) ;
#18123 = CARTESIAN_POINT ( 'NONE',  ( -2.121150477449813534E-15, -11.54700538379251284, -29.75000000409674783 ) ) ;
#18124 = FACE_OUTER_BOUND ( 'NONE', #19356, .T. ) ;
#18125 = CARTESIAN_POINT ( 'NONE',  ( 7.644554776091147741E-16, 12.48450537969573659, -134.6562500020483810 ) ) ;
#18126 = CARTESIAN_POINT ( 'NONE',  ( 6.220988656785935156, 8.439441497390092195, -8.678191841965558546E-15 ) ) ;
#18127 = CARTESIAN_POINT ( 'NONE',  ( -5.000000000000003553, -8.660254037844383745, -188.5000000000000000 ) ) ;
#18128 = VERTEX_POINT ( 'NONE', #26144 ) ;
#18129 = CARTESIAN_POINT ( 'NONE',  ( -10.81189881249999729, 1.324075727343319199E-15, -60.78125000204836681 ) ) ;
#18130 = ADVANCED_FACE ( 'NONE', ( #35447 ), #29176, .T. ) ;
#18131 = PERSON_AND_ORGANIZATION_ROLE ( 'design_supplier' ) ;
#18133 = ORIENTED_EDGE ( 'NONE', *, *, #18202, .T. ) ;
#18132 = ORIENTED_EDGE ( 'NONE', *, *, #23049, .F. ) ;
#18134 = FACE_OUTER_BOUND ( 'NONE', #7739, .T. ) ;
#18135 = PLANE ( 'NONE',  #15276 ) ;
#18136 = CARTESIAN_POINT ( 'NONE',  ( -10.81189881249999729, 6.242252689847871849, -156.7187500020483810 ) ) ;
#18137 = CARTESIAN_POINT ( 'NONE',  ( -2.293366432827344421E-15, -12.48450537969573659, -184.9062500020484094 ) ) ;
#18138 = CARTESIAN_POINT ( 'NONE',  ( 7.644554776091147741E-16, 12.48450537969573659, -8.468750002048357928 ) ) ;
#18139 = CARTESIAN_POINT ( 'NONE',  ( 9.999999999999998224, 0.000000000000000000, -42.87500000409677625 ) ) ;
#18140 = CARTESIAN_POINT ( 'NONE',  ( 10.81189881249999551, -6.242252689847874514, -149.9687500020483810 ) ) ;
#18141 = CARTESIAN_POINT ( 'NONE',  ( 7.644554776091147741E-16, 12.48450537969573659, -107.6562500020483810 ) ) ;
#18142 = CARTESIAN_POINT ( 'NONE',  ( -2.293366432827344421E-15, -12.48450537969573659, -109.7187500020483668 ) ) ;
#18143 = CARTESIAN_POINT ( 'NONE',  ( -9.999999999999998224, 1.224646799147353059E-15, -144.1250000040967905 ) ) ;
#18144 = CARTESIAN_POINT ( 'NONE',  ( -2.293366432827344421E-15, -12.48450537969573659, -120.4062500020483952 ) ) ;
#18145 = CARTESIAN_POINT ( 'NONE',  ( -5.405949406250003975, -9.363379034771801557, -1.843750002048366587 ) ) ;
#18147 = EDGE_CURVE ( 'NONE', #14397, #1637, #1563, .T. ) ;
#18146 = CARTESIAN_POINT ( 'NONE',  ( -10.81189881249999729, 6.242252689847871849, -131.2187500020483810 ) ) ;
#18148 = CARTESIAN_POINT ( 'NONE',  ( -5.405949406249996869, 9.363379034771805109, -196.0312500020484094 ) ) ;
#18149 = CARTESIAN_POINT ( 'NONE',  ( -9.999999999999998224, 1.224646799147353059E-15, -11.74999999999995559 ) ) ;
#18150 = CARTESIAN_POINT ( 'NONE',  ( -10.00000000000000000, -5.773502691896251982, -146.6249999999999716 ) ) ;
#18151 = CARTESIAN_POINT ( 'NONE',  ( 7.070501591499377789E-16, 11.54700538379251284, -13.62499999999996980 ) ) ;
#18152 = CARTESIAN_POINT ( 'NONE',  ( 10.81189881249999729, 6.242252689847867408, -77.71875000204838102 ) ) ;
#18153 = CARTESIAN_POINT ( 'NONE',  ( -2.293366432827344421E-15, -12.48450537969573659, -58.71875000204836681 ) ) ;
#18154 = CARTESIAN_POINT ( 'NONE',  ( 7.070501591499377789E-16, 11.54700538379251284, -185.0000000040967905 ) ) ;
#18155 = CARTESIAN_POINT ( 'NONE',  ( -5.405949406249996869, 9.363379034771805109, -37.03125000204837391 ) ) ;
#18156 = CARTESIAN_POINT ( 'NONE',  ( 5.405949406249992428, -9.363379034771808662, -39.09375000204837391 ) ) ;
#18157 = CARTESIAN_POINT ( 'NONE',  ( 5.000000000000000000, 8.660254037844385522, -136.7499999999999716 ) ) ;
#18158 = CARTESIAN_POINT ( 'NONE',  ( 10.81189881249999729, 0.000000000000000000, -148.3437500020483810 ) ) ;
#18159 = CARTESIAN_POINT ( 'NONE',  ( 4.999999999999992006, -8.660254037844389075, -125.2500000000000000 ) ) ;
#18160 =( BOUNDED_CURVE ( )  B_SPLINE_CURVE ( 2, ( #41036, #8484, #11479, #21416, #5240, #1800, #28770 ),
 .UNSPECIFIED., .F., .F. ) 
 B_SPLINE_CURVE_WITH_KNOTS ( ( 3, 2, 2, 3 ),
 ( 0.3097014925373136052, 0.3109452736318408794, 0.3121890547263682092, 0.3134328358208955390 ),
 .UNSPECIFIED. ) 
 CURVE ( )  GEOMETRIC_REPRESENTATION_ITEM ( )  RATIONAL_B_SPLINE_CURVE ( ( 0.9999999999999820144, 0.8660254037844566932, 1.000000000000000000, 0.8660254037844387076, 1.000000000000000000, 0.8660254037844387076, 1.000000000000000000 ) ) 
 REPRESENTATION_ITEM ( '' )  );
#18161 = CARTESIAN_POINT ( 'NONE',  ( -2.121150477449813534E-15, -11.54700538379251284, -170.3750000000000000 ) ) ;
#18162 = CARTESIAN_POINT ( 'NONE',  ( 10.00000000000000000, 5.773502691896255534, -76.87499999999997158 ) ) ;
#18163 = CARTESIAN_POINT ( 'NONE',  ( -10.81189881249999729, 1.324075727343319199E-15, -6.781250002048377468 ) ) ;
#18164 = ORIENTED_EDGE ( 'NONE', *, *, #19331, .F. ) ;
#18165 = CARTESIAN_POINT ( 'NONE',  ( -10.81189881249999729, 6.242252689847871849, -102.9062500020483952 ) ) ;
#18166 = CARTESIAN_POINT ( 'NONE',  ( -10.00000000000000000, -5.773502691896251982, -127.5000000040967905 ) ) ;
#18167 = CARTESIAN_POINT ( 'NONE',  ( -9.999999999999479527, -5.773502691896549521, -144.0000000040967620 ) ) ;
#18168 = CARTESIAN_POINT ( 'NONE',  ( 10.81189881249999729, 0.000000000000000000, -80.84375000204838102 ) ) ;
#18169 = CARTESIAN_POINT ( 'NONE',  ( 9.999999999999998224, 0.000000000000000000, -32.37500000409676204 ) ) ;
#18170 = CARTESIAN_POINT ( 'NONE',  ( 9.999999999999998224, 0.000000000000000000, -200.0000000000000000 ) ) ;
#18171 = CARTESIAN_POINT ( 'NONE',  ( 10.81189881249999551, -6.242252689847874514, -42.15625000204836681 ) ) ;
#18172 = EDGE_CURVE ( 'NONE', #1637, #14397, #25684, .T. ) ;
#18173 = DIRECTION ( 'NONE',  ( -0.000000000000000000, -0.000000000000000000, 1.000000000000000000 ) ) ;
#18174 = CARTESIAN_POINT ( 'NONE',  ( 5.405949406249992428, -9.363379034771808662, -145.7812500020483810 ) ) ;
#18175 = EDGE_CURVE ( 'NONE', #19929, #18454, #5453, .T. ) ;
#18176 = CARTESIAN_POINT ( 'NONE',  ( -10.81189881249999729, 1.324075727343319199E-15, -128.0937500020483810 ) ) ;
#18177 = DIRECTION ( 'NONE',  ( -0.000000000000000000, -0.000000000000000000, 1.000000000000000000 ) ) ;
#18178 = CARTESIAN_POINT ( 'NONE',  ( -5.000000000000003553, -8.660254037844383745, -121.0000000000000000 ) ) ;
#18179 = ORIENTED_EDGE ( 'NONE', *, *, #40656, .T. ) ;
#18180 = EDGE_CURVE ( 'NONE', #15306, #38211, #25173, .T. ) ;
#18181 = ORIENTED_EDGE ( 'NONE', *, *, #9949, .F. ) ;
#18182 = EDGE_LOOP ( 'NONE', ( #30074, #35294, #8158, #27109 ) ) ;
#18183 =( BOUNDED_CURVE ( )  B_SPLINE_CURVE ( 2, ( #15314, #12698, #41641, #25893, #12077, #9485, #22653 ),
 .UNSPECIFIED., .F., .F. ) 
 B_SPLINE_CURVE_WITH_KNOTS ( ( 3, 2, 2, 3 ),
 ( 0.8843283582089555006, 0.8855721393034827749, 0.8868159203980102712, 0.8880597014925376564 ),
 .UNSPECIFIED. ) 
 CURVE ( )  GEOMETRIC_REPRESENTATION_ITEM ( )  RATIONAL_B_SPLINE_CURVE ( ( 0.9999999999999761302, 0.8660254037844625774, 1.000000000000000000, 0.8660254037844387076, 1.000000000000000000, 0.8660254037844028474, 1.000000000000035971 ) ) 
 REPRESENTATION_ITEM ( '' )  );
#18184 = PLANE ( 'NONE',  #29981 ) ;
#18185 = CARTESIAN_POINT ( 'NONE',  ( 10.81189881249999551, -6.242252689847874514, -184.4687500020483810 ) ) ;
#18186 = CARTESIAN_POINT ( 'NONE',  ( -10.81189881249999907, -6.242252689847864744, -40.96875000204834549 ) ) ;
#18187 = LINE ( 'NONE', #41048, #16354 ) ;
#18188 = CARTESIAN_POINT ( 'NONE',  ( -10.81189881249999729, 6.242252689847871849, -174.7187500020484379 ) ) ;
#18189 = CARTESIAN_POINT ( 'NONE',  ( -10.81189881249999729, 6.242252689847871849, -156.7187500020483810 ) ) ;
#18190 = CARTESIAN_POINT ( 'NONE',  ( -9.999999999999479527, -5.773502691896549521, -76.50000000409674783 ) ) ;
#18191 = CARTESIAN_POINT ( 'NONE',  ( -10.81189881249999729, 1.324075727343319199E-15, -132.5937500020483810 ) ) ;
#18192 = CARTESIAN_POINT ( 'NONE',  ( 10.81189881249999551, -6.242252689847874514, -138.1562500020484094 ) ) ;
#18193 = CARTESIAN_POINT ( 'NONE',  ( -10.81189881249999729, 6.242252689847871849, -158.2187500020483810 ) ) ;
#18194 = CARTESIAN_POINT ( 'NONE',  ( -9.999999999999998224, 1.224646799147353059E-15, -127.2499999999999716 ) ) ;
#18195 =( BOUNDED_CURVE ( )  B_SPLINE_CURVE ( 2, ( #30869, #27416, #18919, #35338, #40552, #4532, #32102 ),
 .UNSPECIFIED., .F., .F. ) 
 B_SPLINE_CURVE_WITH_KNOTS ( ( 3, 2, 2, 3 ),
 ( 0.4067164179104478250, 0.4079601990049751548, 0.4092039800995025400, 0.4104477611940299253 ),
 .UNSPECIFIED. ) 
 CURVE ( )  GEOMETRIC_REPRESENTATION_ITEM ( )  RATIONAL_B_SPLINE_CURVE ( ( 0.9999999999999940048, 0.8660254037844447028, 1.000000000000000000, 0.8660254037844387076, 1.000000000000000000, 0.8660254037844327124, 1.000000000000005995 ) ) 
 REPRESENTATION_ITEM ( '' )  );
#18196 = CARTESIAN_POINT ( 'NONE',  ( -4.999999999999996447, 8.660254037844387298, -169.5000000000000000 ) ) ;
#18197 = CARTESIAN_POINT ( 'NONE',  ( 10.00000000000000000, 5.773502691896255534, -169.8750000000000000 ) ) ;
#18198 = CARTESIAN_POINT ( 'NONE',  ( -5.405949406250003975, -9.363379034771801557, -78.34375000204838102 ) ) ;
#18199 = CARTESIAN_POINT ( 'NONE',  ( 9.999999999999998224, 0.000000000000000000, -135.5000000000000000 ) ) ;
#18200 = CARTESIAN_POINT ( 'NONE',  ( 10.81189881249999551, -6.242252689847874514, -61.65625000204838813 ) ) ;
#18201 = CARTESIAN_POINT ( 'NONE',  ( 9.999999999999998224, 0.000000000000000000, -64.99999999999997158 ) ) ;
#18202 = EDGE_CURVE ( 'NONE', #33493, #22601, #41136, .T. ) ;
#18203 = CARTESIAN_POINT ( 'NONE',  ( 5.405949406249992428, -9.363379034771808662, -177.0937500020484094 ) ) ;
#18204 = CARTESIAN_POINT ( 'NONE',  ( 10.81189881249999907, 6.242252689847868297, -110.9062500020483952 ) ) ;
#18205 = CARTESIAN_POINT ( 'NONE',  ( 10.81189881249999551, -6.242252689847874514, -154.6562500020484094 ) ) ;
#18206 = CARTESIAN_POINT ( 'NONE',  ( 4.999999999999992006, -8.660254037844389075, -11.24999999999995381 ) ) ;
#18207 = CARTESIAN_POINT ( 'NONE',  ( 5.405949406249992428, -9.363379034771808662, -46.78125000204838813 ) ) ;
#18208 = CARTESIAN_POINT ( 'NONE',  ( -10.00000000000000000, -5.773502691896251982, -132.0000000040967905 ) ) ;
#18209 = CARTESIAN_POINT ( 'NONE',  ( 9.999999999999998224, 0.000000000000000000, -102.5000000000000000 ) ) ;
#18210 = ORIENTED_EDGE ( 'NONE', *, *, #17633, .T. ) ;
#18211 =( BOUNDED_CURVE ( )  B_SPLINE_CURVE ( 2, ( #39408, #33383, #23662, #36390, #3597, #3377, #3802 ),
 .UNSPECIFIED., .F., .F. ) 
 B_SPLINE_CURVE_WITH_KNOTS ( ( 3, 2, 2, 3 ),
 ( 0.7910447761194031591, 0.7922885572139305443, 0.7935323383084578186, 0.7947761194029852039 ),
 .UNSPECIFIED. ) 
 CURVE ( )  GEOMETRIC_REPRESENTATION_ITEM ( )  RATIONAL_B_SPLINE_CURVE ( ( 0.9999999999999761302, 0.8660254037844625774, 1.000000000000000000, 0.8660254037844387076, 1.000000000000000000, 0.8660254037844267172, 1.000000000000011990 ) ) 
 REPRESENTATION_ITEM ( '' )  );
#18212 = CARTESIAN_POINT ( 'NONE',  ( 7.644554776091147741E-16, 12.48450537969573659, -125.6562500020483810 ) ) ;
#18213 = CARTESIAN_POINT ( 'NONE',  ( 7.070501591499377789E-16, 11.54700538379251284, -149.0000000040968189 ) ) ;
#18214 = DIRECTION ( 'NONE',  ( -1.000000000000000000, 0.000000000000000000, 0.000000000000000000 ) ) ;
#18215 = CARTESIAN_POINT ( 'NONE',  ( 10.81189881249999729, 0.000000000000000000, -181.5312500020483810 ) ) ;
#18216 = ORIENTED_EDGE ( 'NONE', *, *, #22997, .F. ) ;
#18217 = CARTESIAN_POINT ( 'NONE',  ( -10.81189881249999907, -6.242252689847864744, -172.9687500020484094 ) ) ;
#18218 = CARTESIAN_POINT ( 'NONE',  ( 10.00000000000000000, 5.773502691896255534, -59.25000000409676915 ) ) ;
#18219 = CARTESIAN_POINT ( 'NONE',  ( -9.999999999999998224, 1.224646799147353059E-15, -166.2500000000000000 ) ) ;
#18220 = CARTESIAN_POINT ( 'NONE',  ( 9.999999999999998224, 0.000000000000000000, -131.3750000040967905 ) ) ;
#18221 = CARTESIAN_POINT ( 'NONE',  ( 10.81189881249999551, -6.242252689847874514, -72.15625000204836681 ) ) ;
#18222 = CARTESIAN_POINT ( 'NONE',  ( -9.999999999999998224, 1.224646799147353059E-15, -40.62500000409677625 ) ) ;
#18223 = CARTESIAN_POINT ( 'NONE',  ( 10.81189881249999551, -6.242252689847874514, -4.468750002048355263 ) ) ;
#18224 = CARTESIAN_POINT ( 'NONE',  ( 5.500000000000003553, 20.00000000000000000, -232.0000000000000000 ) ) ;
#18225 = CARTESIAN_POINT ( 'NONE',  ( -10.81189881249999729, 1.324075727343319199E-15, -165.7812500020484094 ) ) ;
#18226 = CARTESIAN_POINT ( 'NONE',  ( 10.00000000000012257, -5.773502691896188921, -162.6250000000000568 ) ) ;
#18227 = CARTESIAN_POINT ( 'NONE',  ( -10.00000000000005329, 5.773502691896226224, -197.8750000000000000 ) ) ;
#18228 = ORIENTED_EDGE ( 'NONE', *, *, #11385, .F. ) ;
#18229 = DIRECTION ( 'NONE',  ( -0.5000000000000007772, 0.8660254037844381525, 0.000000000000000000 ) ) ;
#18230 = CARTESIAN_POINT ( 'NONE',  ( 9.999999999999998224, 0.000000000000000000, -105.8750000040967763 ) ) ;
#18231 = DIRECTION ( 'NONE',  ( -0.000000000000000000, -0.000000000000000000, 1.000000000000000000 ) ) ;
#18233 = VERTEX_POINT ( 'NONE', #26357 ) ;
#18232 = CARTESIAN_POINT ( 'NONE',  ( -5.405949406249996869, 9.363379034771805109, -80.53125000204838102 ) ) ;
#18234 =( NAMED_UNIT ( * ) SI_UNIT ( $, .STERADIAN. ) SOLID_ANGLE_UNIT ( ) );
#18236 = EDGE_LOOP ( 'NONE', ( #9014, #3664, #36344, #1807 ) ) ;
#18235 = DIRECTION ( 'NONE',  ( -0.000000000000000000, -0.000000000000000000, 1.000000000000000000 ) ) ;
#18237 = ORIENTED_EDGE ( 'NONE', *, *, #9293, .F. ) ;
#18238 = CARTESIAN_POINT ( 'NONE',  ( -2.293366432827344421E-15, -12.48450537969573659, -40.71875000204834549 ) ) ;
#18239 = CARTESIAN_POINT ( 'NONE',  ( -9.999999999999742428, -5.773502691896402084, -187.1250000000000000 ) ) ;
#18240 = CARTESIAN_POINT ( 'NONE',  ( 5.405949406249999534, 9.363379034771803333, -16.28125000204835970 ) ) ;
#18242 = ORIENTED_EDGE ( 'NONE', *, *, #3634, .F. ) ;
#18241 = CARTESIAN_POINT ( 'NONE',  ( 10.81189881249999551, -6.242252689847874514, -61.46875000204838102 ) ) ;
#18243 = CARTESIAN_POINT ( 'NONE',  ( -2.121150477449813534E-15, -11.54700538379251284, -109.2500000040967763 ) ) ;
#18244 = CARTESIAN_POINT ( 'NONE',  ( -2.121150477449813534E-15, -11.54700538379251284, -39.87499999999996447 ) ) ;
#18245 = CARTESIAN_POINT ( 'NONE',  ( -5.405949406250003975, -9.363379034771801557, -195.3437500020484094 ) ) ;
#18246 = CARTESIAN_POINT ( 'NONE',  ( -10.81189881249999729, 6.242252689847871849, -173.2187500020483810 ) ) ;
#18247 = CARTESIAN_POINT ( 'NONE',  ( -10.81189881249999729, 6.242252689847871849, -164.2187500020483810 ) ) ;
#18248 = CARTESIAN_POINT ( 'NONE',  ( -2.293366432827344421E-15, -12.48450537969573659, -178.7187500020484094 ) ) ;
#18249 = CARTESIAN_POINT ( 'NONE',  ( -9.999999999999998224, 1.224646799147353059E-15, -58.62500000409676204 ) ) ;
#18250 = CARTESIAN_POINT ( 'NONE',  ( 5.000000000000000000, 8.660254037844385522, -195.2500000000000000 ) ) ;
#18251 = EDGE_CURVE ( 'NONE', #35515, #5023, #1722, .T. ) ;
#18252 = CARTESIAN_POINT ( 'NONE',  ( -10.81189881249999729, 6.242252689847871849, -114.7187500020483810 ) ) ;
#18253 = CARTESIAN_POINT ( 'NONE',  ( -5.321294541346989426, 0.000000000000000000, -219.9999999999999716 ) ) ;
#18254 = CARTESIAN_POINT ( 'NONE',  ( 10.81189881249999907, 6.242252689847868297, -85.40625000204839523 ) ) ;
#18255 = EDGE_CURVE ( 'NONE', #10744, #34185, #2855, .T. ) ;
#18256 = CARTESIAN_POINT ( 'NONE',  ( 5.405949406249992428, -9.363379034771808662, -96.09375000204838102 ) ) ;
#18257 = CARTESIAN_POINT ( 'NONE',  ( 10.81189881249999907, 6.242252689847868297, -65.71875000204838102 ) ) ;
#18258 = EDGE_CURVE ( 'NONE', #13583, #25373, #7066, .T. ) ;
#18259 = CARTESIAN_POINT ( 'NONE',  ( 5.405949406249992428, -9.363379034771808662, -69.28125000204838102 ) ) ;
#18260 = CARTESIAN_POINT ( 'NONE',  ( -9.999999999999998224, 5.773502691896259087, -154.7500000040967620 ) ) ;
#18261 = CARTESIAN_POINT ( 'NONE',  ( -10.00000000000000000, -5.773502691896251982, -122.6250000000000000 ) ) ;
#18262 = CARTESIAN_POINT ( 'NONE',  ( -10.81189881249999729, 1.324075727343319199E-15, -147.7812500020483810 ) ) ;
#18263 = CARTESIAN_POINT ( 'NONE',  ( -10.81189881249999729, 6.242252689847871849, -162.9062500020484094 ) ) ;
#18264 = CARTESIAN_POINT ( 'NONE',  ( 9.999999999999998224, 0.000000000000000000, -98.37500000409677625 ) ) ;
#18265 = CARTESIAN_POINT ( 'NONE',  ( -2.121150477449813534E-15, -11.54700538379251284, -182.3750000000000000 ) ) ;
#18266 = CARTESIAN_POINT ( 'NONE',  ( 10.81189881249999729, 0.000000000000000000, -95.84375000204838102 ) ) ;
#18267 = ORIENTED_EDGE ( 'NONE', *, *, #29898, .T. ) ;
#18268 = CARTESIAN_POINT ( 'NONE',  ( 10.00000000000000000, 5.773502691896255534, -63.37499999999998579 ) ) ;
#18269 = CARTESIAN_POINT ( 'NONE',  ( 10.81189881249999907, 6.242252689847868297, -199.2187500020484094 ) ) ;
#18270 = CARTESIAN_POINT ( 'NONE',  ( 10.00000000000000000, 5.773502691896255534, -81.75000000409677625 ) ) ;
#18271 = CARTESIAN_POINT ( 'NONE',  ( 9.999999999998969713, 5.773502691896851502, -26.25000000409674783 ) ) ;
#18272 = CARTESIAN_POINT ( 'NONE',  ( 10.81189881249999551, -6.242252689847874514, -93.15625000204838102 ) ) ;
#18273 = CARTESIAN_POINT ( 'NONE',  ( -2.293366432827344421E-15, -12.48450537969573659, -76.90625000204839523 ) ) ;
#18274 = CARTESIAN_POINT ( 'NONE',  ( 7.070501591499377789E-16, 11.54700538379251284, -68.00000000409679046 ) ) ;
#18275 = FACE_OUTER_BOUND ( 'NONE', #24259, .T. ) ;
#18276 = CARTESIAN_POINT ( 'NONE',  ( 10.81189881249999551, -6.242252689847874514, -25.46875000204837391 ) ) ;
#18277 = ORIENTED_EDGE ( 'NONE', *, *, #28344, .T. ) ;
#18278 = CARTESIAN_POINT ( 'NONE',  ( 5.000000000000000000, 8.660254037844385522, -4.749999999999976907 ) ) ;
#18279 = CARTESIAN_POINT ( 'NONE',  ( 5.405949406249999534, 9.363379034771803333, -22.28125000204836326 ) ) ;
#18280 = CARTESIAN_POINT ( 'NONE',  ( -5.405949406249996869, 9.363379034771805109, -9.843750002048345493 ) ) ;
#18281 = CARTESIAN_POINT ( 'NONE',  ( -9.999999999999998224, 1.224646799147353059E-15, -120.1250000040967905 ) ) ;
#18282 = EDGE_CURVE ( 'NONE', #40199, #4599, #11910, .T. ) ;
#18283 = CARTESIAN_POINT ( 'NONE',  ( 5.405949406249992428, -9.363379034771808662, -141.0937500020483810 ) ) ;
#18284 =( BOUNDED_CURVE ( )  B_SPLINE_CURVE ( 2, ( #38227, #1560, #22256, #35426, #8672, #2202, #5854 ),
 .UNSPECIFIED., .F., .F. ) 
 B_SPLINE_CURVE_WITH_KNOTS ( ( 3, 2, 2, 3 ),
 ( 0.2089552238805970630, 0.2101990049751244205, 0.2114427860696518058, 0.2126865671641791633 ),
 .UNSPECIFIED. ) 
 CURVE ( )  GEOMETRIC_REPRESENTATION_ITEM ( )  RATIONAL_B_SPLINE_CURVE ( ( 0.9999999999999940048, 0.8660254037844447028, 1.000000000000000000, 0.8660254037844387076, 1.000000000000000000, 0.8660254037844327124, 1.000000000000005995 ) ) 
 REPRESENTATION_ITEM ( '' )  );
#18285 = CARTESIAN_POINT ( 'NONE',  ( -9.999999999999998224, 1.224646799147353059E-15, -109.2499999999999858 ) ) ;
#18286 = CARTESIAN_POINT ( 'NONE',  ( 9.999999999999998224, 0.000000000000000000, -134.0000000000000000 ) ) ;
#18287 = CARTESIAN_POINT ( 'NONE',  ( 10.81189881249999907, 6.242252689847868297, -130.4062500020483810 ) ) ;
#18288 = AXIS2_PLACEMENT_3D ( 'NONE', #29808, #39289, #23328 ) ;
#18289 = CARTESIAN_POINT ( 'NONE',  ( 9.999999999999996447, -5.773502691896262640, -183.6250000000000000 ) ) ;
#18290 = CARTESIAN_POINT ( 'NONE',  ( 9.999999999999998224, 0.000000000000000000, -35.37500000409676915 ) ) ;
#18292 = ORIENTED_EDGE ( 'NONE', *, *, #38102, .F. ) ;
#18291 = CARTESIAN_POINT ( 'NONE',  ( -5.405949406250003975, -9.363379034771801557, -105.5312500020483810 ) ) ;
#18293 = DIRECTION ( 'NONE',  ( -0.000000000000000000, -0.000000000000000000, 1.000000000000000000 ) ) ;
#18294 = EDGE_CURVE ( 'NONE', #7309, #5725, #39718, .T. ) ;
#18295 = ORIENTED_EDGE ( 'NONE', *, *, #18835, .F. ) ;
#18296 = ORIENTED_EDGE ( 'NONE', *, *, #31197, .F. ) ;
#18297 = CARTESIAN_POINT ( 'NONE',  ( -10.81189881249999907, -6.242252689847864744, -35.15625000204837391 ) ) ;
#18298 = PERSON_AND_ORGANIZATION ( #11915, #17965 ) ;
#18299 = CARTESIAN_POINT ( 'NONE',  ( -2.293366432827344421E-15, -12.48450537969573659, -90.21875000204838102 ) ) ;
#18300 = CARTESIAN_POINT ( 'NONE',  ( -9.999999999999998224, 1.224646799147353059E-15, -55.62500000409676204 ) ) ;
#18301 = CARTESIAN_POINT ( 'NONE',  ( 4.999999999999992006, -8.660254037844389075, -108.7499999999999858 ) ) ;
#18302 = VECTOR ( 'NONE', #4825, 1000.000000000000000 ) ;
#18303 = AXIS2_PLACEMENT_3D ( 'NONE', #39616, #36393, #41092 ) ;
#18304 = CARTESIAN_POINT ( 'NONE',  ( -4.999999999999996447, 8.660254037844387298, -156.3750000040967905 ) ) ;
#18305 = CARTESIAN_POINT ( 'NONE',  ( 10.81189881249999729, 0.000000000000000000, -163.5312500020484094 ) ) ;
#18306 = CARTESIAN_POINT ( 'NONE',  ( -9.999999999999998224, 1.224646799147353059E-15, -100.2499999999999858 ) ) ;
#18307 = CARTESIAN_POINT ( 'NONE',  ( -10.81189881249999729, 6.242252689847871849, -117.7187500020483952 ) ) ;
#18308 = VECTOR ( 'NONE', #8650, 1000.000000000000000 ) ;
#18309 = CARTESIAN_POINT ( 'NONE',  ( -2.293366432827344421E-15, -12.48450537969573659, -88.71875000204838102 ) ) ;
#18310 = CARTESIAN_POINT ( 'NONE',  ( -10.81189881249999729, 1.324075727343319199E-15, -5.281250002048376579 ) ) ;
#18311 = CARTESIAN_POINT ( 'NONE',  ( 5.405949406249999534, 9.363379034771803333, -194.5937500020484094 ) ) ;
#18312 = CARTESIAN_POINT ( 'NONE',  ( 10.81189881249999907, 6.242252689847868297, -92.90625000204839523 ) ) ;
#18313 = CARTESIAN_POINT ( 'NONE',  ( -4.999999999999996447, 8.660254037844387298, -180.3750000040967905 ) ) ;
#18314 = CARTESIAN_POINT ( 'NONE',  ( -10.81189881249999729, 1.324075727343319199E-15, -170.2812500020484094 ) ) ;
#18315 = EDGE_CURVE ( 'NONE', #16498, #15872, #19097, .T. ) ;
#18316 = CARTESIAN_POINT ( 'NONE',  ( 10.81189881249999729, 0.000000000000000000, -175.5312500020483810 ) ) ;
#18317 = CARTESIAN_POINT ( 'NONE',  ( -10.81189881249999729, 6.242252689847871849, -186.9062500020484094 ) ) ;
#18318 = CARTESIAN_POINT ( 'NONE',  ( 5.405949406249992428, -9.363379034771808662, -45.09375000204837391 ) ) ;
#18319 = ADVANCED_FACE ( 'NONE', ( #36909 ), #7355, .T. ) ;
#18320 = CARTESIAN_POINT ( 'NONE',  ( -10.00000000000000000, -5.773502691896251982, -165.0000000040967905 ) ) ;
#18321 = CARTESIAN_POINT ( 'NONE',  ( -5.405949406250003975, -9.363379034771801557, -5.031250002048376579 ) ) ;
#18322 = CARTESIAN_POINT ( 'NONE',  ( 5.405949406249999534, 9.363379034771803333, -14.59375000204835082 ) ) ;
#18323 = DIRECTION ( 'NONE',  ( -0.000000000000000000, -0.000000000000000000, 1.000000000000000000 ) ) ;
#18324 = CARTESIAN_POINT ( 'NONE',  ( -2.293366432827344421E-15, -12.48450537969573659, -120.2187500020483952 ) ) ;
#18325 = CARTESIAN_POINT ( 'NONE',  ( 9.999999999999998224, 0.000000000000000000, -100.9999999999999858 ) ) ;
#18326 = CARTESIAN_POINT ( 'NONE',  ( -10.81189881249999729, 6.242252689847871849, -17.40625000204837391 ) ) ;
#18327 = CARTESIAN_POINT ( 'NONE',  ( -5.000000000000003553, -8.660254037844383745, -109.3750000040967763 ) ) ;
#18328 = DIRECTION ( 'NONE',  ( -0.000000000000000000, -0.000000000000000000, 1.000000000000000000 ) ) ;
#18329 = CARTESIAN_POINT ( 'NONE',  ( -4.999999999999996447, 8.660254037844387298, -52.49999999999996447 ) ) ;
#18330 = CARTESIAN_POINT ( 'NONE',  ( -2.293366432827344421E-15, -12.48450537969573659, -117.4062500020483952 ) ) ;
#18331 = CARTESIAN_POINT ( 'NONE',  ( -2.293366432827344421E-15, -12.48450537969573659, -102.4062500020484094 ) ) ;
#18332 = ORIENTED_EDGE ( 'NONE', *, *, #36970, .F. ) ;
#18333 =( BOUNDED_CURVE ( )  B_SPLINE_CURVE ( 2, ( #9674, #19381, #36009, #22632, #19588, #25665, #35805 ),
 .UNSPECIFIED., .F., .F. ) 
 B_SPLINE_CURVE_WITH_KNOTS ( ( 3, 2, 2, 3 ),
 ( 0.6902985074626868389, 0.6915422885572141132, 0.6927860696517414985, 0.6940298507462688837 ),
 .UNSPECIFIED. ) 
 CURVE ( )  GEOMETRIC_REPRESENTATION_ITEM ( )  RATIONAL_B_SPLINE_CURVE ( ( 0.9999999999999761302, 0.8660254037844625774, 1.000000000000000000, 0.8660254037844387076, 1.000000000000000000, 0.8660254037844148378, 1.000000000000023981 ) ) 
 REPRESENTATION_ITEM ( '' )  );
#18334 = CARTESIAN_POINT ( 'NONE',  ( -9.999999999999998224, 5.773502691896259087, -94.75000000409677625 ) ) ;
#18335 = CARTESIAN_POINT ( 'NONE',  ( 9.999999999999479527, 5.773502691896553074, -91.87499999999998579 ) ) ;
#18336 = CARTESIAN_POINT ( 'NONE',  ( 10.81189881249999551, -6.242252689847874514, -157.6562500020484094 ) ) ;
#18337 = CARTESIAN_POINT ( 'NONE',  ( -10.81189881249999907, -6.242252689847864744, -52.96875000204837391 ) ) ;
#18338 = ORIENTED_EDGE ( 'NONE', *, *, #6321, .F. ) ;
#18339 = CARTESIAN_POINT ( 'NONE',  ( 9.999999999999998224, 0.000000000000000000, -24.49999999999996447 ) ) ;
#18340 = CARTESIAN_POINT ( 'NONE',  ( 7.644554776091147741E-16, 12.48450537969573659, -26.65625000204837747 ) ) ;
#18341 = CARTESIAN_POINT ( 'NONE',  ( 4.999999999999992006, -8.660254037844389075, -159.7500000000000000 ) ) ;
#18342 = DIRECTION ( 'NONE',  ( -0.000000000000000000, -0.000000000000000000, 1.000000000000000000 ) ) ;
#18343 = CARTESIAN_POINT ( 'NONE',  ( 10.00000000000000000, 5.773502691896255534, -23.25000000409676915 ) ) ;
#18344 = AXIS2_PLACEMENT_3D ( 'NONE', #9700, #7, #36038 ) ;
#18345 = EDGE_CURVE ( 'NONE', #30831, #38366, #23519, .T. ) ;
#18346 = CARTESIAN_POINT ( 'NONE',  ( -9.999999999999998224, 1.224646799147353059E-15, -81.12500000409677625 ) ) ;
#18347 = CARTESIAN_POINT ( 'NONE',  ( 10.81189881249999551, -6.242252689847874514, -133.6562500020483810 ) ) ;
#18348 = CARTESIAN_POINT ( 'NONE',  ( -9.999999999999998224, 1.224646799147353059E-15, -139.6250000040967905 ) ) ;
#18349 = DIRECTION ( 'NONE',  ( -0.000000000000000000, -0.000000000000000000, -1.000000000000000000 ) ) ;
#18350 = VERTEX_POINT ( 'NONE', #1953 ) ;
#18351 = CARTESIAN_POINT ( 'NONE',  ( 5.405949406249999534, 9.363379034771803333, -58.28125000204836681 ) ) ;
#18352 = APPROVAL_DATE_TIME ( #5196, #40192 ) ;
#18354 = ORIENTED_EDGE ( 'NONE', *, *, #35728, .T. ) ;
#18353 = ORIENTED_EDGE ( 'NONE', *, *, #29097, .F. ) ;
#18355 = CARTESIAN_POINT ( 'NONE',  ( 4.999999999999992006, -8.660254037844389075, -46.12500000409677625 ) ) ;
#18356 = CARTESIAN_POINT ( 'NONE',  ( -4.999999999999996447, 8.660254037844387298, -171.0000000000000000 ) ) ;
#18357 = CARTESIAN_POINT ( 'NONE',  ( 5.405949406249999534, 9.363379034771803333, -160.0937500020484094 ) ) ;
#18358 = CARTESIAN_POINT ( 'NONE',  ( -2.293366432827344421E-15, -12.48450537969573659, -192.4062500020484094 ) ) ;
#18359 = CARTESIAN_POINT ( 'NONE',  ( 5.405949406249999534, 9.363379034771803333, -4.093750002048368586 ) ) ;
#18360 = CARTESIAN_POINT ( 'NONE',  ( -10.81189881249999729, -6.242252689847864744, -136.9687500020483810 ) ) ;
#18361 = CARTESIAN_POINT ( 'NONE',  ( 10.81189881249999907, 6.242252689847868297, -101.9062500020484094 ) ) ;
#18362 = CARTESIAN_POINT ( 'NONE',  ( -5.405949406250003975, -9.363379034771801557, -106.8437500020483810 ) ) ;
#18363 = DIRECTION ( 'NONE',  ( -0.000000000000000000, -0.000000000000000000, 1.000000000000000000 ) ) ;
#18364 = VECTOR ( 'NONE', #1447, 1000.000000000000000 ) ;
#18365 = CARTESIAN_POINT ( 'NONE',  ( 10.81189881249999729, 0.000000000000000000, -118.5312500020483952 ) ) ;
#18366 = CARTESIAN_POINT ( 'NONE',  ( 10.81189881249999907, 6.242252689847868297, -4.218750002048367698 ) ) ;
#18367 = CARTESIAN_POINT ( 'NONE',  ( -10.81189881249999729, 6.242252689847871849, -123.7187500020483952 ) ) ;
#18368 = CARTESIAN_POINT ( 'NONE',  ( 5.405949406249992428, -9.363379034771808662, -195.2812500020484094 ) ) ;
#18369 = CARTESIAN_POINT ( 'NONE',  ( -9.999999999999479527, -5.773502691896549521, -6.000000004096727402 ) ) ;
#18370 = CARTESIAN_POINT ( 'NONE',  ( 4.999999999999992006, -8.660254037844389075, -149.2500000000000000 ) ) ;
#18371 = CARTESIAN_POINT ( 'NONE',  ( -2.121150477449813534E-15, -11.54700538379251284, -9.874999999999966249 ) ) ;
#18372 = CARTESIAN_POINT ( 'NONE',  ( 10.81189881249999729, 0.000000000000000000, -73.34375000204838102 ) ) ;
#18373 = CARTESIAN_POINT ( 'NONE',  ( 10.81189881249999729, 0.000000000000000000, -56.84375000204835970 ) ) ;
#18374 = CARTESIAN_POINT ( 'NONE',  ( -9.999999999999998224, 1.224646799147353059E-15, -190.6250000040967905 ) ) ;
#18375 = CARTESIAN_POINT ( 'NONE',  ( -10.81189881249999907, -6.242252689847864744, -38.15625000204835260 ) ) ;
#18376 = CARTESIAN_POINT ( 'NONE',  ( -2.293366432827344421E-15, -12.48450537969573659, -34.71875000204835260 ) ) ;
#18377 = CARTESIAN_POINT ( 'NONE',  ( 5.000000000000000000, 8.660254037844385522, -53.12500000409675494 ) ) ;
#18378 = CARTESIAN_POINT ( 'NONE',  ( 10.81189881249999907, 6.242252689847868297, -148.2187500020484094 ) ) ;
#18379 = CARTESIAN_POINT ( 'NONE',  ( -2.121150477449813534E-15, -11.54700538379251284, -122.3750000000000142 ) ) ;
#18380 = CARTESIAN_POINT ( 'NONE',  ( 5.000000000000000000, 8.660254037844385522, -145.7500000000000000 ) ) ;
#18381 = CARTESIAN_POINT ( 'NONE',  ( 4.999999999999992006, -8.660254037844389075, -74.24999999999998579 ) ) ;
#18382 = CARTESIAN_POINT ( 'NONE',  ( -5.405949406250003975, -9.363379034771801557, -140.0312500020484094 ) ) ;
#18383 = CARTESIAN_POINT ( 'NONE',  ( -2.293366432827344421E-15, -12.48450537969573659, -12.40625000204835793 ) ) ;
#18384 = ORIENTED_EDGE ( 'NONE', *, *, #24323, .T. ) ;
#18385 = CARTESIAN_POINT ( 'NONE',  ( 9.999999999999996447, -5.773502691896262640, -115.0000000040967763 ) ) ;
#18386 = CARTESIAN_POINT ( 'NONE',  ( 9.999999999999998224, 0.000000000000000000, -60.49999999999997158 ) ) ;
#18387 = CARTESIAN_POINT ( 'NONE',  ( -5.405949406249996869, 9.363379034771805109, -71.34375000204836681 ) ) ;
#18388 = EDGE_CURVE ( 'NONE', #3950, #31053, #28065, .T. ) ;
#18389 = CARTESIAN_POINT ( 'NONE',  ( -4.999999999999996447, 8.660254037844387298, -28.87500000409676204 ) ) ;
#18390 = PRODUCT ( 'reaction body', 'reaction body', '', ( #14182 ) ) ;
#18391 = DIRECTION ( 'NONE',  ( -0.000000000000000000, -0.000000000000000000, 1.000000000000000000 ) ) ;
#18392 = CARTESIAN_POINT ( 'NONE',  ( -2.293366432827344421E-15, -12.48450537969573659, -43.90625000204837391 ) ) ;
#18393 = CARTESIAN_POINT ( 'NONE',  ( 0.000000000000000000, 0.000000000000000000, -200.0000000000000000 ) ) ;
#18394 = CARTESIAN_POINT ( 'NONE',  ( 10.81189881249999907, 6.242252689847868297, -143.9062500020484094 ) ) ;
#18395 = CARTESIAN_POINT ( 'NONE',  ( 7.644554776091147741E-16, 12.48450537969573659, -125.4687500020483952 ) ) ;
#18396 = CARTESIAN_POINT ( 'NONE',  ( 9.999999999999612754, 5.773502691896477579, -153.3749999999999716 ) ) ;
#18397 = CARTESIAN_POINT ( 'NONE',  ( 9.999999999999998224, 0.000000000000000000, -0.4999999999999726885 ) ) ;
#18399 = EDGE_CURVE ( 'NONE', #9953, #36081, #36744, .T. ) ;
#18398 = ORIENTED_EDGE ( 'NONE', *, *, #13277, .F. ) ;
#18400 = VERTEX_POINT ( 'NONE', #1525 ) ;
#18401 = ORIENTED_EDGE ( 'NONE', *, *, #34286, .T. ) ;
#18402 = CARTESIAN_POINT ( 'NONE',  ( -9.999999999999998224, 1.224646799147353059E-15, -7.625000004096743389 ) ) ;
#18403 = CARTESIAN_POINT ( 'NONE',  ( -5.405949406249996869, 9.363379034771805109, -183.8437500020483810 ) ) ;
#18404 = CARTESIAN_POINT ( 'NONE',  ( -10.81189881249999729, 1.324075727343319199E-15, -32.09375000204836681 ) ) ;
#18405 = CARTESIAN_POINT ( 'NONE',  ( -5.000000000000003553, -8.660254037844383745, -130.3750000040967905 ) ) ;
#18406 = CARTESIAN_POINT ( 'NONE',  ( 5.405949406249992428, -9.363379034771808662, -171.0937500020484094 ) ) ;
#18407 = CARTESIAN_POINT ( 'NONE',  ( 10.81189881249999551, -6.242252689847874514, -149.9687500020483810 ) ) ;
#18408 = CARTESIAN_POINT ( 'NONE',  ( 9.999999999999998224, 0.000000000000000000, -200.0000000000000000 ) ) ;
#18409 = CARTESIAN_POINT ( 'NONE',  ( 10.81189881249999729, 0.000000000000000000, -130.3437500020484094 ) ) ;
#18410 = CARTESIAN_POINT ( 'NONE',  ( -10.81189881249999907, -6.242252689847864744, -138.6562500020484094 ) ) ;
#18411 = CARTESIAN_POINT ( 'NONE',  ( -10.81189881249999729, 6.242252689847871849, -150.7187500020483810 ) ) ;
#18412 = CARTESIAN_POINT ( 'NONE',  ( 9.999999999999998224, 1.224646799147353059E-15, -99.99999999999998579 ) ) ;
#18413 = CARTESIAN_POINT ( 'NONE',  ( -10.00000000000025580, 5.773502691896109873, -157.3750000000000000 ) ) ;
#18414 = CARTESIAN_POINT ( 'NONE',  ( -2.121150477449813534E-15, -11.54700538379251284, -174.8750000000000000 ) ) ;
#18415 = CARTESIAN_POINT ( 'NONE',  ( -5.405949406250003975, -9.363379034771801557, -82.84375000204836681 ) ) ;
#18416 = CARTESIAN_POINT ( 'NONE',  ( -10.00000000000001421, 5.773502691896249317, -198.2500000040967905 ) ) ;
#18417 = CARTESIAN_POINT ( 'NONE',  ( -2.293366432827344421E-15, -12.48450537969573659, -58.90625000204838813 ) ) ;
#18418 = CARTESIAN_POINT ( 'NONE',  ( -6.438708744581160381, -7.749506880439706258, -99.99999999999995737 ) ) ;
#18419 = CARTESIAN_POINT ( 'NONE',  ( -2.293366432827344421E-15, -12.48450537969573659, -169.7187500020483810 ) ) ;
#18420 = CARTESIAN_POINT ( 'NONE',  ( 10.81189881249999907, 6.242252689847868297, -115.4062500020484094 ) ) ;
#18421 = CARTESIAN_POINT ( 'NONE',  ( 7.644554776091147741E-16, 12.48450537969573659, -145.1562500020484094 ) ) ;
#18422 = CYLINDRICAL_SURFACE ( 'NONE', #26166, 9.999999999999998224 ) ;
#18423 = CARTESIAN_POINT ( 'NONE',  ( 5.405949406249992428, -9.363379034771808662, -45.28125000204838102 ) ) ;
#18424 = CARTESIAN_POINT ( 'NONE',  ( 9.999999999999996447, -5.773502691896262640, -119.5000000040967763 ) ) ;
#18425 = CARTESIAN_POINT ( 'NONE',  ( -10.00000000000000000, -5.773502691896251982, -100.1249999999999858 ) ) ;
#18426 = EDGE_CURVE ( 'NONE', #30416, #22978, #21143, .T. ) ;
#18427 = ORIENTED_EDGE ( 'NONE', *, *, #41255, .F. ) ;
#18428 = CARTESIAN_POINT ( 'NONE',  ( 5.405949406249999534, 9.363379034771803333, -128.7812500020483810 ) ) ;
#18429 = CARTESIAN_POINT ( 'NONE',  ( -9.999999999999998224, 1.224646799147353059E-15, -150.1250000040967905 ) ) ;
#18430 = CARTESIAN_POINT ( 'NONE',  ( 9.999999999999872102, 5.773502691896329253, -192.7500000040968473 ) ) ;
#18431 = CARTESIAN_POINT ( 'NONE',  ( 10.81189881249999729, 0.000000000000000000, -177.0312500020483810 ) ) ;
#18432 = ORIENTED_EDGE ( 'NONE', *, *, #6065, .T. ) ;
#18433 = CARTESIAN_POINT ( 'NONE',  ( 5.405949406249999534, 9.363379034771803333, -173.5937500020484094 ) ) ;
#18434 = CARTESIAN_POINT ( 'NONE',  ( -9.999999999999998224, 1.224646799147353059E-15, -49.62500000409675494 ) ) ;
#18435 = DIRECTION ( 'NONE',  ( 1.000000000000000000, 0.000000000000000000, 0.000000000000000000 ) ) ;
#18436 = CARTESIAN_POINT ( 'NONE',  ( -5.000000000000003553, -8.660254037844383745, -155.5000000000000000 ) ) ;
#18437 = CARTESIAN_POINT ( 'NONE',  ( -2.293366432827344421E-15, -12.48450537969573659, -66.40625000204838102 ) ) ;
#18438 = CARTESIAN_POINT ( 'NONE',  ( 4.999999999999992006, -8.660254037844389075, -43.12500000409677625 ) ) ;
#18439 = CARTESIAN_POINT ( 'NONE',  ( -10.81189881249999729, 1.324075727343319199E-15, -0.5937500020483654772 ) ) ;
#18440 = CARTESIAN_POINT ( 'NONE',  ( -4.999999999999996447, 8.660254037844387298, -83.99999999999997158 ) ) ;
#18441 = CARTESIAN_POINT ( 'NONE',  ( -10.81189881249999907, -6.242252689847864744, -168.6562500020483810 ) ) ;
#18442 = AXIS2_PLACEMENT_3D ( 'NONE', #9029, #42027, #31711 ) ;
#18443 = CARTESIAN_POINT ( 'NONE',  ( 9.999999999999998224, 0.000000000000000000, -2.375000004096766482 ) ) ;
#18444 = CARTESIAN_POINT ( 'NONE',  ( -2.121150477449813534E-15, -11.54700538379251284, -177.8750000000000000 ) ) ;
#18446 = ORIENTED_EDGE ( 'NONE', *, *, #6276, .F. ) ;
#18445 = EDGE_CURVE ( 'NONE', #33430, #33047, #4480, .T. ) ;
#18447 = CARTESIAN_POINT ( 'NONE',  ( -2.121150477449813534E-15, -11.54700538379251284, -0.8749999999999721334 ) ) ;
#18448 = CARTESIAN_POINT ( 'NONE',  ( -4.999999999999996447, 8.660254037844387298, -172.8750000040968189 ) ) ;
#18449 =( BOUNDED_CURVE ( )  B_SPLINE_CURVE ( 2, ( #21744, #5345, #2122, #15252, #40504, #10949, #6198 ),
 .UNSPECIFIED., .F., .F. ) 
 B_SPLINE_CURVE_WITH_KNOTS ( ( 3, 2, 2, 3 ),
 ( 0.1940298507462686894, 0.1952736318407960470, 0.1965174129353234322, 0.1977611940298507898 ),
 .UNSPECIFIED. ) 
 CURVE ( )  GEOMETRIC_REPRESENTATION_ITEM ( )  RATIONAL_B_SPLINE_CURVE ( ( 0.9999999999999970024, 0.8660254037844417052, 1.000000000000000000, 0.8660254037844387076, 1.000000000000000000, 0.8660254037844327124, 1.000000000000005995 ) ) 
 REPRESENTATION_ITEM ( '' )  );
#18450 = CARTESIAN_POINT ( 'NONE',  ( -9.999999999999998224, 1.224646799147353059E-15, -20.74999999999996447 ) ) ;
#18452 = ORIENTED_EDGE ( 'NONE', *, *, #13647, .F. ) ;
#18451 = CARTESIAN_POINT ( 'NONE',  ( 10.81189881249999729, 0.000000000000000000, -78.03125000204838102 ) ) ;
#18453 = ORIENTED_EDGE ( 'NONE', *, *, #11974, .F. ) ;
#18454 = VERTEX_POINT ( 'NONE', #27631 ) ;
#18455 = CARTESIAN_POINT ( 'NONE',  ( -10.81189881249999729, -6.242252689847864744, -34.96875000204835260 ) ) ;
#18457 = CARTESIAN_POINT ( 'NONE',  ( 9.999999999999994671, -5.773502691896262640, -170.5000000040967905 ) ) ;
#18456 =( BOUNDED_CURVE ( )  B_SPLINE_CURVE ( 2, ( #39698, #41925, #28581, #32242, #35481, #16807, #13143 ),
 .UNSPECIFIED., .F., .F. ) 
 B_SPLINE_CURVE_WITH_KNOTS ( ( 3, 2, 2, 3 ),
 ( 0.4216417910447762818, 0.4228855721393036671, 0.4241293532338309413, 0.4253731343283583266 ),
 .UNSPECIFIED. ) 
 CURVE ( )  GEOMETRIC_REPRESENTATION_ITEM ( )  RATIONAL_B_SPLINE_CURVE ( ( 0.9999999999999820144, 0.8660254037844566932, 1.000000000000000000, 0.8660254037844387076, 1.000000000000000000, 0.8660254037844267172, 1.000000000000011990 ) ) 
 REPRESENTATION_ITEM ( '' )  );
#18458 = CARTESIAN_POINT ( 'NONE',  ( 5.405949406249999534, 9.363379034771803333, -8.781250002048352599 ) ) ;
#18460 = ORIENTED_EDGE ( 'NONE', *, *, #5480, .T. ) ;
#18459 = CARTESIAN_POINT ( 'NONE',  ( -5.405949406250003975, -9.363379034771801557, -55.84375000204835970 ) ) ;
#18461 = CARTESIAN_POINT ( 'NONE',  ( 0.000000000000000000, 0.000000000000000000, -99.99999999999998579 ) ) ;
#18462 = CARTESIAN_POINT ( 'NONE',  ( 9.999999999999996447, -5.773502691896262640, -38.12499999999997158 ) ) ;
#18463 = CARTESIAN_POINT ( 'NONE',  ( 10.81189881249999729, 0.000000000000000000, -196.3437500020484094 ) ) ;
#18464 = CARTESIAN_POINT ( 'NONE',  ( -10.81189881249999729, 6.242252689847871849, -180.7187500020483810 ) ) ;
#18465 = CARTESIAN_POINT ( 'NONE',  ( 10.81189881249999907, 6.242252689847868297, -160.2187500020483810 ) ) ;
#18466 = CARTESIAN_POINT ( 'NONE',  ( -10.81189881249999729, 1.324075727343319199E-15, -177.5937500020484094 ) ) ;
#18467 = CARTESIAN_POINT ( 'NONE',  ( 9.999999999998969713, 5.773502691896851502, -18.75000000409674428 ) ) ;
#18468 =( BOUNDED_CURVE ( )  B_SPLINE_CURVE ( 2, ( #34339, #40990, #36756, #41426, #11433, #24631, #14668 ),
 .UNSPECIFIED., .F., .F. ) 
 B_SPLINE_CURVE_WITH_KNOTS ( ( 3, 2, 2, 3 ),
 ( 0.8768656716417913000, 0.8781094527363186852, 0.8793532338308460705, 0.8805970149253734558 ),
 .UNSPECIFIED. ) 
 CURVE ( )  GEOMETRIC_REPRESENTATION_ITEM ( )  RATIONAL_B_SPLINE_CURVE ( ( 0.9999999999999761302, 0.8660254037844625774, 1.000000000000000000, 0.8660254037844387076, 1.000000000000000000, 0.8660254037844028474, 1.000000000000035971 ) ) 
 REPRESENTATION_ITEM ( '' )  );
#18469 = CARTESIAN_POINT ( 'NONE',  ( 9.999999999999998224, 0.000000000000000000, -144.5000000000000000 ) ) ;
#18470 = CARTESIAN_POINT ( 'NONE',  ( 9.999999999999998224, 0.000000000000000000, -197.0000000000000000 ) ) ;
#18471 = CARTESIAN_POINT ( 'NONE',  ( 10.81189881249999907, 6.242252689847868297, -104.7187500020483810 ) ) ;
#18472 = CARTESIAN_POINT ( 'NONE',  ( 0.000000000000000000, 0.000000000000000000, -200.0000000000000000 ) ) ;
#18473 = CONICAL_SURFACE ( 'NONE', #27441, 31.99999999999997158, 0.7853981633974447263 ) ;
#18474 = CARTESIAN_POINT ( 'NONE',  ( -5.405949406249996869, 9.363379034771805109, -80.53125000204838102 ) ) ;
#18475 = CARTESIAN_POINT ( 'NONE',  ( 10.81189881249999729, 0.000000000000000000, -95.84375000204838102 ) ) ;
#18476 = CARTESIAN_POINT ( 'NONE',  ( -2.293366432827344421E-15, -12.48450537969573659, -64.90625000204838102 ) ) ;
#18477 = CARTESIAN_POINT ( 'NONE',  ( 9.999999999999998224, 0.000000000000000000, -143.3750000040967905 ) ) ;
#18478 = CARTESIAN_POINT ( 'NONE',  ( -5.000000000000003553, -8.660254037844383745, -127.0000000000000000 ) ) ;
#18479 = ORIENTED_EDGE ( 'NONE', *, *, #31528, .T. ) ;
#18480 = CARTESIAN_POINT ( 'NONE',  ( 10.81189881249999551, -6.242252689847874514, -150.1562500020484094 ) ) ;
#18481 = CARTESIAN_POINT ( 'NONE',  ( 5.405949406249999534, 9.363379034771803333, -166.2812500020484094 ) ) ;
#18482 = CARTESIAN_POINT ( 'NONE',  ( -9.999999999999998224, 1.224646799147353059E-15, -40.24999999999997868 ) ) ;
#18483 = CARTESIAN_POINT ( 'NONE',  ( -9.999999999999996447, 5.773502691896259975, -172.3750000000000568 ) ) ;
#18484 = CARTESIAN_POINT ( 'NONE',  ( 10.81189881249999551, -6.242252689847874514, -97.46875000204838102 ) ) ;
#18485 = ORIENTED_EDGE ( 'NONE', *, *, #5390, .T. ) ;
#18486 = CARTESIAN_POINT ( 'NONE',  ( 7.070501591499377789E-16, 11.54700538379251284, -66.12500000000000000 ) ) ;
#18487 = CARTESIAN_POINT ( 'NONE',  ( -10.81189881249999907, -6.242252689847864744, -193.9687500020484094 ) ) ;
#18488 = CARTESIAN_POINT ( 'NONE',  ( -4.999999999999996447, 8.660254037844387298, -82.87500000409676204 ) ) ;
#18489 = CARTESIAN_POINT ( 'NONE',  ( -2.138652185739045919, -10.15658843976767400, -179.9999999999999716 ) ) ;
#18490 = CARTESIAN_POINT ( 'NONE',  ( -9.999999999999998224, 1.224646799147353059E-15, -106.6250000040967763 ) ) ;
#18491 = CARTESIAN_POINT ( 'NONE',  ( 5.405949406249992428, -9.363379034771808662, -94.78125000204838102 ) ) ;
#18492 = CARTESIAN_POINT ( 'NONE',  ( 5.405949406249992428, -9.363379034771808662, -72.28125000204838102 ) ) ;
#18493 = CARTESIAN_POINT ( 'NONE',  ( -5.000000000000003553, -8.660254037844383745, -70.37500000409677625 ) ) ;
#18494 = FACE_OUTER_BOUND ( 'NONE', #39052, .T. ) ;
#18495 = CARTESIAN_POINT ( 'NONE',  ( 10.81189881249999907, 6.242252689847868297, -23.71875000204837036 ) ) ;
#18496 = ORIENTED_EDGE ( 'NONE', *, *, #11870, .F. ) ;
#18497 = CARTESIAN_POINT ( 'NONE',  ( -5.405949406250003975, -9.363379034771801557, -194.0312500020484094 ) ) ;
#18498 = CARTESIAN_POINT ( 'NONE',  ( -10.81189881249999729, 1.324075727343319199E-15, -20.28125000204836326 ) ) ;
#18499 = CARTESIAN_POINT ( 'NONE',  ( -2.293366432827344421E-15, -12.48450537969573659, -4.718750002048370362 ) ) ;
#18500 = CARTESIAN_POINT ( 'NONE',  ( -5.000000000000003553, -8.660254037844383745, -118.3750000040967905 ) ) ;
#18501 = CARTESIAN_POINT ( 'NONE',  ( -5.405949406250003975, -9.363379034771801557, -145.8437500020483810 ) ) ;
#18502 = CARTESIAN_POINT ( 'NONE',  ( 9.999999999999834799, 5.773502691896347905, -192.3750000000000284 ) ) ;
#18503 = CARTESIAN_POINT ( 'NONE',  ( 23.09401076758504345, 1.040834085586084257E-14, 49.99999999999998579 ) ) ;
#18504 = CARTESIAN_POINT ( 'NONE',  ( -9.999999999999998224, 5.773502691896259087, -170.8750000000000000 ) ) ;
#18505 = CARTESIAN_POINT ( 'NONE',  ( 9.999999999999227285, 5.773502691896701400, -106.8749999999999432 ) ) ;
#18507 = EDGE_LOOP ( 'NONE', ( #28935, #31467, #22867, #41847 ) ) ;
#18506 = CARTESIAN_POINT ( 'NONE',  ( 10.81189881249999551, -6.242252689847874514, -100.6562500020483952 ) ) ;
#18508 = CARTESIAN_POINT ( 'NONE',  ( -4.999999999999996447, 8.660254037844387298, -169.8750000040967905 ) ) ;
#18509 = EDGE_CURVE ( 'NONE', #3542, #38155, #24192, .T. ) ;
#18510 = CONICAL_SURFACE ( 'NONE', #23327, 15.00000000000001421, 0.7853981633974469467 ) ;
#18511 = ORIENTED_EDGE ( 'NONE', *, *, #1167, .F. ) ;
#18512 = ADVANCED_FACE ( 'NONE', ( #27199 ), #4534, .F. ) ;
#18513 = VERTEX_POINT ( 'NONE', #21360 ) ;
#18514 = CARTESIAN_POINT ( 'NONE',  ( 10.81189881249999729, 0.000000000000000000, -28.53125000204837036 ) ) ;
#18515 = APPROVAL_DATE_TIME ( #40735, #9846 ) ;
#18516 = CARTESIAN_POINT ( 'NONE',  ( 10.81189881249999729, 0.000000000000000000, -88.34375000204838102 ) ) ;
#18517 = CARTESIAN_POINT ( 'NONE',  ( 10.00000000000102318, -5.773502691895667560, -4.000000004096737172 ) ) ;
#18518 = CARTESIAN_POINT ( 'NONE',  ( 7.070501591499376803E-16, 11.54700538379251284, -126.1249999999999858 ) ) ;
#18519 = CARTESIAN_POINT ( 'NONE',  ( -9.999999999999998224, 1.224646799147353059E-15, -200.0000000000000000 ) ) ;
#18520 = CARTESIAN_POINT ( 'NONE',  ( 10.81189881249999729, 0.000000000000000000, -162.0312500020484094 ) ) ;
#18521 = CARTESIAN_POINT ( 'NONE',  ( -2.121150477449813534E-15, -11.54700538379251284, -13.25000000409675849 ) ) ;
#18522 = CARTESIAN_POINT ( 'NONE',  ( 4.999999999999992006, -8.660254037844389075, -172.1250000040968189 ) ) ;
#18523 = CARTESIAN_POINT ( 'NONE',  ( -2.293366432827344421E-15, -12.48450537969573659, -114.2187500020483668 ) ) ;
#18524 = CARTESIAN_POINT ( 'NONE',  ( 5.405949406249999534, 9.363379034771803333, -88.09375000204836681 ) ) ;
#18525 = CARTESIAN_POINT ( 'NONE',  ( 10.81189881249999729, 0.000000000000000000, -191.8437500020484094 ) ) ;
#18526 = CARTESIAN_POINT ( 'NONE',  ( 5.405949406249992428, -9.363379034771808662, -90.28125000204838102 ) ) ;
#18527 = CARTESIAN_POINT ( 'NONE',  ( -9.999999999999998224, 5.773502691896259087, -180.2500000040967905 ) ) ;
#18528 = CARTESIAN_POINT ( 'NONE',  ( -2.293366432827344421E-15, -12.48450537969573659, -174.4062500020484379 ) ) ;
#18529 = CARTESIAN_POINT ( 'NONE',  ( -9.999999999999998224, 1.224646799147353059E-15, -68.74999999999997158 ) ) ;
#18530 = CARTESIAN_POINT ( 'NONE',  ( 5.405949406249992428, -9.363379034771808662, -172.7812500020484094 ) ) ;
#18531 = CARTESIAN_POINT ( 'NONE',  ( 10.81189881249999729, 0.000000000000000000, -184.5312500020484094 ) ) ;
#18532 = CARTESIAN_POINT ( 'NONE',  ( 10.81189881249999729, 6.242252689847867408, -46.21875000204838102 ) ) ;
#18533 = CARTESIAN_POINT ( 'NONE',  ( -9.999999999999998224, 5.773502691896259087, -162.2500000040967620 ) ) ;
#18534 = CARTESIAN_POINT ( 'NONE',  ( -5.405949406250003975, -9.363379034771801557, -3.531250002048374803 ) ) ;
#18535 = CARTESIAN_POINT ( 'NONE',  ( 5.405949406249999534, 9.363379034771803333, -13.09375000204834905 ) ) ;
#18536 = DIRECTION ( 'NONE',  ( 1.000000000000000000, 0.000000000000000000, 0.000000000000000000 ) ) ;
#18537 = CARTESIAN_POINT ( 'NONE',  ( 10.81189881249999907, 6.242252689847868297, -122.7187500020483810 ) ) ;
#18538 = CARTESIAN_POINT ( 'NONE',  ( 9.999999999999996447, -5.773502691896262640, -90.62499999999998579 ) ) ;
#18539 = CARTESIAN_POINT ( 'NONE',  ( 5.405949406249992428, -9.363379034771808662, -24.28125000204836681 ) ) ;
#18540 = CARTESIAN_POINT ( 'NONE',  ( -5.000000000000003553, -8.660254037844383745, -107.8750000040967763 ) ) ;
#18541 = VECTOR ( 'NONE', #9975, 1000.000000000000000 ) ;
#18542 =( BOUNDED_CURVE ( )  B_SPLINE_CURVE ( 2, ( #11551, #37250, #24760, #4888, #40266, #37689, #18035 ),
 .UNSPECIFIED., .F., .F. ) 
 B_SPLINE_CURVE_WITH_KNOTS ( ( 3, 2, 2, 3 ),
 ( 0.1529850746268656692, 0.1542288557213930267, 0.1554726368159203842, 0.1567164179104477695 ),
 .UNSPECIFIED. ) 
 CURVE ( )  GEOMETRIC_REPRESENTATION_ITEM ( )  RATIONAL_B_SPLINE_CURVE ( ( 1.000000000000000000, 0.8660254037844387076, 1.000000000000000000, 0.8660254037844387076, 1.000000000000000000, 0.8660254037844387076, 1.000000000000000000 ) ) 
 REPRESENTATION_ITEM ( '' )  );
#18543 = DIRECTION ( 'NONE',  ( 1.000000000000000000, 0.000000000000000000, 0.000000000000000000 ) ) ;
#18544 = CARTESIAN_POINT ( 'NONE',  ( -5.000000000000003553, -8.660254037844383745, -50.49999999999998579 ) ) ;
#18545 = CARTESIAN_POINT ( 'NONE',  ( -2.293366432827344421E-15, -12.48450537969573659, -115.9062500020483810 ) ) ;
#18546 = CARTESIAN_POINT ( 'NONE',  ( 5.405949406249999534, 9.363379034771803333, -98.78125000204839523 ) ) ;
#18547 = ORIENTED_EDGE ( 'NONE', *, *, #41692, .T. ) ;
#18548 = CARTESIAN_POINT ( 'NONE',  ( -10.00000000000000000, -5.773502691896251982, -90.00000000409677625 ) ) ;
#18549 = DIRECTION ( 'NONE',  ( 1.000000000000000000, 0.000000000000000000, 0.000000000000000000 ) ) ;
#18550 = CARTESIAN_POINT ( 'NONE',  ( 10.81189881249999907, 6.242252689847868297, -155.9062500020484094 ) ) ;
#18551 = CARTESIAN_POINT ( 'NONE',  ( 7.644554776091147741E-16, 12.48450537969573659, -51.96875000204836681 ) ) ;
#18552 = VERTEX_POINT ( 'NONE', #34543 ) ;
#18553 = CARTESIAN_POINT ( 'NONE',  ( 4.999999999999992006, -8.660254037844389075, -14.24999999999995737 ) ) ;
#18554 = VECTOR ( 'NONE', #11358, 1000.000000000000000 ) ;
#18555 = CARTESIAN_POINT ( 'NONE',  ( 5.405949406249992428, -9.363379034771808662, -30.28125000204837036 ) ) ;
#18556 = CARTESIAN_POINT ( 'NONE',  ( 10.00000000000000000, 5.773502691896255534, -156.3749999999999716 ) ) ;
#18557 = CARTESIAN_POINT ( 'NONE',  ( 9.999999999999998224, 0.000000000000000000, -18.87500000409675494 ) ) ;
#18558 = AXIS2_PLACEMENT_3D ( 'NONE', #39539, #9969, #40803 ) ;
#18559 = DIRECTION ( 'NONE',  ( -1.000000000000000000, -0.000000000000000000, -0.000000000000000000 ) ) ;
#18560 = CARTESIAN_POINT ( 'NONE',  ( 10.81189881249999907, 6.242252689847868297, -124.4062500020483810 ) ) ;
#18561 = DIRECTION ( 'NONE',  ( -0.000000000000000000, -0.000000000000000000, 1.000000000000000000 ) ) ;
#18562 = EDGE_CURVE ( 'NONE', #8113, #14562, #7253, .T. ) ;
#18563 = CARTESIAN_POINT ( 'NONE',  ( 9.999999999999998224, 1.224646799147353059E-15, -99.99999999999998579 ) ) ;
#18564 = ORIENTED_EDGE ( 'NONE', *, *, #42227, .F. ) ;
#18565 = ADVANCED_FACE ( 'NONE', ( #37984 ), #8428, .T. ) ;
#18566 = CARTESIAN_POINT ( 'NONE',  ( -10.81189881249999729, 6.242252689847871849, -62.40625000204838813 ) ) ;
#18567 = SECURITY_CLASSIFICATION_LEVEL ( 'unclassified' ) ;
#18568 = EDGE_CURVE ( 'NONE', #35978, #35357, #24917, .T. ) ;
#18569 = CARTESIAN_POINT ( 'NONE',  ( -10.81189881249999907, -6.242252689847864744, -112.9687500020483810 ) ) ;
#18571 = ORIENTED_EDGE ( 'NONE', *, *, #5126, .T. ) ;
#18570 = VERTEX_POINT ( 'NONE', #37119 ) ;
#18572 = CARTESIAN_POINT ( 'NONE',  ( 5.000000000000000000, 8.660254037844385522, -175.7500000000000284 ) ) ;
#18573 = CC_DESIGN_PERSON_AND_ORGANIZATION_ASSIGNMENT ( #19826, #20466, ( #4933 ) ) ;
#18574 = CARTESIAN_POINT ( 'NONE',  ( -9.999999999999998224, 1.224646799147353059E-15, -200.0000000000000000 ) ) ;
#18575 = CARTESIAN_POINT ( 'NONE',  ( 7.644554776091147741E-16, 12.48450537969573659, -155.4687500020484094 ) ) ;
#18576 = CARTESIAN_POINT ( 'NONE',  ( 5.405949406249992428, -9.363379034771808662, -184.7812500020484094 ) ) ;
#18577 = CARTESIAN_POINT ( 'NONE',  ( 5.405949406249992428, -9.363379034771808662, -9.093750002048345493 ) ) ;
#18578 = CARTESIAN_POINT ( 'NONE',  ( -2.293366432827344421E-15, -12.48450537969573659, -138.2187500020483810 ) ) ;
#18579 = CARTESIAN_POINT ( 'NONE',  ( -10.81189881249999729, 6.242252689847871849, -107.2187500020483810 ) ) ;
#18580 = CARTESIAN_POINT ( 'NONE',  ( -9.999999999999998224, 1.224646799147353059E-15, -55.24999999999996447 ) ) ;
#18581 = CARTESIAN_POINT ( 'NONE',  ( -10.81189881249999729, 6.242252689847871849, -119.4062500020483952 ) ) ;
#18582 = CARTESIAN_POINT ( 'NONE',  ( 5.405949406249992428, -9.363379034771808662, -1.593750002048366365 ) ) ;
#18583 = CARTESIAN_POINT ( 'NONE',  ( -10.81189881249999729, 1.324075727343319199E-15, -122.0937500020483952 ) ) ;
#18584 = CARTESIAN_POINT ( 'NONE',  ( -5.405949406250003975, -9.363379034771801557, -197.0312500020484094 ) ) ;
#18585 =( BOUNDED_CURVE ( )  B_SPLINE_CURVE ( 2, ( #15220, #25597, #38755, #22352, #35528, #35935, #42605 ),
 .UNSPECIFIED., .F., .F. ) 
 B_SPLINE_CURVE_WITH_KNOTS ( ( 3, 2, 2, 3 ),
 ( 0.7835820895522389584, 0.7848258706467662327, 0.7860696517412937290, 0.7873134328358211143 ),
 .UNSPECIFIED. ) 
 CURVE ( )  GEOMETRIC_REPRESENTATION_ITEM ( )  RATIONAL_B_SPLINE_CURVE ( ( 0.9999999999999880096, 0.8660254037844506980, 1.000000000000000000, 0.8660254037844387076, 1.000000000000000000, 0.8660254037844148378, 1.000000000000023981 ) ) 
 REPRESENTATION_ITEM ( '' )  );
#18586 = CARTESIAN_POINT ( 'NONE',  ( -1.040834085586084257E-14, 125.0000000000000000, 22.49999999999999289 ) ) ;
#18587 = CARTESIAN_POINT ( 'NONE',  ( -9.999999999999998224, 5.773502691896259087, -151.3750000000000000 ) ) ;
#18588 = CARTESIAN_POINT ( 'NONE',  ( 5.000000000000000000, 8.660254037844385522, -13.74999999999995737 ) ) ;
#18589 = EDGE_CURVE ( 'NONE', #11765, #16918, #11649, .T. ) ;
#18590 = CARTESIAN_POINT ( 'NONE',  ( -5.405949406250003975, -9.363379034771801557, -69.34375000204836681 ) ) ;
#18591 = CARTESIAN_POINT ( 'NONE',  ( 10.81189881249999907, 6.242252689847868297, -53.71875000204838102 ) ) ;
#18592 = CARTESIAN_POINT ( 'NONE',  ( -10.00000000000000000, -5.773502691896251982, -184.5000000040968189 ) ) ;
#18593 = CARTESIAN_POINT ( 'NONE',  ( 10.81189881249999729, 0.000000000000000000, -25.53125000204836681 ) ) ;
#18594 = CARTESIAN_POINT ( 'NONE',  ( -5.405949406250003975, -9.363379034771801557, -37.84375000204837391 ) ) ;
#18595 = CARTESIAN_POINT ( 'NONE',  ( -2.293366432827344421E-15, -12.48450537969573659, -142.7187500020484094 ) ) ;
#18596 = CARTESIAN_POINT ( 'NONE',  ( -2.121150477449813534E-15, -11.54700538379251284, -110.3749999999999858 ) ) ;
#18597 = CARTESIAN_POINT ( 'NONE',  ( -9.999999999999998224, 1.224646799147353059E-15, -136.2499999999999716 ) ) ;
#18598 = CARTESIAN_POINT ( 'NONE',  ( -4.999999999999996447, 8.660254037844387298, -76.49999999999998579 ) ) ;
#18599 = CARTESIAN_POINT ( 'NONE',  ( -10.81189881249999729, 1.324075727343319199E-15, -143.2812500020483810 ) ) ;
#18600 = CARTESIAN_POINT ( 'NONE',  ( 10.81189881249999551, -6.242252689847874514, -12.15625000204835615 ) ) ;
#18601 = ORIENTED_EDGE ( 'NONE', *, *, #15615, .F. ) ;
#18602 = CARTESIAN_POINT ( 'NONE',  ( -4.999999999999996447, 8.660254037844387298, -117.3750000040967905 ) ) ;
#18603 = CARTESIAN_POINT ( 'NONE',  ( -2.275517850991317657E-15, -20.00000000000000000, -219.9999999999999716 ) ) ;
#18604 = CARTESIAN_POINT ( 'NONE',  ( 10.81189881249999907, 6.242252689847868297, -77.71875000204838102 ) ) ;
#18605 = CARTESIAN_POINT ( 'NONE',  ( -10.00000000000000000, -5.773502691896251982, -47.62499999999997158 ) ) ;
#18606 = CARTESIAN_POINT ( 'NONE',  ( -2.121150477449813534E-15, -11.54700538379251284, -26.75000000409677270 ) ) ;
#18607 = CARTESIAN_POINT ( 'NONE',  ( 9.999999999999998224, 0.000000000000000000, -2.375000004096766482 ) ) ;
#18608 = CARTESIAN_POINT ( 'NONE',  ( -5.405949406249996869, 9.363379034771805109, -46.03125000204838813 ) ) ;
#18609 = CARTESIAN_POINT ( 'NONE',  ( -10.81189881249999907, -6.242252689847864744, -147.6562500020483810 ) ) ;
#18610 = AXIS2_PLACEMENT_3D ( 'NONE', #37725, #5142, #24366 ) ;
#18611 = CARTESIAN_POINT ( 'NONE',  ( 10.81189881249999907, 6.242252689847868297, -152.9062500020483810 ) ) ;
#18612 = CARTESIAN_POINT ( 'NONE',  ( -5.000000000000003553, -8.660254037844383745, -65.49999999999997158 ) ) ;
#18613 = ORIENTED_EDGE ( 'NONE', *, *, #41740, .F. ) ;
#18614 = EDGE_LOOP ( 'NONE', ( #39357, #38341, #29722, #38468 ) ) ;
#18615 = VERTEX_POINT ( 'NONE', #12482 ) ;
#18616 = CARTESIAN_POINT ( 'NONE',  ( 4.999999999999992006, -8.660254037844389075, -7.125000004096743389 ) ) ;
#18617 = CARTESIAN_POINT ( 'NONE',  ( 5.405949406249992428, -9.363379034771808662, -178.5937500020484094 ) ) ;
#18619 = ADVANCED_FACE ( 'NONE', ( #41630 ), #12275, .T. ) ;
#18618 = CARTESIAN_POINT ( 'NONE',  ( 5.405949406249999534, 9.363379034771803333, -28.09375000204836326 ) ) ;
#18620 = CARTESIAN_POINT ( 'NONE',  ( 4.999999999999992006, -8.660254037844389075, -41.24999999999997868 ) ) ;
#18621 = CARTESIAN_POINT ( 'NONE',  ( 5.405949406249992428, -9.363379034771808662, -166.5937500020484094 ) ) ;
#18622 = CARTESIAN_POINT ( 'NONE',  ( 5.405949406249999534, 9.363379034771803333, -149.5937500020483810 ) ) ;
#18623 = CARTESIAN_POINT ( 'NONE',  ( 9.999999999999998224, 1.224646799147353059E-15, -99.99999999999998579 ) ) ;
#18624 = CARTESIAN_POINT ( 'NONE',  ( -10.81189881249999907, -6.242252689847864744, -132.4687500020483810 ) ) ;
#18625 = CARTESIAN_POINT ( 'NONE',  ( 7.644554776091147741E-16, 12.48450537969573659, -139.1562500020483810 ) ) ;
#18626 = CARTESIAN_POINT ( 'NONE',  ( -10.81189881249999729, 6.242252689847871849, -144.7187500020484094 ) ) ;
#18627 = CARTESIAN_POINT ( 'NONE',  ( 7.070501591499376803E-16, 11.54700538379251284, -129.1250000000000000 ) ) ;
#18628 = DIRECTION ( 'NONE',  ( -0.000000000000000000, -0.000000000000000000, 1.000000000000000000 ) ) ;
#18629 = CARTESIAN_POINT ( 'NONE',  ( 9.999999999999998224, 0.000000000000000000, -171.5000000000000000 ) ) ;
#18630 = AXIS2_PLACEMENT_3D ( 'NONE', #22383, #2545, #2336 ) ;
#18631 = CARTESIAN_POINT ( 'NONE',  ( 7.644554776091147741E-16, 12.48450537969573659, -84.96875000204835260 ) ) ;
#18632 = FACE_OUTER_BOUND ( 'NONE', #9174, .T. ) ;
#18633 = CARTESIAN_POINT ( 'NONE',  ( -10.81189881249999907, -6.242252689847864744, -50.15625000204837391 ) ) ;
#18634 = CARTESIAN_POINT ( 'NONE',  ( -10.00000000000076916, 5.773502691895813221, -133.3749999999999716 ) ) ;
#18635 = CARTESIAN_POINT ( 'NONE',  ( 10.81189881249999551, -6.242252689847874514, -173.9687500020484094 ) ) ;
#18636 = CARTESIAN_POINT ( 'NONE',  ( 5.405949406249992428, -9.363379034771808662, -112.7812500020483952 ) ) ;
#18637 = CARTESIAN_POINT ( 'NONE',  ( -10.81189881249999729, 6.242252689847871849, -146.4062500020484094 ) ) ;
#18638 = CARTESIAN_POINT ( 'NONE',  ( -10.00000000000051337, 5.773502691895962435, -142.7500000040967905 ) ) ;
#18639 = CARTESIAN_POINT ( 'NONE',  ( 7.644554776091147741E-16, 12.48450537969573659, -34.15625000204835970 ) ) ;
#18640 = CARTESIAN_POINT ( 'NONE',  ( 10.00000000000000000, 5.773502691896255534, -125.2500000040967905 ) ) ;
#18641 = CARTESIAN_POINT ( 'NONE',  ( -9.999999999999998224, 1.224646799147353059E-15, -103.2500000000000000 ) ) ;
#18642 = ORIENTED_EDGE ( 'NONE', *, *, #22547, .T. ) ;
#18643 = CARTESIAN_POINT ( 'NONE',  ( 10.81189881249999729, 6.242252689847867408, -125.9062500020483810 ) ) ;
#18644 = CARTESIAN_POINT ( 'NONE',  ( 4.999999999999992006, -8.660254037844389075, -143.6250000040967905 ) ) ;
#18645 = CARTESIAN_POINT ( 'NONE',  ( 7.070501591499376803E-16, 11.54700538379251284, -184.6250000000000000 ) ) ;
#18646 = CARTESIAN_POINT ( 'NONE',  ( -10.81189881249999729, 1.324075727343319199E-15, -182.2812500020483810 ) ) ;
#18647 = VERTEX_POINT ( 'NONE', #15718 ) ;
#18648 = CARTESIAN_POINT ( 'NONE',  ( -2.121150477449813534E-15, -11.54700538379251284, -50.75000000409676204 ) ) ;
#18649 = FACE_OUTER_BOUND ( 'NONE', #3753, .T. ) ;
#18650 = CARTESIAN_POINT ( 'NONE',  ( 7.644554776091147741E-16, 12.48450537969573659, -68.65625000204839523 ) ) ;
#18651 = DIRECTION ( 'NONE',  ( -1.000000000000000000, 0.000000000000000000, 0.000000000000000000 ) ) ;
#18652 = CARTESIAN_POINT ( 'NONE',  ( -5.405949406249996869, 9.363379034771805109, -169.0312500020484094 ) ) ;
#18653 = CARTESIAN_POINT ( 'NONE',  ( -4.999999999999996447, 8.660254037844387298, -7.499999999999978684 ) ) ;
#18654 = DIRECTION ( 'NONE',  ( 1.000000000000000000, 0.000000000000000000, 0.000000000000000000 ) ) ;
#18655 = ORIENTED_EDGE ( 'NONE', *, *, #23971, .T. ) ;
#18656 = FACE_OUTER_BOUND ( 'NONE', #35813, .T. ) ;
#18657 = CARTESIAN_POINT ( 'NONE',  ( -9.999999999998969713, -5.773502691896847949, -52.50000000409674072 ) ) ;
#18658 = DIRECTION ( 'NONE',  ( 0.000000000000000000, 1.000000000000000000, 0.000000000000000000 ) ) ;
#18659 = CC_DESIGN_APPROVAL ( #5916, ( #8303 ) ) ;
#18661 = ORIENTED_EDGE ( 'NONE', *, *, #39253, .F. ) ;
#18660 = CARTESIAN_POINT ( 'NONE',  ( -10.81189881249999907, -6.242252689847864744, -78.65625000204839523 ) ) ;
#18662 = AXIS2_PLACEMENT_3D ( 'NONE', #42423, #29492, #23018 ) ;
#18664 = ORIENTED_EDGE ( 'NONE', *, *, #13238, .T. ) ;
#18663 = CARTESIAN_POINT ( 'NONE',  ( 10.00000000000051159, -5.773502691895965988, -178.0000000040967336 ) ) ;
#18665 = ORIENTED_EDGE ( 'NONE', *, *, #37514, .T. ) ;
#18666 = CARTESIAN_POINT ( 'NONE',  ( -5.405949406249996869, 9.363379034771805109, -32.34375000204836681 ) ) ;
#18667 = DIRECTION ( 'NONE',  ( -1.000000000000000000, 0.000000000000000000, 0.000000000000000000 ) ) ;
#18668 = CARTESIAN_POINT ( 'NONE',  ( 5.405949406249992428, -9.363379034771808662, -3.281250002048374803 ) ) ;
#18670 = EDGE_LOOP ( 'NONE', ( #41374, #24067, #6710, #35722 ) ) ;
#18669 = CARTESIAN_POINT ( 'NONE',  ( -5.405949406249996869, 9.363379034771805109, -57.84375000204835970 ) ) ;
#18671 = DIRECTION ( 'NONE',  ( 0.4999999999999997780, 0.8660254037844388186, 0.000000000000000000 ) ) ;
#18672 = CARTESIAN_POINT ( 'NONE',  ( 4.999999999999992006, -8.660254037844389075, -33.74999999999997158 ) ) ;
#18673 = CARTESIAN_POINT ( 'NONE',  ( 10.81189881249999729, 6.242252689847867408, -184.2187500020483810 ) ) ;
#18674 = CARTESIAN_POINT ( 'NONE',  ( 10.81189881249999551, -6.242252689847874514, -178.4687500020484094 ) ) ;
#18675 = CARTESIAN_POINT ( 'NONE',  ( 5.405949406249999534, 9.363379034771803333, -161.5937500020484094 ) ) ;
#18676 = CARTESIAN_POINT ( 'NONE',  ( -2.293366432827344421E-15, -12.48450537969573659, -174.2187500020483810 ) ) ;
#18677 = DIRECTION ( 'NONE',  ( -0.000000000000000000, -0.000000000000000000, 1.000000000000000000 ) ) ;
#18678 = CARTESIAN_POINT ( 'NONE',  ( 0.000000000000000000, 0.000000000000000000, -99.99999999999998579 ) ) ;
#18679 = CARTESIAN_POINT ( 'NONE',  ( 9.999999999999998224, 0.000000000000000000, -195.5000000000000000 ) ) ;
#18680 = CARTESIAN_POINT ( 'NONE',  ( 5.405949406249999534, 9.363379034771803333, -101.5937500020483810 ) ) ;
#18681 = CARTESIAN_POINT ( 'NONE',  ( -5.000000000000003553, -8.660254037844383745, -84.99999999999997158 ) ) ;
#18682 = CARTESIAN_POINT ( 'NONE',  ( -5.405949406250003975, -9.363379034771801557, -71.03125000204838102 ) ) ;
#18683 = CARTESIAN_POINT ( 'NONE',  ( 10.81189881249999729, 6.242252689847867408, -94.21875000204838102 ) ) ;
#18684 = CARTESIAN_POINT ( 'NONE',  ( 10.81189881249999551, -6.242252689847874514, -69.15625000204839523 ) ) ;
#18685 = CARTESIAN_POINT ( 'NONE',  ( 7.070501591499377789E-16, 11.54700538379251284, -143.0000000040967905 ) ) ;
#18686 = CARTESIAN_POINT ( 'NONE',  ( 10.00000000000000000, 5.773502691896255534, -123.3749999999999858 ) ) ;
#18687 = ADVANCED_FACE ( 'NONE', ( #35606 ), #31739, .F. ) ;
#18688 = AXIS2_PLACEMENT_3D ( 'NONE', #40561, #11430, #24419 ) ;
#18689 = ORIENTED_EDGE ( 'NONE', *, *, #38167, .F. ) ;
#18690 = CARTESIAN_POINT ( 'NONE',  ( 10.81189881249999551, -6.242252689847874514, -151.6562500020484094 ) ) ;
#18691 = CARTESIAN_POINT ( 'NONE',  ( -2.293366432827344421E-15, -12.48450537969573659, -166.9062500020483810 ) ) ;
#18692 = CC_DESIGN_SECURITY_CLASSIFICATION ( #4933, ( #26987 ) ) ;
#18693 = DIRECTION ( 'NONE',  ( -0.000000000000000000, -0.000000000000000000, 1.000000000000000000 ) ) ;
#18694 = CARTESIAN_POINT ( 'NONE',  ( 9.999999999999998224, 0.000000000000000000, -102.8750000040967763 ) ) ;
#18695 = CARTESIAN_POINT ( 'NONE',  ( 5.405949406249992428, -9.363379034771808662, -94.59375000204838102 ) ) ;
#18696 = ORIENTED_EDGE ( 'NONE', *, *, #2253, .T. ) ;
#18697 = CARTESIAN_POINT ( 'NONE',  ( -5.000000000000003553, -8.660254037844383745, -68.49999999999997158 ) ) ;
#18698 = CARTESIAN_POINT ( 'NONE',  ( 10.81189881249999551, -6.242252689847874514, -193.4687500020484094 ) ) ;
#18699 = CARTESIAN_POINT ( 'NONE',  ( 9.999999999999996447, -5.773502691896262640, -77.50000000409677625 ) ) ;
#18700 = CARTESIAN_POINT ( 'NONE',  ( -6.604780291884596366, -7.711322195483102604, -180.0000000000000000 ) ) ;
#18701 = CARTESIAN_POINT ( 'NONE',  ( 9.999999999999998224, 0.000000000000000000, -11.37500000409674783 ) ) ;
#18702 = CARTESIAN_POINT ( 'NONE',  ( -10.81189881249999729, 1.324075727343319199E-15, -95.28125000204838102 ) ) ;
#18703 = CARTESIAN_POINT ( 'NONE',  ( 10.81189881249999551, -6.242252689847874514, -67.65625000204839523 ) ) ;
#18704 =( BOUNDED_CURVE ( )  B_SPLINE_CURVE ( 2, ( #2750, #21955, #29283, #35972, #35561, #9007, #25215 ),
 .UNSPECIFIED., .F., .F. ) 
 B_SPLINE_CURVE_WITH_KNOTS ( ( 3, 2, 2, 3 ),
 ( 0.05970149253731348721, 0.06094527363184085167, 0.06218905472636821613, 0.06343283582089558059 ),
 .UNSPECIFIED. ) 
 CURVE ( )  GEOMETRIC_REPRESENTATION_ITEM ( )  RATIONAL_B_SPLINE_CURVE ( ( 0.9999999999999940048, 0.8660254037844447028, 1.000000000000000000, 0.8660254037844387076, 1.000000000000000000, 0.8660254037844327124, 1.000000000000005995 ) ) 
 REPRESENTATION_ITEM ( '' )  );
#18705 = CARTESIAN_POINT ( 'NONE',  ( -9.999999999999998224, 5.773502691896259087, -64.75000000409677625 ) ) ;
#18706 = LINE ( 'NONE', #5770, #16933 ) ;
#18707 = CARTESIAN_POINT ( 'NONE',  ( -5.405949406250003975, -9.363379034771801557, -28.84375000204836326 ) ) ;
#18708 = CARTESIAN_POINT ( 'NONE',  ( 9.999999999999998224, 0.000000000000000000, -182.0000000000000000 ) ) ;
#18709 = CARTESIAN_POINT ( 'NONE',  ( -5.405949406250003975, -9.363379034771801557, -191.0312500020484094 ) ) ;
#18710 = VECTOR ( 'NONE', #19461, 1000.000000000000000 ) ;
#18711 = CARTESIAN_POINT ( 'NONE',  ( 10.81189881249999729, 0.000000000000000000, -16.53125000204835970 ) ) ;
#18712 = CARTESIAN_POINT ( 'NONE',  ( -10.81189881249999729, 1.324075727343319199E-15, -2.093750002048366810 ) ) ;
#18713 = CARTESIAN_POINT ( 'NONE',  ( 9.999999999999998224, 0.000000000000000000, -149.3750000040967905 ) ) ;
#18714 = CARTESIAN_POINT ( 'NONE',  ( -10.00000000000015987, 5.773502691896167605, -191.8750000000000000 ) ) ;
#18715 = CARTESIAN_POINT ( 'NONE',  ( -2.121150477449813534E-15, -11.54700538379251284, -173.3750000000000000 ) ) ;
#18716 = CARTESIAN_POINT ( 'NONE',  ( 4.999999999999992006, -8.660254037844389075, -174.7500000000000284 ) ) ;
#18717 = CARTESIAN_POINT ( 'NONE',  ( -9.999999999998969713, -5.773502691896847949, -37.12499999999993605 ) ) ;
#18719 = VERTEX_POINT ( 'NONE', #25471 ) ;
#18718 = CARTESIAN_POINT ( 'NONE',  ( -5.405949406249996869, 9.363379034771805109, -103.0312500020483952 ) ) ;
#18720 = EDGE_CURVE ( 'NONE', #19924, #13418, #38194, .T. ) ;
#18721 = CARTESIAN_POINT ( 'NONE',  ( -8.660253955908514101, -5.000000141917089636, -180.0000000000000284 ) ) ;
#18722 = VERTEX_POINT ( 'NONE', #35815 ) ;
#18723 = ORIENTED_EDGE ( 'NONE', *, *, #36718, .F. ) ;
#18724 = VECTOR ( 'NONE', #4866, 1000.000000000000000 ) ;
#18725 = CARTESIAN_POINT ( 'NONE',  ( 5.405949406249992428, -9.363379034771808662, -33.28125000204837391 ) ) ;
#18726 = LOCAL_TIME ( 11, 57, 6.000000000000000000, #35359 ) ;
#18727 = CARTESIAN_POINT ( 'NONE',  ( 10.81189881249999551, -6.242252689847874514, -76.46875000204838102 ) ) ;
#18728 = CARTESIAN_POINT ( 'NONE',  ( -2.121150477449813534E-15, -11.54700538379251284, -173.3750000000000000 ) ) ;
#18729 = CARTESIAN_POINT ( 'NONE',  ( -5.405949406250003975, -9.363379034771801557, -198.3437500020484094 ) ) ;
#18730 = CARTESIAN_POINT ( 'NONE',  ( 9.999999999999742428, 5.773502691896404748, -124.8749999999999858 ) ) ;
#18731 = CARTESIAN_POINT ( 'NONE',  ( -10.81189881249999729, 1.324075727343319199E-15, -161.2812500020484094 ) ) ;
#18732 = CARTESIAN_POINT ( 'NONE',  ( -2.121150477449813534E-15, -11.54700538379251284, -11.75000000409676737 ) ) ;
#18733 = VECTOR ( 'NONE', #3413, 1000.000000000000000 ) ;
#18734 = CARTESIAN_POINT ( 'NONE',  ( -9.999999999999998224, 1.224646799147353059E-15, -91.62500000409677625 ) ) ;
#18735 = CARTESIAN_POINT ( 'NONE',  ( -2.293366432827344421E-15, -12.48450537969573659, -127.7187500020483668 ) ) ;
#18736 = CARTESIAN_POINT ( 'NONE',  ( 5.405949406249999534, 9.363379034771803333, -115.0937500020483810 ) ) ;
#18737 = CARTESIAN_POINT ( 'NONE',  ( 7.644554776091147741E-16, 12.48450537969573659, -87.96875000204838102 ) ) ;
#18738 = CARTESIAN_POINT ( 'NONE',  ( -10.81189881249999907, -6.242252689847864744, -190.9687500020484379 ) ) ;
#18739 = CARTESIAN_POINT ( 'NONE',  ( 10.81189881249999551, -6.242252689847874514, -94.65625000204838102 ) ) ;
#18740 = CARTESIAN_POINT ( 'NONE',  ( -5.000000000000003553, -8.660254037844383745, -170.8750000040968189 ) ) ;
#18741 = CARTESIAN_POINT ( 'NONE',  ( -5.405949406250003975, -9.363379034771801557, -170.0312500020484094 ) ) ;
#18742 = CARTESIAN_POINT ( 'NONE',  ( 4.999999999999992006, -8.660254037844389075, -70.12500000409677625 ) ) ;
#18743 = CARTESIAN_POINT ( 'NONE',  ( -5.405949406250003975, -9.363379034771801557, -171.5312500020484094 ) ) ;
#18744 = CARTESIAN_POINT ( 'NONE',  ( 5.405949406249992428, -9.363379034771808662, -190.7812500020484094 ) ) ;
#18745 = CARTESIAN_POINT ( 'NONE',  ( 10.81189881249999729, 0.000000000000000000, -47.84375000204838102 ) ) ;
#18746 = CARTESIAN_POINT ( 'NONE',  ( -4.999999999999996447, 8.660254037844387298, -165.3750000040967905 ) ) ;
#18747 = CARTESIAN_POINT ( 'NONE',  ( 10.81189881249999729, 0.000000000000000000, -4.531250002048375691 ) ) ;
#18748 = CARTESIAN_POINT ( 'NONE',  ( -10.81189881249999907, -6.242252689847864744, -12.46875000204836326 ) ) ;
#18749 = CARTESIAN_POINT ( 'NONE',  ( -9.999999999999998224, 1.224646799147353059E-15, -5.749999999999976907 ) ) ;
#18750 = CARTESIAN_POINT ( 'NONE',  ( -10.81189881249999729, 1.324075727343319199E-15, -123.5937500020483952 ) ) ;
#18751 = EDGE_CURVE ( 'NONE', #30149, #29666, #30713, .T. ) ;
#18752 = CARTESIAN_POINT ( 'NONE',  ( -10.00000000000000000, -5.773502691896251982, -86.62499999999997158 ) ) ;
#18753 = CARTESIAN_POINT ( 'NONE',  ( 10.81189881249999907, 6.242252689847868297, -23.90625000204838102 ) ) ;
#18754 = CARTESIAN_POINT ( 'NONE',  ( -2.121150477449813534E-15, -11.54700538379251284, -94.25000000409677625 ) ) ;
#18755 = CARTESIAN_POINT ( 'NONE',  ( -10.00000000000012434, 5.773502691896184480, -157.7500000040967905 ) ) ;
#18756 = CARTESIAN_POINT ( 'NONE',  ( 5.405949406249992428, -9.363379034771808662, -118.7812500020483952 ) ) ;
#18757 = CARTESIAN_POINT ( 'NONE',  ( 10.81189881249999729, 6.242252689847867408, -101.9062500020483952 ) ) ;
#18758 = ORIENTED_EDGE ( 'NONE', *, *, #39117, .T. ) ;
#18759 = VECTOR ( 'NONE', #4935, 1000.000000000000000 ) ;
#18760 = CARTESIAN_POINT ( 'NONE',  ( -5.000000000000003553, -8.660254037844383745, -88.37500000409677625 ) ) ;
#18761 = DIRECTION ( 'NONE',  ( -0.000000000000000000, -0.000000000000000000, -1.000000000000000000 ) ) ;
#18762 = CARTESIAN_POINT ( 'NONE',  ( -10.81189881249999729, 6.242252689847871849, -156.9062500020483810 ) ) ;
#18763 = CARTESIAN_POINT ( 'NONE',  ( -10.81189881249999729, 1.324075727343319199E-15, -51.59375000204835260 ) ) ;
#18764 = ORIENTED_EDGE ( 'NONE', *, *, #30335, .T. ) ;
#18765 = CARTESIAN_POINT ( 'NONE',  ( 5.000000000000000000, 8.660254037844385522, -18.24999999999996092 ) ) ;
#18766 = CARTESIAN_POINT ( 'NONE',  ( 5.405949406249992428, -9.363379034771808662, -28.78125000204837036 ) ) ;
#18767 = CARTESIAN_POINT ( 'NONE',  ( -4.999999999999996447, 8.660254037844387298, -153.0000000000000000 ) ) ;
#18768 = CARTESIAN_POINT ( 'NONE',  ( -9.999999999999998224, 5.773502691896259087, -19.75000000409676915 ) ) ;
#18769 = VECTOR ( 'NONE', #19600, 1000.000000000000000 ) ;
#18770 = CARTESIAN_POINT ( 'NONE',  ( 4.999999999999992006, -8.660254037844389075, -198.7500000000000000 ) ) ;
#18772 = EDGE_LOOP ( 'NONE', ( #6890, #12653, #3857, #13051 ) ) ;
#18771 = CARTESIAN_POINT ( 'NONE',  ( 7.644554776091147741E-16, 12.48450537969573659, -125.6562500020483810 ) ) ;
#18773 = CARTESIAN_POINT ( 'NONE',  ( -2.121150477449813534E-15, -11.54700538379251284, -152.3749999999999716 ) ) ;
#18774 = CARTESIAN_POINT ( 'NONE',  ( -4.999999999999996447, 8.660254037844387298, -142.8750000040967905 ) ) ;
#18775 = ORIENTED_EDGE ( 'NONE', *, *, #9727, .F. ) ;
#18776 = CARTESIAN_POINT ( 'NONE',  ( 5.405949406249992428, -9.363379034771808662, -54.28125000204836681 ) ) ;
#18777 = PERSON_AND_ORGANIZATION ( #11915, #17965 ) ;
#18778 = CARTESIAN_POINT ( 'NONE',  ( -5.405949406249996869, 9.363379034771805109, -102.8437500020483810 ) ) ;
#18780 = VERTEX_POINT ( 'NONE', #18974 ) ;
#18779 = VERTEX_POINT ( 'NONE', #8847 ) ;
#18781 = CARTESIAN_POINT ( 'NONE',  ( -9.999999999999998224, 1.224646799147353059E-15, -175.6250000040968189 ) ) ;
#18782 = CARTESIAN_POINT ( 'NONE',  ( 9.999999999999998224, 0.000000000000000000, -171.5000000000000000 ) ) ;
#18783 = CARTESIAN_POINT ( 'NONE',  ( -5.405949406250003975, -9.363379034771801557, -159.3437500020484094 ) ) ;
#18784 = CARTESIAN_POINT ( 'NONE',  ( 7.644554776091147741E-16, 12.48450537969573659, -188.6562500020484379 ) ) ;
#18785 = CARTESIAN_POINT ( 'NONE',  ( -5.405949406250003975, -9.363379034771801557, -4.843750002048369474 ) ) ;
#18786 = CARTESIAN_POINT ( 'NONE',  ( -5.000000000000003553, -8.660254037844383745, -74.49999999999998579 ) ) ;
#18787 = CARTESIAN_POINT ( 'NONE',  ( -10.81189881249999729, 1.324075727343319199E-15, -141.5937500020483810 ) ) ;
#18788 =( BOUNDED_CURVE ( )  B_SPLINE_CURVE ( 2, ( #37403, #17526, #14277, #7846, #27481, #34181, #5681 ),
 .UNSPECIFIED., .F., .F. ) 
 B_SPLINE_CURVE_WITH_KNOTS ( ( 3, 2, 2, 3 ),
 ( 0.8358208955223882519, 0.8370646766169156372, 0.8383084577114430225, 0.8395522388059704078 ),
 .UNSPECIFIED. ) 
 CURVE ( )  GEOMETRIC_REPRESENTATION_ITEM ( )  RATIONAL_B_SPLINE_CURVE ( ( 0.9999999999999761302, 0.8660254037844625774, 1.000000000000000000, 0.8660254037844387076, 1.000000000000000000, 0.8660254037844148378, 1.000000000000023981 ) ) 
 REPRESENTATION_ITEM ( '' )  );
#18789 = CARTESIAN_POINT ( 'NONE',  ( -10.81189881249999729, 6.242252689847871849, -111.7187500020483810 ) ) ;
#18790 = CARTESIAN_POINT ( 'NONE',  ( 9.999999999999998224, 0.000000000000000000, -191.3750000040967905 ) ) ;
#18791 = CARTESIAN_POINT ( 'NONE',  ( 5.405949406249999534, 9.363379034771803333, -115.2812500020483952 ) ) ;
#18792 = CARTESIAN_POINT ( 'NONE',  ( -10.00000000000000000, -5.773502691896251982, -198.0000000040968189 ) ) ;
#18793 = CARTESIAN_POINT ( 'NONE',  ( 7.644554776091147741E-16, 12.48450537969573659, -120.9687500020483952 ) ) ;
#18794 = CARTESIAN_POINT ( 'NONE',  ( 10.81189881249999729, 6.242252689847867408, -193.4062500020484094 ) ) ;
#18795 = DIRECTION ( 'NONE',  ( -1.000000000000000000, 0.000000000000000000, 0.000000000000000000 ) ) ;
#18796 = CARTESIAN_POINT ( 'NONE',  ( -5.000000000000003553, -8.660254037844383745, -140.5000000000000000 ) ) ;
#18797 = CARTESIAN_POINT ( 'NONE',  ( 7.070501591499377789E-16, 11.54700538379251284, -15.12499999999997158 ) ) ;
#18798 = VECTOR ( 'NONE', #16990, 1000.000000000000000 ) ;
#18799 = CARTESIAN_POINT ( 'NONE',  ( 10.81189881249999729, 0.000000000000000000, -67.34375000204836681 ) ) ;
#18800 = CARTESIAN_POINT ( 'NONE',  ( -2.293366432827344421E-15, -12.48450537969573659, -55.71875000204837391 ) ) ;
#18801 = CARTESIAN_POINT ( 'NONE',  ( 10.00000000000000000, 5.773502691896255534, -186.7500000040967905 ) ) ;
#18802 = CARTESIAN_POINT ( 'NONE',  ( -10.81189881249999729, 1.324075727343319199E-15, -29.28125000204837036 ) ) ;
#18803 = CARTESIAN_POINT ( 'NONE',  ( -2.293366432827344421E-15, -12.48450537969573659, -36.21875000204835970 ) ) ;
#18804 = CARTESIAN_POINT ( 'NONE',  ( 9.999999999999998224, 0.000000000000000000, -32.37500000409676204 ) ) ;
#18805 = CARTESIAN_POINT ( 'NONE',  ( -10.81189881249999729, 1.324075727343319199E-15, -144.5937500020483810 ) ) ;
#18806 = EDGE_CURVE ( 'NONE', #18815, #38638, #22005, .T. ) ;
#18807 = CARTESIAN_POINT ( 'NONE',  ( 10.00000000000000000, 5.773502691896255534, -117.3750000000000000 ) ) ;
#18808 = ADVANCED_FACE ( 'NONE', ( #2589 ), #31888, .T. ) ;
#18809 = CARTESIAN_POINT ( 'NONE',  ( 7.070501591499376803E-16, 11.54700538379251284, -145.6250000000000000 ) ) ;
#18810 = ADVANCED_FACE ( 'NONE', ( #39038 ), #19391, .T. ) ;
#18811 = CARTESIAN_POINT ( 'NONE',  ( -9.999999999999998224, 5.773502691896259087, -74.87499999999997158 ) ) ;
#18812 = CARTESIAN_POINT ( 'NONE',  ( -2.293366432827344421E-15, -12.48450537969573659, -136.9062500020484094 ) ) ;
#18813 = CARTESIAN_POINT ( 'NONE',  ( -5.405949406249996869, 9.363379034771805109, -10.03125000204835260 ) ) ;
#18814 = EDGE_CURVE ( 'NONE', #28805, #16041, #3102, .T. ) ;
#18815 = VERTEX_POINT ( 'NONE', #12066 ) ;
#18816 = CARTESIAN_POINT ( 'NONE',  ( -9.999999999999998224, 1.224646799147353059E-15, -83.74999999999997158 ) ) ;
#18817 = CARTESIAN_POINT ( 'NONE',  ( -9.999999999999998224, 1.224646799147353059E-15, -112.6250000040967763 ) ) ;
#18818 = CARTESIAN_POINT ( 'NONE',  ( 4.999999999999992006, -8.660254037844389075, -38.62500000409676915 ) ) ;
#18819 = CARTESIAN_POINT ( 'NONE',  ( 5.405949406249999534, 9.363379034771803333, -74.59375000204838102 ) ) ;
#18820 = CARTESIAN_POINT ( 'NONE',  ( -4.999999999999996447, 8.660254037844387298, -38.99999999999997868 ) ) ;
#18821 = CARTESIAN_POINT ( 'NONE',  ( -10.00000000000000000, -5.773502691896251982, -24.00000000409677625 ) ) ;
#18822 = CARTESIAN_POINT ( 'NONE',  ( -10.81189881249999729, -6.242252689847864744, -50.15625000204837391 ) ) ;
#18823 = CARTESIAN_POINT ( 'NONE',  ( -2.121150477449813534E-15, -11.54700538379251284, -157.2500000040968189 ) ) ;
#18824 = CARTESIAN_POINT ( 'NONE',  ( 10.81189881249999907, 6.242252689847868297, -34.40625000204835970 ) ) ;
#18825 = CARTESIAN_POINT ( 'NONE',  ( 57.00000000000002132, 0.000000000000000000, -240.0000000000000000 ) ) ;
#18826 = CARTESIAN_POINT ( 'NONE',  ( 5.405949406249992428, -9.363379034771808662, -141.2812500020483810 ) ) ;
#18827 = CARTESIAN_POINT ( 'NONE',  ( 10.81189881249999551, -6.242252689847874514, -147.1562500020484094 ) ) ;
#18828 = CARTESIAN_POINT ( 'NONE',  ( 9.999999999999998224, 0.000000000000000000, -153.5000000000000000 ) ) ;
#18829 = EDGE_CURVE ( 'NONE', #26311, #27538, #20730, .T. ) ;
#18830 = CARTESIAN_POINT ( 'NONE',  ( -9.999999999999998224, 1.224646799147353059E-15, -200.0000000000000000 ) ) ;
#18831 = ORIENTED_EDGE ( 'NONE', *, *, #4082, .T. ) ;
#18832 = EDGE_CURVE ( 'NONE', #20303, #29817, #41837, .T. ) ;
#18833 = VERTEX_POINT ( 'NONE', #7089 ) ;
#18834 = ORIENTED_EDGE ( 'NONE', *, *, #32055, .T. ) ;
#18835 = EDGE_CURVE ( 'NONE', #8170, #4745, #20239, .T. ) ;
#18836 = DIRECTION ( 'NONE',  ( -0.000000000000000000, -0.000000000000000000, 1.000000000000000000 ) ) ;
#18837 =( BOUNDED_CURVE ( )  B_SPLINE_CURVE ( 2, ( #9600, #19733, #19943, #26430, #36562, #29890, #26854 ),
 .UNSPECIFIED., .F., .F. ) 
 B_SPLINE_CURVE_WITH_KNOTS ( ( 3, 2, 2, 3 ),
 ( 0.4552238805970150737, 0.4564676616915424590, 0.4577114427860698442, 0.4589552238805971740 ),
 .UNSPECIFIED. ) 
 CURVE ( )  GEOMETRIC_REPRESENTATION_ITEM ( )  RATIONAL_B_SPLINE_CURVE ( ( 0.9999999999999820144, 0.8660254037844566932, 1.000000000000000000, 0.8660254037844387076, 1.000000000000000000, 0.8660254037844207220, 1.000000000000017986 ) ) 
 REPRESENTATION_ITEM ( '' )  );
#18838 = CARTESIAN_POINT ( 'NONE',  ( 10.81189881249999551, -6.242252689847874514, -179.9687500020484094 ) ) ;
#18839 = CARTESIAN_POINT ( 'NONE',  ( -2.293366432827344421E-15, -12.48450537969573659, -30.21875000204834905 ) ) ;
#18840 = LINE ( 'NONE', #32231, #6734 ) ;
#18841 = CARTESIAN_POINT ( 'NONE',  ( -5.405949406249996869, 9.363379034771805109, -162.8437500020484094 ) ) ;
#18842 = CARTESIAN_POINT ( 'NONE',  ( 10.81189881249999551, -6.242252689847874514, -154.4687500020484094 ) ) ;
#18843 = EDGE_CURVE ( 'NONE', #12639, #6263, #35376, .T. ) ;
#18844 = CARTESIAN_POINT ( 'NONE',  ( 9.999999999999998224, 0.000000000000000000, -89.37500000409677625 ) ) ;
#18845 = CARTESIAN_POINT ( 'NONE',  ( -5.405949406249996869, 9.363379034771805109, -132.8437500020484094 ) ) ;
#18846 = CARTESIAN_POINT ( 'NONE',  ( -10.81189881249999729, 1.324075727343319199E-15, -140.2812500020483810 ) ) ;
#18847 = CARTESIAN_POINT ( 'NONE',  ( 9.999999999999479527, 5.773502691896553074, -144.3750000000000000 ) ) ;
#18848 = CARTESIAN_POINT ( 'NONE',  ( 10.81189881249999551, -6.242252689847874514, -145.4687500020484094 ) ) ;
#18849 = CARTESIAN_POINT ( 'NONE',  ( -9.999999999999998224, 1.224646799147353059E-15, -200.0000000000000000 ) ) ;
#18850 =( BOUNDED_CURVE ( )  B_SPLINE_CURVE ( 2, ( #30888, #11443, #27647, #1975, #18355, #11654, #24854 ),
 .UNSPECIFIED., .F., .F. ) 
 B_SPLINE_CURVE_WITH_KNOTS ( ( 3, 2, 2, 3 ),
 ( 0.7574626865671643117, 0.7587064676616916969, 0.7599502487562190822, 0.7611940298507464675 ),
 .UNSPECIFIED. ) 
 CURVE ( )  GEOMETRIC_REPRESENTATION_ITEM ( )  RATIONAL_B_SPLINE_CURVE ( ( 0.9999999999999880096, 0.8660254037844506980, 1.000000000000000000, 0.8660254037844387076, 1.000000000000000000, 0.8660254037844148378, 1.000000000000023981 ) ) 
 REPRESENTATION_ITEM ( '' )  );
#18851 = CARTESIAN_POINT ( 'NONE',  ( -4.999999999999996447, 8.660254037844387298, -33.37500000409676915 ) ) ;
#18852 = CARTESIAN_POINT ( 'NONE',  ( -2.121150477449813534E-15, -11.54700538379251284, -168.8750000000000000 ) ) ;
#18853 = CARTESIAN_POINT ( 'NONE',  ( 5.405949406249992428, -9.363379034771808662, -82.59375000204836681 ) ) ;
#18854 = CYLINDRICAL_SURFACE ( 'NONE', #34834, 9.999999999999998224 ) ;
#18855 = CARTESIAN_POINT ( 'NONE',  ( -10.81189881249999729, 6.242252689847871849, -50.40625000204837391 ) ) ;
#18856 = FACE_OUTER_BOUND ( 'NONE', #7560, .T. ) ;
#18857 = CARTESIAN_POINT ( 'NONE',  ( -5.405949406250003975, -9.363379034771801557, -172.8437500020484094 ) ) ;
#18858 = CARTESIAN_POINT ( 'NONE',  ( 9.999999999999996447, -5.773502691896262640, -135.6250000000000000 ) ) ;
#18859 = CARTESIAN_POINT ( 'NONE',  ( -5.405949406250003975, -9.363379034771801557, -143.0312500020483810 ) ) ;
#18860 = DIRECTION ( 'NONE',  ( 1.000000000000000000, 0.000000000000000000, 0.000000000000000000 ) ) ;
#18861 = CARTESIAN_POINT ( 'NONE',  ( -2.293366432827344421E-15, -12.48450537969573659, -33.40625000204835970 ) ) ;
#18862 = CARTESIAN_POINT ( 'NONE',  ( 9.999999999999998224, 0.000000000000000000, -125.3750000040967905 ) ) ;
#18863 = CARTESIAN_POINT ( 'NONE',  ( -10.00000000000000000, -5.773502691896251982, -97.12500000000000000 ) ) ;
#18864 = EDGE_CURVE ( 'NONE', #27593, #12898, #32603, .T. ) ;
#18865 = ORIENTED_EDGE ( 'NONE', *, *, #10403, .T. ) ;
#18866 = CARTESIAN_POINT ( 'NONE',  ( 5.405949406249992428, -9.363379034771808662, -121.7812500020483952 ) ) ;
#18867 = CARTESIAN_POINT ( 'NONE',  ( -4.999999999999996447, 8.660254037844387298, -138.3750000040967905 ) ) ;
#18868 = DIRECTION ( 'NONE',  ( -0.000000000000000000, -0.000000000000000000, 1.000000000000000000 ) ) ;
#18869 = CARTESIAN_POINT ( 'NONE',  ( 10.81189881249999907, 6.242252689847868297, -172.4062500020484094 ) ) ;
#18870 = CARTESIAN_POINT ( 'NONE',  ( -9.999999999999998224, 1.224646799147353059E-15, -52.62500000409675494 ) ) ;
#18871 = FACE_OUTER_BOUND ( 'NONE', #20980, .T. ) ;
#18872 = CARTESIAN_POINT ( 'NONE',  ( -10.81189881249999907, -6.242252689847864744, -60.65625000204838813 ) ) ;
#18873 = CARTESIAN_POINT ( 'NONE',  ( 0.000000000000000000, 0.000000000000000000, -170.0000000000000000 ) ) ;
#18874 = CARTESIAN_POINT ( 'NONE',  ( 5.405949406249992428, -9.363379034771808662, -171.2812500020484094 ) ) ;
#18875 = CARTESIAN_POINT ( 'NONE',  ( -9.999999999999998224, 1.224646799147353059E-15, -163.2500000000000000 ) ) ;
#18876 = CARTESIAN_POINT ( 'NONE',  ( 4.999999999999992006, -8.660254037844389075, -56.24999999999996447 ) ) ;
#18877 = ORIENTED_EDGE ( 'NONE', *, *, #6560, .T. ) ;
#18878 = CARTESIAN_POINT ( 'NONE',  ( -9.999999999999998224, 1.224646799147353059E-15, -194.7500000000000000 ) ) ;
#18879 = ADVANCED_FACE ( 'NONE', ( #22857 ), #39459, .T. ) ;
#18880 = CARTESIAN_POINT ( 'NONE',  ( -9.999999999999998224, 1.224646799147353059E-15, -26.74999999999996803 ) ) ;
#18882 = ORIENTED_EDGE ( 'NONE', *, *, #27828, .T. ) ;
#18881 = CARTESIAN_POINT ( 'NONE',  ( -5.405949406249996869, 9.363379034771805109, -74.53125000204838102 ) ) ;
#18883 = DIRECTION ( 'NONE',  ( 1.000000000000000000, 0.000000000000000000, 0.000000000000000000 ) ) ;
#18885 = ORIENTED_EDGE ( 'NONE', *, *, #40947, .F. ) ;
#18884 = CARTESIAN_POINT ( 'NONE',  ( -9.999999999999998224, 1.224646799147353059E-15, -189.1250000040967905 ) ) ;
#18886 = EDGE_LOOP ( 'NONE', ( #5465, #36501, #39209, #29608 ) ) ;
#18887 = CARTESIAN_POINT ( 'NONE',  ( 5.405949406249992428, -9.363379034771808662, -28.59375000204836326 ) ) ;
#18888 = CARTESIAN_POINT ( 'NONE',  ( 7.070501591499376803E-16, 11.54700538379251284, -77.00000000409677625 ) ) ;
#18889 = CARTESIAN_POINT ( 'NONE',  ( 5.405949406249999534, 9.363379034771803333, -7.281250002048378356 ) ) ;
#18891 = EDGE_LOOP ( 'NONE', ( #16360, #21245, #6501 ) ) ;
#18890 = CARTESIAN_POINT ( 'NONE',  ( 10.81189881249999907, 6.242252689847868297, -53.71875000204838102 ) ) ;
#18892 = CARTESIAN_POINT ( 'NONE',  ( -10.00000000000154188, 5.773502691895366468, -28.37499999999993605 ) ) ;
#18893 = CARTESIAN_POINT ( 'NONE',  ( -4.999999999999996447, 8.660254037844387298, -35.99999999999997868 ) ) ;
#18894 = CARTESIAN_POINT ( 'NONE',  ( -5.405949406250003975, -9.363379034771801557, -189.3437500020483810 ) ) ;
#18895 = CARTESIAN_POINT ( 'NONE',  ( 5.405949406249999534, 9.363379034771803333, -175.0937500020484094 ) ) ;
#18896 = CARTESIAN_POINT ( 'NONE',  ( -10.81189881249999729, 6.242252689847871849, -156.7187500020483810 ) ) ;
#18897 = CARTESIAN_POINT ( 'NONE',  ( -10.81189881249999729, 1.324075727343319199E-15, -171.5937500020484094 ) ) ;
#18898 = LINE ( 'NONE', #21922, #24725 ) ;
#18899 = CARTESIAN_POINT ( 'NONE',  ( -9.999999999999998224, 1.224646799147353059E-15, -131.7499999999999716 ) ) ;
#18900 = CARTESIAN_POINT ( 'NONE',  ( 4.999999999999992006, -8.660254037844389075, -192.7500000000000000 ) ) ;
#18901 = CARTESIAN_POINT ( 'NONE',  ( 5.405949406249999534, 9.363379034771803333, -103.0937500020483810 ) ) ;
#18902 = CARTESIAN_POINT ( 'NONE',  ( 9.999999999999932498, 5.773502691896291950, -196.8750000000000284 ) ) ;
#18903 = CARTESIAN_POINT ( 'NONE',  ( -10.81189881249999729, 1.324075727343319199E-15, -77.28125000204838102 ) ) ;
#18904 = CARTESIAN_POINT ( 'NONE',  ( 5.405949406249999534, 9.363379034771803333, -92.59375000204838102 ) ) ;
#18905 = CARTESIAN_POINT ( 'NONE',  ( 5.405949406249999534, 9.363379034771803333, -61.28125000204837391 ) ) ;
#18906 = CARTESIAN_POINT ( 'NONE',  ( -4.999999999999996447, 8.660254037844387298, -144.3750000040967905 ) ) ;
#18907 = CARTESIAN_POINT ( 'NONE',  ( -2.121150477449813534E-15, -11.54700538379251284, -123.8749999999999858 ) ) ;
#18908 = ORIENTED_EDGE ( 'NONE', *, *, #11028, .T. ) ;
#18909 = CARTESIAN_POINT ( 'NONE',  ( -10.81189881249999729, 6.242252689847871849, -138.9062500020484094 ) ) ;
#18910 = CARTESIAN_POINT ( 'NONE',  ( -10.81189881249999729, 1.324075727343319199E-15, -159.7812500020484094 ) ) ;
#18911 = CARTESIAN_POINT ( 'NONE',  ( -2.293366432827344421E-15, -12.48450537969573659, -196.9062500020484094 ) ) ;
#18912 = CARTESIAN_POINT ( 'NONE',  ( 9.999999999999998224, 0.000000000000000000, -105.4999999999999858 ) ) ;
#18913 = CARTESIAN_POINT ( 'NONE',  ( -10.81189881249999729, 6.242252689847871849, -86.21875000204838102 ) ) ;
#18914 = VERTEX_POINT ( 'NONE', #6872 ) ;
#18915 = CARTESIAN_POINT ( 'NONE',  ( -2.121150477449813534E-15, -11.54700538379251284, -68.37499999999998579 ) ) ;
#18916 = CARTESIAN_POINT ( 'NONE',  ( 10.81189881249999551, -6.242252689847874514, -196.4687500020484094 ) ) ;
#18917 = CARTESIAN_POINT ( 'NONE',  ( 5.000000000000000000, 8.660254037844385522, -71.12500000409677625 ) ) ;
#18918 = CARTESIAN_POINT ( 'NONE',  ( 9.999999999999998224, 0.000000000000000000, -165.5000000000000000 ) ) ;
#18919 = CARTESIAN_POINT ( 'NONE',  ( -5.000000000000003553, -8.660254037844383745, -118.0000000000000000 ) ) ;
#18920 = CARTESIAN_POINT ( 'NONE',  ( -5.405949406249996869, 9.363379034771805109, -92.53125000204838102 ) ) ;
#18921 = CARTESIAN_POINT ( 'NONE',  ( 5.405949406249992428, -9.363379034771808662, -64.78125000204838102 ) ) ;
#18922 = CARTESIAN_POINT ( 'NONE',  ( -10.00000000000000000, -5.773502691896251982, -72.00000000409674783 ) ) ;
#18923 = CARTESIAN_POINT ( 'NONE',  ( 9.999999999999479527, 5.773502691896553074, -93.75000000409674783 ) ) ;
#18924 = CARTESIAN_POINT ( 'NONE',  ( 5.405949406249992428, -9.363379034771808662, -22.59375000204835615 ) ) ;
#18925 = EDGE_LOOP ( 'NONE', ( #5604, #15408, #20995, #10321 ) ) ;
#18926 = CARTESIAN_POINT ( 'NONE',  ( -5.405949406249996869, 9.363379034771805109, -193.0312500020484094 ) ) ;
#18927 = EDGE_CURVE ( 'NONE', #4329, #17318, #27927, .T. ) ;
#18928 = CARTESIAN_POINT ( 'NONE',  ( 7.644554776091147741E-16, 12.48450537969573659, -20.65625000204837747 ) ) ;
#18929 = CARTESIAN_POINT ( 'NONE',  ( -2.293366432827344421E-15, -12.48450537969573659, -6.218750002048345493 ) ) ;
#18930 = CARTESIAN_POINT ( 'NONE',  ( 9.999999999999998224, 0.000000000000000000, -137.3750000040967905 ) ) ;
#18931 = CARTESIAN_POINT ( 'NONE',  ( 4.999999999999992006, -8.660254037844389075, -50.24999999999998579 ) ) ;
#18932 = CARTESIAN_POINT ( 'NONE',  ( 10.00000000000076916, -5.773502691895816774, -112.0000000040967620 ) ) ;
#18933 = CARTESIAN_POINT ( 'NONE',  ( -9.999999999999998224, 5.773502691896259087, -178.3750000000000000 ) ) ;
#18934 = DIRECTION ( 'NONE',  ( -0.7071067811865459074, 0.000000000000000000, -0.7071067811865491270 ) ) ;
#18936 = VERTEX_POINT ( 'NONE', #9893 ) ;
#18935 = CARTESIAN_POINT ( 'NONE',  ( -2.293366432827344421E-15, -12.48450537969573659, -99.40625000204839523 ) ) ;
#18937 = CARTESIAN_POINT ( 'NONE',  ( 9.999999999999998224, 0.000000000000000000, -164.0000000000000000 ) ) ;
#18938 = VERTEX_POINT ( 'NONE', #39664 ) ;
#18939 = VERTEX_POINT ( 'NONE', #29974 ) ;
#18940 = ADVANCED_FACE ( 'NONE', ( #32997 ), #26722, .T. ) ;
#18941 = CARTESIAN_POINT ( 'NONE',  ( 10.81189881249999551, -6.242252689847874514, -31.65625000204834905 ) ) ;
#18942 = CARTESIAN_POINT ( 'NONE',  ( -2.293366432827344421E-15, -12.48450537969573659, -81.21875000204838102 ) ) ;
#18943 = CARTESIAN_POINT ( 'NONE',  ( 4.999999999999992006, -8.660254037844389075, -173.2500000000000284 ) ) ;
#18944 = CARTESIAN_POINT ( 'NONE',  ( -5.405949406249996869, 9.363379034771805109, -197.3437500020484094 ) ) ;
#18945 = FACE_OUTER_BOUND ( 'NONE', #33907, .T. ) ;
#18946 = CARTESIAN_POINT ( 'NONE',  ( -10.00000000000076916, 5.773502691895813221, -128.8749999999999716 ) ) ;
#18947 = CARTESIAN_POINT ( 'NONE',  ( -2.293366432827344421E-15, -12.48450537969573659, -156.4062500020483810 ) ) ;
#18948 = CARTESIAN_POINT ( 'NONE',  ( 5.000000000000000000, 8.660254037844385522, -8.125000004096744277 ) ) ;
#18949 = CARTESIAN_POINT ( 'NONE',  ( -10.81189881249999729, 1.324075727343319199E-15, -126.5937500020483668 ) ) ;
#18950 = CARTESIAN_POINT ( 'NONE',  ( -5.405949406250003975, -9.363379034771801557, -118.8437500020483810 ) ) ;
#18951 = CARTESIAN_POINT ( 'NONE',  ( -10.81189881249999907, -6.242252689847864744, -73.96875000204836681 ) ) ;
#18952 = CARTESIAN_POINT ( 'NONE',  ( -2.293366432827344421E-15, -12.48450537969573659, -81.40625000204838102 ) ) ;
#18953 = CARTESIAN_POINT ( 'NONE',  ( -2.121150477449813534E-15, -11.54700538379251284, -167.7500000040968189 ) ) ;
#18954 =( BOUNDED_CURVE ( )  B_SPLINE_CURVE ( 2, ( #13547, #4282, #23933, #13334, #10530, #7097, #20249 ),
 .UNSPECIFIED., .F., .F. ) 
 B_SPLINE_CURVE_WITH_KNOTS ( ( 3, 2, 2, 3 ),
 ( 0.2126865671641791633, 0.2139303482587065208, 0.2151741293532339061, 0.2164179104477612636 ),
 .UNSPECIFIED. ) 
 CURVE ( )  GEOMETRIC_REPRESENTATION_ITEM ( )  RATIONAL_B_SPLINE_CURVE ( ( 0.9999999999999940048, 0.8660254037844447028, 1.000000000000000000, 0.8660254037844387076, 1.000000000000000000, 0.8660254037844297148, 1.000000000000008882 ) ) 
 REPRESENTATION_ITEM ( '' )  );
#18955 = CARTESIAN_POINT ( 'NONE',  ( 10.00000000000102318, -5.773502691895667560, -66.62499999999995737 ) ) ;
#18956 = CARTESIAN_POINT ( 'NONE',  ( 5.405949406249992428, -9.363379034771808662, -171.2812500020484094 ) ) ;
#18957 = CARTESIAN_POINT ( 'NONE',  ( -5.405949406249996869, 9.363379034771805109, -185.5312500020484094 ) ) ;
#18958 = CARTESIAN_POINT ( 'NONE',  ( -2.293366432827344421E-15, -12.48450537969573659, -43.71875000204835970 ) ) ;
#18959 = CARTESIAN_POINT ( 'NONE',  ( -5.000000000000003553, -8.660254037844383745, -164.8750000040967905 ) ) ;
#18960 = CARTESIAN_POINT ( 'NONE',  ( -2.293366432827344421E-15, -12.48450537969573659, -6.406250002048362369 ) ) ;
#18961 = CARTESIAN_POINT ( 'NONE',  ( -10.81189881249999729, 6.242252689847871849, -17.21875000204836681 ) ) ;
#18962 = DIRECTION ( 'NONE',  ( 1.000000000000000000, 0.000000000000000000, 0.000000000000000000 ) ) ;
#18963 = CARTESIAN_POINT ( 'NONE',  ( 10.81189881249999551, -6.242252689847874514, -118.4687500020483810 ) ) ;
#18964 = CARTESIAN_POINT ( 'NONE',  ( 5.000000000000000000, 8.660254037844385522, -87.24999999999998579 ) ) ;
#18965 = CARTESIAN_POINT ( 'NONE',  ( 5.405949406249992428, -9.363379034771808662, -22.78125000204836326 ) ) ;
#18966 = CARTESIAN_POINT ( 'NONE',  ( 9.999999999999998224, 0.000000000000000000, -101.3750000040967905 ) ) ;
#18967 = CARTESIAN_POINT ( 'NONE',  ( -9.999999999999998224, 1.224646799147353059E-15, -190.6250000040967905 ) ) ;
#18968 = CARTESIAN_POINT ( 'NONE',  ( -2.293366432827344421E-15, -12.48450537969573659, -112.9062500020483952 ) ) ;
#18969 = CARTESIAN_POINT ( 'NONE',  ( -5.405949406249996869, 9.363379034771805109, -89.53125000204838102 ) ) ;
#18970 = EDGE_LOOP ( 'NONE', ( #21841, #26210, #30785, #14501 ) ) ;
#18971 = EDGE_CURVE ( 'NONE', #6595, #3659, #32781, .T. ) ;
#18972 = AXIS2_PLACEMENT_3D ( 'NONE', #39191, #25826, #6599 ) ;
#18973 = CARTESIAN_POINT ( 'NONE',  ( -5.000000000000003553, -8.660254037844383745, -89.87500000409677625 ) ) ;
#18974 = CARTESIAN_POINT ( 'NONE',  ( 9.999999999999998224, 0.000000000000000000, -197.3750000040967905 ) ) ;
#18975 = CARTESIAN_POINT ( 'NONE',  ( 10.81189881249999551, -6.242252689847874514, -160.6562500020484379 ) ) ;
#18976 = CARTESIAN_POINT ( 'NONE',  ( 5.405949406249992428, -9.363379034771808662, -48.09375000204838102 ) ) ;
#18977 = ORIENTED_EDGE ( 'NONE', *, *, #39009, .T. ) ;
#18978 = CARTESIAN_POINT ( 'NONE',  ( -9.999999999999998224, 1.224646799147353059E-15, -20.74999999999996447 ) ) ;
#18979 = CARTESIAN_POINT ( 'NONE',  ( 5.405949406249999534, 9.363379034771803333, -26.78125000204836681 ) ) ;
#18980 = CARTESIAN_POINT ( 'NONE',  ( 9.999999999999998224, 0.000000000000000000, -152.0000000000000000 ) ) ;
#18981 = CARTESIAN_POINT ( 'NONE',  ( 9.999999999999998224, 0.000000000000000000, -20.37500000409675494 ) ) ;
#18982 = CARTESIAN_POINT ( 'NONE',  ( -4.999999999999996447, 8.660254037844387298, -199.5000000000000000 ) ) ;
#18984 = ORIENTED_EDGE ( 'NONE', *, *, #14043, .T. ) ;
#18983 = CARTESIAN_POINT ( 'NONE',  ( -5.405949406249996869, 9.363379034771805109, -125.5312500020483952 ) ) ;
#18985 = CARTESIAN_POINT ( 'NONE',  ( 100.0000000000000284, -40.00000000000001421, -170.0000000000000000 ) ) ;
#18986 = VECTOR ( 'NONE', #5335, 1000.000000000000000 ) ;
#18987 = EDGE_LOOP ( 'NONE', ( #26449, #9798, #24801, #21909, #30622 ) ) ;
#18988 = CARTESIAN_POINT ( 'NONE',  ( 10.81189881249999907, 6.242252689847868297, -50.90625000204838102 ) ) ;
#18989 = DATE_TIME_ROLE ( 'classification_date' ) ;
#18990 = CARTESIAN_POINT ( 'NONE',  ( -5.405949406250003975, -9.363379034771801557, -106.8437500020483810 ) ) ;
#18991 = EDGE_CURVE ( 'NONE', #21406, #7623, #3008, .T. ) ;
#18993 = ORIENTED_EDGE ( 'NONE', *, *, #26217, .F. ) ;
#18992 = ORIENTED_EDGE ( 'NONE', *, *, #21916, .T. ) ;
#18994 = AXIS2_PLACEMENT_3D ( 'NONE', #33282, #26369, #9951 ) ;
#18995 = CARTESIAN_POINT ( 'NONE',  ( 0.000000000000000000, 0.000000000000000000, -200.0000000000000000 ) ) ;
#18996 = CARTESIAN_POINT ( 'NONE',  ( 0.000000000000000000, 0.000000000000000000, -200.0000000000000000 ) ) ;
#18997 = CARTESIAN_POINT ( 'NONE',  ( -10.81189881249999729, 6.242252689847871849, -159.7187500020483526 ) ) ;
#18998 = CARTESIAN_POINT ( 'NONE',  ( -10.81189881249999907, -6.242252689847864744, -177.6562500020484094 ) ) ;
#18999 = CARTESIAN_POINT ( 'NONE',  ( -10.81189881249999907, -6.242252689847864744, -6.468750002048346381 ) ) ;
#19000 = CARTESIAN_POINT ( 'NONE',  ( -9.999999999999998224, 1.224646799147353059E-15, -139.2499999999999716 ) ) ;
#19001 = CARTESIAN_POINT ( 'NONE',  ( -10.81189881249999729, -6.242252689847864744, -142.9687500020483810 ) ) ;
#19002 = CARTESIAN_POINT ( 'NONE',  ( 5.405949406249999534, 9.363379034771803333, -106.0937500020483810 ) ) ;
#19003 = CARTESIAN_POINT ( 'NONE',  ( 9.999999999999998224, 0.000000000000000000, -143.0000000000000000 ) ) ;
#19004 = CARTESIAN_POINT ( 'NONE',  ( 5.405949406249999534, 9.363379034771803333, -116.7812500020483952 ) ) ;
#19005 = CARTESIAN_POINT ( 'NONE',  ( -4.999999999999996447, 8.660254037844387298, -192.3750000040967905 ) ) ;
#19006 = CARTESIAN_POINT ( 'NONE',  ( -5.405949406249996869, 9.363379034771805109, -119.3437500020483810 ) ) ;
#19007 = CARTESIAN_POINT ( 'NONE',  ( 10.81189881249999729, 0.000000000000000000, -196.5312500020484094 ) ) ;
#19008 = CARTESIAN_POINT ( 'NONE',  ( -9.999999999999998224, 1.224646799147353059E-15, -47.74999999999998579 ) ) ;
#19009 = CARTESIAN_POINT ( 'NONE',  ( 5.000000000000000000, 8.660254037844385522, -136.7499999999999716 ) ) ;
#19010 = CARTESIAN_POINT ( 'NONE',  ( -4.999999999999996447, 8.660254037844387298, -14.99999999999995737 ) ) ;
#19011 = CARTESIAN_POINT ( 'NONE',  ( -5.405949406250003975, -9.363379034771801557, -66.34375000204836681 ) ) ;
#19012 = CARTESIAN_POINT ( 'NONE',  ( -5.405949406250003975, -9.363379034771801557, -54.34375000204835970 ) ) ;
#19013 = CARTESIAN_POINT ( 'NONE',  ( -2.121150477449813534E-15, -11.54700538379251284, -191.7500000040967905 ) ) ;
#19014 = CARTESIAN_POINT ( 'NONE',  ( 7.644554776091147741E-16, 12.48450537969573659, -23.65625000204838102 ) ) ;
#19015 = CARTESIAN_POINT ( 'NONE',  ( 10.81189881249999907, 6.242252689847868297, -40.21875000204835970 ) ) ;
#19016 = CARTESIAN_POINT ( 'NONE',  ( -9.999999999999998224, 1.224646799147353059E-15, -116.7499999999999858 ) ) ;
#19017 = CARTESIAN_POINT ( 'NONE',  ( 5.405949406249999534, 9.363379034771803333, -148.0937500020483810 ) ) ;
#19018 = CARTESIAN_POINT ( 'NONE',  ( 5.000000000000000000, 8.660254037844385522, -109.7499999999999858 ) ) ;
#19019 = CARTESIAN_POINT ( 'NONE',  ( -5.000000000000003553, -8.660254037844383745, -101.8750000040967905 ) ) ;
#19020 = CARTESIAN_POINT ( 'NONE',  ( -4.999999999999996447, 8.660254037844387298, -70.49999999999998579 ) ) ;
#19021 = CARTESIAN_POINT ( 'NONE',  ( 5.405949406249992428, -9.363379034771808662, -139.7812500020483810 ) ) ;
#19022 = CARTESIAN_POINT ( 'NONE',  ( 5.405949406249992428, -9.363379034771808662, -112.7812500020483952 ) ) ;
#19023 = ORIENTED_EDGE ( 'NONE', *, *, #26692, .T. ) ;
#19024 = VECTOR ( 'NONE', #39519, 1000.000000000000000 ) ;
#19025 = CARTESIAN_POINT ( 'NONE',  ( -10.00000000000025580, 5.773502691896109873, -121.3749999999999858 ) ) ;
#19026 = CARTESIAN_POINT ( 'NONE',  ( 7.070501591499377789E-16, 11.54700538379251284, -119.0000000040967763 ) ) ;
#19027 = CARTESIAN_POINT ( 'NONE',  ( -9.999999999998969713, -5.773502691896847949, -87.00000000409676204 ) ) ;
#19028 = CARTESIAN_POINT ( 'NONE',  ( -10.81189881249999729, 1.324075727343319199E-15, -71.09375000204836681 ) ) ;
#19029 = CARTESIAN_POINT ( 'NONE',  ( 4.999999999999992006, -8.660254037844389075, -41.24999999999997868 ) ) ;
#19030 = CARTESIAN_POINT ( 'NONE',  ( 4.999999999999992006, -8.660254037844389075, -22.12500000409675494 ) ) ;
#19031 = CARTESIAN_POINT ( 'NONE',  ( -5.405949406250003975, -9.363379034771801557, -53.03125000204836681 ) ) ;
#19032 = AXIS2_PLACEMENT_3D ( 'NONE', #25907, #12510, #25704 ) ;
#19033 = CARTESIAN_POINT ( 'NONE',  ( 9.999999999999994671, -5.773502691896262640, -131.5000000040967905 ) ) ;
#19034 = CARTESIAN_POINT ( 'NONE',  ( 7.644554776091147741E-16, 12.48450537969573659, -40.15625000204836681 ) ) ;
#19035 = CARTESIAN_POINT ( 'NONE',  ( -9.999999999999998224, 1.224646799147353059E-15, -106.2499999999999858 ) ) ;
#19036 = CARTESIAN_POINT ( 'NONE',  ( 10.81189881249999551, -6.242252689847874514, -144.1562500020484094 ) ) ;
#19037 = CARTESIAN_POINT ( 'NONE',  ( -10.81189881249999729, 6.242252689847871849, -150.9062500020484094 ) ) ;
#19038 = DIRECTION ( 'NONE',  ( 1.000000000000000000, 0.000000000000000000, 0.000000000000000000 ) ) ;
#19039 = ORIENTED_EDGE ( 'NONE', *, *, #11302, .F. ) ;
#19040 = ORIENTED_EDGE ( 'NONE', *, *, #41015, .T. ) ;
#19041 = EDGE_CURVE ( 'NONE', #23457, #270, #20473, .T. ) ;
#19042 = EDGE_LOOP ( 'NONE', ( #14230, #22170, #20717, #3023 ) ) ;
#19043 =( BOUNDED_CURVE ( )  B_SPLINE_CURVE ( 2, ( #38166, #28251, #41813, #41387, #28475, #31926, #21766 ),
 .UNSPECIFIED., .F., .F. ) 
 B_SPLINE_CURVE_WITH_KNOTS ( ( 3, 2, 2, 3 ),
 ( 0.003731343283582092950, 0.004975124378109457846, 0.006218905472636822307, 0.007462686567164185901 ),
 .UNSPECIFIED. ) 
 CURVE ( )  GEOMETRIC_REPRESENTATION_ITEM ( )  RATIONAL_B_SPLINE_CURVE ( ( 0.9999999999999996669, 0.8660254037844390407, 1.000000000000000000, 0.8660254037844387076, 1.000000000000000000, 0.8660254037844379305, 1.000000000000000666 ) ) 
 REPRESENTATION_ITEM ( '' )  );
#19044 = EDGE_CURVE ( 'NONE', #134, #35669, #40833, .T. ) ;
#19045 = AXIS2_PLACEMENT_3D ( 'NONE', #17013, #36247, #3665 ) ;
#19046 = CARTESIAN_POINT ( 'NONE',  ( 9.999999999999998224, 0.000000000000000000, -99.87500000409679046 ) ) ;
#19047 = CARTESIAN_POINT ( 'NONE',  ( 10.81189881249999729, 0.000000000000000000, -182.8437500020483810 ) ) ;
#19048 = CARTESIAN_POINT ( 'NONE',  ( -5.405949406249996869, 9.363379034771805109, -32.34375000204836681 ) ) ;
#19049 = CARTESIAN_POINT ( 'NONE',  ( -9.999999999999998224, 1.224646799147353059E-15, -118.2500000000000000 ) ) ;
#19050 = CARTESIAN_POINT ( 'NONE',  ( -10.81189881249999729, 1.324075727343319199E-15, -161.0937500020484094 ) ) ;
#19051 = CARTESIAN_POINT ( 'NONE',  ( 10.81189881249999907, 6.242252689847868297, -152.7187500020483810 ) ) ;
#19052 = CARTESIAN_POINT ( 'NONE',  ( 35.00000000000000711, 4.286263797015737285E-15, -169.9999999999999716 ) ) ;
#19053 = CARTESIAN_POINT ( 'NONE',  ( -5.405949406250003975, -9.363379034771801557, -132.3437500020484094 ) ) ;
#19054 = CARTESIAN_POINT ( 'NONE',  ( 10.81189881249999551, -6.242252689847874514, -144.1562500020484094 ) ) ;
#19055 = CARTESIAN_POINT ( 'NONE',  ( -5.405949406250003975, -9.363379034771801557, -16.84375000204835260 ) ) ;
#19056 = CARTESIAN_POINT ( 'NONE',  ( -10.81189881249999729, 6.242252689847871849, -146.2187500020484094 ) ) ;
#19057 = CARTESIAN_POINT ( 'NONE',  ( -4.999999999999996447, 8.660254037844387298, -127.5000000000000000 ) ) ;
#19058 = CARTESIAN_POINT ( 'NONE',  ( 7.070501591499376803E-16, 11.54700538379251284, -177.5000000040967905 ) ) ;
#19059 = CARTESIAN_POINT ( 'NONE',  ( 9.999999999999996447, -5.773502691896262640, -164.1249999999999716 ) ) ;
#19060 = CARTESIAN_POINT ( 'NONE',  ( 10.81189881249999907, 6.242252689847868297, -80.71875000204838102 ) ) ;
#19061 = CARTESIAN_POINT ( 'NONE',  ( -18.76388374866292708, -2.499999999999947153, 49.99999999999998579 ) ) ;
#19062 = CARTESIAN_POINT ( 'NONE',  ( 10.81189881249999729, 0.000000000000000000, -46.53125000204838813 ) ) ;
#19063 = CARTESIAN_POINT ( 'NONE',  ( 10.81189881249999907, 6.242252689847868297, -58.21875000204838102 ) ) ;
#19064 = CARTESIAN_POINT ( 'NONE',  ( 5.000000000000000000, 8.660254037844385522, -90.62500000409677625 ) ) ;
#19065 = CARTESIAN_POINT ( 'NONE',  ( -5.405949406249996869, 9.363379034771805109, -170.3437500020484094 ) ) ;
#19066 = CARTESIAN_POINT ( 'NONE',  ( -9.999999999999998224, 1.224646799147353059E-15, -134.7499999999999716 ) ) ;
#19067 = CARTESIAN_POINT ( 'NONE',  ( 10.81189881249999551, -6.242252689847874514, -147.1562500020484379 ) ) ;
#19068 = CARTESIAN_POINT ( 'NONE',  ( -9.999999999999998224, 1.224646799147353059E-15, -29.74999999999997158 ) ) ;
#19069 = CARTESIAN_POINT ( 'NONE',  ( 9.999999999999998224, 0.000000000000000000, -119.3750000040967905 ) ) ;
#19070 = CARTESIAN_POINT ( 'NONE',  ( -2.121150477449813534E-15, -11.54700538379251284, -99.87500000000000000 ) ) ;
#19071 = ORIENTED_EDGE ( 'NONE', *, *, #23823, .T. ) ;
#19072 = CARTESIAN_POINT ( 'NONE',  ( 5.405949406249992428, -9.363379034771808662, -118.7812500020483952 ) ) ;
#19073 = CARTESIAN_POINT ( 'NONE',  ( -5.000000000000003553, -8.660254037844383745, -139.3750000040968189 ) ) ;
#19074 = CARTESIAN_POINT ( 'NONE',  ( 4.999999999999992006, -8.660254037844389075, -48.74999999999998579 ) ) ;
#19075 = CARTESIAN_POINT ( 'NONE',  ( -10.81189881249999907, -6.242252689847864744, -171.6562500020484094 ) ) ;
#19076 = CARTESIAN_POINT ( 'NONE',  ( 7.070501591499377789E-16, 11.54700538379251284, -50.00000000409675494 ) ) ;
#19077 = EDGE_CURVE ( 'NONE', #1644, #25640, #29330, .T. ) ;
#19078 = CARTESIAN_POINT ( 'NONE',  ( -9.999999999999998224, 1.224646799147353059E-15, -135.1250000040967620 ) ) ;
#19079 = CARTESIAN_POINT ( 'NONE',  ( -5.405949406249996869, 9.363379034771805109, -62.53125000204837391 ) ) ;
#19080 = DIRECTION ( 'NONE',  ( -0.000000000000000000, -0.000000000000000000, 1.000000000000000000 ) ) ;
#19081 = CARTESIAN_POINT ( 'NONE',  ( 5.405949406249999534, 9.363379034771803333, -167.7812500020484094 ) ) ;
#19082 = CARTESIAN_POINT ( 'NONE',  ( -4.999999999999996447, 8.660254037844387298, -183.3750000040967905 ) ) ;
#19083 = ORIENTED_EDGE ( 'NONE', *, *, #39777, .T. ) ;
#19084 =( BOUNDED_CURVE ( )  B_SPLINE_CURVE ( 2, ( #36823, #39428, #3187, #7265, #33605, #12870, #7058 ),
 .UNSPECIFIED., .F., .F. ) 
 B_SPLINE_CURVE_WITH_KNOTS ( ( 3, 2, 2, 3 ),
 ( 0.5708955223880599616, 0.5721393034825872359, 0.5733830845771146212, 0.5746268656716420065 ),
 .UNSPECIFIED. ) 
 CURVE ( )  GEOMETRIC_REPRESENTATION_ITEM ( )  RATIONAL_B_SPLINE_CURVE ( ( 0.9999999999999761302, 0.8660254037844625774, 1.000000000000000000, 0.8660254037844387076, 1.000000000000000000, 0.8660254037844148378, 1.000000000000023981 ) ) 
 REPRESENTATION_ITEM ( '' )  );
#19085 = CARTESIAN_POINT ( 'NONE',  ( 10.00000000000000000, 5.773502691896255534, -137.2500000040967905 ) ) ;
#19087 = ORIENTED_EDGE ( 'NONE', *, *, #32185, .F. ) ;
#19086 = CARTESIAN_POINT ( 'NONE',  ( -5.405949406250003975, -9.363379034771801557, -78.53125000204838102 ) ) ;
#19088 = DIRECTION ( 'NONE',  ( 1.000000000000000000, 0.000000000000000000, 0.000000000000000000 ) ) ;
#19089 = EDGE_CURVE ( 'NONE', #26720, #21669, #38387, .T. ) ;
#19091 = VERTEX_POINT ( 'NONE', #14381 ) ;
#19090 = CARTESIAN_POINT ( 'NONE',  ( 9.999999999998456346, 5.773502691897149042, -30.37499999999991829 ) ) ;
#19092 = VERTEX_POINT ( 'NONE', #27794 ) ;
#19093 = EDGE_CURVE ( 'NONE', #21961, #14889, #29562, .T. ) ;
#19094 = CARTESIAN_POINT ( 'NONE',  ( -10.81189881249999729, 1.324075727343319199E-15, -26.09375000204835970 ) ) ;
#19095 = CARTESIAN_POINT ( 'NONE',  ( -9.999999999999998224, 1.224646799147353059E-15, -158.7500000000000000 ) ) ;
#19096 = CARTESIAN_POINT ( 'NONE',  ( 10.81189881249999551, -6.242252689847874514, -7.656250002048367698 ) ) ;
#19097 =( BOUNDED_CURVE ( )  B_SPLINE_CURVE ( 2, ( #23756, #23550, #6504, #33271, #6924, #10570, #33689 ),
 .UNSPECIFIED., .F., .F. ) 
 B_SPLINE_CURVE_WITH_KNOTS ( ( 3, 2, 2, 3 ),
 ( 0.3097014925373136052, 0.3109452736318408794, 0.3121890547263682092, 0.3134328358208955390 ),
 .UNSPECIFIED. ) 
 CURVE ( )  GEOMETRIC_REPRESENTATION_ITEM ( )  RATIONAL_B_SPLINE_CURVE ( ( 0.9999999999999820144, 0.8660254037844566932, 1.000000000000000000, 0.8660254037844387076, 1.000000000000000000, 0.8660254037844387076, 1.000000000000000000 ) ) 
 REPRESENTATION_ITEM ( '' )  );
#19100 = EDGE_CURVE ( 'NONE', #5730, #35357, #20659, .T. ) ;
#19099 = VERTEX_POINT ( 'NONE', #24565 ) ;
#19098 = CARTESIAN_POINT ( 'NONE',  ( -10.81189881249999907, -6.242252689847864744, -55.96875000204836681 ) ) ;
#19101 = FACE_OUTER_BOUND ( 'NONE', #41536, .T. ) ;
#19102 = CARTESIAN_POINT ( 'NONE',  ( -4.999999999999996447, 8.660254037844387298, -26.99999999999996803 ) ) ;
#19103 = CARTESIAN_POINT ( 'NONE',  ( -10.81189881249999729, 1.324075727343319199E-15, -188.0937500020483810 ) ) ;
#19104 = CARTESIAN_POINT ( 'NONE',  ( -2.293366432827344421E-15, -12.48450537969573659, -180.2187500020484094 ) ) ;
#19105 = CARTESIAN_POINT ( 'NONE',  ( -10.81189881249999729, 1.324075727343319199E-15, -159.5937500020484094 ) ) ;
#19106 = CARTESIAN_POINT ( 'NONE',  ( 5.405949406249999534, 9.363379034771803333, -170.5937500020484094 ) ) ;
#19107 = CYLINDRICAL_SURFACE ( 'NONE', #5427, 9.999999999999998224 ) ;
#19108 = CARTESIAN_POINT ( 'NONE',  ( 4.999999999999992006, -8.660254037844389075, -191.6250000040967905 ) ) ;
#19109 = CARTESIAN_POINT ( 'NONE',  ( -9.999999999999998224, 5.773502691896259087, -184.3750000000000000 ) ) ;
#19110 = CARTESIAN_POINT ( 'NONE',  ( -10.81189881249999729, 1.324075727343319199E-15, -108.5937500020483810 ) ) ;
#19111 = PLANE ( 'NONE',  #16893 ) ;
#19112 = CARTESIAN_POINT ( 'NONE',  ( 7.644554776091147741E-16, 12.48450537969573659, -71.65625000204836681 ) ) ;
#19113 = CARTESIAN_POINT ( 'NONE',  ( -5.405949406249996869, 9.363379034771805109, -1.031250002048372805 ) ) ;
#19114 = CARTESIAN_POINT ( 'NONE',  ( -5.405949406249996869, 9.363379034771805109, -80.34375000204838102 ) ) ;
#19115 = CARTESIAN_POINT ( 'NONE',  ( -2.293366432827344421E-15, -12.48450537969573659, -57.40625000204838102 ) ) ;
#19116 = CARTESIAN_POINT ( 'NONE',  ( -10.00000000000000000, -5.773502691896251982, -147.0000000040967905 ) ) ;
#19117 = CARTESIAN_POINT ( 'NONE',  ( -4.999999999999996447, 8.660254037844387298, -121.5000000000000000 ) ) ;
#19118 = EDGE_CURVE ( 'NONE', #31902, #31053, #7507, .T. ) ;
#19119 = ORIENTED_EDGE ( 'NONE', *, *, #14286, .T. ) ;
#19120 = CARTESIAN_POINT ( 'NONE',  ( -10.81189881249999729, 6.242252689847871849, -146.4062500020484094 ) ) ;
#19121 = CARTESIAN_POINT ( 'NONE',  ( -2.293366432827344421E-15, -12.48450537969573659, -156.4062500020483810 ) ) ;
#19122 = CARTESIAN_POINT ( 'NONE',  ( -5.405949406250003975, -9.363379034771801557, -194.0312500020484094 ) ) ;
#19123 = CARTESIAN_POINT ( 'NONE',  ( 4.999999999999992006, -8.660254037844389075, -51.74999999999996447 ) ) ;
#19124 = CARTESIAN_POINT ( 'NONE',  ( -5.405949406249996869, 9.363379034771805109, -92.34375000204838102 ) ) ;
#19125 = ORIENTED_EDGE ( 'NONE', *, *, #17469, .F. ) ;
#19126 = CARTESIAN_POINT ( 'NONE',  ( -5.000000000000003553, -8.660254037844383745, -63.99999999999997158 ) ) ;
#19127 = CARTESIAN_POINT ( 'NONE',  ( 5.405949406249992428, -9.363379034771808662, -184.5937500020483810 ) ) ;
#19128 = CARTESIAN_POINT ( 'NONE',  ( -5.000000000000003553, -8.660254037844383745, -74.87500000409677625 ) ) ;
#19129 = DIRECTION ( 'NONE',  ( 1.000000000000000000, 0.000000000000000000, 0.000000000000000000 ) ) ;
#19130 = CARTESIAN_POINT ( 'NONE',  ( -4.999999999999996447, 8.660254037844387298, -139.8750000040968189 ) ) ;
#19131 = CARTESIAN_POINT ( 'NONE',  ( -10.81189881249999729, 6.242252689847871849, -84.90625000204838102 ) ) ;
#19132 = CARTESIAN_POINT ( 'NONE',  ( 7.644554776091147741E-16, 12.48450537969573659, -65.65625000204839523 ) ) ;
#19133 = CARTESIAN_POINT ( 'NONE',  ( 7.070501591499377789E-16, 11.54700538379251284, -57.50000000409677625 ) ) ;
#19134 = CARTESIAN_POINT ( 'NONE',  ( 10.81189881249999729, 0.000000000000000000, -14.84375000204835082 ) ) ;
#19135 = FACE_OUTER_BOUND ( 'NONE', #36605, .T. ) ;
#19136 = CARTESIAN_POINT ( 'NONE',  ( 5.405949406249999534, 9.363379034771803333, -193.2812500020484094 ) ) ;
#19137 = CARTESIAN_POINT ( 'NONE',  ( -5.405949406249996869, 9.363379034771805109, -8.531250002048352599 ) ) ;
#19138 = CARTESIAN_POINT ( 'NONE',  ( -10.81189881249999729, 1.324075727343319199E-15, -8.093750002048343717 ) ) ;
#19139 = CARTESIAN_POINT ( 'NONE',  ( 0.000000000000000000, 20.00000000000000000, -219.9999999999999716 ) ) ;
#19140 = CARTESIAN_POINT ( 'NONE',  ( 9.999999999999998224, 0.000000000000000000, -180.5000000000000000 ) ) ;
#19141 = CARTESIAN_POINT ( 'NONE',  ( 7.070501591499376803E-16, 11.54700538379251284, -159.5000000040968189 ) ) ;
#19142 = CARTESIAN_POINT ( 'NONE',  ( -5.000000000000003553, -8.660254037844383745, -176.5000000000000000 ) ) ;
#19144 = ORIENTED_EDGE ( 'NONE', *, *, #5309, .F. ) ;
#19143 = CARTESIAN_POINT ( 'NONE',  ( 5.405949406249992428, -9.363379034771808662, -103.7812500020483810 ) ) ;
#19145 = FACE_OUTER_BOUND ( 'NONE', #38953, .T. ) ;
#19146 = EDGE_LOOP ( 'NONE', ( #37769, #33779, #14067, #12278 ) ) ;
#19147 = ORIENTED_EDGE ( 'NONE', *, *, #22665, .F. ) ;
#19148 = CARTESIAN_POINT ( 'NONE',  ( -5.405949406249996869, 9.363379034771805109, -28.03125000204837036 ) ) ;
#19149 = APPROVAL_ROLE ( '' ) ;
#19150 = CARTESIAN_POINT ( 'NONE',  ( -5.405949406250003975, -9.363379034771801557, -76.84375000204838102 ) ) ;
#19151 = CYLINDRICAL_SURFACE ( 'NONE', #30513, 9.999999999999998224 ) ;
#19152 = AXIS2_PLACEMENT_3D ( 'NONE', #32135, #12039, #9234 ) ;
#19153 = CARTESIAN_POINT ( 'NONE',  ( 9.099922391974125446, -4.256835254723014828, -100.0000000000000000 ) ) ;
#19154 = CARTESIAN_POINT ( 'NONE',  ( -9.999999999999998224, 0.000000000000000000, -180.0000000000000000 ) ) ;
#19155 = CARTESIAN_POINT ( 'NONE',  ( -2.293366432827344421E-15, -12.48450537969573659, -159.4062500020483810 ) ) ;
#19156 = CARTESIAN_POINT ( 'NONE',  ( -5.000000000000003553, -8.660254037844383745, -13.37500000409674783 ) ) ;
#19157 = CARTESIAN_POINT ( 'NONE',  ( -9.999999999999227285, -5.773502691896698735, -125.6249999999999574 ) ) ;
#19158 = EDGE_CURVE ( 'NONE', #33970, #27845, #16049, .T. ) ;
#19159 = CARTESIAN_POINT ( 'NONE',  ( 10.81189881249999551, -6.242252689847874514, -128.9687500020483810 ) ) ;
#19160 = CARTESIAN_POINT ( 'NONE',  ( 7.644554776091147741E-16, 12.48450537969573659, -98.65625000204838102 ) ) ;
#19161 = CARTESIAN_POINT ( 'NONE',  ( 7.644554776091147741E-16, 12.48450537969573659, -113.4687500020483668 ) ) ;
#19162 =( BOUNDED_CURVE ( )  B_SPLINE_CURVE ( 2, ( #1615, #41066, #37645, #10085, #18206, #21449, #5059 ),
 .UNSPECIFIED., .F., .F. ) 
 B_SPLINE_CURVE_WITH_KNOTS ( ( 3, 2, 2, 3 ),
 ( 0.9365671641791047941, 0.9378109452736321794, 0.9390547263681594536, 0.9402985074626868389 ),
 .UNSPECIFIED. ) 
 CURVE ( )  GEOMETRIC_REPRESENTATION_ITEM ( )  RATIONAL_B_SPLINE_CURVE ( ( 0.9999999999999641398, 0.8660254037844745678, 1.000000000000000000, 0.8660254037844387076, 1.000000000000000000, 0.8660254037844148378, 1.000000000000023981 ) ) 
 REPRESENTATION_ITEM ( '' )  );
#19163 = CARTESIAN_POINT ( 'NONE',  ( 5.405949406249999534, 9.363379034771803333, -80.59375000204838102 ) ) ;
#19164 = CARTESIAN_POINT ( 'NONE',  ( 10.81189881249999551, -6.242252689847874514, -82.65625000204836681 ) ) ;
#19165 = CARTESIAN_POINT ( 'NONE',  ( -2.121150477449813534E-15, -11.54700538379251284, -172.2500000040968189 ) ) ;
#19166 = DIRECTION ( 'NONE',  ( 1.000000000000000000, 0.000000000000000000, 0.000000000000000000 ) ) ;
#19167 = CARTESIAN_POINT ( 'NONE',  ( -10.81189881249999729, -6.242252689847864744, -164.1562500020483810 ) ) ;
#19168 = CARTESIAN_POINT ( 'NONE',  ( 10.81189881249999729, 0.000000000000000000, -178.5312500020483810 ) ) ;
#19169 = CARTESIAN_POINT ( 'NONE',  ( -10.81189881249999729, 1.324075727343319199E-15, -44.09375000204837391 ) ) ;
#19170 = CARTESIAN_POINT ( 'NONE',  ( -10.00000000000000000, -5.773502691896251982, -153.0000000040967905 ) ) ;
#19171 = CARTESIAN_POINT ( 'NONE',  ( 5.405949406249992428, -9.363379034771808662, -0.2812500020483721386 ) ) ;
#19172 = CARTESIAN_POINT ( 'NONE',  ( -10.81189881249999729, 6.242252689847871849, -3.718750002048354819 ) ) ;
#19173 = CARTESIAN_POINT ( 'NONE',  ( -9.999999999999998224, 1.224646799147353059E-15, -200.0000000000000000 ) ) ;
#19174 = CARTESIAN_POINT ( 'NONE',  ( 5.405949406249999534, 9.363379034771803333, -110.5937500020483810 ) ) ;
#19175 = CARTESIAN_POINT ( 'NONE',  ( 9.999999999999998224, 0.000000000000000000, -90.49999999999998579 ) ) ;
#19176 = CARTESIAN_POINT ( 'NONE',  ( 5.405949406249992428, -9.363379034771808662, -15.28125000204835793 ) ) ;
#19177 = CARTESIAN_POINT ( 'NONE',  ( -9.999999999999998224, 5.773502691896259087, -100.7500000040967905 ) ) ;
#19178 = CARTESIAN_POINT ( 'NONE',  ( 9.999999999999998224, 0.000000000000000000, -128.0000000000000000 ) ) ;
#19179 = CARTESIAN_POINT ( 'NONE',  ( -10.81189881249999729, 6.242252689847871849, -107.4062500020483810 ) ) ;
#19180 = CARTESIAN_POINT ( 'NONE',  ( 10.81189881249999729, 6.242252689847867408, -94.40625000204836681 ) ) ;
#19181 = ORIENTED_EDGE ( 'NONE', *, *, #8554, .F. ) ;
#19182 = CARTESIAN_POINT ( 'NONE',  ( 4.999999999999992006, -8.660254037844389075, -95.62500000409677625 ) ) ;
#19183 = CARTESIAN_POINT ( 'NONE',  ( 0.000000000000000000, 0.000000000000000000, -99.99999999999998579 ) ) ;
#19184 = CARTESIAN_POINT ( 'NONE',  ( 10.81189881249999907, 6.242252689847868297, -40.21875000204835970 ) ) ;
#19185 = ORIENTED_EDGE ( 'NONE', *, *, #26161, .T. ) ;
#19186 = CARTESIAN_POINT ( 'NONE',  ( -10.00000000000000000, -5.773502691896251982, -17.62499999999997158 ) ) ;
#19187 = CARTESIAN_POINT ( 'NONE',  ( -4.999999999999996447, 8.660254037844387298, -156.0000000000000000 ) ) ;
#19188 = VECTOR ( 'NONE', #18677, 1000.000000000000000 ) ;
#19189 = CARTESIAN_POINT ( 'NONE',  ( -5.000000000000003553, -8.660254037844383745, -19.37500000409675494 ) ) ;
#19190 = ADVANCED_BREP_SHAPE_REPRESENTATION ( '', ( #1204, #39998 ), #28334 ) ;
#19191 = CARTESIAN_POINT ( 'NONE',  ( -4.999999999999996447, 8.660254037844387298, -195.0000000000000000 ) ) ;
#19193 = ORIENTED_EDGE ( 'NONE', *, *, #32820, .T. ) ;
#19192 = CARTESIAN_POINT ( 'NONE',  ( 7.644554776091147741E-16, 12.48450537969573659, -122.6562500020483952 ) ) ;
#19194 = CARTESIAN_POINT ( 'NONE',  ( 9.999999999999479527, 5.773502691896553074, -117.7500000040968189 ) ) ;
#19195 = ORIENTED_EDGE ( 'NONE', *, *, #2245, .T. ) ;
#19196 = CARTESIAN_POINT ( 'NONE',  ( -10.81189881249999907, -6.242252689847864744, -50.15625000204837391 ) ) ;
#19197 = DATE_TIME_ROLE ( 'classification_date' ) ;
#19198 = CARTESIAN_POINT ( 'NONE',  ( -10.81189881249999907, -6.242252689847864744, -105.4687500020483668 ) ) ;
#19200 = ORIENTED_EDGE ( 'NONE', *, *, #11974, .T. ) ;
#19199 = VERTEX_POINT ( 'NONE', #23923 ) ;
#19201 = FACE_OUTER_BOUND ( 'NONE', #6360, .T. ) ;
#19202 = CARTESIAN_POINT ( 'NONE',  ( -10.00000000000051337, 5.773502691895962435, -144.2500000040967905 ) ) ;
#19203 =( BOUNDED_CURVE ( )  B_SPLINE_CURVE ( 2, ( #5327, #31245, #37918, #31889, #21514, #1673, #24774 ),
 .UNSPECIFIED., .F., .F. ) 
 B_SPLINE_CURVE_WITH_KNOTS ( ( 3, 2, 2, 3 ),
 ( 0.9216417910447763928, 0.9228855721393036671, 0.9241293532338311634, 0.9253731343283585487 ),
 .UNSPECIFIED. ) 
 CURVE ( )  GEOMETRIC_REPRESENTATION_ITEM ( )  RATIONAL_B_SPLINE_CURVE ( ( 0.9999999999999761302, 0.8660254037844625774, 1.000000000000000000, 0.8660254037844387076, 1.000000000000000000, 0.8660254037844028474, 1.000000000000035971 ) ) 
 REPRESENTATION_ITEM ( '' )  );
#19204 = CARTESIAN_POINT ( 'NONE',  ( -10.81189881249999907, -6.242252689847864744, -147.4687500020484094 ) ) ;
#19205 = CARTESIAN_POINT ( 'NONE',  ( -10.81189881249999729, 1.324075727343319199E-15, -182.2812500020483810 ) ) ;
#19206 = CARTESIAN_POINT ( 'NONE',  ( 10.00000000000154010, -5.773502691895370020, -26.12499999999993960 ) ) ;
#19207 = LINE ( 'NONE', #32395, #22485 ) ;
#19208 = CARTESIAN_POINT ( 'NONE',  ( -5.405949406250003975, -9.363379034771801557, -142.8437500020483810 ) ) ;
#19209 = CARTESIAN_POINT ( 'NONE',  ( -10.81189881249999729, 1.324075727343319199E-15, -98.09375000204838102 ) ) ;
#19210 = CARTESIAN_POINT ( 'NONE',  ( 4.999999999999992006, -8.660254037844389075, -143.2500000000000000 ) ) ;
#19211 = CARTESIAN_POINT ( 'NONE',  ( 10.81189881249999729, 0.000000000000000000, -108.0312500020483810 ) ) ;
#19212 = CARTESIAN_POINT ( 'NONE',  ( 9.999999999999998224, 0.000000000000000000, -194.3750000040967905 ) ) ;
#19213 = CARTESIAN_POINT ( 'NONE',  ( 10.81189881249999551, -6.242252689847874514, -118.4687500020483810 ) ) ;
#19214 = CARTESIAN_POINT ( 'NONE',  ( 7.644554776091147741E-16, 12.48450537969573659, -185.6562500020484094 ) ) ;
#19215 = DIRECTION ( 'NONE',  ( 0.8660254037844384856, 0.5000000000000004441, -0.000000000000000000 ) ) ;
#19216 = CARTESIAN_POINT ( 'NONE',  ( -2.121150477449813534E-15, -11.54700538379251284, -141.8750000000000000 ) ) ;
#19217 = CARTESIAN_POINT ( 'NONE',  ( 10.00000000000000000, 5.773502691896255534, -3.374999999999961364 ) ) ;
#19218 = CARTESIAN_POINT ( 'NONE',  ( -5.405949406249996869, 9.363379034771805109, -69.84375000204836681 ) ) ;
#19219 = CARTESIAN_POINT ( 'NONE',  ( 10.81189881249999551, -6.242252689847874514, -49.46875000204835970 ) ) ;
#19220 = CARTESIAN_POINT ( 'NONE',  ( 7.070501591499377789E-16, 11.54700538379251284, -177.5000000040967905 ) ) ;
#19221 = CARTESIAN_POINT ( 'NONE',  ( 7.644554776091147741E-16, 12.48450537969573659, -29.65625000204835970 ) ) ;
#19222 = CARTESIAN_POINT ( 'NONE',  ( 10.81189881249999907, 6.242252689847868297, -29.71875000204834549 ) ) ;
#19223 = CARTESIAN_POINT ( 'NONE',  ( 7.070501591499376803E-16, 11.54700538379251284, -117.1249999999999858 ) ) ;
#19224 = CARTESIAN_POINT ( 'NONE',  ( 10.81189881249999551, -6.242252689847874514, -140.9687500020483810 ) ) ;
#19225 = CARTESIAN_POINT ( 'NONE',  ( 9.999999999999996447, -5.773502691896262640, -114.6249999999999858 ) ) ;
#19226 = CARTESIAN_POINT ( 'NONE',  ( 9.999999999999998224, 0.000000000000000000, -119.3750000040967905 ) ) ;
#19227 = CARTESIAN_POINT ( 'NONE',  ( 9.999999999999998224, 0.000000000000000000, -67.99999999999997158 ) ) ;
#19228 = CARTESIAN_POINT ( 'NONE',  ( 10.81189881249999907, 6.242252689847868297, -136.4062500020484094 ) ) ;
#19229 = CARTESIAN_POINT ( 'NONE',  ( -2.293366432827344421E-15, -12.48450537969573659, -118.9062500020483952 ) ) ;
#19230 = EDGE_CURVE ( 'NONE', #37069, #36923, #32355, .T. ) ;
#19231 = ORIENTED_EDGE ( 'NONE', *, *, #29132, .F. ) ;
#19232 = CARTESIAN_POINT ( 'NONE',  ( -5.000000000000003553, -8.660254037844383745, -176.5000000000000000 ) ) ;
#19233 = CARTESIAN_POINT ( 'NONE',  ( -10.00000000000000000, -5.773502691896251982, -118.5000000040967905 ) ) ;
#19234 = PLANE ( 'NONE',  #29819 ) ;
#19235 = CARTESIAN_POINT ( 'NONE',  ( 5.405949406249999534, 9.363379034771803333, -76.09375000204838102 ) ) ;
#19236 = CARTESIAN_POINT ( 'NONE',  ( -4.999999999999996447, 8.660254037844387298, -43.49999999999998579 ) ) ;
#19237 = CARTESIAN_POINT ( 'NONE',  ( -9.999999999999998224, 5.773502691896259087, -27.25000000409677625 ) ) ;
#19238 = CARTESIAN_POINT ( 'NONE',  ( 10.81189881249999551, -6.242252689847874514, -46.65625000204835970 ) ) ;
#19239 = DIRECTION ( 'NONE',  ( -0.000000000000000000, -0.000000000000000000, 1.000000000000000000 ) ) ;
#19240 = CARTESIAN_POINT ( 'NONE',  ( -5.000000000000003553, -8.660254037844383745, -46.37500000409677625 ) ) ;
#19241 = CARTESIAN_POINT ( 'NONE',  ( -2.293366432827344421E-15, -12.48450537969573659, -36.40625000204835970 ) ) ;
#19242 = LINE ( 'NONE', #22922, #19024 ) ;
#19243 = CARTESIAN_POINT ( 'NONE',  ( 10.81189881249999729, 0.000000000000000000, -133.5312500020484094 ) ) ;
#19244 = CARTESIAN_POINT ( 'NONE',  ( 10.81189881249999551, -6.242252689847874514, -153.1562500020484379 ) ) ;
#19245 = CARTESIAN_POINT ( 'NONE',  ( 10.00000000000102318, -5.773502691895667560, -65.12499999999994316 ) ) ;
#19246 = CARTESIAN_POINT ( 'NONE',  ( 9.999999999999998224, 0.000000000000000000, -150.8750000040967905 ) ) ;
#19247 = VERTEX_POINT ( 'NONE', #11156 ) ;
#19248 = ORIENTED_EDGE ( 'NONE', *, *, #21208, .T. ) ;
#19249 = ORIENTED_EDGE ( 'NONE', *, *, #41532, .T. ) ;
#19250 = CARTESIAN_POINT ( 'NONE',  ( -10.81189881249999907, -6.242252689847864744, -169.9687500020484094 ) ) ;
#19251 = AXIS2_PLACEMENT_3D ( 'NONE', #16545, #29743, #9458 ) ;
#19252 = CARTESIAN_POINT ( 'NONE',  ( 10.81189881249999551, -6.242252689847874514, -29.96875000204834549 ) ) ;
#19253 = CARTESIAN_POINT ( 'NONE',  ( -5.000000000000003553, -8.660254037844383745, -61.37500000409676204 ) ) ;
#19254 = CARTESIAN_POINT ( 'NONE',  ( -2.293366432827344421E-15, -12.48450537969573659, -162.2187500020483810 ) ) ;
#19255 = CARTESIAN_POINT ( 'NONE',  ( -5.405949406249996869, 9.363379034771805109, -146.3437500020483810 ) ) ;
#19256 = CARTESIAN_POINT ( 'NONE',  ( 0.000000000000000000, 0.000000000000000000, -200.0000000000000000 ) ) ;
#19257 = CARTESIAN_POINT ( 'NONE',  ( -10.81189881249999907, -6.242252689847864744, -127.9687500020483810 ) ) ;
#19258 = CARTESIAN_POINT ( 'NONE',  ( 10.81189881249999907, 6.242252689847868297, -136.4062500020484094 ) ) ;
#19259 = CARTESIAN_POINT ( 'NONE',  ( 5.405949406249992428, -9.363379034771808662, -16.59375000204835260 ) ) ;
#19260 = CARTESIAN_POINT ( 'NONE',  ( -2.293366432827344421E-15, -12.48450537969573659, -150.2187500020484094 ) ) ;
#19261 = CARTESIAN_POINT ( 'NONE',  ( 9.999999999999998224, 0.000000000000000000, -125.3750000040967905 ) ) ;
#19262 = CARTESIAN_POINT ( 'NONE',  ( 4.999999999999992006, -8.660254037844389075, -165.7500000000000000 ) ) ;
#19263 = CARTESIAN_POINT ( 'NONE',  ( -5.405949406249996869, 9.363379034771805109, -71.34375000204836681 ) ) ;
#19264 = CARTESIAN_POINT ( 'NONE',  ( -10.81189881249999907, -6.242252689847864744, -48.65625000204836681 ) ) ;
#19265 = CARTESIAN_POINT ( 'NONE',  ( -10.81189881249999907, -6.242252689847864744, -64.96875000204838102 ) ) ;
#19266 = CARTESIAN_POINT ( 'NONE',  ( -9.999999999999998224, 1.224646799147353059E-15, -200.0000000000000000 ) ) ;
#19267 = CARTESIAN_POINT ( 'NONE',  ( 5.405949406249992428, -9.363379034771808662, -159.0937500020484094 ) ) ;
#19268 = CARTESIAN_POINT ( 'NONE',  ( 9.999999999999998224, 0.000000000000000000, -134.0000000000000000 ) ) ;
#19269 = CARTESIAN_POINT ( 'NONE',  ( 5.405949406249992428, -9.363379034771808662, -148.7812500020483810 ) ) ;
#19270 = CARTESIAN_POINT ( 'NONE',  ( 4.999999999999992006, -8.660254037844389075, -119.6250000040967905 ) ) ;
#19271 = CARTESIAN_POINT ( 'NONE',  ( 9.999999999999996447, -5.773502691896262640, -89.12499999999997158 ) ) ;
#19272 = ORIENTED_EDGE ( 'NONE', *, *, #16750, .T. ) ;
#19273 = CARTESIAN_POINT ( 'NONE',  ( -5.405949406249996869, 9.363379034771805109, -119.5312500020483952 ) ) ;
#19274 = CARTESIAN_POINT ( 'NONE',  ( 9.999999999999998224, 0.000000000000000000, -143.3750000040967905 ) ) ;
#19275 = CARTESIAN_POINT ( 'NONE',  ( 5.000000000000000000, 8.660254037844385522, -159.2500000000000000 ) ) ;
#19276 = CARTESIAN_POINT ( 'NONE',  ( -5.405949406250003975, -9.363379034771801557, -174.5312500020484094 ) ) ;
#19277 = CARTESIAN_POINT ( 'NONE',  ( -9.999999999999998224, 5.773502691896259087, -48.25000000409676915 ) ) ;
#19278 = EDGE_CURVE ( 'NONE', #23210, #25155, #28192, .T. ) ;
#19279 = CARTESIAN_POINT ( 'NONE',  ( 9.999999999999998224, 0.000000000000000000, -200.0000000000000000 ) ) ;
#19280 = EDGE_CURVE ( 'NONE', #30868, #35982, #33981, .T. ) ;
#19281 = CARTESIAN_POINT ( 'NONE',  ( 10.81189881249999729, 0.000000000000000000, -61.53125000204837391 ) ) ;
#19282 = CARTESIAN_POINT ( 'NONE',  ( -4.999999999999996447, 8.660254037844387298, -44.99999999999998579 ) ) ;
#19283 = CARTESIAN_POINT ( 'NONE',  ( -10.81189881249999729, 6.242252689847871849, -158.4062500020483810 ) ) ;
#19284 = CARTESIAN_POINT ( 'NONE',  ( 10.81189881249999551, -6.242252689847874514, -140.9687500020483810 ) ) ;
#19285 = CARTESIAN_POINT ( 'NONE',  ( 9.999999999999998224, 0.000000000000000000, -100.9999999999999858 ) ) ;
#19286 = DIRECTION ( 'NONE',  ( -0.000000000000000000, -0.000000000000000000, 1.000000000000000000 ) ) ;
#19287 = ORIENTED_EDGE ( 'NONE', *, *, #29928, .T. ) ;
#19288 =( BOUNDED_CURVE ( )  B_SPLINE_CURVE ( 2, ( #32269, #29659, #23175, #20350, #39989, #36128, #9581 ),
 .UNSPECIFIED., .F., .F. ) 
 B_SPLINE_CURVE_WITH_KNOTS ( ( 3, 2, 2, 3 ),
 ( 0.6007462686567165422, 0.6019900497512439275, 0.6032338308457712017, 0.6044776119402985870 ),
 .UNSPECIFIED. ) 
 CURVE ( )  GEOMETRIC_REPRESENTATION_ITEM ( )  RATIONAL_B_SPLINE_CURVE ( ( 0.9999999999999880096, 0.8660254037844506980, 1.000000000000000000, 0.8660254037844387076, 1.000000000000000000, 0.8660254037844267172, 1.000000000000011990 ) ) 
 REPRESENTATION_ITEM ( '' )  );
#19289 = CARTESIAN_POINT ( 'NONE',  ( 10.00000000000102318, -5.773502691895667560, -52.00000000409674072 ) ) ;
#19291 = EDGE_LOOP ( 'NONE', ( #4630, #39311, #8706, #3116 ) ) ;
#19290 = CARTESIAN_POINT ( 'NONE',  ( -10.81189881249999907, -6.242252689847864744, -68.15625000204840944 ) ) ;
#19293 = ORIENTED_EDGE ( 'NONE', *, *, #19400, .T. ) ;
#19292 = CARTESIAN_POINT ( 'NONE',  ( -9.999999999999804601, -5.773502691896363892, -189.0000000040968473 ) ) ;
#19294 = EDGE_LOOP ( 'NONE', ( #33595, #38311, #22028, #3919 ) ) ;
#19295 = CARTESIAN_POINT ( 'NONE',  ( -10.81189881249999729, 6.242252689847871849, -27.71875000204838102 ) ) ;
#19296 = CARTESIAN_POINT ( 'NONE',  ( -79.99999999999994316, -20.00000000000000711, -170.0000000000000000 ) ) ;
#19297 = CARTESIAN_POINT ( 'NONE',  ( 7.644554776091147741E-16, 12.48450537969573659, -4.156250002048351710 ) ) ;
#19298 = CARTESIAN_POINT ( 'NONE',  ( -10.81189881249999729, 1.324075727343319199E-15, -53.09375000204835970 ) ) ;
#19299 = CYLINDRICAL_SURFACE ( 'NONE', #11559, 45.00000000000000711 ) ;
#19300 = CARTESIAN_POINT ( 'NONE',  ( 5.000000000000000000, 8.660254037844385522, -30.24999999999997158 ) ) ;
#19301 = CARTESIAN_POINT ( 'NONE',  ( 10.81189881249999729, 6.242252689847867408, -187.2187500020484094 ) ) ;
#19302 = CARTESIAN_POINT ( 'NONE',  ( -10.81189881249999729, 6.242252689847871849, -170.2187500020483810 ) ) ;
#19303 = CARTESIAN_POINT ( 'NONE',  ( -10.81189881249999907, -6.242252689847864744, -154.9687500020484094 ) ) ;
#19304 = CARTESIAN_POINT ( 'NONE',  ( 10.81189881249999729, 6.242252689847867408, -169.2187500020483810 ) ) ;
#19305 = CARTESIAN_POINT ( 'NONE',  ( 7.070501591499376803E-16, 11.54700538379251284, -124.6249999999999858 ) ) ;
#19306 = CARTESIAN_POINT ( 'NONE',  ( 9.999999999999998224, 0.000000000000000000, -194.0000000000000000 ) ) ;
#19307 = CARTESIAN_POINT ( 'NONE',  ( 5.000000000000000000, 8.660254037844385522, -187.7500000000000000 ) ) ;
#19308 = CARTESIAN_POINT ( 'NONE',  ( -10.81189881249999729, 6.242252689847871849, -104.2187500020483810 ) ) ;
#19309 = PRODUCT_DEFINITION_SHAPE ( 'NONE', 'NONE',  #42694 ) ;
#19310 = CARTESIAN_POINT ( 'NONE',  ( -9.999999999999998224, 1.224646799147353059E-15, -196.2500000000000000 ) ) ;
#19311 = CARTESIAN_POINT ( 'NONE',  ( 10.81189881249999551, -6.242252689847874514, -76.65625000204838102 ) ) ;
#19312 = CARTESIAN_POINT ( 'NONE',  ( -4.999999999999996447, 8.660254037844387298, -96.37500000409677625 ) ) ;
#19313 = CARTESIAN_POINT ( 'NONE',  ( 10.81189881249999551, -6.242252689847874514, -86.96875000204836681 ) ) ;
#19314 = CARTESIAN_POINT ( 'NONE',  ( -10.81189881249999729, 6.242252689847871849, -63.90625000204838813 ) ) ;
#19315 = CARTESIAN_POINT ( 'NONE',  ( 9.999999999999998224, 0.000000000000000000, -149.3750000040967905 ) ) ;
#19316 = CARTESIAN_POINT ( 'NONE',  ( 4.999999999999992006, -8.660254037844389075, -114.7499999999999858 ) ) ;
#19317 = ORIENTED_EDGE ( 'NONE', *, *, #25815, .T. ) ;
#19318 = CARTESIAN_POINT ( 'NONE',  ( 5.405949406249999534, 9.363379034771803333, -142.2812500020483810 ) ) ;
#19319 = CARTESIAN_POINT ( 'NONE',  ( -10.81189881249999729, 6.242252689847871849, -159.9062500020483810 ) ) ;
#19320 = CARTESIAN_POINT ( 'NONE',  ( -10.81189881249999729, 6.242252689847871849, -192.9062500020484094 ) ) ;
#19321 = CARTESIAN_POINT ( 'NONE',  ( 9.999999999999998224, 0.000000000000000000, -161.3750000040967905 ) ) ;
#19322 = CARTESIAN_POINT ( 'NONE',  ( 10.81189881249999907, 6.242252689847868297, -91.21875000204838102 ) ) ;
#19323 = EDGE_LOOP ( 'NONE', ( #8807, #6725, #10419, #14780 ) ) ;
#19324 = CARTESIAN_POINT ( 'NONE',  ( 10.00000000000000000, 5.773502691896255534, -57.37499999999997868 ) ) ;
#19325 = CARTESIAN_POINT ( 'NONE',  ( -10.81189881249999729, 6.242252689847871849, -189.7187500020484379 ) ) ;
#19326 = CARTESIAN_POINT ( 'NONE',  ( 10.00000000000000000, 5.773502691896255534, -77.25000000409677625 ) ) ;
#19327 = EDGE_CURVE ( 'NONE', #35521, #23854, #15027, .T. ) ;
#19328 = ADVANCED_FACE ( 'NONE', ( #18494 ), #1898, .F. ) ;
#19329 = CARTESIAN_POINT ( 'NONE',  ( -9.999999999999998224, 1.224646799147353059E-15, -164.7500000000000000 ) ) ;
#19330 = CARTESIAN_POINT ( 'NONE',  ( -2.121150477449813534E-15, -11.54700538379251284, -123.8749999999999858 ) ) ;
#19331 = EDGE_CURVE ( 'NONE', #14889, #31836, #28657, .T. ) ;
#19332 = CARTESIAN_POINT ( 'NONE',  ( -5.405949406250003975, -9.363379034771801557, -83.03125000204838102 ) ) ;
#19333 = CARTESIAN_POINT ( 'NONE',  ( -10.81189881249999729, 6.242252689847871849, -66.90625000204839523 ) ) ;
#19334 = EDGE_CURVE ( 'NONE', #19666, #32484, #5339, .T. ) ;
#19335 =( BOUNDED_CURVE ( )  B_SPLINE_CURVE ( 2, ( #29603, #6930, #20084, #36289, #16832, #30031, #26784 ),
 .UNSPECIFIED., .F., .F. ) 
 B_SPLINE_CURVE_WITH_KNOTS ( ( 3, 2, 2, 3 ),
 ( 0.3656716417910448325, 0.3669154228855722177, 0.3681592039800996030, 0.3694029850746269883 ),
 .UNSPECIFIED. ) 
 CURVE ( )  GEOMETRIC_REPRESENTATION_ITEM ( )  RATIONAL_B_SPLINE_CURVE ( ( 0.9999999999999940048, 0.8660254037844447028, 1.000000000000000000, 0.8660254037844387076, 1.000000000000000000, 0.8660254037844267172, 1.000000000000011990 ) ) 
 REPRESENTATION_ITEM ( '' )  );
#19336 = CARTESIAN_POINT ( 'NONE',  ( 9.999999999999998224, 0.000000000000000000, -60.87500000409676204 ) ) ;
#19337 = CARTESIAN_POINT ( 'NONE',  ( 7.644554776091147741E-16, 12.48450537969573659, -18.96875000204837036 ) ) ;
#19338 = VERTEX_POINT ( 'NONE', #12222 ) ;
#19339 = CARTESIAN_POINT ( 'NONE',  ( 10.81189881249999551, -6.242252689847874514, -192.1562500020484094 ) ) ;
#19340 = AXIS2_PLACEMENT_3D ( 'NONE', #11382, #24580, #8171 ) ;
#19341 = CARTESIAN_POINT ( 'NONE',  ( 10.81189881249999907, 6.242252689847868297, -11.90625000204836859 ) ) ;
#19342 = CARTESIAN_POINT ( 'NONE',  ( 10.81189881249999729, 0.000000000000000000, -5.843750002048370362 ) ) ;
#19343 = DIRECTION ( 'NONE',  ( 0.000000000000000000, 0.000000000000000000, -1.000000000000000000 ) ) ;
#19344 = CIRCLE ( 'NONE', #41389, 9.999999999999998224 ) ;
#19345 = CARTESIAN_POINT ( 'NONE',  ( -1.040834085586084257E-14, 145.0000000000000000, 7.500000000000003553 ) ) ;
#19346 = APPROVAL ( #38845, 'UNSPECIFIED' ) ;
#19347 = CARTESIAN_POINT ( 'NONE',  ( 24.99999999999999645, 3.061616997868382648E-15, -169.9999999999999716 ) ) ;
#19348 =( BOUNDED_CURVE ( )  B_SPLINE_CURVE ( 2, ( #18086, #21327, #37520, #31280, #34515, #30630, #37735 ),
 .UNSPECIFIED., .F., .F. ) 
 B_SPLINE_CURVE_WITH_KNOTS ( ( 3, 2, 2, 3 ),
 ( 0.3470149253731344974, 0.3482587064676618271, 0.3495024875621891569, 0.3507462686567164867 ),
 .UNSPECIFIED. ) 
 CURVE ( )  GEOMETRIC_REPRESENTATION_ITEM ( )  RATIONAL_B_SPLINE_CURVE ( ( 0.9999999999999820144, 0.8660254037844566932, 1.000000000000000000, 0.8660254037844387076, 1.000000000000000000, 0.8660254037844327124, 1.000000000000005995 ) ) 
 REPRESENTATION_ITEM ( '' )  );
#19349 = CARTESIAN_POINT ( 'NONE',  ( -9.999999999999998224, 5.773502691896259087, -176.8750000000000000 ) ) ;
#19350 = CARTESIAN_POINT ( 'NONE',  ( 9.999999999999998224, 0.000000000000000000, -120.5000000000000000 ) ) ;
#19352 = ORIENTED_EDGE ( 'NONE', *, *, #25815, .F. ) ;
#19351 = CARTESIAN_POINT ( 'NONE',  ( 10.81189881249999729, 0.000000000000000000, -90.03125000204838102 ) ) ;
#19353 = CARTESIAN_POINT ( 'NONE',  ( -7.320507999635632146, -7.320508119598070351, -179.9330127040876732 ) ) ;
#19354 = ADVANCED_FACE ( 'NONE', ( #2116 ), #21738, .T. ) ;
#19355 = ORIENTED_EDGE ( 'NONE', *, *, #16256, .F. ) ;
#19356 = EDGE_LOOP ( 'NONE', ( #21579, #29340, #15520, #39675 ) ) ;
#19357 = CARTESIAN_POINT ( 'NONE',  ( 5.405949406249999534, 9.363379034771803333, -37.09375000204836681 ) ) ;
#19358 = CARTESIAN_POINT ( 'NONE',  ( 10.81189881249999907, 6.242252689847868297, -32.90625000204835970 ) ) ;
#19359 = PERSON_AND_ORGANIZATION ( #5283, #26315 ) ;
#19360 = EDGE_CURVE ( 'NONE', #1371, #28132, #4227, .T. ) ;
#19361 = CARTESIAN_POINT ( 'NONE',  ( 10.81189881249999729, 0.000000000000000000, -77.84375000204838102 ) ) ;
#19362 = CARTESIAN_POINT ( 'NONE',  ( -7.959047257566134870E-15, -145.0000000000000000, 2.499999999999992006 ) ) ;
#19363 = CARTESIAN_POINT ( 'NONE',  ( 10.81189881249999907, 6.242252689847868297, -191.7187500020484094 ) ) ;
#19364 = DIRECTION ( 'NONE',  ( -0.000000000000000000, -0.000000000000000000, 1.000000000000000000 ) ) ;
#19365 = CARTESIAN_POINT ( 'NONE',  ( 9.999999999999998224, 0.000000000000000000, -200.0000000000000000 ) ) ;
#19366 = CARTESIAN_POINT ( 'NONE',  ( -10.81189881249999729, 6.242252689847871849, -159.9062500020483810 ) ) ;
#19367 = CARTESIAN_POINT ( 'NONE',  ( 9.999999999999998224, 0.000000000000000000, -9.875000004096746054 ) ) ;
#19368 = LOCAL_TIME ( 11, 57, 6.000000000000000000, #39358 ) ;
#19369 = CARTESIAN_POINT ( 'NONE',  ( 10.81189881249999907, 6.242252689847868297, -127.2187500020483668 ) ) ;
#19370 = CARTESIAN_POINT ( 'NONE',  ( -10.81189881249999729, 6.242252689847871849, -101.4062500020483952 ) ) ;
#19371 = CARTESIAN_POINT ( 'NONE',  ( -10.81189881249999729, -6.242252689847864744, -108.4687500020483810 ) ) ;
#19372 = EDGE_CURVE ( 'NONE', #22578, #12639, #12013, .T. ) ;
#19373 = CARTESIAN_POINT ( 'NONE',  ( 7.644554776091147741E-16, 12.48450537969573659, -77.46875000204838102 ) ) ;
#19374 = CARTESIAN_POINT ( 'NONE',  ( -10.81189881249999907, -6.242252689847864744, -87.65625000204836681 ) ) ;
#19375 = CARTESIAN_POINT ( 'NONE',  ( 10.00000000000000000, 5.773502691896255534, -171.7500000040967905 ) ) ;
#19376 = CARTESIAN_POINT ( 'NONE',  ( -9.999999999999998224, 0.000000000000000000, -99.99999999999998579 ) ) ;
#19377 = CARTESIAN_POINT ( 'NONE',  ( 7.644554776091147741E-16, 12.48450537969573659, -169.1562500020484094 ) ) ;
#19378 = CARTESIAN_POINT ( 'NONE',  ( -5.405949406249996869, 9.363379034771805109, -178.0312500020483810 ) ) ;
#19379 = CARTESIAN_POINT ( 'NONE',  ( 9.999999999999998224, 0.000000000000000000, -159.8750000040967905 ) ) ;
#19380 = CARTESIAN_POINT ( 'NONE',  ( -10.81189881249999907, -6.242252689847864744, -9.468750002048357928 ) ) ;
#19381 = CARTESIAN_POINT ( 'NONE',  ( -9.999999999998969713, -5.773502691896847949, -60.00000000409674072 ) ) ;
#19382 = CARTESIAN_POINT ( 'NONE',  ( -2.293366432827344421E-15, -12.48450537969573659, -111.2187500020483668 ) ) ;
#19383 = CARTESIAN_POINT ( 'NONE',  ( 7.070501591499377789E-16, 11.54700538379251284, -87.12499999999997158 ) ) ;
#19384 = CARTESIAN_POINT ( 'NONE',  ( -5.405949406250003975, -9.363379034771801557, -15.53125000204835793 ) ) ;
#19385 = CARTESIAN_POINT ( 'NONE',  ( -9.999999999999998224, 1.224646799147353059E-15, -96.12500000409677625 ) ) ;
#19386 = FACE_OUTER_BOUND ( 'NONE', #13075, .T. ) ;
#19387 = CARTESIAN_POINT ( 'NONE',  ( -5.405949406249996869, 9.363379034771805109, -107.5312500020483810 ) ) ;
#19388 = CARTESIAN_POINT ( 'NONE',  ( 7.644554776091147741E-16, 12.48450537969573659, -89.65625000204838102 ) ) ;
#19389 = ORIENTED_EDGE ( 'NONE', *, *, #1611, .F. ) ;
#19390 = CARTESIAN_POINT ( 'NONE',  ( -9.999999999999998224, 5.773502691896259087, -84.25000000409677625 ) ) ;
#19391 = CYLINDRICAL_SURFACE ( 'NONE', #5689, 9.999999999999998224 ) ;
#19392 = CARTESIAN_POINT ( 'NONE',  ( 10.81189881249999551, -6.242252689847874514, -40.46875000204835970 ) ) ;
#19393 = EDGE_LOOP ( 'NONE', ( #9995, #37181, #25679, #38669 ) ) ;
#19394 = CARTESIAN_POINT ( 'NONE',  ( -10.00000000000000000, -5.773502691896251982, -16.12499999999998224 ) ) ;
#19395 = CARTESIAN_POINT ( 'NONE',  ( -5.000000000000003553, -8.660254037844383745, -155.5000000000000000 ) ) ;
#19396 = CARTESIAN_POINT ( 'NONE',  ( 9.999999999999998224, 0.000000000000000000, -9.875000004096746054 ) ) ;
#19397 = VECTOR ( 'NONE', #28768, 1000.000000000000000 ) ;
#19398 = CC_DESIGN_APPROVAL ( #15389, ( #24384 ) ) ;
#19399 = CARTESIAN_POINT ( 'NONE',  ( 9.999999999999998224, 0.000000000000000000, -119.3750000040967905 ) ) ;
#19400 = EDGE_CURVE ( 'NONE', #38971, #30360, #18706, .T. ) ;
#19402 = VERTEX_POINT ( 'NONE', #31465 ) ;
#19401 = CARTESIAN_POINT ( 'NONE',  ( -2.293366432827344421E-15, -12.48450537969573659, -124.9062500020483810 ) ) ;
#19403 = CARTESIAN_POINT ( 'NONE',  ( 9.999999999999998224, 0.000000000000000000, -90.49999999999998579 ) ) ;
#19404 = ORIENTED_EDGE ( 'NONE', *, *, #25324, .T. ) ;
#19405 = CARTESIAN_POINT ( 'NONE',  ( -10.81189881249999729, 6.242252689847871849, -54.90625000204836681 ) ) ;
#19406 = PERSON_AND_ORGANIZATION_ROLE ( 'classification_officer' ) ;
#19407 = AXIS2_PLACEMENT_3D ( 'NONE', #12505, #15528, #38427 ) ;
#19408 = CARTESIAN_POINT ( 'NONE',  ( 10.81189881249999729, 0.000000000000000000, -100.3437500020483810 ) ) ;
#19410 = ORIENTED_EDGE ( 'NONE', *, *, #15854, .T. ) ;
#19409 = EDGE_LOOP ( 'NONE', ( #27089, #29142, #6250, #16075 ) ) ;
#19411 =( BOUNDED_CURVE ( )  B_SPLINE_CURVE ( 2, ( #26877, #27093, #17144, #40442, #10886, #30345, #10462 ),
 .UNSPECIFIED., .F., .F. ) 
 B_SPLINE_CURVE_WITH_KNOTS ( ( 3, 2, 2, 3 ),
 ( 0.4440298507462688282, 0.4452736318407962135, 0.4465174129353234878, 0.4477611940298508730 ),
 .UNSPECIFIED. ) 
 CURVE ( )  GEOMETRIC_REPRESENTATION_ITEM ( )  RATIONAL_B_SPLINE_CURVE ( ( 0.9999999999999820144, 0.8660254037844566932, 1.000000000000000000, 0.8660254037844387076, 1.000000000000000000, 0.8660254037844267172, 1.000000000000011990 ) ) 
 REPRESENTATION_ITEM ( '' )  );
#19412 = CARTESIAN_POINT ( 'NONE',  ( 9.999999999999998224, 0.000000000000000000, -174.8750000040967905 ) ) ;
#19413 = LINE ( 'NONE', #16153, #31147 ) ;
#19414 = CARTESIAN_POINT ( 'NONE',  ( 7.644554776091147741E-16, 12.48450537969573659, -184.1562500020484094 ) ) ;
#19415 = CARTESIAN_POINT ( 'NONE',  ( -10.81189881249999907, -6.242252689847864744, -1.968750002048357262 ) ) ;
#19416 = CARTESIAN_POINT ( 'NONE',  ( 7.644554776091147741E-16, 12.48450537969573659, -128.4687500020483810 ) ) ;
#19417 = CARTESIAN_POINT ( 'NONE',  ( 10.81189881249999907, 6.242252689847868297, -103.2187500020483810 ) ) ;
#19418 = DIRECTION ( 'NONE',  ( 0.000000000000000000, 1.000000000000000000, 0.000000000000000000 ) ) ;
#19419 = CARTESIAN_POINT ( 'NONE',  ( -10.81189881249999907, -6.242252689847864744, -105.6562500020483952 ) ) ;
#19420 = CARTESIAN_POINT ( 'NONE',  ( 9.999999999999996447, -5.773502691896262640, -196.0000000040968189 ) ) ;
#19421 = CARTESIAN_POINT ( 'NONE',  ( -5.405949406249996869, 9.363379034771805109, -116.3437500020483810 ) ) ;
#19422 = AXIS2_PLACEMENT_3D ( 'NONE', #35421, #18363, #21388 ) ;
#19423 = CARTESIAN_POINT ( 'NONE',  ( 10.81189881249999551, -6.242252689847874514, -189.1562500020484094 ) ) ;
#19424 = CARTESIAN_POINT ( 'NONE',  ( -2.121150477449813534E-15, -11.54700538379251284, -185.7500000040967905 ) ) ;
#19425 = CARTESIAN_POINT ( 'NONE',  ( -10.00000000000000000, -5.773502691896251982, -136.1250000000000000 ) ) ;
#19426 = CARTESIAN_POINT ( 'NONE',  ( -10.00000000000000000, -5.773502691896251982, -8.624999999999966249 ) ) ;
#19427 = CARTESIAN_POINT ( 'NONE',  ( 10.81189881249999729, 0.000000000000000000, -68.84375000204836681 ) ) ;
#19428 = CARTESIAN_POINT ( 'NONE',  ( -2.293366432827344421E-15, -12.48450537969573659, -51.21875000204836681 ) ) ;
#19429 = CARTESIAN_POINT ( 'NONE',  ( 10.00000000000000000, 5.773502691896255534, -176.2500000040968189 ) ) ;
#19430 = CARTESIAN_POINT ( 'NONE',  ( -2.293366432827344421E-15, -12.48450537969573659, -16.90625000204838102 ) ) ;
#19431 = CARTESIAN_POINT ( 'NONE',  ( 7.644554776091147741E-16, 12.48450537969573659, -29.46875000204835260 ) ) ;
#19432 = CARTESIAN_POINT ( 'NONE',  ( 5.405949406249999534, 9.363379034771803333, -136.0937500020483810 ) ) ;
#19433 = CARTESIAN_POINT ( 'NONE',  ( -5.000000000000003553, -8.660254037844383745, -116.4999999999999858 ) ) ;
#19434 = CARTESIAN_POINT ( 'NONE',  ( 9.999999999999998224, 0.000000000000000000, -69.49999999999997158 ) ) ;
#19435 = CARTESIAN_POINT ( 'NONE',  ( -5.405949406250003975, -9.363379034771801557, -134.0312500020484094 ) ) ;
#19436 = CARTESIAN_POINT ( 'NONE',  ( -5.405949406249996869, 9.363379034771805109, -115.0312500020483952 ) ) ;
#19437 = ORIENTED_EDGE ( 'NONE', *, *, #42029, .T. ) ;
#19438 = CARTESIAN_POINT ( 'NONE',  ( 9.999999999999998224, 0.000000000000000000, -161.0000000000000000 ) ) ;
#19439 = CARTESIAN_POINT ( 'NONE',  ( -10.00000000000000000, -5.773502691896251982, -108.0000000040967763 ) ) ;
#19440 = CARTESIAN_POINT ( 'NONE',  ( -5.000000000000003553, -8.660254037844383745, -128.5000000000000000 ) ) ;
#19441 = CARTESIAN_POINT ( 'NONE',  ( -5.405949406250003975, -9.363379034771801557, -66.34375000204836681 ) ) ;
#19442 = ORIENTED_EDGE ( 'NONE', *, *, #10897, .T. ) ;
#19443 = CARTESIAN_POINT ( 'NONE',  ( 5.000000000000000000, 8.660254037844385522, -45.24999999999998579 ) ) ;
#19444 = AXIS2_PLACEMENT_3D ( 'NONE', #19586, #613, #16331 ) ;
#19445 = CARTESIAN_POINT ( 'NONE',  ( 9.999999999999996447, -5.773502691896262640, -22.00000000409676915 ) ) ;
#19446 = CARTESIAN_POINT ( 'NONE',  ( -10.81189881249999729, 1.324075727343319199E-15, -45.78125000204838813 ) ) ;
#19447 = CARTESIAN_POINT ( 'NONE',  ( 9.999999999999998224, 0.000000000000000000, -41.37500000409677625 ) ) ;
#19448 = CARTESIAN_POINT ( 'NONE',  ( -9.999999999999998224, 5.773502691896259087, -40.75000000409676204 ) ) ;
#19449 = CARTESIAN_POINT ( 'NONE',  ( -5.405949406250003975, -9.363379034771801557, -39.53125000204838102 ) ) ;
#19450 = CARTESIAN_POINT ( 'NONE',  ( 9.999999999999998224, 0.000000000000000000, -141.5000000000000000 ) ) ;
#19451 = CARTESIAN_POINT ( 'NONE',  ( 5.405949406249992428, -9.363379034771808662, -138.2812500020483810 ) ) ;
#19452 = EDGE_CURVE ( 'NONE', #38772, #19609, #29312, .T. ) ;
#19453 = CARTESIAN_POINT ( 'NONE',  ( -10.81189881249999729, 1.324075727343319199E-15, -153.7812500020484094 ) ) ;
#19454 = CARTESIAN_POINT ( 'NONE',  ( 10.00000000000051159, -5.773502691895965988, -110.1249999999999858 ) ) ;
#19455 = ORIENTED_EDGE ( 'NONE', *, *, #38668, .F. ) ;
#19456 = VECTOR ( 'NONE', #3393, 1000.000000000000000 ) ;
#19457 =( BOUNDED_CURVE ( )  B_SPLINE_CURVE ( 2, ( #42610, #29468, #22993, #39379, #2720, #29684, #29255 ),
 .UNSPECIFIED., .F., .F. ) 
 B_SPLINE_CURVE_WITH_KNOTS ( ( 3, 2, 2, 3 ),
 ( 0.5447761194029852039, 0.5460199004975125892, 0.5472636815920398634, 0.5485074626865672487 ),
 .UNSPECIFIED. ) 
 CURVE ( )  GEOMETRIC_REPRESENTATION_ITEM ( )  RATIONAL_B_SPLINE_CURVE ( ( 0.9999999999999880096, 0.8660254037844506980, 1.000000000000000000, 0.8660254037844387076, 1.000000000000000000, 0.8660254037844267172, 1.000000000000011990 ) ) 
 REPRESENTATION_ITEM ( '' )  );
#19458 = ORIENTED_EDGE ( 'NONE', *, *, #36440, .F. ) ;
#19459 = VERTEX_POINT ( 'NONE', #22377 ) ;
#19460 = ADVANCED_FACE ( 'NONE', ( #2329 ), #31682, .T. ) ;
#19461 = DIRECTION ( 'NONE',  ( -0.000000000000000000, -0.000000000000000000, -1.000000000000000000 ) ) ;
#19462 = CARTESIAN_POINT ( 'NONE',  ( -5.405949406249996869, 9.363379034771805109, -176.3437500020483810 ) ) ;
#19463 = VECTOR ( 'NONE', #13848, 1000.000000000000000 ) ;
#19464 = CARTESIAN_POINT ( 'NONE',  ( 5.405949406249992428, -9.363379034771808662, -21.09375000204835615 ) ) ;
#19465 = CARTESIAN_POINT ( 'NONE',  ( 10.00000000000102318, -5.773502691895667560, -61.00000000409674072 ) ) ;
#19466 = CARTESIAN_POINT ( 'NONE',  ( 10.81189881249999551, -6.242252689847874514, -166.4687500020483810 ) ) ;
#19467 = CARTESIAN_POINT ( 'NONE',  ( -5.405949406250003975, -9.363379034771801557, -145.8437500020483810 ) ) ;
#19468 = CARTESIAN_POINT ( 'NONE',  ( 4.999999999999992006, -8.660254037844389075, -119.2500000000000000 ) ) ;
#19469 = CARTESIAN_POINT ( 'NONE',  ( 10.81189881249999551, -6.242252689847874514, -122.9687500020483810 ) ) ;
#19470 = CARTESIAN_POINT ( 'NONE',  ( -5.405949406250003975, -9.363379034771801557, -135.5312500020484094 ) ) ;
#19471 = CARTESIAN_POINT ( 'NONE',  ( 10.81189881249999907, 6.242252689847868297, -14.71875000204837036 ) ) ;
#19472 = CARTESIAN_POINT ( 'NONE',  ( -10.81189881249999729, -6.242252689847864744, -135.4687500020483810 ) ) ;
#19473 = CARTESIAN_POINT ( 'NONE',  ( 4.999999999999992006, -8.660254037844389075, -125.6250000040967620 ) ) ;
#19474 = CARTESIAN_POINT ( 'NONE',  ( -10.00000000000000000, -5.773502691896251982, -161.6250000000000284 ) ) ;
#19475 = CARTESIAN_POINT ( 'NONE',  ( 9.999999999999998224, 0.000000000000000000, -99.87500000409679046 ) ) ;
#19476 = CARTESIAN_POINT ( 'NONE',  ( -2.293366432827344421E-15, -12.48450537969573659, -72.21875000204835260 ) ) ;
#19477 = CARTESIAN_POINT ( 'NONE',  ( 5.405949406249992428, -9.363379034771808662, -49.78125000204838813 ) ) ;
#19478 = CARTESIAN_POINT ( 'NONE',  ( -10.81189881249999729, 6.242252689847871849, -50.21875000204837391 ) ) ;
#19479 = DIRECTION ( 'NONE',  ( -0.000000000000000000, -0.000000000000000000, 1.000000000000000000 ) ) ;
#19480 = CARTESIAN_POINT ( 'NONE',  ( -10.81189881249999729, 6.242252689847871849, -161.2187500020483526 ) ) ;
#19481 = CARTESIAN_POINT ( 'NONE',  ( -9.999999999999998224, 5.773502691896259087, -140.8750000000000000 ) ) ;
#19482 = CARTESIAN_POINT ( 'NONE',  ( 7.644554776091147741E-16, 12.48450537969573659, -142.1562500020484094 ) ) ;
#19483 = CARTESIAN_POINT ( 'NONE',  ( -9.999999999999479527, -5.773502691896549521, -99.00000000409677625 ) ) ;
#19484 = CARTESIAN_POINT ( 'NONE',  ( -9.999999999999998224, 1.224646799147353059E-15, -111.1250000040967763 ) ) ;
#19485 = CARTESIAN_POINT ( 'NONE',  ( 7.070501591499377789E-16, 11.54700538379251284, -88.62500000000000000 ) ) ;
#19486 = ORIENTED_EDGE ( 'NONE', *, *, #15086, .F. ) ;
#19487 = CARTESIAN_POINT ( 'NONE',  ( -10.81189881249999729, -6.242252689847864744, -114.6562500020483952 ) ) ;
#19488 = CARTESIAN_POINT ( 'NONE',  ( -2.121150477449813534E-15, -11.54700538379251284, -128.7500000040967620 ) ) ;
#19489 = CARTESIAN_POINT ( 'NONE',  ( -5.000000000000003553, -8.660254037844383745, -140.8750000040967905 ) ) ;
#19490 = EDGE_CURVE ( 'NONE', #26724, #16786, #15246, .T. ) ;
#19491 = CARTESIAN_POINT ( 'NONE',  ( -10.81189881249999907, -6.242252689847864744, -176.1562500020483810 ) ) ;
#19492 = CARTESIAN_POINT ( 'NONE',  ( 9.999999999999998224, 0.000000000000000000, -38.37500000409676915 ) ) ;
#19493 = CARTESIAN_POINT ( 'NONE',  ( -9.999999999999998224, 1.224646799147353059E-15, -158.7500000000000000 ) ) ;
#19494 = CARTESIAN_POINT ( 'NONE',  ( 5.405949406249992428, -9.363379034771808662, -58.78125000204836681 ) ) ;
#19495 = ADVANCED_FACE ( 'NONE', ( #18275 ), #25209, .T. ) ;
#19496 = CARTESIAN_POINT ( 'NONE',  ( -9.999999999998969713, -5.773502691896847949, -64.12499999999997158 ) ) ;
#19497 = CARTESIAN_POINT ( 'NONE',  ( -10.81189881249999729, 6.242252689847871849, -161.4062500020483810 ) ) ;
#19498 = CARTESIAN_POINT ( 'NONE',  ( 10.81189881249999551, -6.242252689847874514, -142.4687500020483810 ) ) ;
#19499 = CARTESIAN_POINT ( 'NONE',  ( 10.00000000000000000, 5.773502691896255534, -167.2500000040967905 ) ) ;
#19500 = CARTESIAN_POINT ( 'NONE',  ( 9.999999999999998224, 0.000000000000000000, -114.8750000040967905 ) ) ;
#19501 = VERTEX_POINT ( 'NONE', #14730 ) ;
#19502 = LINE ( 'NONE', #23613, #409 ) ;
#19504 = ORIENTED_EDGE ( 'NONE', *, *, #21741, .T. ) ;
#19503 = CARTESIAN_POINT ( 'NONE',  ( -5.405949406249996869, 9.363379034771805109, -73.03125000204838102 ) ) ;
#19505 = PERSON_AND_ORGANIZATION ( #11915, #17965 ) ;
#19507 = ORIENTED_EDGE ( 'NONE', *, *, #39410, .F. ) ;
#19506 = CARTESIAN_POINT ( 'NONE',  ( 10.81189881249999907, 6.242252689847868297, -118.2187500020483810 ) ) ;
#19508 = ORIENTED_EDGE ( 'NONE', *, *, #523, .F. ) ;
#19509 = CARTESIAN_POINT ( 'NONE',  ( 10.81189881249999729, 0.000000000000000000, -23.84375000204835970 ) ) ;
#19510 = CARTESIAN_POINT ( 'NONE',  ( 5.405949406249999534, 9.363379034771803333, -199.0937500020484094 ) ) ;
#19511 = CARTESIAN_POINT ( 'NONE',  ( 7.644554776091147741E-16, 12.48450537969573659, -47.46875000204836681 ) ) ;
#19512 = CARTESIAN_POINT ( 'NONE',  ( 4.999999999999992006, -8.660254037844389075, -112.1250000040967763 ) ) ;
#19513 = EDGE_CURVE ( 'NONE', #6937, #30149, #34832, .T. ) ;
#19514 = CARTESIAN_POINT ( 'NONE',  ( -10.00000000000000000, -5.773502691896251982, -29.62499999999995737 ) ) ;
#19515 = CARTESIAN_POINT ( 'NONE',  ( 7.644554776091147741E-16, 12.48450537969573659, -186.9687500020484094 ) ) ;
#19516 = CARTESIAN_POINT ( 'NONE',  ( -10.81189881249999907, -6.242252689847864744, -168.4687500020483526 ) ) ;
#19517 = CARTESIAN_POINT ( 'NONE',  ( 7.644554776091147741E-16, 12.48450537969573659, -150.9687500020483810 ) ) ;
#19518 = CARTESIAN_POINT ( 'NONE',  ( 10.81189881249999729, 0.000000000000000000, -167.8437500020484094 ) ) ;
#19519 = CARTESIAN_POINT ( 'NONE',  ( -9.999999999999998224, 1.224646799147353059E-15, -159.1250000040967905 ) ) ;
#19520 = DIRECTION ( 'NONE',  ( -1.000000000000000000, 0.000000000000000000, 0.000000000000000000 ) ) ;
#19521 = CARTESIAN_POINT ( 'NONE',  ( -2.121150477449813534E-15, -11.54700538379251284, -186.8750000000000284 ) ) ;
#19522 = CARTESIAN_POINT ( 'NONE',  ( 5.405949406249999534, 9.363379034771803333, -100.0937500020483810 ) ) ;
#19523 = CARTESIAN_POINT ( 'NONE',  ( 5.000000000000000000, 8.660254037844385522, -108.6250000040967763 ) ) ;
#19524 = CARTESIAN_POINT ( 'NONE',  ( -5.405949406249996869, 9.363379034771805109, -76.03125000204838102 ) ) ;
#19525 = DIRECTION ( 'NONE',  ( -0.000000000000000000, -0.000000000000000000, -1.000000000000000000 ) ) ;
#19526 = CARTESIAN_POINT ( 'NONE',  ( -5.405949406250003975, -9.363379034771801557, -184.8437500020483810 ) ) ;
#19527 = CARTESIAN_POINT ( 'NONE',  ( -5.405949406249996869, 9.363379034771805109, -160.0312500020484094 ) ) ;
#19528 = CARTESIAN_POINT ( 'NONE',  ( 7.644554776091147741E-16, 12.48450537969573659, -56.65625000204838813 ) ) ;
#19529 = CARTESIAN_POINT ( 'NONE',  ( 9.999999999999996447, -5.773502691896262640, -134.5000000040967905 ) ) ;
#19530 = CARTESIAN_POINT ( 'NONE',  ( -9.999999999999998224, 1.224646799147353059E-15, -112.2499999999999858 ) ) ;
#19531 = VERTEX_POINT ( 'NONE', #31171 ) ;
#19532 = CARTESIAN_POINT ( 'NONE',  ( -5.405949406250003975, -9.363379034771801557, -140.0312500020484094 ) ) ;
#19533 = CARTESIAN_POINT ( 'NONE',  ( 10.81189881249999907, 6.242252689847868297, -157.4062500020483810 ) ) ;
#19534 = CARTESIAN_POINT ( 'NONE',  ( -5.405949406250003975, -9.363379034771801557, -195.5312500020484094 ) ) ;
#19535 = CARTESIAN_POINT ( 'NONE',  ( -9.999999999999998224, 1.224646799147353059E-15, -104.7499999999999858 ) ) ;
#19536 = CARTESIAN_POINT ( 'NONE',  ( 10.81189881249999907, 6.242252689847868297, -89.71875000204836681 ) ) ;
#19537 = ORIENTED_EDGE ( 'NONE', *, *, #32848, .T. ) ;
#19538 = CARTESIAN_POINT ( 'NONE',  ( 9.999999999999998224, 0.000000000000000000, -55.99999999999996447 ) ) ;
#19539 = CARTESIAN_POINT ( 'NONE',  ( -10.81189881249999729, 6.242252689847871849, -188.2187500020483810 ) ) ;
#19540 = CARTESIAN_POINT ( 'NONE',  ( -2.121150477449813534E-15, -11.54700538379251284, -73.25000000409674783 ) ) ;
#19541 =( BOUNDED_CURVE ( )  B_SPLINE_CURVE ( 2, ( #22757, #39565, #26837, #16245, #29445, #3539, #6987 ),
 .UNSPECIFIED., .F., .F. ) 
 B_SPLINE_CURVE_WITH_KNOTS ( ( 3, 2, 2, 3 ),
 ( 0.4179104477611941260, 0.4191542288557215112, 0.4203980099502488965, 0.4216417910447762818 ),
 .UNSPECIFIED. ) 
 CURVE ( )  GEOMETRIC_REPRESENTATION_ITEM ( )  RATIONAL_B_SPLINE_CURVE ( ( 0.9999999999999880096, 0.8660254037844506980, 1.000000000000000000, 0.8660254037844387076, 1.000000000000000000, 0.8660254037844207220, 1.000000000000017986 ) ) 
 REPRESENTATION_ITEM ( '' )  );
#19542 = FACE_OUTER_BOUND ( 'NONE', #24787, .T. ) ;
#19543 = CARTESIAN_POINT ( 'NONE',  ( -10.81189881249999729, 1.324075727343319199E-15, -81.78125000204839523 ) ) ;
#19544 = CARTESIAN_POINT ( 'NONE',  ( -5.405949406250003975, -9.363379034771801557, -66.53125000204838102 ) ) ;
#19545 = CARTESIAN_POINT ( 'NONE',  ( 9.999999999999998224, 0.000000000000000000, -57.87500000409676204 ) ) ;
#19546 = CARTESIAN_POINT ( 'NONE',  ( 10.81189881249999729, 0.000000000000000000, -20.84375000204835615 ) ) ;
#19547 = CARTESIAN_POINT ( 'NONE',  ( -9.999999999999227285, -5.773502691896698735, -138.0000000040967620 ) ) ;
#19548 = CARTESIAN_POINT ( 'NONE',  ( -2.293366432827344421E-15, -12.48450537969573659, -184.9062500020484094 ) ) ;
#19549 = CARTESIAN_POINT ( 'NONE',  ( -5.405949406250003975, -9.363379034771801557, -15.53125000204835793 ) ) ;
#19550 = CARTESIAN_POINT ( 'NONE',  ( -4.999999999999996447, 8.660254037844387298, -85.49999999999998579 ) ) ;
#19551 = DIRECTION ( 'NONE',  ( 0.000000000000000000, 0.000000000000000000, -1.000000000000000000 ) ) ;
#19552 = DIRECTION ( 'NONE',  ( 0.000000000000000000, 0.000000000000000000, 1.000000000000000000 ) ) ;
#19553 = CARTESIAN_POINT ( 'NONE',  ( -9.999999999999998224, 1.224646799147353059E-15, -167.7500000000000000 ) ) ;
#19554 = LINE ( 'NONE', #38996, #2080 ) ;
#19556 = ORIENTED_EDGE ( 'NONE', *, *, #36546, .T. ) ;
#19555 = CARTESIAN_POINT ( 'NONE',  ( -2.293366432827344421E-15, -12.48450537969573659, -97.90625000204839523 ) ) ;
#19557 = CARTESIAN_POINT ( 'NONE',  ( 4.999999999999992006, -8.660254037844389075, -181.1250000040967905 ) ) ;
#19559 = ORIENTED_EDGE ( 'NONE', *, *, #19569, .T. ) ;
#19558 = CARTESIAN_POINT ( 'NONE',  ( 10.81189881249999551, -6.242252689847874514, -103.4687500020483668 ) ) ;
#19560 = VERTEX_POINT ( 'NONE', #8287 ) ;
#19561 = CARTESIAN_POINT ( 'NONE',  ( 5.405949406249992428, -9.363379034771808662, -34.59375000204836681 ) ) ;
#19562 = CARTESIAN_POINT ( 'NONE',  ( -10.81189881249999907, -6.242252689847864744, -21.65625000204837036 ) ) ;
#19563 = DATE_TIME_ROLE ( 'classification_date' ) ;
#19564 = EDGE_CURVE ( 'NONE', #4695, #18570, #36990, .T. ) ;
#19565 = CARTESIAN_POINT ( 'NONE',  ( 5.405949406249999534, 9.363379034771803333, -76.09375000204838102 ) ) ;
#19566 = CYLINDRICAL_SURFACE ( 'NONE', #16666, 9.999999999999998224 ) ;
#19567 = EDGE_CURVE ( 'NONE', #12287, #16734, #960, .T. ) ;
#19568 = CARTESIAN_POINT ( 'NONE',  ( -10.81189881249999907, -6.242252689847864744, -193.9687500020484094 ) ) ;
#19569 = EDGE_CURVE ( 'NONE', #27433, #20021, #33736, .T. ) ;
#19570 = CARTESIAN_POINT ( 'NONE',  ( 9.999999999999998224, 0.000000000000000000, -99.49999999999998579 ) ) ;
#19571 = CYLINDRICAL_SURFACE ( 'NONE', #14317, 9.999999999999998224 ) ;
#19572 = CARTESIAN_POINT ( 'NONE',  ( -10.81189881249999907, -6.242252689847864744, -153.6562500020484094 ) ) ;
#19573 = CARTESIAN_POINT ( 'NONE',  ( 10.00000000000000000, 5.773502691896255534, -0.7500000040967473858 ) ) ;
#19574 = CARTESIAN_POINT ( 'NONE',  ( 5.000000000000000000, 8.660254037844385522, -178.7500000000000284 ) ) ;
#19575 = CARTESIAN_POINT ( 'NONE',  ( -10.81189881249999729, 6.242252689847871849, -119.2187500020483810 ) ) ;
#19576 = CARTESIAN_POINT ( 'NONE',  ( 5.405949406249992428, -9.363379034771808662, -97.78125000204839523 ) ) ;
#19577 = CARTESIAN_POINT ( 'NONE',  ( 7.644554776091147741E-16, 12.48450537969573659, -104.4687500020483668 ) ) ;
#19578 = CARTESIAN_POINT ( 'NONE',  ( -10.81189881249999907, -6.242252689847864744, -75.46875000204836681 ) ) ;
#19579 = CARTESIAN_POINT ( 'NONE',  ( 10.81189881249999729, 0.000000000000000000, -87.03125000204838102 ) ) ;
#19580 = CARTESIAN_POINT ( 'NONE',  ( -5.000000000000003553, -8.660254037844383745, -169.3750000040967905 ) ) ;
#19581 =( BOUNDED_CURVE ( )  B_SPLINE_CURVE ( 2, ( #7700, #40904, #5697, #8926, #18036, #4889, #21064 ),
 .UNSPECIFIED., .F., .F. ) 
 B_SPLINE_CURVE_WITH_KNOTS ( ( 3, 2, 2, 3 ),
 ( 0.4701492537313434195, 0.4713930348258707492, 0.4726368159203981900, 0.4738805970149255198 ),
 .UNSPECIFIED. ) 
 CURVE ( )  GEOMETRIC_REPRESENTATION_ITEM ( )  RATIONAL_B_SPLINE_CURVE ( ( 0.9999999999999880096, 0.8660254037844506980, 1.000000000000000000, 0.8660254037844387076, 1.000000000000000000, 0.8660254037844207220, 1.000000000000017986 ) ) 
 REPRESENTATION_ITEM ( '' )  );
#19582 = FACE_OUTER_BOUND ( 'NONE', #31788, .T. ) ;
#19583 = CARTESIAN_POINT ( 'NONE',  ( 10.81189881249999729, 0.000000000000000000, -163.5312500020484094 ) ) ;
#19584 = CARTESIAN_POINT ( 'NONE',  ( 10.81189881249999729, 0.000000000000000000, -177.0312500020483810 ) ) ;
#19585 = CARTESIAN_POINT ( 'NONE',  ( 7.070501591499377789E-16, 11.54700538379251284, -153.5000000040967905 ) ) ;
#19586 = CARTESIAN_POINT ( 'NONE',  ( 0.000000000000000000, 0.000000000000000000, -200.0000000000000000 ) ) ;
#19587 = CARTESIAN_POINT ( 'NONE',  ( 10.81189881249999907, 6.242252689847868297, -8.718750002048359704 ) ) ;
#19588 = CARTESIAN_POINT ( 'NONE',  ( 4.999999999999992006, -8.660254037844389075, -59.62500000409676204 ) ) ;
#19589 = CARTESIAN_POINT ( 'NONE',  ( 10.81189881249999907, 6.242252689847868297, -113.7187500020483810 ) ) ;
#19590 = CARTESIAN_POINT ( 'NONE',  ( -9.999999999999998224, 1.224646799147353059E-15, -85.24999999999997158 ) ) ;
#19591 = CARTESIAN_POINT ( 'NONE',  ( 10.81189881249999907, 6.242252689847868297, -11.90625000204836859 ) ) ;
#19592 = CARTESIAN_POINT ( 'NONE',  ( -5.000000000000003553, -8.660254037844383745, -100.3750000040967905 ) ) ;
#19593 = EDGE_CURVE ( 'NONE', #20886, #2600, #41397, .T. ) ;
#19594 = DIRECTION ( 'NONE',  ( -0.000000000000000000, -0.000000000000000000, 1.000000000000000000 ) ) ;
#19595 = CARTESIAN_POINT ( 'NONE',  ( 10.81189881249999729, 0.000000000000000000, -111.0312500020483810 ) ) ;
#19596 = CARTESIAN_POINT ( 'NONE',  ( 7.644554776091147741E-16, 12.48450537969573659, -95.65625000204838102 ) ) ;
#19597 = VERTEX_POINT ( 'NONE', #40845 ) ;
#19598 =( BOUNDED_CURVE ( )  B_SPLINE_CURVE ( 2, ( #15738, #25070, #28938, #11874, #5200, #38214, #28521 ),
 .UNSPECIFIED., .F., .F. ) 
 B_SPLINE_CURVE_WITH_KNOTS ( ( 3, 2, 2, 3 ),
 ( 0.07835820895522395413, 0.07960199004975131165, 0.08084577114427868305, 0.08208955223880604057 ),
 .UNSPECIFIED. ) 
 CURVE ( )  GEOMETRIC_REPRESENTATION_ITEM ( )  RATIONAL_B_SPLINE_CURVE ( ( 0.9999999999999924505, 0.8660254037844461461, 1.000000000000000000, 0.8660254037844387076, 1.000000000000000000, 0.8660254037844312691, 1.000000000000007550 ) ) 
 REPRESENTATION_ITEM ( '' )  );
#19599 = CARTESIAN_POINT ( 'NONE',  ( 5.000000000000000000, 8.660254037844385522, -81.62500000409676204 ) ) ;
#19600 = DIRECTION ( 'NONE',  ( -0.000000000000000000, -0.000000000000000000, 1.000000000000000000 ) ) ;
#19601 = CARTESIAN_POINT ( 'NONE',  ( 5.405949406249992428, -9.363379034771808662, -45.09375000204837391 ) ) ;
#19602 = ORIENTED_EDGE ( 'NONE', *, *, #29664, .T. ) ;
#19603 = CARTESIAN_POINT ( 'NONE',  ( -5.000000000000003553, -8.660254037844383745, -9.999999999999953815 ) ) ;
#19604 = CARTESIAN_POINT ( 'NONE',  ( 10.00000000000000000, 5.773502691896255534, -145.8750000000000284 ) ) ;
#19605 = EDGE_CURVE ( 'NONE', #26580, #26059, #38140, .T. ) ;
#19606 = CARTESIAN_POINT ( 'NONE',  ( -5.000000000000003553, -8.660254037844383745, -14.87500000409674961 ) ) ;
#19607 = CARTESIAN_POINT ( 'NONE',  ( 10.00000000000000000, 5.773502691896255534, -199.8750000000000284 ) ) ;
#19609 = VERTEX_POINT ( 'NONE', #21007 ) ;
#19608 = CARTESIAN_POINT ( 'NONE',  ( -10.81189881249999729, 1.324075727343319199E-15, -116.2812500020483952 ) ) ;
#19610 = CARTESIAN_POINT ( 'NONE',  ( 9.999999999999998224, 0.000000000000000000, -94.99999999999998579 ) ) ;
#19611 = ORIENTED_EDGE ( 'NONE', *, *, #22023, .T. ) ;
#19612 = CARTESIAN_POINT ( 'NONE',  ( 5.405949406249992428, -9.363379034771808662, -43.78125000204838102 ) ) ;
#19613 = PERSON_AND_ORGANIZATION ( #11915, #17965 ) ;
#19614 = CARTESIAN_POINT ( 'NONE',  ( 10.81189881249999907, 6.242252689847868297, -100.2187500020483810 ) ) ;
#19615 = CARTESIAN_POINT ( 'NONE',  ( 5.405949406249999534, 9.363379034771803333, -124.2812500020483952 ) ) ;
#19617 = ORIENTED_EDGE ( 'NONE', *, *, #7041, .F. ) ;
#19616 = EDGE_CURVE ( 'NONE', #39684, #414, #21220, .T. ) ;
#19618 = CYLINDRICAL_SURFACE ( 'NONE', #19045, 9.999999999999998224 ) ;
#19619 = CARTESIAN_POINT ( 'NONE',  ( -9.999999999999998224, 1.224646799147353059E-15, -85.24999999999997158 ) ) ;
#19620 = EDGE_CURVE ( 'NONE', #32541, #14017, #10858, .T. ) ;
#19621 = CARTESIAN_POINT ( 'NONE',  ( 10.81189881249999551, -6.242252689847874514, -183.1562500020484094 ) ) ;
#19622 = DIRECTION ( 'NONE',  ( -0.000000000000000000, -0.000000000000000000, 1.000000000000000000 ) ) ;
#19623 = CARTESIAN_POINT ( 'NONE',  ( -9.999999999999998224, 1.224646799147353059E-15, -24.12500000409675849 ) ) ;
#19624 = EDGE_CURVE ( 'NONE', #38740, #3867, #23261, .T. ) ;
#19625 = CARTESIAN_POINT ( 'NONE',  ( -5.405949406250003975, -9.363379034771801557, -135.3437500020484094 ) ) ;
#19626 = PRODUCT_DEFINITION ( 'UNKNOWN', '', #2849, #22681 ) ;
#19627 = CARTESIAN_POINT ( 'NONE',  ( -2.293366432827344421E-15, -12.48450537969573659, -103.7187500020483668 ) ) ;
#19628 = PLANE ( 'NONE',  #34609 ) ;
#19629 = CARTESIAN_POINT ( 'NONE',  ( -5.405949406250003975, -9.363379034771801557, -105.5312500020483810 ) ) ;
#19630 = CARTESIAN_POINT ( 'NONE',  ( 9.999999999999998224, 0.000000000000000000, -192.8750000040967905 ) ) ;
#19631 = CARTESIAN_POINT ( 'NONE',  ( -10.81189881249999729, -6.242252689847864744, -115.9687500020483810 ) ) ;
#19632 = CARTESIAN_POINT ( 'NONE',  ( -10.81189881249999729, 6.242252689847871849, -183.9062500020484094 ) ) ;
#19633 = AXIS2_PLACEMENT_3D ( 'NONE', #2584, #15713, #32576 ) ;
#19634 = CARTESIAN_POINT ( 'NONE',  ( 9.999999999997939426, 5.773502691897446581, -6.750000004096692763 ) ) ;
#19635 = CARTESIAN_POINT ( 'NONE',  ( 5.000000000000000000, 8.660254037844385522, -141.2500000000000000 ) ) ;
#19636 = CARTESIAN_POINT ( 'NONE',  ( -4.999999999999996447, 8.660254037844387298, -2.999999999999975131 ) ) ;
#19637 = CARTESIAN_POINT ( 'NONE',  ( -2.293366432827344421E-15, -12.48450537969573659, -63.21875000204839523 ) ) ;
#19638 = CARTESIAN_POINT ( 'NONE',  ( 10.81189881249999907, 6.242252689847868297, -50.71875000204835970 ) ) ;
#19639 = CARTESIAN_POINT ( 'NONE',  ( 5.000000000000000000, 8.660254037844385522, -183.6250000040967905 ) ) ;
#19640 = CARTESIAN_POINT ( 'NONE',  ( -2.293366432827344421E-15, -12.48450537969573659, -19.90625000204837747 ) ) ;
#19641 = CARTESIAN_POINT ( 'NONE',  ( -10.81189881249999729, 1.324075727343319199E-15, -29.09375000204836326 ) ) ;
#19642 = CARTESIAN_POINT ( 'NONE',  ( 9.999999999998969713, 5.773502691896851502, -27.75000000409675494 ) ) ;
#19643 = CARTESIAN_POINT ( 'NONE',  ( -10.81189881249999729, 6.242252689847871849, -134.2187500020483810 ) ) ;
#19644 = CARTESIAN_POINT ( 'NONE',  ( -4.999999999999996447, 8.660254037844387298, -103.5000000000000000 ) ) ;
#19645 = CARTESIAN_POINT ( 'NONE',  ( -5.405949406249996869, 9.363379034771805109, -37.03125000204837391 ) ) ;
#19646 = CARTESIAN_POINT ( 'NONE',  ( -9.999999999999227285, -5.773502691896698735, -115.1249999999999574 ) ) ;
#19647 = CARTESIAN_POINT ( 'NONE',  ( 4.999999999999992006, -8.660254037844389075, -66.74999999999997158 ) ) ;
#19648 = CARTESIAN_POINT ( 'NONE',  ( 5.405949406249999534, 9.363379034771803333, -130.2812500020483810 ) ) ;
#19649 = CARTESIAN_POINT ( 'NONE',  ( -2.293366432827344421E-15, -12.48450537969573659, -112.9062500020483952 ) ) ;
#19650 = EDGE_CURVE ( 'NONE', #34451, #39187, #1383, .T. ) ;
#19651 = ORIENTED_EDGE ( 'NONE', *, *, #3826, .F. ) ;
#19652 = CARTESIAN_POINT ( 'NONE',  ( -2.121150477449813534E-15, -11.54700538379251284, -128.3750000000000000 ) ) ;
#19653 = CARTESIAN_POINT ( 'NONE',  ( 9.999999999999998224, 0.000000000000000000, -107.3750000040967763 ) ) ;
#19654 = CARTESIAN_POINT ( 'NONE',  ( 10.00000000000051159, -5.773502691895965988, -146.1250000000000284 ) ) ;
#19655 = CARTESIAN_POINT ( 'NONE',  ( -10.81189881249999907, -6.242252689847864744, -63.46875000204838102 ) ) ;
#19656 = EDGE_LOOP ( 'NONE', ( #9169, #19200, #12382, #16524 ) ) ;
#19657 = CARTESIAN_POINT ( 'NONE',  ( 9.999999999999998224, 0.000000000000000000, -39.49999999999997868 ) ) ;
#19658 = CARTESIAN_POINT ( 'NONE',  ( 7.070501591499377789E-16, 11.54700538379251284, -15.50000000409676915 ) ) ;
#19659 = CARTESIAN_POINT ( 'NONE',  ( 10.81189881249999729, 0.000000000000000000, -43.53125000204838102 ) ) ;
#19660 = CARTESIAN_POINT ( 'NONE',  ( 5.000000000000000000, 8.660254037844385522, -119.1250000040967905 ) ) ;
#19661 = CARTESIAN_POINT ( 'NONE',  ( -2.121150477449813534E-15, -11.54700538379251284, -32.75000000409674783 ) ) ;
#19662 = CARTESIAN_POINT ( 'NONE',  ( 10.00000000000000000, 5.773502691896255534, -166.8750000000000000 ) ) ;
#19663 = CARTESIAN_POINT ( 'NONE',  ( -10.81189881249999729, 1.324075727343319199E-15, -140.2812500020483810 ) ) ;
#19664 = CARTESIAN_POINT ( 'NONE',  ( 5.405949406249999534, 9.363379034771803333, -140.7812500020483810 ) ) ;
#19665 =( BOUNDED_CURVE ( )  B_SPLINE_CURVE ( 2, ( #14640, #40961, #8191, #41613, #34312, #17876, #2361 ),
 .UNSPECIFIED., .F., .F. ) 
 B_SPLINE_CURVE_WITH_KNOTS ( ( 3, 2, 2, 3 ),
 ( 0.8470149253731346084, 0.8482587064676619937, 0.8495024875621892679, 0.8507462686567166532 ),
 .UNSPECIFIED. ) 
 CURVE ( )  GEOMETRIC_REPRESENTATION_ITEM ( )  RATIONAL_B_SPLINE_CURVE ( ( 0.9999999999999641398, 0.8660254037844745678, 1.000000000000000000, 0.8660254037844387076, 1.000000000000000000, 0.8660254037844148378, 1.000000000000023981 ) ) 
 REPRESENTATION_ITEM ( '' )  );
#19666 = VERTEX_POINT ( 'NONE', #17971 ) ;
#19667 = VECTOR ( 'NONE', #12059, 1000.000000000000000 ) ;
#19668 = ORIENTED_EDGE ( 'NONE', *, *, #29337, .F. ) ;
#19669 = ORIENTED_EDGE ( 'NONE', *, *, #25456, .T. ) ;
#19670 = CARTESIAN_POINT ( 'NONE',  ( 0.000000000000000000, 0.000000000000000000, -200.0000000000000000 ) ) ;
#19671 = CARTESIAN_POINT ( 'NONE',  ( 10.81189881249999907, 6.242252689847868297, -175.2187500020484094 ) ) ;
#19672 = CARTESIAN_POINT ( 'NONE',  ( 7.644554776091147741E-16, 12.48450537969573659, -23.46875000204836326 ) ) ;
#19673 = CARTESIAN_POINT ( 'NONE',  ( -9.999999999999998224, 1.224646799147353059E-15, -46.62500000409677625 ) ) ;
#19674 = CARTESIAN_POINT ( 'NONE',  ( -5.405949406249996869, 9.363379034771805109, -153.8437500020483810 ) ) ;
#19675 = CARTESIAN_POINT ( 'NONE',  ( -10.81189881249999907, -6.242252689847864744, -147.4687500020484094 ) ) ;
#19676 = CARTESIAN_POINT ( 'NONE',  ( 9.999999999999998224, 0.000000000000000000, -67.99999999999997158 ) ) ;
#19677 = CARTESIAN_POINT ( 'NONE',  ( 5.405949406249999534, 9.363379034771803333, -128.5937500020483810 ) ) ;
#19678 = AXIS2_PLACEMENT_3D ( 'NONE', #19256, #41495, #5473 ) ;
#19679 = CARTESIAN_POINT ( 'NONE',  ( 7.644554776091147741E-16, 12.48450537969573659, -130.1562500020483810 ) ) ;
#19680 = CARTESIAN_POINT ( 'NONE',  ( -10.81189881249999729, 6.242252689847871849, -20.21875000204836326 ) ) ;
#19681 = CARTESIAN_POINT ( 'NONE',  ( 7.644554776091147741E-16, 12.48450537969573659, -134.4687500020483810 ) ) ;
#19682 = CARTESIAN_POINT ( 'NONE',  ( -9.999999999999998224, 1.224646799147353059E-15, -126.1250000040967620 ) ) ;
#19683 = VECTOR ( 'NONE', #7898, 1000.000000000000000 ) ;
#19684 = FACE_OUTER_BOUND ( 'NONE', #13588, .T. ) ;
#19685 = CARTESIAN_POINT ( 'NONE',  ( -4.999999999999996447, 8.660254037844387298, -165.0000000000000000 ) ) ;
#19686 = CARTESIAN_POINT ( 'NONE',  ( -2.293366432827344421E-15, -12.48450537969573659, -0.4062500020483583718 ) ) ;
#19687 = EDGE_CURVE ( 'NONE', #17374, #34823, #42533, .T. ) ;
#19688 = CARTESIAN_POINT ( 'NONE',  ( 5.405949406249999534, 9.363379034771803333, -74.59375000204838102 ) ) ;
#19689 = CARTESIAN_POINT ( 'NONE',  ( -10.81189881249999907, -6.242252689847864744, -39.65625000204835970 ) ) ;
#19690 = CARTESIAN_POINT ( 'NONE',  ( -5.405949406249996869, 9.363379034771805109, -54.84375000204835970 ) ) ;
#19691 = CARTESIAN_POINT ( 'NONE',  ( 9.999999999999998224, 0.000000000000000000, -194.3750000040967905 ) ) ;
#19692 = CARTESIAN_POINT ( 'NONE',  ( 10.81189881249999551, -6.242252689847874514, -164.9687500020484094 ) ) ;
#19693 = CARTESIAN_POINT ( 'NONE',  ( 9.999999999999998224, 0.000000000000000000, -138.5000000000000000 ) ) ;
#19694 = VECTOR ( 'NONE', #4810, 1000.000000000000000 ) ;
#19695 = CARTESIAN_POINT ( 'NONE',  ( -2.293366432827344421E-15, -12.48450537969573659, -138.4062500020484094 ) ) ;
#19696 = FACE_OUTER_BOUND ( 'NONE', #22106, .T. ) ;
#19697 = CARTESIAN_POINT ( 'NONE',  ( -9.999999999999998224, 1.224646799147353059E-15, -117.1250000040967905 ) ) ;
#19698 = CARTESIAN_POINT ( 'NONE',  ( 9.999999999999996447, -5.773502691896262640, -87.62499999999998579 ) ) ;
#19699 = ORIENTED_EDGE ( 'NONE', *, *, #33101, .T. ) ;
#19700 = CARTESIAN_POINT ( 'NONE',  ( -2.293366432827344421E-15, -12.48450537969573659, -118.9062500020483952 ) ) ;
#19701 = CARTESIAN_POINT ( 'NONE',  ( 10.00000000000000000, 5.773502691896255534, -134.2500000040967905 ) ) ;
#19702 = CARTESIAN_POINT ( 'NONE',  ( 0.000000000000000000, 0.000000000000000000, -200.0000000000000000 ) ) ;
#19703 = CARTESIAN_POINT ( 'NONE',  ( 7.644554776091147741E-16, 12.48450537969573659, -170.6562500020484094 ) ) ;
#19704 = CARTESIAN_POINT ( 'NONE',  ( -10.00000000000000000, -5.773502691896251982, -42.00000000409674783 ) ) ;
#19705 = CARTESIAN_POINT ( 'NONE',  ( 4.999999999999992006, -8.660254037844389075, -159.7500000000000000 ) ) ;
#19706 = CARTESIAN_POINT ( 'NONE',  ( 10.81189881249999729, 0.000000000000000000, -57.03125000204836681 ) ) ;
#19707 = EDGE_CURVE ( 'NONE', #27322, #29348, #9338, .T. ) ;
#19708 =( BOUNDED_CURVE ( )  B_SPLINE_CURVE ( 2, ( #38709, #34417, #17981, #76, #35484, #6336, #22733 ),
 .UNSPECIFIED., .F., .F. ) 
 B_SPLINE_CURVE_WITH_KNOTS ( ( 3, 2, 2, 3 ),
 ( 0.9067164179104481025, 0.9079601990049754878, 0.9092039800995028731, 0.9104477611940301474 ),
 .UNSPECIFIED. ) 
 CURVE ( )  GEOMETRIC_REPRESENTATION_ITEM ( )  RATIONAL_B_SPLINE_CURVE ( ( 0.9999999999999641398, 0.8660254037844745678, 1.000000000000000000, 0.8660254037844387076, 1.000000000000000000, 0.8660254037844028474, 1.000000000000035971 ) ) 
 REPRESENTATION_ITEM ( '' )  );
#19709 = CARTESIAN_POINT ( 'NONE',  ( -4.999999999999996447, 8.660254037844387298, -73.49999999999998579 ) ) ;
#19710 = CARTESIAN_POINT ( 'NONE',  ( -2.293366432827344421E-15, -12.48450537969573659, -157.9062500020483810 ) ) ;
#19711 = CARTESIAN_POINT ( 'NONE',  ( -10.81189881249999729, 6.242252689847871849, -140.2187500020483810 ) ) ;
#19712 = CARTESIAN_POINT ( 'NONE',  ( 9.999999999999998224, 0.000000000000000000, -100.9999999999999858 ) ) ;
#19713 = CARTESIAN_POINT ( 'NONE',  ( 45.00000000000000711, 5.510910596163090344E-15, -217.0000000000000853 ) ) ;
#19714 = VERTEX_POINT ( 'NONE', #35472 ) ;
#19715 = CARTESIAN_POINT ( 'NONE',  ( -1.040834085586084257E-14, -145.0000000000000000, 22.49999999999999289 ) ) ;
#19716 = AXIS2_PLACEMENT_3D ( 'NONE', #8770, #4892, #5106 ) ;
#19718 = ORIENTED_EDGE ( 'NONE', *, *, #21677, .T. ) ;
#19717 = CARTESIAN_POINT ( 'NONE',  ( 7.644554776091147741E-16, 12.48450537969573659, -70.15625000204839523 ) ) ;
#19719 = APPROVAL_ROLE ( '' ) ;
#19721 = ORIENTED_EDGE ( 'NONE', *, *, #19707, .T. ) ;
#19720 = CARTESIAN_POINT ( 'NONE',  ( 5.405949406249999534, 9.363379034771803333, -122.5937500020483952 ) ) ;
#19722 = ORIENTED_EDGE ( 'NONE', *, *, #22707, .T. ) ;
#19723 = CARTESIAN_POINT ( 'NONE',  ( -10.81189881249999729, -6.242252689847864744, -22.96875000204837747 ) ) ;
#19724 = CARTESIAN_POINT ( 'NONE',  ( -5.405949406250003975, -9.363379034771801557, -198.3437500020484094 ) ) ;
#19725 = CARTESIAN_POINT ( 'NONE',  ( 7.644554776091147741E-16, 12.48450537969573659, -50.46875000204835970 ) ) ;
#19726 = CARTESIAN_POINT ( 'NONE',  ( -9.999999999999998224, 1.224646799147353059E-15, -200.0000000000000000 ) ) ;
#19727 = CARTESIAN_POINT ( 'NONE',  ( -9.999999999999998224, 5.773502691896259087, -31.37499999999995737 ) ) ;
#19728 = CARTESIAN_POINT ( 'NONE',  ( -10.81189881249999729, 6.242252689847871849, -182.2187500020484379 ) ) ;
#19729 = CARTESIAN_POINT ( 'NONE',  ( -10.81189881249999907, -6.242252689847864744, -166.9687500020484094 ) ) ;
#19730 = CARTESIAN_POINT ( 'NONE',  ( -5.405949406250003975, -9.363379034771801557, -150.3437500020483810 ) ) ;
#19732 = ADVANCED_FACE ( 'NONE', ( #6109 ), #22085, .T. ) ;
#19731 = CARTESIAN_POINT ( 'NONE',  ( -2.293366432827344421E-15, -12.48450537969573659, -162.2187500020483810 ) ) ;
#19733 = CARTESIAN_POINT ( 'NONE',  ( 9.999999999999227285, 5.773502691896701400, -107.2500000040967620 ) ) ;
#19734 = CARTESIAN_POINT ( 'NONE',  ( -4.999999999999996447, 8.660254037844387298, -193.5000000000000000 ) ) ;
#19735 = CARTESIAN_POINT ( 'NONE',  ( 10.00000000000000000, 5.773502691896255534, -189.3750000000000000 ) ) ;
#19736 = CARTESIAN_POINT ( 'NONE',  ( -10.81189881249999729, 1.324075727343319199E-15, -93.59375000204838102 ) ) ;
#19737 = CARTESIAN_POINT ( 'NONE',  ( 9.999999999999998224, 0.000000000000000000, -198.8750000040967905 ) ) ;
#19738 = CARTESIAN_POINT ( 'NONE',  ( 5.405949406249999534, 9.363379034771803333, -68.78125000204838102 ) ) ;
#19739 = CARTESIAN_POINT ( 'NONE',  ( -2.121150477449813534E-15, -11.54700538379251284, -159.8750000000000000 ) ) ;
#19740 = CARTESIAN_POINT ( 'NONE',  ( 5.405949406249992428, -9.363379034771808662, -189.0937500020483810 ) ) ;
#19741 = CARTESIAN_POINT ( 'NONE',  ( -2.293366432827344421E-15, -12.48450537969573659, -160.9062500020483810 ) ) ;
#19742 = CARTESIAN_POINT ( 'NONE',  ( 10.81189881249999551, -6.242252689847874514, -63.15625000204838813 ) ) ;
#19743 = CARTESIAN_POINT ( 'NONE',  ( -4.999999999999996447, 8.660254037844387298, -139.8750000040968189 ) ) ;
#19744 = CARTESIAN_POINT ( 'NONE',  ( -2.121150477449813534E-15, -11.54700538379251284, -117.8749999999999858 ) ) ;
#19745 = ORIENTED_EDGE ( 'NONE', *, *, #34029, .F. ) ;
#19746 = CARTESIAN_POINT ( 'NONE',  ( -10.81189881249999729, -6.242252689847864744, -146.1562500020484094 ) ) ;
#19747 = CC_DESIGN_APPROVAL ( #32804, ( #27695 ) ) ;
#19748 = CARTESIAN_POINT ( 'NONE',  ( 7.644554776091147741E-16, 12.48450537969573659, -152.6562500020484094 ) ) ;
#19749 = CARTESIAN_POINT ( 'NONE',  ( 10.81189881249999551, -6.242252689847874514, -198.1562500020484379 ) ) ;
#19750 = CARTESIAN_POINT ( 'NONE',  ( 10.81189881249999551, -6.242252689847874514, -92.96875000204838102 ) ) ;
#19751 = ORIENTED_EDGE ( 'NONE', *, *, #10961, .F. ) ;
#19752 = CARTESIAN_POINT ( 'NONE',  ( -9.999999999999998224, 5.773502691896259087, -58.37499999999999289 ) ) ;
#19753 = CARTESIAN_POINT ( 'NONE',  ( 10.81189881249999551, -6.242252689847874514, -188.9687500020484094 ) ) ;
#19754 = CARTESIAN_POINT ( 'NONE',  ( -5.000000000000003553, -8.660254037844383745, -64.37500000409676204 ) ) ;
#19755 = EDGE_CURVE ( 'NONE', #9902, #39730, #32024, .T. ) ;
#19756 = CARTESIAN_POINT ( 'NONE',  ( 0.000000000000000000, 0.000000000000000000, -200.0000000000000000 ) ) ;
#19757 = CARTESIAN_POINT ( 'NONE',  ( 7.644554776091147741E-16, 12.48450537969573659, -86.65625000204838102 ) ) ;
#19758 = CARTESIAN_POINT ( 'NONE',  ( -10.81189881249999729, 6.242252689847871849, -59.40625000204838813 ) ) ;
#19759 = CARTESIAN_POINT ( 'NONE',  ( -10.00000000000000000, -5.773502691896251982, -58.50000000409676915 ) ) ;
#19760 = CARTESIAN_POINT ( 'NONE',  ( 7.644554776091147741E-16, 12.48450537969573659, -15.96875000204836503 ) ) ;
#19761 = DIRECTION ( 'NONE',  ( -0.000000000000000000, -0.000000000000000000, 1.000000000000000000 ) ) ;
#19762 = CARTESIAN_POINT ( 'NONE',  ( 10.81189881249999729, 0.000000000000000000, -187.5312500020484094 ) ) ;
#19763 = CARTESIAN_POINT ( 'NONE',  ( 10.81189881249999907, 6.242252689847868297, -14.90625000204837036 ) ) ;
#19764 = CARTESIAN_POINT ( 'NONE',  ( 9.999999999999998224, 0.000000000000000000, -79.99999999999998579 ) ) ;
#19765 = CARTESIAN_POINT ( 'NONE',  ( -4.999999999999996447, 8.660254037844387298, -165.0000000000000000 ) ) ;
#19766 = CARTESIAN_POINT ( 'NONE',  ( 10.00000000000051159, -5.773502691895965988, -45.62499999999994316 ) ) ;
#19767 = CARTESIAN_POINT ( 'NONE',  ( -5.000020801129981152, 8.660290040615111096, 0.000000000000000000 ) ) ;
#19768 = CARTESIAN_POINT ( 'NONE',  ( -2.121150477449813534E-15, -11.54700538379251284, -165.8750000000000000 ) ) ;
#19769 = CARTESIAN_POINT ( 'NONE',  ( -9.999999999998969713, -5.773502691896847949, -62.62499999999996447 ) ) ;
#19771 = EDGE_LOOP ( 'NONE', ( #1407, #562, #32066, #14063 ) ) ;
#19770 = CARTESIAN_POINT ( 'NONE',  ( -10.81189881249999729, 1.324075727343319199E-15, -96.78125000204839523 ) ) ;
#19772 = FACE_OUTER_BOUND ( 'NONE', #19409, .T. ) ;
#19774 = ORIENTED_EDGE ( 'NONE', *, *, #34237, .T. ) ;
#19773 = CARTESIAN_POINT ( 'NONE',  ( -10.81189881249999729, -6.242252689847864744, -100.9687500020483668 ) ) ;
#19775 = ORIENTED_EDGE ( 'NONE', *, *, #15202, .F. ) ;
#19776 = CARTESIAN_POINT ( 'NONE',  ( -5.405949406250003975, -9.363379034771801557, -31.84375000204836681 ) ) ;
#19777 = CARTESIAN_POINT ( 'NONE',  ( -10.81189881249999729, 6.242252689847871849, -24.90625000204838813 ) ) ;
#19778 = PERSON_AND_ORGANIZATION_ROLE ( 'classification_officer' ) ;
#19779 = CARTESIAN_POINT ( 'NONE',  ( 5.405949406249992428, -9.363379034771808662, -75.09375000204838102 ) ) ;
#19780 = DIRECTION ( 'NONE',  ( -0.000000000000000000, -0.000000000000000000, -1.000000000000000000 ) ) ;
#19781 = CARTESIAN_POINT ( 'NONE',  ( 7.644554776091147741E-16, 12.48450537969573659, -189.9687500020484094 ) ) ;
#19782 = CARTESIAN_POINT ( 'NONE',  ( -9.999999999999998224, 1.224646799147353059E-15, -132.1250000040967620 ) ) ;
#19783 = DIRECTION ( 'NONE',  ( -0.000000000000000000, -0.000000000000000000, 1.000000000000000000 ) ) ;
#19784 = CARTESIAN_POINT ( 'NONE',  ( -5.405949406249996869, 9.363379034771805109, -157.0312500020484094 ) ) ;
#19785 = CARTESIAN_POINT ( 'NONE',  ( -9.999999999999998224, 1.224646799147353059E-15, -1.625000004096766038 ) ) ;
#19786 = DIRECTION ( 'NONE',  ( -0.000000000000000000, -0.000000000000000000, 1.000000000000000000 ) ) ;
#19787 = CARTESIAN_POINT ( 'NONE',  ( -5.405949406250003975, -9.363379034771801557, -123.3437500020483952 ) ) ;
#19788 = CARTESIAN_POINT ( 'NONE',  ( 10.81189881249999729, 0.000000000000000000, -99.03125000204839523 ) ) ;
#19789 = CARTESIAN_POINT ( 'NONE',  ( 10.81189881249999729, 0.000000000000000000, -107.8437500020483810 ) ) ;
#19790 = CARTESIAN_POINT ( 'NONE',  ( -10.81189881249999729, 1.324075727343319199E-15, -77.09375000204838102 ) ) ;
#19791 = CARTESIAN_POINT ( 'NONE',  ( 10.81189881249999907, 6.242252689847868297, -86.90625000204836681 ) ) ;
#19792 = CARTESIAN_POINT ( 'NONE',  ( -4.999999999999996447, 8.660254037844387298, -163.8750000040967905 ) ) ;
#19793 = CYLINDRICAL_SURFACE ( 'NONE', #36486, 9.999999999999998224 ) ;
#19794 = CARTESIAN_POINT ( 'NONE',  ( 10.81189881249999729, 0.000000000000000000, -169.5312500020484094 ) ) ;
#19795 = CARTESIAN_POINT ( 'NONE',  ( -2.293366432827344421E-15, -12.48450537969573659, -180.4062500020484379 ) ) ;
#19796 = CARTESIAN_POINT ( 'NONE',  ( -5.000000000000003553, -8.660254037844383745, -158.8750000040967905 ) ) ;
#19797 = DIRECTION ( 'NONE',  ( -1.000000000000000000, 0.000000000000000000, 0.000000000000000000 ) ) ;
#19798 = CARTESIAN_POINT ( 'NONE',  ( 5.405949406249999534, 9.363379034771803333, -8.593750002048345493 ) ) ;
#19799 = CARTESIAN_POINT ( 'NONE',  ( 9.999999999999998224, 0.000000000000000000, -149.0000000000000000 ) ) ;
#19800 = CARTESIAN_POINT ( 'NONE',  ( 5.405949406249999534, 9.363379034771803333, -118.0937500020483810 ) ) ;
#19801 = CARTESIAN_POINT ( 'NONE',  ( 7.070501591499377789E-16, 11.54700538379251284, -81.12499999999997158 ) ) ;
#19802 = CARTESIAN_POINT ( 'NONE',  ( -5.405949406249996869, 9.363379034771805109, -10.03125000204835260 ) ) ;
#19803 = CARTESIAN_POINT ( 'NONE',  ( -10.00000000000000000, -5.773502691896251982, -87.00000000409677625 ) ) ;
#19804 = DIRECTION ( 'NONE',  ( -0.000000000000000000, -0.000000000000000000, 1.000000000000000000 ) ) ;
#19805 = CARTESIAN_POINT ( 'NONE',  ( -10.81189881249999729, 1.324075727343319199E-15, -105.7812500020483810 ) ) ;
#19806 = CARTESIAN_POINT ( 'NONE',  ( -5.405949406249996869, 9.363379034771805109, -94.03125000204838102 ) ) ;
#19807 = ORIENTED_EDGE ( 'NONE', *, *, #4732, .F. ) ;
#19808 = CARTESIAN_POINT ( 'NONE',  ( 9.999999999999998224, 0.000000000000000000, -87.87500000409677625 ) ) ;
#19809 = CARTESIAN_POINT ( 'NONE',  ( -4.999999999999996447, 8.660254037844387298, -145.8750000040967905 ) ) ;
#19810 = CARTESIAN_POINT ( 'NONE',  ( -10.81189881249999907, -6.242252689847864744, -43.96875000204835970 ) ) ;
#19811 = ORIENTED_EDGE ( 'NONE', *, *, #32446, .T. ) ;
#19812 = CARTESIAN_POINT ( 'NONE',  ( 4.999999999999992006, -8.660254037844389075, -11.24999999999995381 ) ) ;
#19813 = EDGE_CURVE ( 'NONE', #2320, #33286, #5225, .T. ) ;
#19814 = CARTESIAN_POINT ( 'NONE',  ( -2.121150477449813534E-15, -11.54700538379251284, -149.3750000000000000 ) ) ;
#19815 = CARTESIAN_POINT ( 'NONE',  ( -9.999999999999998224, 1.224646799147353059E-15, -9.125000004096744277 ) ) ;
#19816 = EDGE_CURVE ( 'NONE', #36111, #18400, #23178, .T. ) ;
#19817 = CARTESIAN_POINT ( 'NONE',  ( 9.999999999999998224, 0.000000000000000000, -189.5000000000000000 ) ) ;
#19819 = VERTEX_POINT ( 'NONE', #42338 ) ;
#19818 = CARTESIAN_POINT ( 'NONE',  ( -10.81189881249999729, 6.242252689847871849, -116.4062500020483810 ) ) ;
#19820 = CIRCLE ( 'NONE', #10848, 5.000000000000002665 ) ;
#19821 = CARTESIAN_POINT ( 'NONE',  ( -9.999999999999998224, 1.224646799147353059E-15, -200.0000000000000000 ) ) ;
#19822 = VECTOR ( 'NONE', #41971, 1000.000000000000000 ) ;
#19823 = ORIENTED_EDGE ( 'NONE', *, *, #29925, .T. ) ;
#19824 =( BOUNDED_CURVE ( )  B_SPLINE_CURVE ( 2, ( #16735, #13072, #32955, #10478, #16522, #32742, #3180 ),
 .UNSPECIFIED., .F., .F. ) 
 B_SPLINE_CURVE_WITH_KNOTS ( ( 3, 2, 2, 3 ),
 ( 0.1828358208955224162, 0.1840796019900497738, 0.1853233830845771313, 0.1865671641791045166 ),
 .UNSPECIFIED. ) 
 CURVE ( )  GEOMETRIC_REPRESENTATION_ITEM ( )  RATIONAL_B_SPLINE_CURVE ( ( 0.9999999999999970024, 0.8660254037844417052, 1.000000000000000000, 0.8660254037844387076, 1.000000000000000000, 0.8660254037844357100, 1.000000000000002887 ) ) 
 REPRESENTATION_ITEM ( '' )  );
#19825 = CARTESIAN_POINT ( 'NONE',  ( -2.293366432827344421E-15, -12.48450537969573659, -43.90625000204838102 ) ) ;
#19826 = PERSON_AND_ORGANIZATION ( #11915, #17965 ) ;
#19827 = CARTESIAN_POINT ( 'NONE',  ( 5.405949406249999534, 9.363379034771803333, -94.09375000204838102 ) ) ;
#19828 = CARTESIAN_POINT ( 'NONE',  ( 7.644554776091147741E-16, 12.48450537969573659, -124.1562500020483810 ) ) ;
#19829 = ORIENTED_EDGE ( 'NONE', *, *, #28465, .T. ) ;
#19830 = CARTESIAN_POINT ( 'NONE',  ( 10.81189881249999729, 0.000000000000000000, -199.5312500020484094 ) ) ;
#19831 = DIRECTION ( 'NONE',  ( 0.08715574274765837404, 0.000000000000000000, -0.9961946980917455452 ) ) ;
#19832 =( BOUNDED_CURVE ( )  B_SPLINE_CURVE ( 2, ( #33480, #6922, #20075, #33269, #3695, #3906, #29595 ),
 .UNSPECIFIED., .F., .F. ) 
 B_SPLINE_CURVE_WITH_KNOTS ( ( 3, 2, 2, 3 ),
 ( 0.3395522388059703522, 0.3407960199004976820, 0.3420398009950250118, 0.3432835820895522860 ),
 .UNSPECIFIED. ) 
 CURVE ( )  GEOMETRIC_REPRESENTATION_ITEM ( )  RATIONAL_B_SPLINE_CURVE ( ( 0.9999999999999761302, 0.8660254037844625774, 1.000000000000000000, 0.8660254037844387076, 1.000000000000000000, 0.8660254037844327124, 1.000000000000005995 ) ) 
 REPRESENTATION_ITEM ( '' )  );
#19833 = CARTESIAN_POINT ( 'NONE',  ( -10.81189881249999729, 1.324075727343319199E-15, -180.7812500020484094 ) ) ;
#19834 = CARTESIAN_POINT ( 'NONE',  ( -1.040834085586084257E-14, 145.0000000000000000, 22.49999999999999289 ) ) ;
#19835 = CARTESIAN_POINT ( 'NONE',  ( -5.405949406250003975, -9.363379034771801557, -133.8437500020484094 ) ) ;
#19836 = CARTESIAN_POINT ( 'NONE',  ( 10.81189881249999729, 0.000000000000000000, -98.84375000204838102 ) ) ;
#19837 = DIRECTION ( 'NONE',  ( 1.000000000000000000, 0.000000000000000000, 0.000000000000000000 ) ) ;
#19838 = CARTESIAN_POINT ( 'NONE',  ( 5.405949406249992428, -9.363379034771808662, -108.2812500020483810 ) ) ;
#19839 = CARTESIAN_POINT ( 'NONE',  ( -5.000000000000003553, -8.660254037844383745, -185.8750000040967905 ) ) ;
#19840 = CARTESIAN_POINT ( 'NONE',  ( 10.81189881249999729, 6.242252689847867408, -112.2187500020483810 ) ) ;
#19841 = CARTESIAN_POINT ( 'NONE',  ( 10.81189881249999729, 6.242252689847867408, -190.4062500020483810 ) ) ;
#19842 =( BOUNDED_CURVE ( )  B_SPLINE_CURVE ( 2, ( #2366, #29114, #15493, #28698, #41825, #38603, #9042 ),
 .UNSPECIFIED., .F., .F. ) 
 B_SPLINE_CURVE_WITH_KNOTS ( ( 3, 2, 2, 3 ),
 ( 0.5597014925373136052, 0.5609452736318409904, 0.5621890547263683757, 0.5634328358208957610 ),
 .UNSPECIFIED. ) 
 CURVE ( )  GEOMETRIC_REPRESENTATION_ITEM ( )  RATIONAL_B_SPLINE_CURVE ( ( 0.9999999999999761302, 0.8660254037844625774, 1.000000000000000000, 0.8660254037844387076, 1.000000000000000000, 0.8660254037844148378, 1.000000000000023981 ) ) 
 REPRESENTATION_ITEM ( '' )  );
#19843 = DIRECTION ( 'NONE',  ( 1.000000000000000000, 0.000000000000000000, 0.000000000000000000 ) ) ;
#19844 = LINE ( 'NONE', #38488, #41025 ) ;
#19845 = CARTESIAN_POINT ( 'NONE',  ( -9.999999999999998224, 5.773502691896259087, -133.3750000000000000 ) ) ;
#19846 = CARTESIAN_POINT ( 'NONE',  ( 4.999999999999992006, -8.660254037844389075, -6.749999999999978684 ) ) ;
#19847 = CARTESIAN_POINT ( 'NONE',  ( 10.81189881249999729, 6.242252689847867408, -56.71875000204838813 ) ) ;
#19848 = CARTESIAN_POINT ( 'NONE',  ( 10.81189881249999551, -6.242252689847874514, -52.46875000204837391 ) ) ;
#19849 = CARTESIAN_POINT ( 'NONE',  ( 5.000000000000000000, 8.660254037844385522, -177.6250000040968189 ) ) ;
#19850 = CARTESIAN_POINT ( 'NONE',  ( -5.405949406249996869, 9.363379034771805109, -14.53125000204835615 ) ) ;
#19851 = VECTOR ( 'NONE', #21063, 1000.000000000000000 ) ;
#19852 = CARTESIAN_POINT ( 'NONE',  ( 10.81189881249999907, 6.242252689847868297, -32.71875000204835260 ) ) ;
#19853 = CARTESIAN_POINT ( 'NONE',  ( -9.999999999999998224, 1.224646799147353059E-15, -27.12500000409676204 ) ) ;
#19854 = CARTESIAN_POINT ( 'NONE',  ( 5.405949406249992428, -9.363379034771808662, -135.0937500020483810 ) ) ;
#19855 = CARTESIAN_POINT ( 'NONE',  ( 4.999999999999992006, -8.660254037844389075, -108.7499999999999858 ) ) ;
#19856 = CARTESIAN_POINT ( 'NONE',  ( -10.81189881249999729, 1.324075727343319199E-15, -35.28125000204837391 ) ) ;
#19857 = AXIS2_PLACEMENT_3D ( 'NONE', #20371, #30962, #7648 ) ;
#19858 = CARTESIAN_POINT ( 'NONE',  ( -2.121150477449813534E-15, -11.54700538379251284, -27.87499999999999289 ) ) ;
#19859 = CARTESIAN_POINT ( 'NONE',  ( -5.000000000000003553, -8.660254037844383745, -63.99999999999997158 ) ) ;
#19860 = CARTESIAN_POINT ( 'NONE',  ( -2.293366432827344421E-15, -12.48450537969573659, -130.9062500020483810 ) ) ;
#19861 = CARTESIAN_POINT ( 'NONE',  ( 10.81189881249999729, 6.242252689847867408, -115.4062500020484094 ) ) ;
#19862 = ORIENTED_EDGE ( 'NONE', *, *, #38049, .F. ) ;
#19863 = CARTESIAN_POINT ( 'NONE',  ( 10.00000000000051159, -5.773502691895965988, -128.1250000000000000 ) ) ;
#19864 = CARTESIAN_POINT ( 'NONE',  ( -10.00000000000000000, -5.773502691896251982, -109.5000000040967905 ) ) ;
#19865 = CARTESIAN_POINT ( 'NONE',  ( 9.999999999999998224, 0.000000000000000000, -162.5000000000000000 ) ) ;
#19866 = CARTESIAN_POINT ( 'NONE',  ( -2.293366432827344421E-15, -12.48450537969573659, -64.71875000204838102 ) ) ;
#19867 = ORIENTED_EDGE ( 'NONE', *, *, #11329, .F. ) ;
#19868 = CARTESIAN_POINT ( 'NONE',  ( -9.999999999999998224, 5.773502691896259087, -34.37499999999997158 ) ) ;
#19869 = CARTESIAN_POINT ( 'NONE',  ( -2.121150477449813534E-15, -11.54700538379251284, -19.25000000409676915 ) ) ;
#19870 = ADVANCED_FACE ( 'NONE', ( #15159 ), #35046, .T. ) ;
#19871 = CARTESIAN_POINT ( 'NONE',  ( 5.405949406249992428, -9.363379034771808662, -46.78125000204838813 ) ) ;
#19872 = CARTESIAN_POINT ( 'NONE',  ( -9.999999999998969713, -5.773502691896847949, -2.624999999999922728 ) ) ;
#19873 = CARTESIAN_POINT ( 'NONE',  ( 10.00000000000000000, 5.773502691896255534, -35.25000000409675494 ) ) ;
#19874 = EDGE_CURVE ( 'NONE', #5096, #25139, #9130, .T. ) ;
#19875 = FACE_OUTER_BOUND ( 'NONE', #12628, .T. ) ;
#19876 = CARTESIAN_POINT ( 'NONE',  ( 10.81189881249999729, 0.000000000000000000, -138.0312500020484094 ) ) ;
#19877 = APPROVAL ( #24637, 'UNSPECIFIED' ) ;
#19878 = CARTESIAN_POINT ( 'NONE',  ( 4.999999999999992006, -8.660254037844389075, -15.74999999999995914 ) ) ;
#19879 = ORIENTED_EDGE ( 'NONE', *, *, #31089, .F. ) ;
#19880 = ORIENTED_EDGE ( 'NONE', *, *, #7750, .F. ) ;
#19881 = EDGE_LOOP ( 'NONE', ( #29327, #3658, #15197, #12389 ) ) ;
#19882 = VECTOR ( 'NONE', #19902, 1000.000000000000000 ) ;
#19883 = CARTESIAN_POINT ( 'NONE',  ( -9.999999999999998224, 1.224646799147353059E-15, -38.74999999999997868 ) ) ;
#19884 = CARTESIAN_POINT ( 'NONE',  ( -5.405949406249996869, 9.363379034771805109, -177.8437500020483810 ) ) ;
#19885 = ADVANCED_FACE ( 'NONE', ( #2873 ), #12561, .T. ) ;
#19886 = CARTESIAN_POINT ( 'NONE',  ( -2.293366432827344421E-15, -12.48450537969573659, -24.21875000204836326 ) ) ;
#19887 = CARTESIAN_POINT ( 'NONE',  ( -9.999999999999227285, -5.773502691896698735, -129.0000000040967620 ) ) ;
#19888 = CARTESIAN_POINT ( 'NONE',  ( -10.81189881249999729, -6.242252689847864744, -157.9687500020484379 ) ) ;
#19889 = CARTESIAN_POINT ( 'NONE',  ( -10.81189881249999729, 6.242252689847871849, -147.7187500020484094 ) ) ;
#19890 = CARTESIAN_POINT ( 'NONE',  ( 10.00000000000154010, -5.773502691895370020, -9.624999999999943157 ) ) ;
#19891 = CARTESIAN_POINT ( 'NONE',  ( -10.81189881249999729, 1.324075727343319199E-15, -123.5937500020483952 ) ) ;
#19892 = CARTESIAN_POINT ( 'NONE',  ( -10.81189881249999907, -6.242252689847864744, -135.6562500020484094 ) ) ;
#19893 = CARTESIAN_POINT ( 'NONE',  ( -10.81189881249999729, 1.324075727343319199E-15, -20.09375000204835615 ) ) ;
#19894 = CARTESIAN_POINT ( 'NONE',  ( 10.81189881249999729, 6.242252689847867408, -137.7187500020483810 ) ) ;
#19895 = CARTESIAN_POINT ( 'NONE',  ( -9.999999999999998224, 1.224646799147353059E-15, -31.62500000409676559 ) ) ;
#19896 = CARTESIAN_POINT ( 'NONE',  ( -4.999999999999996447, 8.660254037844387298, -120.0000000000000000 ) ) ;
#19897 = CARTESIAN_POINT ( 'NONE',  ( 9.999999999999996447, -5.773502691896262640, -167.1250000000000000 ) ) ;
#19898 = CARTESIAN_POINT ( 'NONE',  ( 5.000000000000000000, 8.660254037844385522, -99.62500000409679046 ) ) ;
#19899 = CARTESIAN_POINT ( 'NONE',  ( 7.644554776091147741E-16, 12.48450537969573659, -75.96875000204838102 ) ) ;
#19900 = CARTESIAN_POINT ( 'NONE',  ( 7.644554776091147741E-16, 12.48450537969573659, -41.65625000204837391 ) ) ;
#19901 = CARTESIAN_POINT ( 'NONE',  ( -10.81189881249999729, 1.324075727343319199E-15, -53.09375000204835970 ) ) ;
#19902 = DIRECTION ( 'NONE',  ( -0.000000000000000000, -0.000000000000000000, 1.000000000000000000 ) ) ;
#19903 = CARTESIAN_POINT ( 'NONE',  ( -10.81189881249999729, 6.242252689847871849, -162.7187500020483810 ) ) ;
#19904 = CARTESIAN_POINT ( 'NONE',  ( -9.999999999999998224, 5.773502691896259087, -127.3750000000000000 ) ) ;
#19905 = CARTESIAN_POINT ( 'NONE',  ( -10.81189881249999729, -6.242252689847864744, -141.6562500020484094 ) ) ;
#19906 = FACE_OUTER_BOUND ( 'NONE', #35925, .T. ) ;
#19907 = CARTESIAN_POINT ( 'NONE',  ( 7.070501591499377789E-16, 11.54700538379251284, -113.0000000040967905 ) ) ;
#19908 = CARTESIAN_POINT ( 'NONE',  ( -2.121150477449813534E-15, -11.54700538379251284, -92.37500000000000000 ) ) ;
#19909 = EDGE_LOOP ( 'NONE', ( #12622, #11788, #31161, #20620 ) ) ;
#19910 = CARTESIAN_POINT ( 'NONE',  ( 5.405949406249999534, 9.363379034771803333, -112.2812500020483952 ) ) ;
#19911 = CARTESIAN_POINT ( 'NONE',  ( 9.999999999999996447, -5.773502691896262640, -128.5000000040967905 ) ) ;
#19912 = CARTESIAN_POINT ( 'NONE',  ( -10.00000000000051337, 5.773502691895962435, -38.87499999999994316 ) ) ;
#19913 = CARTESIAN_POINT ( 'NONE',  ( -2.293366432827344421E-15, -12.48450537969573659, -168.4062500020483810 ) ) ;
#19914 = CARTESIAN_POINT ( 'NONE',  ( 9.999999999999996447, -5.773502691896262640, -46.00000000409676915 ) ) ;
#19915 =( BOUNDED_CURVE ( )  B_SPLINE_CURVE ( 2, ( #4306, #40324, #10766, #23955, #7542, #20696, #33884 ),
 .UNSPECIFIED., .F., .F. ) 
 B_SPLINE_CURVE_WITH_KNOTS ( ( 3, 2, 2, 3 ),
 ( 0.09701492537313441411, 0.09825870646766173000, 0.09950248756218905977, 0.1007462686567163757 ),
 .UNSPECIFIED. ) 
 CURVE ( )  GEOMETRIC_REPRESENTATION_ITEM ( )  RATIONAL_B_SPLINE_CURVE ( ( 0.9999999999999910072, 0.8660254037844477004, 1.000000000000000000, 0.8660254037844387076, 1.000000000000000000, 0.8660254037844431485, 0.9999999999999955591 ) ) 
 REPRESENTATION_ITEM ( '' )  );
#19916 = CARTESIAN_POINT ( 'NONE',  ( 4.999999999999992006, -8.660254037844389075, -58.12500000409676204 ) ) ;
#19917 = CARTESIAN_POINT ( 'NONE',  ( 10.81189881249999729, 0.000000000000000000, -54.03125000204836681 ) ) ;
#19918 = CARTESIAN_POINT ( 'NONE',  ( -10.00000000000102496, 5.773502691895664007, -44.87499999999994316 ) ) ;
#19919 = CARTESIAN_POINT ( 'NONE',  ( 5.405949406249992428, -9.363379034771808662, -162.2812500020484094 ) ) ;
#19920 = VECTOR ( 'NONE', #41989, 1000.000000000000000 ) ;
#19921 = CARTESIAN_POINT ( 'NONE',  ( -5.405949406249996869, 9.363379034771805109, -131.3437500020484094 ) ) ;
#19922 = CARTESIAN_POINT ( 'NONE',  ( -1.040834085586084257E-14, 20.00000000000000711, 22.49999999999999289 ) ) ;
#19923 = CARTESIAN_POINT ( 'NONE',  ( 9.999999999999998224, 1.224646799147353059E-15, -99.99999999999998579 ) ) ;
#19924 = VERTEX_POINT ( 'NONE', #28358 ) ;
#19925 = CARTESIAN_POINT ( 'NONE',  ( 9.999999999999776179, 5.773502691896386985, -189.7500000040968189 ) ) ;
#19926 = VECTOR ( 'NONE', #2572, 1000.000000000000000 ) ;
#19927 = EDGE_CURVE ( 'NONE', #5147, #6299, #16003, .T. ) ;
#19929 = VERTEX_POINT ( 'NONE', #18844 ) ;
#19928 = CARTESIAN_POINT ( 'NONE',  ( -5.405949406249996869, 9.363379034771805109, -70.03125000204838102 ) ) ;
#19930 = APPROVAL_DATE_TIME ( #26841, #5680 ) ;
#19932 = ORIENTED_EDGE ( 'NONE', *, *, #8126, .F. ) ;
#19931 = CARTESIAN_POINT ( 'NONE',  ( 5.405949406249992428, -9.363379034771808662, -123.0937500020483952 ) ) ;
#19933 = ORIENTED_EDGE ( 'NONE', *, *, #27941, .T. ) ;
#19934 = CARTESIAN_POINT ( 'NONE',  ( -2.293366432827344421E-15, -12.48450537969573659, -19.71875000204837747 ) ) ;
#19935 = CARTESIAN_POINT ( 'NONE',  ( 10.81189881249999729, 0.000000000000000000, -196.3437500020484094 ) ) ;
#19936 = CARTESIAN_POINT ( 'NONE',  ( -10.81189881249999729, 1.324075727343319199E-15, -45.59375000204838102 ) ) ;
#19937 = CARTESIAN_POINT ( 'NONE',  ( 9.999999999999998224, 0.000000000000000000, -134.0000000000000000 ) ) ;
#19938 = CARTESIAN_POINT ( 'NONE',  ( 4.999999999999992006, -8.660254037844389075, -24.74999999999996803 ) ) ;
#19939 = CARTESIAN_POINT ( 'NONE',  ( -5.405949406250003975, -9.363379034771801557, -180.3437500020483810 ) ) ;
#19940 = CARTESIAN_POINT ( 'NONE',  ( -5.405949406250003975, -9.363379034771801557, -172.8437500020484094 ) ) ;
#19941 = CARTESIAN_POINT ( 'NONE',  ( 10.81189881249999729, 0.000000000000000000, -146.8437500020483810 ) ) ;
#19942 = CARTESIAN_POINT ( 'NONE',  ( -10.81189881249999729, 6.242252689847871849, -162.7187500020483810 ) ) ;
#19943 = CARTESIAN_POINT ( 'NONE',  ( 5.000000000000000000, 8.660254037844385522, -107.1250000040967763 ) ) ;
#19944 = CARTESIAN_POINT ( 'NONE',  ( 5.000000000000000000, 8.660254037844385522, -194.1250000040967905 ) ) ;
#19945 = CARTESIAN_POINT ( 'NONE',  ( 5.000000000000000000, 8.660254037844385522, -186.2500000000000000 ) ) ;
#19946 = VECTOR ( 'NONE', #3598, 1000.000000000000000 ) ;
#19947 = CARTESIAN_POINT ( 'NONE',  ( 10.81189881249999907, 6.242252689847868297, -97.21875000204836681 ) ) ;
#19948 = DIRECTION ( 'NONE',  ( -0.000000000000000000, -0.000000000000000000, -1.000000000000000000 ) ) ;
#19949 = CARTESIAN_POINT ( 'NONE',  ( -5.405949406249996869, 9.363379034771805109, -64.03125000204836681 ) ) ;
#19950 = CARTESIAN_POINT ( 'NONE',  ( -4.999999999999996447, 8.660254037844387298, -180.0000000000000000 ) ) ;
#19951 = CARTESIAN_POINT ( 'NONE',  ( 10.81189881249999551, -6.242252689847874514, -187.4687500020484094 ) ) ;
#19952 = CARTESIAN_POINT ( 'NONE',  ( 5.405949406249999534, 9.363379034771803333, -124.2812500020483952 ) ) ;
#19953 = CARTESIAN_POINT ( 'NONE',  ( -10.81189881249999729, -6.242252689847864744, -161.1562500020484094 ) ) ;
#19954 = CARTESIAN_POINT ( 'NONE',  ( 10.81189881249999907, 6.242252689847868297, -55.40625000204837391 ) ) ;
#19955 = CARTESIAN_POINT ( 'NONE',  ( 9.999999999999996447, -5.773502691896262640, -136.0000000040967905 ) ) ;
#19956 = CARTESIAN_POINT ( 'NONE',  ( 7.070501591499377789E-16, 11.54700538379251284, -118.6250000000000142 ) ) ;
#19957 =( BOUNDED_CURVE ( )  B_SPLINE_CURVE ( 2, ( #22090, #41707, #41280, #14947, #35477, #12353, #28577 ),
 .UNSPECIFIED., .F., .F. ) 
 B_SPLINE_CURVE_WITH_KNOTS ( ( 3, 2, 2, 3 ),
 ( 0.2350746268656717097, 0.2363184079601990950, 0.2375621890547264525, 0.2388059701492538378 ),
 .UNSPECIFIED. ) 
 CURVE ( )  GEOMETRIC_REPRESENTATION_ITEM ( )  RATIONAL_B_SPLINE_CURVE ( ( 0.9999999999999940048, 0.8660254037844447028, 1.000000000000000000, 0.8660254037844387076, 1.000000000000000000, 0.8660254037844267172, 1.000000000000011990 ) ) 
 REPRESENTATION_ITEM ( '' )  );
#19958 = ORIENTED_EDGE ( 'NONE', *, *, #38584, .T. ) ;
#19959 = AXIS2_PLACEMENT_3D ( 'NONE', #31185, #23262, #33200 ) ;
#19960 = CARTESIAN_POINT ( 'NONE',  ( -10.81189881249999729, -6.242252689847864744, -131.1562500020483810 ) ) ;
#19961 = CARTESIAN_POINT ( 'NONE',  ( -5.405949406249996869, 9.363379034771805109, -149.5312500020483810 ) ) ;
#19962 = CARTESIAN_POINT ( 'NONE',  ( 10.81189881249999907, 6.242252689847868297, -191.9062500020484094 ) ) ;
#19963 = DIRECTION ( 'NONE',  ( -0.000000000000000000, -0.000000000000000000, 1.000000000000000000 ) ) ;
#19964 = CARTESIAN_POINT ( 'NONE',  ( -2.293366432827344421E-15, -12.48450537969573659, -84.21875000204835260 ) ) ;
#19965 = ORIENTED_EDGE ( 'NONE', *, *, #11078, .T. ) ;
#19966 = CARTESIAN_POINT ( 'NONE',  ( 10.00000000000000000, 5.773502691896255534, -60.37499999999997868 ) ) ;
#19967 = CARTESIAN_POINT ( 'NONE',  ( -10.81189881249999729, 6.242252689847871849, -183.7187500020484379 ) ) ;
#19968 = CARTESIAN_POINT ( 'NONE',  ( -9.999999999999998224, 1.224646799147353059E-15, -66.12500000409676204 ) ) ;
#19969 = CARTESIAN_POINT ( 'NONE',  ( 7.070501591499376803E-16, 11.54700538379251284, -153.1250000000000000 ) ) ;
#19970 = CARTESIAN_POINT ( 'NONE',  ( -5.000000000000003553, -8.660254037844383745, -145.0000000000000000 ) ) ;
#19971 = CARTESIAN_POINT ( 'NONE',  ( 10.81189881249999729, 0.000000000000000000, -81.03125000204839523 ) ) ;
#19972 = CARTESIAN_POINT ( 'NONE',  ( 5.405949406249992428, -9.363379034771808662, -57.28125000204836681 ) ) ;
#19973 = CARTESIAN_POINT ( 'NONE',  ( -10.00000000000000000, -5.773502691896251982, -57.00000000409676915 ) ) ;
#19974 = CARTESIAN_POINT ( 'NONE',  ( -10.81189881249999729, 1.324075727343319199E-15, -18.59375000204835260 ) ) ;
#19975 = CARTESIAN_POINT ( 'NONE',  ( 10.81189881249999907, 6.242252689847868297, -187.4062500020484379 ) ) ;
#19976 = CARTESIAN_POINT ( 'NONE',  ( -2.293366432827344421E-15, -12.48450537969573659, -13.90625000204836859 ) ) ;
#19977 = DIRECTION ( 'NONE',  ( -0.000000000000000000, -0.000000000000000000, -1.000000000000000000 ) ) ;
#19978 = CARTESIAN_POINT ( 'NONE',  ( 9.999999999999548805, 5.773502691896514882, -176.2500000040967905 ) ) ;
#19979 = CARTESIAN_POINT ( 'NONE',  ( -10.00000000000076916, 5.773502691895813221, -114.2500000040967905 ) ) ;
#19980 = CARTESIAN_POINT ( 'NONE',  ( 10.00000000000025402, -5.773502691896113426, -134.5000000040967905 ) ) ;
#19981 = CARTESIAN_POINT ( 'NONE',  ( -9.999999999999998224, 5.773502691896259087, -169.3750000000000000 ) ) ;
#19982 = CONICAL_SURFACE ( 'NONE', #8295, 14.99999999999998579, 0.7853981633974466137 ) ;
#19984 = ORIENTED_EDGE ( 'NONE', *, *, #11850, .T. ) ;
#19983 = CARTESIAN_POINT ( 'NONE',  ( 5.405949406249999534, 9.363379034771803333, -97.28125000204839523 ) ) ;
#19985 = CARTESIAN_POINT ( 'NONE',  ( 7.070501591499376803E-16, 11.54700538379251284, -83.00000000409676204 ) ) ;
#19986 = ORIENTED_EDGE ( 'NONE', *, *, #42543, .T. ) ;
#19987 = ORIENTED_EDGE ( 'NONE', *, *, #25157, .F. ) ;
#19988 = CARTESIAN_POINT ( 'NONE',  ( -10.81189881249999907, -6.242252689847864744, -36.46875000204835970 ) ) ;
#19989 = CARTESIAN_POINT ( 'NONE',  ( -5.405949406249996869, 9.363379034771805109, -19.03125000204835970 ) ) ;
#19990 = COORDINATED_UNIVERSAL_TIME_OFFSET ( 6, 0, .AHEAD. ) ;
#19991 = CARTESIAN_POINT ( 'NONE',  ( 10.81189881249999729, 0.000000000000000000, -70.34375000204836681 ) ) ;
#19992 = CYLINDRICAL_SURFACE ( 'NONE', #28417, 5.000000000000002665 ) ;
#19993 = CARTESIAN_POINT ( 'NONE',  ( -5.405949406250003975, -9.363379034771801557, -189.3437500020483810 ) ) ;
#19994 = CARTESIAN_POINT ( 'NONE',  ( -10.81189881249999729, 6.242252689847871849, -149.2187500020484379 ) ) ;
#19995 = EDGE_CURVE ( 'NONE', #1371, #34292, #39111, .T. ) ;
#19996 = CARTESIAN_POINT ( 'NONE',  ( -4.999999999999996447, 8.660254037844387298, -132.3750000040967905 ) ) ;
#19997 = CARTESIAN_POINT ( 'NONE',  ( 9.999999999999998224, 0.000000000000000000, -56.37500000409676204 ) ) ;
#19998 = CARTESIAN_POINT ( 'NONE',  ( -10.81189881249999729, 1.324075727343319199E-15, -147.7812500020483810 ) ) ;
#19999 = CARTESIAN_POINT ( 'NONE',  ( 4.999999999999992006, -8.660254037844389075, -2.625000004096766926 ) ) ;
#20000 = CARTESIAN_POINT ( 'NONE',  ( 5.321294541346989426, 5.321294541346989426, -220.0000000000000000 ) ) ;
#20001 = CARTESIAN_POINT ( 'NONE',  ( -10.81189881249999729, 1.324075727343319199E-15, -120.5937500020483952 ) ) ;
#20002 = CARTESIAN_POINT ( 'NONE',  ( 5.000000000000000000, 8.660254037844385522, -161.1250000040967905 ) ) ;
#20003 = CARTESIAN_POINT ( 'NONE',  ( -5.405949406249996869, 9.363379034771805109, -86.53125000204838102 ) ) ;
#20004 = CARTESIAN_POINT ( 'NONE',  ( -10.81189881249999729, 1.324075727343319199E-15, -110.0937500020483810 ) ) ;
#20005 = CARTESIAN_POINT ( 'NONE',  ( -5.405949406250003975, -9.363379034771801557, -66.34375000204836681 ) ) ;
#20006 = CARTESIAN_POINT ( 'NONE',  ( -10.81189881249999729, 1.324075727343319199E-15, -78.78125000204838102 ) ) ;
#20007 = CARTESIAN_POINT ( 'NONE',  ( -9.999999999999998224, 1.224646799147353059E-15, -160.6250000040967905 ) ) ;
#20008 = LINE ( 'NONE', #40858, #29614 ) ;
#20009 = CARTESIAN_POINT ( 'NONE',  ( -2.293366432827344421E-15, -12.48450537969573659, -159.4062500020483810 ) ) ;
#20010 = CARTESIAN_POINT ( 'NONE',  ( 5.405949406249992428, -9.363379034771808662, -180.2812500020484094 ) ) ;
#20011 = DIRECTION ( 'NONE',  ( -1.000000000000000000, 0.000000000000000000, 0.000000000000000000 ) ) ;
#20012 = CARTESIAN_POINT ( 'NONE',  ( 10.81189881249999907, 6.242252689847868297, -2.718750002048353043 ) ) ;
#20013 = CARTESIAN_POINT ( 'NONE',  ( 10.00000000000076916, -5.773502691895816774, -108.6249999999999858 ) ) ;
#20014 = CARTESIAN_POINT ( 'NONE',  ( 5.405949406249992428, -9.363379034771808662, -103.5937500020483668 ) ) ;
#20015 = CARTESIAN_POINT ( 'NONE',  ( 9.999999999999996447, -5.773502691896262640, -78.62499999999998579 ) ) ;
#20016 = CARTESIAN_POINT ( 'NONE',  ( -5.405949406250003975, -9.363379034771801557, -9.531250002048352599 ) ) ;
#20017 = CARTESIAN_POINT ( 'NONE',  ( 5.000000000000000000, 8.660254037844385522, -92.12500000409677625 ) ) ;
#20018 = CYLINDRICAL_SURFACE ( 'NONE', #19633, 9.999999999999998224 ) ;
#20019 = CARTESIAN_POINT ( 'NONE',  ( 10.81189881249999551, -6.242252689847874514, -105.1562500020483810 ) ) ;
#20020 = CARTESIAN_POINT ( 'NONE',  ( -5.405949406249996869, 9.363379034771805109, -85.03125000204838102 ) ) ;
#20021 = VERTEX_POINT ( 'NONE', #5694 ) ;
#20022 = EDGE_CURVE ( 'NONE', #21267, #11337, #2254, .T. ) ;
#20023 = CARTESIAN_POINT ( 'NONE',  ( 10.00000000000000000, 5.773502691896255534, -81.75000000409677625 ) ) ;
#20024 = CARTESIAN_POINT ( 'NONE',  ( 9.999999999999479527, 5.773502691896553074, -146.2500000040967905 ) ) ;
#20025 = CARTESIAN_POINT ( 'NONE',  ( -5.405949406249996869, 9.363379034771805109, -42.84375000204837391 ) ) ;
#20026 = EDGE_LOOP ( 'NONE', ( #30935, #34115, #37863, #13043 ) ) ;
#20027 = CARTESIAN_POINT ( 'NONE',  ( 9.999999999999998224, 0.000000000000000000, -10.99999999999995381 ) ) ;
#20028 = ADVANCED_FACE ( 'NONE', ( #2660 ), #31597, .T. ) ;
#20029 = CARTESIAN_POINT ( 'NONE',  ( 7.070501591499377789E-16, 11.54700538379251284, -148.6250000000000000 ) ) ;
#20030 = CARTESIAN_POINT ( 'NONE',  ( -10.00000000000076916, 5.773502691895813221, -139.3750000000000000 ) ) ;
#20031 = CARTESIAN_POINT ( 'NONE',  ( 4.999999999999992006, -8.660254037844389075, -11.62500000409674783 ) ) ;
#20032 = CARTESIAN_POINT ( 'NONE',  ( -9.999999999999998224, 1.224646799147353059E-15, -187.2500000000000000 ) ) ;
#20033 = CARTESIAN_POINT ( 'NONE',  ( -4.999999999999996447, 8.660254037844387298, -95.99999999999998579 ) ) ;
#20035 = VERTEX_POINT ( 'NONE', #28990 ) ;
#20034 = CARTESIAN_POINT ( 'NONE',  ( -10.81189881249999907, -6.242252689847864744, -119.1562500020484237 ) ) ;
#20036 = DIRECTION ( 'NONE',  ( -0.000000000000000000, -0.000000000000000000, 1.000000000000000000 ) ) ;
#20037 = ORIENTED_EDGE ( 'NONE', *, *, #2566, .T. ) ;
#20038 = CARTESIAN_POINT ( 'NONE',  ( -5.405949406250003975, -9.363379034771801557, -48.53125000204838813 ) ) ;
#20039 = COORDINATED_UNIVERSAL_TIME_OFFSET ( 6, 0, .AHEAD. ) ;
#20040 = SECURITY_CLASSIFICATION ( '', '', #3120 ) ;
#20041 = CARTESIAN_POINT ( 'NONE',  ( 10.81189881249999551, -6.242252689847874514, -95.96875000204838102 ) ) ;
#20042 = CARTESIAN_POINT ( 'NONE',  ( 10.81189881249999729, 0.000000000000000000, -126.0312500020483952 ) ) ;
#20043 = VERTEX_POINT ( 'NONE', #25755 ) ;
#20044 = CYLINDRICAL_SURFACE ( 'NONE', #18344, 9.999999999999998224 ) ;
#20045 = CYLINDRICAL_SURFACE ( 'NONE', #39406, 9.999999999999998224 ) ;
#20046 = CARTESIAN_POINT ( 'NONE',  ( -5.405949406249996869, 9.363379034771805109, -173.5312500020484094 ) ) ;
#20047 = FACE_OUTER_BOUND ( 'NONE', #35756, .T. ) ;
#20048 = EDGE_CURVE ( 'NONE', #32999, #25200, #16301, .T. ) ;
#20049 = CARTESIAN_POINT ( 'NONE',  ( -10.81189881249999729, 1.324075727343319199E-15, -129.5937500020483810 ) ) ;
#20050 = CARTESIAN_POINT ( 'NONE',  ( -5.405949406250003975, -9.363379034771801557, -100.8437500020483810 ) ) ;
#20051 = CYLINDRICAL_SURFACE ( 'NONE', #24255, 9.999999999999998224 ) ;
#20052 = CARTESIAN_POINT ( 'NONE',  ( -5.405949406250003975, -9.363379034771801557, -108.5312500020483810 ) ) ;
#20053 = CARTESIAN_POINT ( 'NONE',  ( 9.999999999999996447, -5.773502691896262640, -188.5000000040968189 ) ) ;
#20054 = CARTESIAN_POINT ( 'NONE',  ( 5.405949406249999534, 9.363379034771803333, -116.5937500020483810 ) ) ;
#20055 = CARTESIAN_POINT ( 'NONE',  ( 5.405949406249999534, 9.363379034771803333, -188.7812500020484094 ) ) ;
#20056 = CARTESIAN_POINT ( 'NONE',  ( -25.00000000000000000, 0.000000000000000000, -160.0000000000000000 ) ) ;
#20057 = CARTESIAN_POINT ( 'NONE',  ( 9.999999999999998224, 0.000000000000000000, -113.3750000040967763 ) ) ;
#20058 = CARTESIAN_POINT ( 'NONE',  ( -4.999999999999996447, 8.660254037844387298, -129.0000000000000000 ) ) ;
#20059 = CARTESIAN_POINT ( 'NONE',  ( 5.000000000000000000, 8.660254037844385522, -6.249999999999977796 ) ) ;
#20060 = CARTESIAN_POINT ( 'NONE',  ( 5.405949406249999534, 9.363379034771803333, -59.59375000204835970 ) ) ;
#20061 = CARTESIAN_POINT ( 'NONE',  ( -5.405949406249996869, 9.363379034771805109, -45.84375000204838102 ) ) ;
#20062 = CARTESIAN_POINT ( 'NONE',  ( 9.999999999999998224, 0.000000000000000000, -183.8750000040967905 ) ) ;
#20063 = CARTESIAN_POINT ( 'NONE',  ( 10.81189881249999907, 6.242252689847868297, -14.90625000204837036 ) ) ;
#20064 = CARTESIAN_POINT ( 'NONE',  ( -5.405949406249996869, 9.363379034771805109, -27.84375000204836326 ) ) ;
#20065 = CARTESIAN_POINT ( 'NONE',  ( 9.999999999999998224, 0.000000000000000000, -146.0000000000000000 ) ) ;
#20066 = CARTESIAN_POINT ( 'NONE',  ( 10.81189881249999551, -6.242252689847874514, -134.9687500020483810 ) ) ;
#20067 = CARTESIAN_POINT ( 'NONE',  ( 9.999999999999998224, 0.000000000000000000, -102.5000000000000000 ) ) ;
#20068 = CARTESIAN_POINT ( 'NONE',  ( 5.405949406249999534, 9.363379034771803333, -38.78125000204838102 ) ) ;
#20069 = CARTESIAN_POINT ( 'NONE',  ( -4.999999999999996447, 8.660254037844387298, -118.8750000040967905 ) ) ;
#20070 = CARTESIAN_POINT ( 'NONE',  ( 4.999999999999992006, -8.660254037844389075, -62.24999999999997158 ) ) ;
#20071 = CARTESIAN_POINT ( 'NONE',  ( 10.81189881249999907, 6.242252689847868297, -130.4062500020483810 ) ) ;
#20072 = CARTESIAN_POINT ( 'NONE',  ( -10.81189881249999729, -6.242252689847864744, -110.1562500020483952 ) ) ;
#20073 = ORIENTED_EDGE ( 'NONE', *, *, #40070, .T. ) ;
#20074 = AXIS2_PLACEMENT_3D ( 'NONE', #24727, #41729, #15401 ) ;
#20075 = CARTESIAN_POINT ( 'NONE',  ( -5.000000000000003553, -8.660254037844383745, -131.5000000000000000 ) ) ;
#20076 = CARTESIAN_POINT ( 'NONE',  ( -4.999999999999996447, 8.660254037844387298, -105.3750000040967763 ) ) ;
#20077 = CARTESIAN_POINT ( 'NONE',  ( -9.999999999999227285, -5.773502691896698735, -107.6249999999999574 ) ) ;
#20078 = CARTESIAN_POINT ( 'NONE',  ( 5.405949406249999534, 9.363379034771803333, -65.59375000204836681 ) ) ;
#20079 = EDGE_LOOP ( 'NONE', ( #12080, #12811, #39512, #18689 ) ) ;
#20080 = CARTESIAN_POINT ( 'NONE',  ( 7.070501591499377789E-16, 11.54700538379251284, -31.62499999999995737 ) ) ;
#20081 = LOCAL_TIME ( 11, 57, 6.000000000000000000, #20257 ) ;
#20082 = CARTESIAN_POINT ( 'NONE',  ( -10.00000000000000000, -5.773502691896251982, -16.50000000409675849 ) ) ;
#20083 = CARTESIAN_POINT ( 'NONE',  ( -10.81189881249999729, 6.242252689847871849, -47.40625000204836681 ) ) ;
#20084 = CARTESIAN_POINT ( 'NONE',  ( 5.000000000000000000, 8.660254037844385522, -125.1250000040967620 ) ) ;
#20085 = CARTESIAN_POINT ( 'NONE',  ( 9.999999999999996447, -5.773502691896262640, -32.50000000409675494 ) ) ;
#20086 =( BOUNDED_CURVE ( )  B_SPLINE_CURVE ( 2, ( #28668, #32537, #3177, #22387, #25426, #42431, #15881 ),
 .UNSPECIFIED., .F., .F. ) 
 B_SPLINE_CURVE_WITH_KNOTS ( ( 3, 2, 2, 3 ),
 ( 0.1641791044776119424, 0.1654228855721392999, 0.1666666666666666574, 0.1679104477611940427 ),
 .UNSPECIFIED. ) 
 CURVE ( )  GEOMETRIC_REPRESENTATION_ITEM ( )  RATIONAL_B_SPLINE_CURVE ( ( 1.000000000000000000, 0.8660254037844387076, 1.000000000000000000, 0.8660254037844387076, 1.000000000000000000, 0.8660254037844387076, 1.000000000000000000 ) ) 
 REPRESENTATION_ITEM ( '' )  );
#20087 = CARTESIAN_POINT ( 'NONE',  ( -4.999999999999996447, 8.660254037844387298, -117.3750000040967905 ) ) ;
#20088 = AXIS2_PLACEMENT_3D ( 'NONE', #23021, #19977, #6409 ) ;
#20089 = CARTESIAN_POINT ( 'NONE',  ( -10.81189881249999729, 1.324075727343319199E-15, -143.2812500020483810 ) ) ;
#20090 = DIRECTION ( 'NONE',  ( -0.000000000000000000, -0.000000000000000000, -1.000000000000000000 ) ) ;
#20091 = ORIENTED_EDGE ( 'NONE', *, *, #14883, .F. ) ;
#20092 = ORIENTED_EDGE ( 'NONE', *, *, #38191, .T. ) ;
#20093 = VERTEX_POINT ( 'NONE', #13399 ) ;
#20094 = VECTOR ( 'NONE', #23232, 1000.000000000000000 ) ;
#20095 = DIRECTION ( 'NONE',  ( 1.000000000000000000, 0.000000000000000000, 0.000000000000000000 ) ) ;
#20096 = CARTESIAN_POINT ( 'NONE',  ( 10.81189881249999729, 0.000000000000000000, -175.3437500020483810 ) ) ;
#20097 = EDGE_CURVE ( 'NONE', #25539, #5420, #85, .T. ) ;
#20098 = CARTESIAN_POINT ( 'NONE',  ( 5.405949406249992428, -9.363379034771808662, -22.59375000204835615 ) ) ;
#20099 = CARTESIAN_POINT ( 'NONE',  ( 9.999999999999998224, 0.000000000000000000, -144.8750000040967905 ) ) ;
#20100 = APPLICATION_CONTEXT ( 'configuration controlled 3d designs of mechanical parts and assemblies' ) ;
#20101 = CARTESIAN_POINT ( 'NONE',  ( 0.000000000000000000, 0.000000000000000000, -169.9999999999999716 ) ) ;
#20102 = ADVANCED_FACE ( 'NONE', ( #36091 ), #26381, .F. ) ;
#20103 = CARTESIAN_POINT ( 'NONE',  ( 7.644554776091147741E-16, 12.48450537969573659, -156.9687500020484094 ) ) ;
#20104 = CARTESIAN_POINT ( 'NONE',  ( -5.405949406250003975, -9.363379034771801557, -136.8437500020484094 ) ) ;
#20105 = EDGE_CURVE ( 'NONE', #37673, #33065, #26292, .T. ) ;
#20106 = CARTESIAN_POINT ( 'NONE',  ( -5.000000000000003553, -8.660254037844383745, -119.5000000000000000 ) ) ;
#20107 = CARTESIAN_POINT ( 'NONE',  ( -10.81189881249999907, -6.242252689847864744, -121.9687500020483952 ) ) ;
#20108 = CARTESIAN_POINT ( 'NONE',  ( 5.405949406249992428, -9.363379034771808662, -132.2812500020483810 ) ) ;
#20109 = CARTESIAN_POINT ( 'NONE',  ( -2.293366432827344421E-15, -12.48450537969573659, -13.71875000204836503 ) ) ;
#20111 = EDGE_CURVE ( 'NONE', #28436, #41907, #8905, .T. ) ;
#20110 = CARTESIAN_POINT ( 'NONE',  ( 5.405949406249992428, -9.363379034771808662, -136.5937500020483810 ) ) ;
#20112 = PLANE ( 'NONE',  #13644 ) ;
#20113 = CARTESIAN_POINT ( 'NONE',  ( -9.999999999999998224, 1.224646799147353059E-15, -141.1250000040967905 ) ) ;
#20114 = CARTESIAN_POINT ( 'NONE',  ( 9.999999999999998224, 0.000000000000000000, -153.5000000000000000 ) ) ;
#20115 = CARTESIAN_POINT ( 'NONE',  ( 5.405949406249992428, -9.363379034771808662, -0.2812500020483721386 ) ) ;
#20116 = VECTOR ( 'NONE', #30087, 1000.000000000000000 ) ;
#20117 = CARTESIAN_POINT ( 'NONE',  ( -5.405949406250003975, -9.363379034771801557, -84.34375000204836681 ) ) ;
#20118 = CARTESIAN_POINT ( 'NONE',  ( 7.644554776091147741E-16, 12.48450537969573659, -69.96875000204838102 ) ) ;
#20119 = CARTESIAN_POINT ( 'NONE',  ( 5.405949406249999534, 9.363379034771803333, -46.28125000204838813 ) ) ;
#20120 = CARTESIAN_POINT ( 'NONE',  ( -10.81189881249999907, -6.242252689847864744, -51.46875000204837391 ) ) ;
#20121 = CARTESIAN_POINT ( 'NONE',  ( 9.999999999999998224, 0.000000000000000000, -138.8750000040968189 ) ) ;
#20122 = CARTESIAN_POINT ( 'NONE',  ( 7.644554776091147741E-16, 12.48450537969573659, -162.9687500020483810 ) ) ;
#20123 = CARTESIAN_POINT ( 'NONE',  ( 9.999999999999998224, 0.000000000000000000, -129.5000000000000000 ) ) ;
#20124 = CARTESIAN_POINT ( 'NONE',  ( 10.81189881249999729, 6.242252689847867408, -139.4062500020484094 ) ) ;
#20125 = DIRECTION ( 'NONE',  ( -0.000000000000000000, -0.000000000000000000, -1.000000000000000000 ) ) ;
#20126 = CARTESIAN_POINT ( 'NONE',  ( -9.999999999999998224, 5.773502691896259087, -82.37499999999998579 ) ) ;
#20127 = ORIENTED_EDGE ( 'NONE', *, *, #18147, .F. ) ;
#20128 = CARTESIAN_POINT ( 'NONE',  ( 5.405949406249992428, -9.363379034771808662, -109.7812500020483810 ) ) ;
#20129 = CARTESIAN_POINT ( 'NONE',  ( -5.000000000000003553, -8.660254037844383745, -130.3750000040967905 ) ) ;
#20130 = CARTESIAN_POINT ( 'NONE',  ( 0.000000000000000000, 0.000000000000000000, -99.99999999999998579 ) ) ;
#20131 = CARTESIAN_POINT ( 'NONE',  ( -5.405949406249996869, 9.363379034771805109, -164.5312500020484094 ) ) ;
#20132 = CARTESIAN_POINT ( 'NONE',  ( 9.999999999999998224, 0.000000000000000000, -41.37500000409677625 ) ) ;
#20133 = EDGE_CURVE ( 'NONE', #21791, #29783, #6736, .T. ) ;
#20134 = CARTESIAN_POINT ( 'NONE',  ( -9.999999999999998224, 1.224646799147353059E-15, -154.6250000040967905 ) ) ;
#20135 = CARTESIAN_POINT ( 'NONE',  ( 5.405949406249999534, 9.363379034771803333, -55.28125000204836681 ) ) ;
#20136 = CARTESIAN_POINT ( 'NONE',  ( -9.999999999999998224, 1.224646799147353059E-15, -64.24999999999997158 ) ) ;
#20137 = CARTESIAN_POINT ( 'NONE',  ( -2.293366432827344421E-15, -12.48450537969573659, -160.9062500020483810 ) ) ;
#20138 = EDGE_CURVE ( 'NONE', #24966, #6565, #39518, .T. ) ;
#20139 = CARTESIAN_POINT ( 'NONE',  ( 10.81189881249999551, -6.242252689847874514, -136.4687500020483810 ) ) ;
#20140 = DIRECTION ( 'NONE',  ( -0.000000000000000000, -0.000000000000000000, 1.000000000000000000 ) ) ;
#20141 = CARTESIAN_POINT ( 'NONE',  ( 9.999999999999998224, 0.000000000000000000, -152.0000000000000000 ) ) ;
#20142 = EDGE_CURVE ( 'NONE', #40993, #37069, #8653, .T. ) ;
#20143 = ORIENTED_EDGE ( 'NONE', *, *, #18509, .F. ) ;
#20144 = PLANE ( 'NONE',  #25901 ) ;
#20145 = AXIS2_PLACEMENT_3D ( 'NONE', #28763, #15352, #28967 ) ;
#20147 = ORIENTED_EDGE ( 'NONE', *, *, #33532, .F. ) ;
#20146 = CARTESIAN_POINT ( 'NONE',  ( -5.405949406249996869, 9.363379034771805109, -71.53125000204838102 ) ) ;
#20149 = ORIENTED_EDGE ( 'NONE', *, *, #26939, .F. ) ;
#20148 = CARTESIAN_POINT ( 'NONE',  ( -10.81189881249999729, 6.242252689847871849, -116.2187500020483810 ) ) ;
#20150 = CARTESIAN_POINT ( 'NONE',  ( 10.81189881249999729, 0.000000000000000000, -22.34375000204835615 ) ) ;
#20151 = CARTESIAN_POINT ( 'NONE',  ( -10.81189881249999907, -6.242252689847864744, -195.4687500020484094 ) ) ;
#20152 = CARTESIAN_POINT ( 'NONE',  ( 5.405949406249992428, -9.363379034771808662, -45.09375000204837391 ) ) ;
#20153 = CARTESIAN_POINT ( 'NONE',  ( 9.999999999999998224, 0.000000000000000000, -200.0000000000000000 ) ) ;
#20154 = CYLINDRICAL_SURFACE ( 'NONE', #438, 24.99999999999999645 ) ;
#20155 = CARTESIAN_POINT ( 'NONE',  ( 5.405949406249992428, -9.363379034771808662, -177.0937500020484094 ) ) ;
#20156 = CARTESIAN_POINT ( 'NONE',  ( -10.81189881249999907, -6.242252689847864744, -171.4687500020484094 ) ) ;
#20157 = CARTESIAN_POINT ( 'NONE',  ( -10.81189881249999729, 1.324075727343319199E-15, -147.5937500020483810 ) ) ;
#20159 = EDGE_CURVE ( 'NONE', #13374, #34507, #13023, .T. ) ;
#20158 = CARTESIAN_POINT ( 'NONE',  ( -10.81189881249999729, 1.324075727343319199E-15, -164.0937500020484094 ) ) ;
#20160 = DIRECTION ( 'NONE',  ( -0.000000000000000000, -0.000000000000000000, -1.000000000000000000 ) ) ;
#20161 = CARTESIAN_POINT ( 'NONE',  ( 9.999999999999998224, 0.000000000000000000, -141.8750000040967905 ) ) ;
#20162 = CARTESIAN_POINT ( 'NONE',  ( -2.121150477449813534E-15, -11.54700538379251284, -177.8750000000000284 ) ) ;
#20163 = CARTESIAN_POINT ( 'NONE',  ( -10.81189881249999729, 1.324075727343319199E-15, -98.09375000204838102 ) ) ;
#20164 = CARTESIAN_POINT ( 'NONE',  ( 5.000000000000000000, 8.660254037844385522, -151.7500000000000000 ) ) ;
#20165 = CARTESIAN_POINT ( 'NONE',  ( -2.293366432827344421E-15, -12.48450537969573659, -64.90625000204838102 ) ) ;
#20166 = DIRECTION ( 'NONE',  ( -1.000000000000000000, 0.000000000000000000, 0.000000000000000000 ) ) ;
#20167 = CARTESIAN_POINT ( 'NONE',  ( -10.81189881249999729, 6.242252689847871849, -183.7187500020484379 ) ) ;
#20168 = CARTESIAN_POINT ( 'NONE',  ( -5.405949406250003975, -9.363379034771801557, -119.0312500020483952 ) ) ;
#20169 = CARTESIAN_POINT ( 'NONE',  ( -10.81189881249999729, 1.324075727343319199E-15, -159.7812500020484094 ) ) ;
#20170 =( BOUNDED_CURVE ( )  B_SPLINE_CURVE ( 2, ( #3488, #16625, #12754, #482, #19878, #16836, #29828 ),
 .UNSPECIFIED., .F., .F. ) 
 B_SPLINE_CURVE_WITH_KNOTS ( ( 3, 2, 2, 3 ),
 ( 0.9141791044776121922, 0.9154228855721395774, 0.9166666666666669627, 0.9179104477611943480 ),
 .UNSPECIFIED. ) 
 CURVE ( )  GEOMETRIC_REPRESENTATION_ITEM ( )  RATIONAL_B_SPLINE_CURVE ( ( 0.9999999999999761302, 0.8660254037844625774, 1.000000000000000000, 0.8660254037844387076, 1.000000000000000000, 0.8660254037844028474, 1.000000000000035971 ) ) 
 REPRESENTATION_ITEM ( '' )  );
#20171 = CARTESIAN_POINT ( 'NONE',  ( -10.81189881249999729, 6.242252689847871849, -54.90625000204837391 ) ) ;
#20172 = CARTESIAN_POINT ( 'NONE',  ( 5.000000000000000000, 8.660254037844385522, -134.1250000040967620 ) ) ;
#20173 = CARTESIAN_POINT ( 'NONE',  ( -9.999999999999998224, 1.224646799147353059E-15, -115.2499999999999858 ) ) ;
#20174 = ORIENTED_EDGE ( 'NONE', *, *, #27900, .F. ) ;
#20175 = CARTESIAN_POINT ( 'NONE',  ( -5.405949406250003975, -9.363379034771801557, -134.0312500020484094 ) ) ;
#20176 = CARTESIAN_POINT ( 'NONE',  ( 10.81189881249999551, -6.242252689847874514, -147.1562500020484094 ) ) ;
#20177 = CARTESIAN_POINT ( 'NONE',  ( 7.644554776091147741E-16, 12.48450537969573659, -191.6562500020484094 ) ) ;
#20178 = CARTESIAN_POINT ( 'NONE',  ( -2.121150477449813534E-15, -11.54700538379251284, -125.3749999999999858 ) ) ;
#20179 = CARTESIAN_POINT ( 'NONE',  ( -10.81189881249999729, 6.242252689847871849, -81.71875000204838102 ) ) ;
#20180 = VERTEX_POINT ( 'NONE', #29840 ) ;
#20181 = CARTESIAN_POINT ( 'NONE',  ( 7.070501591499377789E-16, 11.54700538379251284, -55.62499999999997868 ) ) ;
#20182 = CARTESIAN_POINT ( 'NONE',  ( 7.644554776091147741E-16, 12.48450537969573659, -182.4687500020484094 ) ) ;
#20183 = CARTESIAN_POINT ( 'NONE',  ( -9.999999999999998224, 5.773502691896259087, -66.25000000409677625 ) ) ;
#20184 = DIRECTION ( 'NONE',  ( 1.000000000000000000, 0.000000000000000000, 0.000000000000000000 ) ) ;
#20185 = CARTESIAN_POINT ( 'NONE',  ( 9.999999999999998224, 0.000000000000000000, -158.0000000000000000 ) ) ;
#20186 = CARTESIAN_POINT ( 'NONE',  ( 5.405949406249992428, -9.363379034771808662, -75.28125000204838102 ) ) ;
#20187 = CARTESIAN_POINT ( 'NONE',  ( -10.81189881249999729, 1.324075727343319199E-15, -59.28125000204836681 ) ) ;
#20188 = ADVANCED_FACE ( 'NONE', ( #35091 ), #25171, .F. ) ;
#20189 = CARTESIAN_POINT ( 'NONE',  ( -5.000000000000003553, -8.660254037844383745, -55.37500000409675494 ) ) ;
#20190 = CARTESIAN_POINT ( 'NONE',  ( -5.405949406249996869, 9.363379034771805109, -8.343750002048345493 ) ) ;
#20191 = CARTESIAN_POINT ( 'NONE',  ( -9.999999999999998224, 1.224646799147353059E-15, -138.1250000040967620 ) ) ;
#20192 = CARTESIAN_POINT ( 'NONE',  ( -10.81189881249999729, 6.242252689847871849, -183.9062500020484094 ) ) ;
#20193 = CARTESIAN_POINT ( 'NONE',  ( 10.81189881249999551, -6.242252689847874514, -7.656250002048365921 ) ) ;
#20194 = CARTESIAN_POINT ( 'NONE',  ( -5.000000000000003553, -8.660254037844383745, -172.3750000040968189 ) ) ;
#20195 = CARTESIAN_POINT ( 'NONE',  ( 4.999999999999992006, -8.660254037844389075, -148.1250000040967905 ) ) ;
#20196 = CARTESIAN_POINT ( 'NONE',  ( -9.999999999999998224, 1.224646799147353059E-15, -46.24999999999998579 ) ) ;
#20197 = CARTESIAN_POINT ( 'NONE',  ( 0.000000000000000000, 0.000000000000000000, -200.0000000000000000 ) ) ;
#20198 = CARTESIAN_POINT ( 'NONE',  ( 10.00000000000025402, -5.773502691896113426, -122.1250000000000000 ) ) ;
#20200 = ORIENTED_EDGE ( 'NONE', *, *, #948, .T. ) ;
#20199 = CARTESIAN_POINT ( 'NONE',  ( 10.81189881249999729, 0.000000000000000000, -96.03125000204838102 ) ) ;
#20201 = CARTESIAN_POINT ( 'NONE',  ( 5.000000000000000000, 8.660254037844385522, -24.62500000409675849 ) ) ;
#20203 = EDGE_LOOP ( 'NONE', ( #32721, #16248, #37404, #11594, #22240, #4416 ) ) ;
#20202 = CARTESIAN_POINT ( 'NONE',  ( -4.999999999999996447, 8.660254037844387298, -162.0000000000000000 ) ) ;
#20204 = VERTEX_POINT ( 'NONE', #15209 ) ;
#20205 = CARTESIAN_POINT ( 'NONE',  ( -2.293366432827344421E-15, -12.48450537969573659, -31.71875000204834905 ) ) ;
#20206 = CARTESIAN_POINT ( 'NONE',  ( -10.81189881249999907, -6.242252689847864744, -20.15625000204838102 ) ) ;
#20207 = CARTESIAN_POINT ( 'NONE',  ( 10.81189881249999907, 6.242252689847868297, -71.71875000204838102 ) ) ;
#20208 = CARTESIAN_POINT ( 'NONE',  ( -9.999999999999998224, 1.224646799147353059E-15, -18.12500000409675138 ) ) ;
#20209 = CARTESIAN_POINT ( 'NONE',  ( -9.999999999999998224, 1.224646799147353059E-15, -47.74999999999998579 ) ) ;
#20210 = CARTESIAN_POINT ( 'NONE',  ( 10.81189881249999729, 0.000000000000000000, -194.8437500020484094 ) ) ;
#20211 = CARTESIAN_POINT ( 'NONE',  ( -5.405949406250003975, -9.363379034771801557, -148.8437500020483810 ) ) ;
#20212 =( BOUNDED_CURVE ( )  B_SPLINE_CURVE ( 2, ( #38803, #6005, #8816, #5576, #31708, #12247, #2768 ),
 .UNSPECIFIED., .F., .F. ) 
 B_SPLINE_CURVE_WITH_KNOTS ( ( 3, 2, 2, 3 ),
 ( 0.3544776119402986980, 0.3557213930348260278, 0.3569651741293533576, 0.3582089552238806873 ),
 .UNSPECIFIED. ) 
 CURVE ( )  GEOMETRIC_REPRESENTATION_ITEM ( )  RATIONAL_B_SPLINE_CURVE ( ( 0.9999999999999820144, 0.8660254037844566932, 1.000000000000000000, 0.8660254037844387076, 1.000000000000000000, 0.8660254037844267172, 1.000000000000011990 ) ) 
 REPRESENTATION_ITEM ( '' )  );
#20213 = CARTESIAN_POINT ( 'NONE',  ( 4.999999999999992006, -8.660254037844389075, -79.12500000409677625 ) ) ;
#20214 = CARTESIAN_POINT ( 'NONE',  ( 5.000000000000000000, 8.660254037844385522, -112.7499999999999858 ) ) ;
#20215 = CARTESIAN_POINT ( 'NONE',  ( -5.405949406250003975, -9.363379034771801557, -150.5312500020483810 ) ) ;
#20216 = CARTESIAN_POINT ( 'NONE',  ( 9.999999999999996447, -5.773502691896262640, -4.000000004096762929 ) ) ;
#20217 = CARTESIAN_POINT ( 'NONE',  ( 10.81189881249999551, -6.242252689847874514, -124.4687500020483952 ) ) ;
#20218 = CARTESIAN_POINT ( 'NONE',  ( 9.999999999999998224, 0.000000000000000000, -200.0000000000000000 ) ) ;
#20219 = CARTESIAN_POINT ( 'NONE',  ( -10.81189881249999907, -6.242252689847864744, -89.15625000204839523 ) ) ;
#20220 = CARTESIAN_POINT ( 'NONE',  ( -2.293366432827344421E-15, -12.48450537969573659, -105.2187500020483952 ) ) ;
#20221 = CARTESIAN_POINT ( 'NONE',  ( -2.293366432827344421E-15, -12.48450537969573659, -70.71875000204838102 ) ) ;
#20222 = CARTESIAN_POINT ( 'NONE',  ( 10.81189881249999907, 6.242252689847868297, -77.90625000204836681 ) ) ;
#20223 = CARTESIAN_POINT ( 'NONE',  ( 9.999999999999998224, 0.000000000000000000, -158.3750000040967905 ) ) ;
#20224 = CARTESIAN_POINT ( 'NONE',  ( 5.405949406249992428, -9.363379034771808662, -162.2812500020484094 ) ) ;
#20225 = CARTESIAN_POINT ( 'NONE',  ( 5.405949406249992428, -9.363379034771808662, -172.7812500020484094 ) ) ;
#20226 = EDGE_CURVE ( 'NONE', #28132, #4695, #13281, .T. ) ;
#20227 = CARTESIAN_POINT ( 'NONE',  ( 0.000000000000000000, 0.000000000000000000, -99.99999999999998579 ) ) ;
#20228 = CARTESIAN_POINT ( 'NONE',  ( -9.999999999999479527, -5.773502691896549521, -145.5000000040967905 ) ) ;
#20229 = CARTESIAN_POINT ( 'NONE',  ( 9.999999999999998224, 1.224646799147353059E-15, -99.99999999999998579 ) ) ;
#20230 = CARTESIAN_POINT ( 'NONE',  ( 5.405949406249999534, 9.363379034771803333, -107.5937500020483810 ) ) ;
#20231 = CARTESIAN_POINT ( 'NONE',  ( 5.000000000000000000, 8.660254037844385522, -82.74999999999997158 ) ) ;
#20232 = CARTESIAN_POINT ( 'NONE',  ( 10.81189881249999551, -6.242252689847874514, -4.656250002048361480 ) ) ;
#20233 = CARTESIAN_POINT ( 'NONE',  ( -9.999999999999998224, 1.224646799147353059E-15, -90.12500000409677625 ) ) ;
#20234 = CARTESIAN_POINT ( 'NONE',  ( 9.999999999999998224, 0.000000000000000000, -168.8750000040967905 ) ) ;
#20235 = CARTESIAN_POINT ( 'NONE',  ( 10.81189881249999729, 0.000000000000000000, -102.0312500020483952 ) ) ;
#20236 = CARTESIAN_POINT ( 'NONE',  ( 10.81189881249999729, 6.242252689847867408, -83.90625000204836681 ) ) ;
#20237 = ORIENTED_EDGE ( 'NONE', *, *, #11922, .F. ) ;
#20238 = CARTESIAN_POINT ( 'NONE',  ( 5.000000000000000000, 8.660254037844385522, -74.12500000409677625 ) ) ;
#20239 = LINE ( 'NONE', #33428, #13226 ) ;
#20240 = CARTESIAN_POINT ( 'NONE',  ( -5.405949406249996869, 9.363379034771805109, -32.34375000204836681 ) ) ;
#20241 = ORIENTED_EDGE ( 'NONE', *, *, #20405, .F. ) ;
#20242 = CARTESIAN_POINT ( 'NONE',  ( 7.070501591499377789E-16, 11.54700538379251284, -10.62499999999995381 ) ) ;
#20243 = CARTESIAN_POINT ( 'NONE',  ( -5.405949406249996869, 9.363379034771805109, -35.53125000204837391 ) ) ;
#20244 = CARTESIAN_POINT ( 'NONE',  ( 5.000000000000000000, 8.660254037844385522, -145.7500000000000000 ) ) ;
#20245 = CARTESIAN_POINT ( 'NONE',  ( 10.00000000000154010, -5.773502691895370020, -14.50000000409672296 ) ) ;
#20246 = CARTESIAN_POINT ( 'NONE',  ( 9.999999999999996447, -5.773502691896262640, -11.50000000409676026 ) ) ;
#20247 = EDGE_CURVE ( 'NONE', #37944, #32539, #17691, .T. ) ;
#20248 = CARTESIAN_POINT ( 'NONE',  ( -4.999999999999996447, 8.660254037844387298, -189.0000000000000000 ) ) ;
#20249 = CARTESIAN_POINT ( 'NONE',  ( 9.999999999999998224, 0.000000000000000000, -155.3750000040967905 ) ) ;
#20251 = VERTEX_POINT ( 'NONE', #8548 ) ;
#20250 = CARTESIAN_POINT ( 'NONE',  ( -10.81189881249999729, 6.242252689847871849, -117.9062500020483952 ) ) ;
#20252 = CARTESIAN_POINT ( 'NONE',  ( -2.121150477449813534E-15, -11.54700538379251284, -74.75000000409677625 ) ) ;
#20253 = ORIENTED_EDGE ( 'NONE', *, *, #19927, .T. ) ;
#20254 = B_SPLINE_CURVE_WITH_KNOTS ( 'NONE', 3,
 ( #5192, #40783, #11864, #24633, #25062, #4547, #27430, #31104, #1536, #14671, #37778, #11646, #20942, #34984, #21371, #18126, #21592, #24203, #4982, #8441, #40564, #1754, #34127, #24848, #17688, #14882, #37995, #26105 ),
 .UNSPECIFIED., .F., .F.,
 ( 4, 2, 2, 2, 2, 2, 2, 2, 2, 2, 2, 2, 2, 4 ),
 ( 0.000000000000000000, 0.001274091078800513406, 0.002548182157601026811, 0.005096364315202054490, 0.006370455394002568980, 0.007644546472803081735, 0.01019272863040411072, 0.01146681970920462521, 0.01274091078800513796, 0.01401500186680565245, 0.01528909294560616347, 0.01656318402440667623, 0.01783727510320719245, 0.02038545726080821796 ),
 .UNSPECIFIED. ) ;
#20255 = ORIENTED_EDGE ( 'NONE', *, *, #11922, .T. ) ;
#20256 = CARTESIAN_POINT ( 'NONE',  ( 10.81189881249999729, 0.000000000000000000, -46.53125000204838813 ) ) ;
#20257 = COORDINATED_UNIVERSAL_TIME_OFFSET ( 6, 0, .AHEAD. ) ;
#20258 = B_SPLINE_CURVE_WITH_KNOTS ( 'NONE', 3,
 ( #6328, #3086, #29415, #2878, #283, #23580, #29203, #42343, #68, #12774, #25967, #39118 ),
 .UNSPECIFIED., .F., .F.,
 ( 4, 2, 2, 2, 2, 4 ),
 ( 4.983255971813266780E-16, 0.002144051117877383752, 0.004288102235754269638, 0.005360127794692712798, 0.006432153353631154223, 0.008576204471508041410 ),
 .UNSPECIFIED. ) ;
#20259 = CARTESIAN_POINT ( 'NONE',  ( -5.405949406249996869, 9.363379034771805109, -93.84375000204838102 ) ) ;
#20260 = CARTESIAN_POINT ( 'NONE',  ( -10.81189881249999729, 6.242252689847871849, -120.9062500020483952 ) ) ;
#20261 = EDGE_LOOP ( 'NONE', ( #11114, #2243, #2760, #2814 ) ) ;
#20262 = CARTESIAN_POINT ( 'NONE',  ( -9.999999999998456346, -5.773502691897145489, -83.62499999999994316 ) ) ;
#20263 = CARTESIAN_POINT ( 'NONE',  ( 10.81189881249999729, 6.242252689847867408, -197.7187500020484094 ) ) ;
#20264 = CARTESIAN_POINT ( 'NONE',  ( -10.81189881249999907, -6.242252689847864744, -176.1562500020483810 ) ) ;
#20265 = CARTESIAN_POINT ( 'NONE',  ( 5.000000000000000000, 8.660254037844385522, -0.6250000040967651493 ) ) ;
#20266 = CARTESIAN_POINT ( 'NONE',  ( 5.405949406249999534, 9.363379034771803333, -133.0937500020483810 ) ) ;
#20267 = CARTESIAN_POINT ( 'NONE',  ( 5.405949406249992428, -9.363379034771808662, -90.09375000204838102 ) ) ;
#20268 = CARTESIAN_POINT ( 'NONE',  ( -9.999999999999998224, 1.224646799147353059E-15, -17.74999999999996092 ) ) ;
#20269 = CARTESIAN_POINT ( 'NONE',  ( 7.644554776091147741E-16, 12.48450537969573659, -98.65625000204838102 ) ) ;
#20270 = CARTESIAN_POINT ( 'NONE',  ( -4.999999999999996447, 8.660254037844387298, -184.8750000040967905 ) ) ;
#20271 = CARTESIAN_POINT ( 'NONE',  ( -10.81189881249999729, 1.324075727343319199E-15, -113.0937500020483810 ) ) ;
#20272 = CARTESIAN_POINT ( 'NONE',  ( -5.405949406249996869, 9.363379034771805109, -178.0312500020483810 ) ) ;
#20273 = EDGE_CURVE ( 'NONE', #13430, #6396, #22132, .T. ) ;
#20274 = CARTESIAN_POINT ( 'NONE',  ( -9.999999999999998224, 1.224646799147353059E-15, -105.1250000040967763 ) ) ;
#20275 = CARTESIAN_POINT ( 'NONE',  ( 9.999999999999998224, 0.000000000000000000, -122.3750000040967905 ) ) ;
#20276 = CARTESIAN_POINT ( 'NONE',  ( -5.405949406250003975, -9.363379034771801557, -197.0312500020484094 ) ) ;
#20277 = CARTESIAN_POINT ( 'NONE',  ( -10.81189881249999729, 1.324075727343319199E-15, -59.09375000204835970 ) ) ;
#20278 = CARTESIAN_POINT ( 'NONE',  ( -5.405949406250003975, -9.363379034771801557, -43.84375000204837391 ) ) ;
#20279 = CARTESIAN_POINT ( 'NONE',  ( -2.121150477449813534E-15, -11.54700538379251284, -170.7500000040967620 ) ) ;
#20280 = CARTESIAN_POINT ( 'NONE',  ( 10.81189881249999551, -6.242252689847874514, -21.15625000204836681 ) ) ;
#20281 = CARTESIAN_POINT ( 'NONE',  ( 10.81189881249999551, -6.242252689847874514, -20.96875000204837036 ) ) ;
#20282 = CARTESIAN_POINT ( 'NONE',  ( -2.293366432827344421E-15, -12.48450537969573659, -130.7187500020483810 ) ) ;
#20283 = CARTESIAN_POINT ( 'NONE',  ( 5.000000000000000000, 8.660254037844385522, -108.2499999999999858 ) ) ;
#20284 = CARTESIAN_POINT ( 'NONE',  ( 10.81189881249999907, 6.242252689847868297, -26.90625000204838813 ) ) ;
#20285 = CARTESIAN_POINT ( 'NONE',  ( -4.999999999999996447, 8.660254037844387298, -102.0000000000000000 ) ) ;
#20286 = CARTESIAN_POINT ( 'NONE',  ( 9.999999999999996447, -5.773502691896262640, -60.62499999999998579 ) ) ;
#20287 = CARTESIAN_POINT ( 'NONE',  ( -5.405949406249996869, 9.363379034771805109, -131.5312500020484094 ) ) ;
#20288 = CARTESIAN_POINT ( 'NONE',  ( 10.81189881249999729, 0.000000000000000000, -109.5312500020483810 ) ) ;
#20289 = EDGE_LOOP ( 'NONE', ( #31160, #11275, #35249, #41264 ) ) ;
#20290 = CARTESIAN_POINT ( 'NONE',  ( -9.999999999999998224, 1.224646799147353059E-15, -160.2500000000000000 ) ) ;
#20291 = CARTESIAN_POINT ( 'NONE',  ( -2.121150477449813534E-15, -11.54700538379251284, -110.7500000040967763 ) ) ;
#20292 = CARTESIAN_POINT ( 'NONE',  ( 5.405949406249999534, 9.363379034771803333, -62.59375000204836681 ) ) ;
#20293 = ORIENTED_EDGE ( 'NONE', *, *, #15218, .F. ) ;
#20294 = CARTESIAN_POINT ( 'NONE',  ( -9.999999999999998224, 5.773502691896259087, -37.37499999999995026 ) ) ;
#20295 = CARTESIAN_POINT ( 'NONE',  ( 7.644554776091147741E-16, 12.48450537969573659, -34.15625000204836681 ) ) ;
#20296 = CARTESIAN_POINT ( 'NONE',  ( 7.070501591499376803E-16, 11.54700538379251284, -111.5000000040967763 ) ) ;
#20297 = CARTESIAN_POINT ( 'NONE',  ( -2.121150477449813534E-15, -11.54700538379251284, -35.75000000409675494 ) ) ;
#20298 = DIRECTION ( 'NONE',  ( -0.000000000000000000, -0.000000000000000000, -1.000000000000000000 ) ) ;
#20299 = CARTESIAN_POINT ( 'NONE',  ( 10.81189881249999907, 6.242252689847868297, -140.9062500020484094 ) ) ;
#20300 = EDGE_CURVE ( 'NONE', #38638, #38155, #8684, .T. ) ;
#20301 = DIRECTION ( 'NONE',  ( -0.000000000000000000, -0.000000000000000000, -1.000000000000000000 ) ) ;
#20302 = ORIENTED_EDGE ( 'NONE', *, *, #40683, .T. ) ;
#20303 = VERTEX_POINT ( 'NONE', #21911 ) ;
#20304 = CARTESIAN_POINT ( 'NONE',  ( -9.999999999999998224, 0.000000000000000000, -99.99999999999998579 ) ) ;
#20305 = DIRECTION ( 'NONE',  ( -0.000000000000000000, -0.000000000000000000, 1.000000000000000000 ) ) ;
#20306 = CARTESIAN_POINT ( 'NONE',  ( 10.81189881249999729, 0.000000000000000000, -166.3437500020484094 ) ) ;
#20307 = CARTESIAN_POINT ( 'NONE',  ( -5.405949406250003975, -9.363379034771801557, -198.5312500020484094 ) ) ;
#20308 = CARTESIAN_POINT ( 'NONE',  ( 5.405949406249992428, -9.363379034771808662, -27.09375000204835970 ) ) ;
#20309 = LINE ( 'NONE', #27217, #6074 ) ;
#20310 = CARTESIAN_POINT ( 'NONE',  ( -10.81189881249999729, 6.242252689847871849, -156.7187500020483810 ) ) ;
#20311 = CARTESIAN_POINT ( 'NONE',  ( -5.405949406250003975, -9.363379034771801557, -138.3437500020484094 ) ) ;
#20312 = CARTESIAN_POINT ( 'NONE',  ( -9.999999999999479527, -5.773502691896549521, -88.50000000409676204 ) ) ;
#20313 = CARTESIAN_POINT ( 'NONE',  ( -10.81189881249999729, 1.324075727343319199E-15, -120.5937500020483952 ) ) ;
#20314 = CARTESIAN_POINT ( 'NONE',  ( 10.81189881249999729, 0.000000000000000000, 0.1562499979516351889 ) ) ;
#20315 = CARTESIAN_POINT ( 'NONE',  ( 10.81189881249999551, -6.242252689847874514, -126.1562500020483810 ) ) ;
#20316 = CARTESIAN_POINT ( 'NONE',  ( 10.81189881249999907, 6.242252689847868297, -13.21875000204836148 ) ) ;
#20317 = CARTESIAN_POINT ( 'NONE',  ( -10.81189881249999729, 1.324075727343319199E-15, -141.5937500020483810 ) ) ;
#20318 = LINE ( 'NONE', #20748, #20558 ) ;
#20319 = CARTESIAN_POINT ( 'NONE',  ( -4.999999999999996447, 8.660254037844387298, -124.8750000040967763 ) ) ;
#20320 = CARTESIAN_POINT ( 'NONE',  ( 9.999999999999996447, -5.773502691896262640, -153.6250000000000284 ) ) ;
#20321 = CARTESIAN_POINT ( 'NONE',  ( 5.000000000000000000, 8.660254037844385522, -19.74999999999996092 ) ) ;
#20322 = CARTESIAN_POINT ( 'NONE',  ( -10.81189881249999729, -6.242252689847864744, -87.46875000204836681 ) ) ;
#20323 = CARTESIAN_POINT ( 'NONE',  ( 5.405949406249992428, -9.363379034771808662, -66.09375000204836681 ) ) ;
#20324 = CARTESIAN_POINT ( 'NONE',  ( 10.81189881249999907, 6.242252689847868297, -40.40625000204836681 ) ) ;
#20325 = CARTESIAN_POINT ( 'NONE',  ( 10.81189881249999907, 6.242252689847868297, -50.71875000204837391 ) ) ;
#20326 = CARTESIAN_POINT ( 'NONE',  ( -9.999999999999998224, 1.224646799147353059E-15, -185.7500000000000000 ) ) ;
#20327 = CARTESIAN_POINT ( 'NONE',  ( 7.644554776091147741E-16, 12.48450537969573659, -153.9687500020484094 ) ) ;
#20328 = CARTESIAN_POINT ( 'NONE',  ( 9.999999999999998224, 0.000000000000000000, -132.5000000000000000 ) ) ;
#20329 = CARTESIAN_POINT ( 'NONE',  ( -5.405949406250003975, -9.363379034771801557, -140.0312500020484094 ) ) ;
#20330 = CARTESIAN_POINT ( 'NONE',  ( 10.28326034709391834, 3.150834530142504697, -180.0000000000000853 ) ) ;
#20331 = AXIS2_PLACEMENT_3D ( 'NONE', #26981, #39716, #9730 ) ;
#20332 = CARTESIAN_POINT ( 'NONE',  ( -9.999999999999998224, 1.224646799147353059E-15, -82.24999999999998579 ) ) ;
#20333 = CARTESIAN_POINT ( 'NONE',  ( -5.405949406250003975, -9.363379034771801557, -20.03125000204836326 ) ) ;
#20334 =( BOUNDED_CURVE ( )  B_SPLINE_CURVE ( 2, ( #6767, #36757, #3115, #9791, #22970, #13429, #36126 ),
 .UNSPECIFIED., .F., .F. ) 
 B_SPLINE_CURVE_WITH_KNOTS ( ( 3, 2, 2, 3 ),
 ( 0.1268656716417910224, 0.1281094527363183799, 0.1293532338308457652, 0.1305970149253731227 ),
 .UNSPECIFIED. ) 
 CURVE ( )  GEOMETRIC_REPRESENTATION_ITEM ( )  RATIONAL_B_SPLINE_CURVE ( ( 1.000000000000003109, 0.8660254037844358210, 1.000000000000000000, 0.8660254037844387076, 1.000000000000000000, 0.8660254037844387076, 1.000000000000000000 ) ) 
 REPRESENTATION_ITEM ( '' )  );
#20335 = ORIENTED_EDGE ( 'NONE', *, *, #38191, .F. ) ;
#20336 = CARTESIAN_POINT ( 'NONE',  ( 10.81189881249999551, -6.242252689847874514, -106.6562500020484094 ) ) ;
#20337 = CARTESIAN_POINT ( 'NONE',  ( -4.999999999999996447, 8.660254037844387298, -135.3750000040967905 ) ) ;
#20338 = CARTESIAN_POINT ( 'NONE',  ( 10.00000000000031619, -5.773502691896077010, -185.1250000000000000 ) ) ;
#20339 = CARTESIAN_POINT ( 'NONE',  ( 5.000000000000000000, 8.660254037844385522, -45.62500000409677625 ) ) ;
#20340 = CARTESIAN_POINT ( 'NONE',  ( 9.999999999999612754, 5.773502691896477579, -155.2500000040967905 ) ) ;
#20341 = CARTESIAN_POINT ( 'NONE',  ( -5.405949406250003975, -9.363379034771801557, -54.53125000204836681 ) ) ;
#20342 = AXIS2_PLACEMENT_3D ( 'NONE', #22472, #23112, #29373 ) ;
#20343 = CARTESIAN_POINT ( 'NONE',  ( -9.999999999999998224, 1.224646799147353059E-15, -40.62500000409677625 ) ) ;
#20344 = CARTESIAN_POINT ( 'NONE',  ( -10.81189881249999907, -6.242252689847864744, -150.6562500020484094 ) ) ;
#20345 = CARTESIAN_POINT ( 'NONE',  ( 5.405949406249992428, -9.363379034771808662, -133.5937500020483810 ) ) ;
#20347 = EDGE_CURVE ( 'NONE', #10534, #24567, #38742, .T. ) ;
#20346 = CARTESIAN_POINT ( 'NONE',  ( 0.000000000000000000, 0.000000000000000000, -200.0000000000000000 ) ) ;
#20348 = ORIENTED_EDGE ( 'NONE', *, *, #7198, .T. ) ;
#20349 = EDGE_CURVE ( 'NONE', #8431, #18936, #17435, .T. ) ;
#20350 = CARTESIAN_POINT ( 'NONE',  ( -2.121150477449813534E-15, -11.54700538379251284, -78.87500000000000000 ) ) ;
#20352 = ORIENTED_EDGE ( 'NONE', *, *, #901, .T. ) ;
#20351 = CARTESIAN_POINT ( 'NONE',  ( 7.644554776091147741E-16, 12.48450537969573659, -65.65625000204838102 ) ) ;
#20353 = PERSON_AND_ORGANIZATION_ROLE ( 'creator' ) ;
#20355 = ORIENTED_EDGE ( 'NONE', *, *, #23820, .T. ) ;
#20354 = CARTESIAN_POINT ( 'NONE',  ( 10.81189881249999729, 0.000000000000000000, -116.8437500020483810 ) ) ;
#20356 = CARTESIAN_POINT ( 'NONE',  ( -5.405949406250003975, -9.363379034771801557, -19.84375000204835615 ) ) ;
#20357 = CARTESIAN_POINT ( 'NONE',  ( -5.405949406249996869, 9.363379034771805109, -188.3437500020483810 ) ) ;
#20358 = CARTESIAN_POINT ( 'NONE',  ( -5.405949406249996869, 9.363379034771805109, -48.84375000204838102 ) ) ;
#20359 = CARTESIAN_POINT ( 'NONE',  ( -9.999999999999998224, 1.224646799147353059E-15, -151.6250000040967905 ) ) ;
#20360 = CARTESIAN_POINT ( 'NONE',  ( 10.81189881249999551, -6.242252689847874514, -182.9687500020484094 ) ) ;
#20361 = VECTOR ( 'NONE', #41041, 1000.000000000000000 ) ;
#20362 = CARTESIAN_POINT ( 'NONE',  ( 10.81189881249999551, -6.242252689847874514, -160.4687500020484094 ) ) ;
#20363 = CARTESIAN_POINT ( 'NONE',  ( -5.405949406249996869, 9.363379034771805109, -150.8437500020483810 ) ) ;
#20364 = CARTESIAN_POINT ( 'NONE',  ( 5.405949406249999534, 9.363379034771803333, -160.0937500020484094 ) ) ;
#20365 = DIRECTION ( 'NONE',  ( -0.000000000000000000, -0.000000000000000000, 1.000000000000000000 ) ) ;
#20366 = CARTESIAN_POINT ( 'NONE',  ( -4.999999999999996447, 8.660254037844387298, -35.99999999999997868 ) ) ;
#20367 = CARTESIAN_POINT ( 'NONE',  ( 9.999999999999996447, -5.773502691896262640, -180.6250000000000284 ) ) ;
#20368 = CARTESIAN_POINT ( 'NONE',  ( -2.293366432827344421E-15, -12.48450537969573659, -96.21875000204839523 ) ) ;
#20369 = CARTESIAN_POINT ( 'NONE',  ( 9.999999999999479527, 5.773502691896553074, -151.8749999999999716 ) ) ;
#20370 = CARTESIAN_POINT ( 'NONE',  ( 5.405949406249999534, 9.363379034771803333, -67.28125000204838102 ) ) ;
#20371 = CARTESIAN_POINT ( 'NONE',  ( -1.040834085586084257E-14, -125.0000000000000000, 22.49999999999999289 ) ) ;
#20372 = CARTESIAN_POINT ( 'NONE',  ( 10.81189881249999729, 0.000000000000000000, -187.3437500020483810 ) ) ;
#20373 = CARTESIAN_POINT ( 'NONE',  ( 10.81189881249999551, -6.242252689847874514, -118.6562500020483952 ) ) ;
#20374 = CARTESIAN_POINT ( 'NONE',  ( -5.405949406249996869, 9.363379034771805109, -158.5312500020484094 ) ) ;
#20375 = CARTESIAN_POINT ( 'NONE',  ( -10.81189881249999729, 6.242252689847871849, -48.90625000204836681 ) ) ;
#20376 = CARTESIAN_POINT ( 'NONE',  ( 9.999999999999998224, 0.000000000000000000, -141.8750000040967905 ) ) ;
#20377 = CARTESIAN_POINT ( 'NONE',  ( -4.999999999999996447, 8.660254037844387298, -109.4999999999999858 ) ) ;
#20378 = ORIENTED_EDGE ( 'NONE', *, *, #20138, .T. ) ;
#20379 = CARTESIAN_POINT ( 'NONE',  ( 5.405949406249992428, -9.363379034771808662, -130.7812500020483810 ) ) ;
#20380 = CARTESIAN_POINT ( 'NONE',  ( -2.293366432827344421E-15, -12.48450537969573659, -150.4062500020483810 ) ) ;
#20381 = CARTESIAN_POINT ( 'NONE',  ( -10.81189881249999729, 1.324075727343319199E-15, -191.2812500020484094 ) ) ;
#20382 = CARTESIAN_POINT ( 'NONE',  ( 10.81189881249999729, 0.000000000000000000, -82.34375000204836681 ) ) ;
#20383 = ORIENTED_EDGE ( 'NONE', *, *, #13519, .T. ) ;
#20384 = CARTESIAN_POINT ( 'NONE',  ( 10.00000000000000000, 5.773502691896255534, -49.87499999999997868 ) ) ;
#20385 = CARTESIAN_POINT ( 'NONE',  ( -2.293366432827344421E-15, -12.48450537969573659, -183.2187500020484094 ) ) ;
#20386 = CARTESIAN_POINT ( 'NONE',  ( 10.00000000000000000, 5.773502691896255534, -68.25000000409679046 ) ) ;
#20387 = CARTESIAN_POINT ( 'NONE',  ( 10.00000000000051159, -5.773502691895965988, -179.1250000000000000 ) ) ;
#20388 = DIRECTION ( 'NONE',  ( 0.000000000000000000, 0.000000000000000000, -1.000000000000000000 ) ) ;
#20389 = CARTESIAN_POINT ( 'NONE',  ( 10.81189881249999551, -6.242252689847874514, -75.15625000204838102 ) ) ;
#20390 = AXIS2_PLACEMENT_3D ( 'NONE', #1020, #14140, #10498 ) ;
#20391 = CARTESIAN_POINT ( 'NONE',  ( -2.293366432827344421E-15, -12.48450537969573659, -58.90625000204838813 ) ) ;
#20392 = CARTESIAN_POINT ( 'NONE',  ( 9.999999999999996447, -5.773502691896262640, -53.50000000409677625 ) ) ;
#20393 = CARTESIAN_POINT ( 'NONE',  ( 10.81189881249999729, 0.000000000000000000, -7.343750002048343717 ) ) ;
#20394 = CARTESIAN_POINT ( 'NONE',  ( -9.999999999998969713, -5.773502691896847949, -35.62499999999994316 ) ) ;
#20395 = CARTESIAN_POINT ( 'NONE',  ( -10.81189881249999729, 1.324075727343319199E-15, -182.2812500020483810 ) ) ;
#20396 = CARTESIAN_POINT ( 'NONE',  ( 5.405949406249992428, -9.363379034771808662, -3.281250002048374803 ) ) ;
#20397 = CARTESIAN_POINT ( 'NONE',  ( -5.000000000000003553, -8.660254037844383745, -87.99999999999998579 ) ) ;
#20399 = EDGE_CURVE ( 'NONE', #33370, #24961, #21872, .T. ) ;
#20398 = CARTESIAN_POINT ( 'NONE',  ( -9.999999999999998224, 1.224646799147353059E-15, -164.7500000000000000 ) ) ;
#20400 = AXIS2_PLACEMENT_3D ( 'NONE', #42079, #15532, #9080 ) ;
#20401 = CYLINDRICAL_SURFACE ( 'NONE', #31159, 9.999999999999998224 ) ;
#20402 = CARTESIAN_POINT ( 'NONE',  ( -9.999999999999998224, 1.224646799147353059E-15, -105.1250000040967763 ) ) ;
#20403 = ADVANCED_FACE ( 'NONE', ( #31645 ), #35518, .T. ) ;
#20404 = CARTESIAN_POINT ( 'NONE',  ( -1.040834085586084257E-14, 145.0000000000000000, 22.49999999999999289 ) ) ;
#20405 = EDGE_CURVE ( 'NONE', #25211, #35035, #31220, .T. ) ;
#20407 = ORIENTED_EDGE ( 'NONE', *, *, #32820, .F. ) ;
#20406 = CARTESIAN_POINT ( 'NONE',  ( 5.405949406249999534, 9.363379034771803333, -89.78125000204838102 ) ) ;
#20408 = LINE ( 'NONE', #26473, #41364 ) ;
#20410 = ORIENTED_EDGE ( 'NONE', *, *, #26988, .T. ) ;
#20409 = CARTESIAN_POINT ( 'NONE',  ( 9.999999999999998224, 0.000000000000000000, -153.5000000000000000 ) ) ;
#20411 = CC_DESIGN_PERSON_AND_ORGANIZATION_ASSIGNMENT ( #16147, #25694, ( #24948 ) ) ;
#20412 = VERTEX_POINT ( 'NONE', #27973 ) ;
#20413 = CARTESIAN_POINT ( 'NONE',  ( -10.81189881249999907, -6.242252689847864744, -25.96875000204837391 ) ) ;
#20414 = CARTESIAN_POINT ( 'NONE',  ( -5.405949406249996869, 9.363379034771805109, -22.03125000204836326 ) ) ;
#20415 = DATE_AND_TIME ( #26273, #13544 ) ;
#20416 = CARTESIAN_POINT ( 'NONE',  ( 5.405949406249992428, -9.363379034771808662, -70.59375000204836681 ) ) ;
#20417 = CARTESIAN_POINT ( 'NONE',  ( -9.999999999999998224, 1.224646799147353059E-15, -62.74999999999997158 ) ) ;
#20418 = CARTESIAN_POINT ( 'NONE',  ( 7.070501591499377789E-16, 11.54700538379251284, -48.12499999999997158 ) ) ;
#20419 = EDGE_CURVE ( 'NONE', #37668, #27111, #41100, .T. ) ;
#20420 = CARTESIAN_POINT ( 'NONE',  ( -2.293366432827344421E-15, -12.48450537969573659, -187.7187500020484094 ) ) ;
#20421 = CARTESIAN_POINT ( 'NONE',  ( -5.405949406249996869, 9.363379034771805109, -149.3437500020483810 ) ) ;
#20422 =( BOUNDED_CURVE ( )  B_SPLINE_CURVE ( 2, ( #26330, #9914, #20265, #9704, #26115, #36459, #6681 ),
 .UNSPECIFIED., .F., .F. ) 
 B_SPLINE_CURVE_WITH_KNOTS ( ( 3, 2, 2, 3 ),
 ( 0.9850746268656718208, 0.9863184079601992060, 0.9875621890547265913, 0.9888059701492539766 ),
 .UNSPECIFIED. ) 
 CURVE ( )  GEOMETRIC_REPRESENTATION_ITEM ( )  RATIONAL_B_SPLINE_CURVE ( ( 0.9999999999999761302, 0.8660254037844625774, 1.000000000000000000, 0.8660254037844387076, 1.000000000000000000, 0.8660254037844148378, 1.000000000000023981 ) ) 
 REPRESENTATION_ITEM ( '' )  );
#20423 = VECTOR ( 'NONE', #14582, 1000.000000000000000 ) ;
#20424 = EDGE_CURVE ( 'NONE', #30625, #1760, #35128, .T. ) ;
#20425 = DIRECTION ( 'NONE',  ( -0.000000000000000000, -0.000000000000000000, -1.000000000000000000 ) ) ;
#20426 = DIRECTION ( 'NONE',  ( 1.000000000000000000, 0.000000000000000000, 0.000000000000000000 ) ) ;
#20427 = CARTESIAN_POINT ( 'NONE',  ( 5.000000000000000000, 8.660254037844385522, -2.125000004096766482 ) ) ;
#20428 = CARTESIAN_POINT ( 'NONE',  ( 9.999999999999998224, 0.000000000000000000, -140.3750000040967905 ) ) ;
#20429 = CARTESIAN_POINT ( 'NONE',  ( 10.81189881249999729, 0.000000000000000000, -121.3437500020483952 ) ) ;
#20430 = CARTESIAN_POINT ( 'NONE',  ( 9.999999999999872102, 5.773502691896329253, -161.2500000040967905 ) ) ;
#20431 = CARTESIAN_POINT ( 'NONE',  ( 10.81189881249999551, -6.242252689847874514, -91.65625000204838102 ) ) ;
#20432 = CARTESIAN_POINT ( 'NONE',  ( -10.81189881249999729, -6.242252689847864744, -103.9687500020483810 ) ) ;
#20433 = CARTESIAN_POINT ( 'NONE',  ( -10.81189881249999729, 1.324075727343319199E-15, -72.59375000204838102 ) ) ;
#20434 = CARTESIAN_POINT ( 'NONE',  ( -10.81189881249999729, 6.242252689847871849, -72.90625000204838102 ) ) ;
#20435 = CARTESIAN_POINT ( 'NONE',  ( -9.999999999999998224, 5.773502691896259087, -159.2500000040967905 ) ) ;
#20436 = CARTESIAN_POINT ( 'NONE',  ( 10.81189881249999551, -6.242252689847874514, -157.6562500020484094 ) ) ;
#20437 = CARTESIAN_POINT ( 'NONE',  ( 10.81189881249999907, 6.242252689847868297, -169.4062500020484094 ) ) ;
#20438 = FACE_OUTER_BOUND ( 'NONE', #35603, .T. ) ;
#20439 = FACE_OUTER_BOUND ( 'NONE', #1973, .T. ) ;
#20440 = CARTESIAN_POINT ( 'NONE',  ( -10.81189881249999729, 6.242252689847871849, -108.7187500020483810 ) ) ;
#20441 = DIRECTION ( 'NONE',  ( 0.000000000000000000, 1.000000000000000000, 0.000000000000000000 ) ) ;
#20442 = CARTESIAN_POINT ( 'NONE',  ( -2.121150477449813534E-15, -11.54700538379251284, -83.37499999999997158 ) ) ;
#20443 = CARTESIAN_POINT ( 'NONE',  ( 5.405949406249992428, -9.363379034771808662, -6.281250002048377468 ) ) ;
#20444 = CARTESIAN_POINT ( 'NONE',  ( 10.00000000000000000, 5.773502691896255534, -92.25000000409679046 ) ) ;
#20445 = CARTESIAN_POINT ( 'NONE',  ( -2.293366432827344421E-15, -12.48450537969573659, -102.4062500020483952 ) ) ;
#20446 = CARTESIAN_POINT ( 'NONE',  ( 5.405949406249999534, 9.363379034771803333, -83.78125000204838102 ) ) ;
#20447 = CARTESIAN_POINT ( 'NONE',  ( -9.999999999999998224, 1.224646799147353059E-15, -75.12500000409677625 ) ) ;
#20448 = DIRECTION ( 'NONE',  ( 1.000000000000000000, 0.000000000000000000, 0.000000000000000000 ) ) ;
#20449 = CARTESIAN_POINT ( 'NONE',  ( 10.81189881249999551, -6.242252689847874514, -34.46875000204835260 ) ) ;
#20450 = ORIENTED_EDGE ( 'NONE', *, *, #35036, .T. ) ;
#20451 = CARTESIAN_POINT ( 'NONE',  ( 4.999999999999992006, -8.660254037844389075, -8.249999999999952038 ) ) ;
#20452 = CARTESIAN_POINT ( 'NONE',  ( -10.81189881249999729, 1.324075727343319199E-15, -26.28125000204836681 ) ) ;
#20453 = CARTESIAN_POINT ( 'NONE',  ( 10.00000000000000000, 5.773502691896255534, -147.3750000000000000 ) ) ;
#20454 = CARTESIAN_POINT ( 'NONE',  ( 7.070501591499376803E-16, 11.54700538379251284, -45.50000000409676915 ) ) ;
#20455 = CARTESIAN_POINT ( 'NONE',  ( -4.999999999999996447, 8.660254037844387298, -6.375000004096770034 ) ) ;
#20456 = CARTESIAN_POINT ( 'NONE',  ( 7.644554776091147741E-16, 12.48450537969573659, -136.1562500020483810 ) ) ;
#20457 = CARTESIAN_POINT ( 'NONE',  ( -9.999999999999998224, 1.224646799147353059E-15, -191.7500000000000000 ) ) ;
#20458 = CARTESIAN_POINT ( 'NONE',  ( -9.999999999999998224, 1.224646799147353059E-15, -122.7500000000000000 ) ) ;
#20460 = VERTEX_POINT ( 'NONE', #36711 ) ;
#20459 = CARTESIAN_POINT ( 'NONE',  ( -10.81189881249999907, -6.242252689847864744, -114.6562500020483952 ) ) ;
#20461 = CARTESIAN_POINT ( 'NONE',  ( 7.070501591499376803E-16, 11.54700538379251284, -36.50000000409675494 ) ) ;
#20462 = ORIENTED_EDGE ( 'NONE', *, *, #20424, .T. ) ;
#20463 = ORIENTED_EDGE ( 'NONE', *, *, #15202, .T. ) ;
#20464 =( BOUNDED_CURVE ( )  B_SPLINE_CURVE ( 2, ( #41686, #9317, #42111, #12545, #12125, #25737, #22486 ),
 .UNSPECIFIED., .F., .F. ) 
 B_SPLINE_CURVE_WITH_KNOTS ( ( 3, 2, 2, 3 ),
 ( 0.2873134328358210032, 0.2885572139303483885, 0.2898009950248757183, 0.2910447761194031036 ),
 .UNSPECIFIED. ) 
 CURVE ( )  GEOMETRIC_REPRESENTATION_ITEM ( )  RATIONAL_B_SPLINE_CURVE ( ( 0.9999999999999880096, 0.8660254037844506980, 1.000000000000000000, 0.8660254037844387076, 1.000000000000000000, 0.8660254037844267172, 1.000000000000011990 ) ) 
 REPRESENTATION_ITEM ( '' )  );
#20465 = CARTESIAN_POINT ( 'NONE',  ( -2.293366432827344421E-15, -12.48450537969573659, -42.40625000204837391 ) ) ;
#20466 = PERSON_AND_ORGANIZATION_ROLE ( 'classification_officer' ) ;
#20467 = EDGE_CURVE ( 'NONE', #21146, #40566, #38983, .T. ) ;
#20468 = CARTESIAN_POINT ( 'NONE',  ( -5.405949406249996869, 9.363379034771805109, -98.34375000204838102 ) ) ;
#20469 = CARTESIAN_POINT ( 'NONE',  ( 10.81189881249999729, 0.000000000000000000, -127.5312500020483952 ) ) ;
#20470 = ORIENTED_EDGE ( 'NONE', *, *, #30448, .F. ) ;
#20471 = CARTESIAN_POINT ( 'NONE',  ( 10.00000000000102318, -5.773502691895667560, -85.00000000409674783 ) ) ;
#20472 = CARTESIAN_POINT ( 'NONE',  ( -10.81189881249999729, 6.242252689847871849, -194.2187500020484379 ) ) ;
#20473 =( BOUNDED_CURVE ( )  B_SPLINE_CURVE ( 2, ( #39875, #206, #33216, #10308, #23496, #13740, #26930 ),
 .UNSPECIFIED., .F., .F. ) 
 B_SPLINE_CURVE_WITH_KNOTS ( ( 3, 2, 2, 3 ),
 ( 0.3208955223880597396, 0.3221393034825871804, 0.3233830845771145657, 0.3246268656716419510 ),
 .UNSPECIFIED. ) 
 CURVE ( )  GEOMETRIC_REPRESENTATION_ITEM ( )  RATIONAL_B_SPLINE_CURVE ( ( 0.9999999999999940048, 0.8660254037844447028, 1.000000000000000000, 0.8660254037844387076, 1.000000000000000000, 0.8660254037844207220, 1.000000000000017986 ) ) 
 REPRESENTATION_ITEM ( '' )  );
#20474 = CARTESIAN_POINT ( 'NONE',  ( -10.81189881249999729, 1.324075727343319199E-15, -171.7812500020484094 ) ) ;
#20475 = CARTESIAN_POINT ( 'NONE',  ( 9.999999999999998224, 0.000000000000000000, -54.87500000409675494 ) ) ;
#20476 = CARTESIAN_POINT ( 'NONE',  ( 10.81189881249999551, -6.242252689847874514, -122.9687500020483952 ) ) ;
#20477 = CARTESIAN_POINT ( 'NONE',  ( -10.81189881249999729, 6.242252689847871849, -96.71875000204838102 ) ) ;
#20478 = DIRECTION ( 'NONE',  ( -0.000000000000000000, -0.000000000000000000, 1.000000000000000000 ) ) ;
#20479 = CARTESIAN_POINT ( 'NONE',  ( -5.405949406249996869, 9.363379034771805109, -101.5312500020483952 ) ) ;
#20480 = CARTESIAN_POINT ( 'NONE',  ( -10.00000000000000000, -5.773502691896251982, -186.0000000040967905 ) ) ;
#20481 = CARTESIAN_POINT ( 'NONE',  ( -5.405949406250003975, -9.363379034771801557, -108.3437500020483810 ) ) ;
#20482 = CARTESIAN_POINT ( 'NONE',  ( 7.644554776091147741E-16, 12.48450537969573659, -179.6562500020484094 ) ) ;
#20483 = LINE ( 'NONE', #20056, #33048 ) ;
#20484 = CARTESIAN_POINT ( 'NONE',  ( 10.00000000000000000, 5.773502691896255534, -132.7500000040967905 ) ) ;
#20485 = CARTESIAN_POINT ( 'NONE',  ( -10.81189881249999729, 1.324075727343319199E-15, -198.7812500020484094 ) ) ;
#20486 = CARTESIAN_POINT ( 'NONE',  ( 10.81189881249999729, 6.242252689847867408, -59.71875000204836681 ) ) ;
#20487 = CARTESIAN_POINT ( 'NONE',  ( -2.293366432827344421E-15, -12.48450537969573659, -39.21875000204835970 ) ) ;
#20488 = CARTESIAN_POINT ( 'NONE',  ( 5.000000000000000000, 8.660254037844385522, -173.1250000040968189 ) ) ;
#20489 = CARTESIAN_POINT ( 'NONE',  ( -2.293366432827344421E-15, -12.48450537969573659, -7.906250002048370362 ) ) ;
#20490 = CARTESIAN_POINT ( 'NONE',  ( 5.405949406249999534, 9.363379034771803333, -25.09375000204835970 ) ) ;
#20491 = CARTESIAN_POINT ( 'NONE',  ( 9.999999999999998224, 0.000000000000000000, -123.8750000040967905 ) ) ;
#20492 = CARTESIAN_POINT ( 'NONE',  ( 10.81189881249999729, 0.000000000000000000, -133.3437500020484094 ) ) ;
#20493 = CARTESIAN_POINT ( 'NONE',  ( -4.999999999999996447, 8.660254037844387298, -106.4999999999999858 ) ) ;
#20494 = CARTESIAN_POINT ( 'NONE',  ( -5.405949406249996869, 9.363379034771805109, -29.53125000204837036 ) ) ;
#20495 = CARTESIAN_POINT ( 'NONE',  ( 9.999999999999998224, 0.000000000000000000, -200.0000000000000000 ) ) ;
#20496 = CARTESIAN_POINT ( 'NONE',  ( 9.999999999999996447, -5.773502691896262640, -57.62499999999998579 ) ) ;
#20497 = CARTESIAN_POINT ( 'NONE',  ( 10.81189881249999729, 0.000000000000000000, -127.5312500020483952 ) ) ;
#20498 = CARTESIAN_POINT ( 'NONE',  ( -10.81189881249999729, -6.242252689847864744, -107.1562500020483952 ) ) ;
#20499 = ORIENTED_EDGE ( 'NONE', *, *, #17109, .F. ) ;
#20500 = CARTESIAN_POINT ( 'NONE',  ( -9.999999999999998224, 1.224646799147353059E-15, -153.1250000040967905 ) ) ;
#20501 = CARTESIAN_POINT ( 'NONE',  ( -9.999999999999998224, 5.773502691896259087, -102.2500000040967763 ) ) ;
#20502 = CARTESIAN_POINT ( 'NONE',  ( 7.070501591499376803E-16, 11.54700538379251284, -101.0000000040967905 ) ) ;
#20503 = CARTESIAN_POINT ( 'NONE',  ( -10.81189881249999729, 1.324075727343319199E-15, -54.59375000204835970 ) ) ;
#20504 = ORIENTED_EDGE ( 'NONE', *, *, #26372, .F. ) ;
#20505 = CARTESIAN_POINT ( 'NONE',  ( 10.00000000000000000, 5.773502691896255534, -34.87499999999995026 ) ) ;
#20506 = VECTOR ( 'NONE', #17225, 1000.000000000000000 ) ;
#20507 = CARTESIAN_POINT ( 'NONE',  ( -10.81189881249999729, 6.242252689847871849, -36.90625000204835970 ) ) ;
#20508 = DIRECTION ( 'NONE',  ( -0.000000000000000000, -0.000000000000000000, -1.000000000000000000 ) ) ;
#20509 = CARTESIAN_POINT ( 'NONE',  ( -9.999999999999998224, 5.773502691896259087, -39.25000000409676204 ) ) ;
#20510 = CARTESIAN_POINT ( 'NONE',  ( 7.070501591499376803E-16, 11.54700538379251284, -152.0000000040967905 ) ) ;
#20511 = CARTESIAN_POINT ( 'NONE',  ( -5.405949406249996869, 9.363379034771805109, -139.0312500020484094 ) ) ;
#20512 = DIRECTION ( 'NONE',  ( -0.000000000000000000, -0.000000000000000000, -1.000000000000000000 ) ) ;
#20513 = ORIENTED_EDGE ( 'NONE', *, *, #41905, .F. ) ;
#20514 = ORIENTED_EDGE ( 'NONE', *, *, #5893, .T. ) ;
#20515 = CARTESIAN_POINT ( 'NONE',  ( -9.999999999999227285, -5.773502691896698735, -106.5000000040967336 ) ) ;
#20516 = CARTESIAN_POINT ( 'NONE',  ( -9.999999999999998224, 1.224646799147353059E-15, -4.625000004096769146 ) ) ;
#20517 = CARTESIAN_POINT ( 'NONE',  ( 5.405949406249992428, -9.363379034771808662, -169.5937500020484094 ) ) ;
#20518 = CARTESIAN_POINT ( 'NONE',  ( 5.405949406249999534, 9.363379034771803333, -196.2812500020484094 ) ) ;
#20519 = CARTESIAN_POINT ( 'NONE',  ( 5.405949406249999534, 9.363379034771803333, -14.59375000204835082 ) ) ;
#20520 = VECTOR ( 'NONE', #6633, 1000.000000000000000 ) ;
#20521 = CARTESIAN_POINT ( 'NONE',  ( 10.81189881249999729, 0.000000000000000000, -155.8437500020483810 ) ) ;
#20522 = CARTESIAN_POINT ( 'NONE',  ( -5.405949406250003975, -9.363379034771801557, -135.3437500020484094 ) ) ;
#20523 = CARTESIAN_POINT ( 'NONE',  ( -10.81189881249999729, 1.324075727343319199E-15, -102.7812500020483952 ) ) ;
#20524 = CARTESIAN_POINT ( 'NONE',  ( 5.405949406249999534, 9.363379034771803333, -118.0937500020483810 ) ) ;
#20525 = CARTESIAN_POINT ( 'NONE',  ( 5.000000000000000000, 8.660254037844385522, -194.1250000040967905 ) ) ;
#20526 = CARTESIAN_POINT ( 'NONE',  ( -5.405949406249996869, 9.363379034771805109, -128.5312500020484094 ) ) ;
#20527 = CARTESIAN_POINT ( 'NONE',  ( -10.81189881249999907, -6.242252689847864744, -9.468750002048359704 ) ) ;
#20529 = EDGE_CURVE ( 'NONE', #22548, #14748, #25794, .T. ) ;
#20528 = CARTESIAN_POINT ( 'NONE',  ( -5.405949406249996869, 9.363379034771805109, -126.8437500020483952 ) ) ;
#20530 = DIRECTION ( 'NONE',  ( 1.000000000000000000, 0.000000000000000000, 0.000000000000000000 ) ) ;
#20531 = CARTESIAN_POINT ( 'NONE',  ( -5.000000000000003553, -8.660254037844383745, -96.99999999999998579 ) ) ;
#20532 = CARTESIAN_POINT ( 'NONE',  ( 9.999999999999998224, 0.000000000000000000, -155.0000000000000000 ) ) ;
#20533 = CARTESIAN_POINT ( 'NONE',  ( 9.999999999999998224, 0.000000000000000000, -18.49999999999996092 ) ) ;
#20534 = CARTESIAN_POINT ( 'NONE',  ( -5.405949406250003975, -9.363379034771801557, -81.34375000204838102 ) ) ;
#20535 = CARTESIAN_POINT ( 'NONE',  ( 5.405949406249992428, -9.363379034771808662, -64.59375000204836681 ) ) ;
#20536 = CARTESIAN_POINT ( 'NONE',  ( 9.999999999999998224, 0.000000000000000000, -170.0000000000000000 ) ) ;
#20537 = CARTESIAN_POINT ( 'NONE',  ( 7.644554776091147741E-16, 12.48450537969573659, -44.65625000204836681 ) ) ;
#20538 = CARTESIAN_POINT ( 'NONE',  ( -10.81189881249999729, 6.242252689847871849, -44.21875000204836681 ) ) ;
#20539 = CARTESIAN_POINT ( 'NONE',  ( -7.959047257566134870E-15, 139.9999999999999716, 42.49999999999999289 ) ) ;
#20540 = CARTESIAN_POINT ( 'NONE',  ( -2.293366432827344421E-15, -12.48450537969573659, -150.2187500020483810 ) ) ;
#20541 = CARTESIAN_POINT ( 'NONE',  ( 4.999999999999992006, -8.660254037844389075, -132.7499999999999716 ) ) ;
#20542 = CARTESIAN_POINT ( 'NONE',  ( 5.405949406249999534, 9.363379034771803333, -131.7812500020483810 ) ) ;
#20543 =( BOUNDED_CURVE ( )  B_SPLINE_CURVE ( 2, ( #22906, #19646, #6497, #33264, #25928, #39710, #35649 ),
 .UNSPECIFIED., .F., .F. ) 
 B_SPLINE_CURVE_WITH_KNOTS ( ( 3, 2, 2, 3 ),
 ( 0.4216417910447762818, 0.4228855721393036671, 0.4241293532338309413, 0.4253731343283583266 ),
 .UNSPECIFIED. ) 
 CURVE ( )  GEOMETRIC_REPRESENTATION_ITEM ( )  RATIONAL_B_SPLINE_CURVE ( ( 0.9999999999999820144, 0.8660254037844566932, 1.000000000000000000, 0.8660254037844387076, 1.000000000000000000, 0.8660254037844267172, 1.000000000000011990 ) ) 
 REPRESENTATION_ITEM ( '' )  );
#20544 = CARTESIAN_POINT ( 'NONE',  ( 0.6533489177094430334, 10.23204748536553588, -179.9999999999998863 ) ) ;
#20545 = CARTESIAN_POINT ( 'NONE',  ( -9.999999999999998224, 5.773502691896259087, -85.37499999999997158 ) ) ;
#20546 = CARTESIAN_POINT ( 'NONE',  ( 10.81189881249999729, 6.242252689847867408, -17.90625000204837036 ) ) ;
#20547 = ORIENTED_EDGE ( 'NONE', *, *, #30982, .F. ) ;
#20548 = CARTESIAN_POINT ( 'NONE',  ( -10.81189881249999729, -6.242252689847864744, -111.6562500020483952 ) ) ;
#20549 = CARTESIAN_POINT ( 'NONE',  ( 7.070501591499377789E-16, 11.54700538379251284, -128.0000000040967620 ) ) ;
#20550 = CARTESIAN_POINT ( 'NONE',  ( -2.121150477449813534E-15, -11.54700538379251284, -185.3750000000000000 ) ) ;
#20551 = CARTESIAN_POINT ( 'NONE',  ( 5.000000000000000000, 8.660254037844385522, -30.62500000409676559 ) ) ;
#20552 = DIRECTION ( 'NONE',  ( -0.000000000000000000, -0.000000000000000000, 1.000000000000000000 ) ) ;
#20553 = CARTESIAN_POINT ( 'NONE',  ( -5.405949406249996869, 9.363379034771805109, -55.03125000204836681 ) ) ;
#20554 = CARTESIAN_POINT ( 'NONE',  ( -10.00000000000102496, 5.773502691895664007, -76.37499999999992895 ) ) ;
#20555 = CARTESIAN_POINT ( 'NONE',  ( 7.644554776091147741E-16, 12.48450537969573659, -157.1562500020484094 ) ) ;
#20556 = CARTESIAN_POINT ( 'NONE',  ( 7.644554776091147741E-16, 12.48450537969573659, -134.4687500020483810 ) ) ;
#20557 = CARTESIAN_POINT ( 'NONE',  ( -10.00000000000076916, 5.773502691895813221, -103.7500000040967763 ) ) ;
#20558 = VECTOR ( 'NONE', #40372, 1000.000000000000000 ) ;
#20559 = ORIENTED_EDGE ( 'NONE', *, *, #40135, .T. ) ;
#20560 = CARTESIAN_POINT ( 'NONE',  ( 9.999999999999548805, 5.773502691896514882, -177.3749999999999716 ) ) ;
#20561 = ORIENTED_EDGE ( 'NONE', *, *, #18009, .F. ) ;
#20562 = ORIENTED_EDGE ( 'NONE', *, *, #5190, .T. ) ;
#20563 = PERSON_AND_ORGANIZATION_ROLE ( 'classification_officer' ) ;
#20565 = ORIENTED_EDGE ( 'NONE', *, *, #39253, .T. ) ;
#20564 = CARTESIAN_POINT ( 'NONE',  ( 10.81189881249999729, 0.000000000000000000, -113.8437500020483810 ) ) ;
#20566 = DIRECTION ( 'NONE',  ( -0.000000000000000000, -0.000000000000000000, 1.000000000000000000 ) ) ;
#20567 = CARTESIAN_POINT ( 'NONE',  ( 10.81189881249999729, 0.000000000000000000, -188.8437500020483810 ) ) ;
#20568 = CARTESIAN_POINT ( 'NONE',  ( -2.293366432827344421E-15, -12.48450537969573659, -36.21875000204835970 ) ) ;
#20569 = CARTESIAN_POINT ( 'NONE',  ( -4.888400856004290418, -8.992219867142372536, 2.111525036386560869E-16 ) ) ;
#20570 = CARTESIAN_POINT ( 'NONE',  ( 0.000000000000000000, 0.000000000000000000, -99.99999999999998579 ) ) ;
#20571 = CARTESIAN_POINT ( 'NONE',  ( 7.644554776091147741E-16, 12.48450537969573659, -177.9687500020484094 ) ) ;
#20572 = CARTESIAN_POINT ( 'NONE',  ( -10.81189881249999729, 6.242252689847871849, -159.7187500020483526 ) ) ;
#20573 = CARTESIAN_POINT ( 'NONE',  ( 10.81189881249999551, -6.242252689847874514, -140.9687500020483810 ) ) ;
#20574 =( BOUNDED_CURVE ( )  B_SPLINE_CURVE ( 2, ( #37452, #14980, #4225, #17366, #24514, #27530, #37667 ),
 .UNSPECIFIED., .F., .F. ) 
 B_SPLINE_CURVE_WITH_KNOTS ( ( 3, 2, 2, 3 ),
 ( 0.5858208955223881409, 0.5870646766169155262, 0.5883084577114429115, 0.5895522388059702967 ),
 .UNSPECIFIED. ) 
 CURVE ( )  GEOMETRIC_REPRESENTATION_ITEM ( )  RATIONAL_B_SPLINE_CURVE ( ( 0.9999999999999880096, 0.8660254037844506980, 1.000000000000000000, 0.8660254037844387076, 1.000000000000000000, 0.8660254037844267172, 1.000000000000011990 ) ) 
 REPRESENTATION_ITEM ( '' )  );
#20575 = CARTESIAN_POINT ( 'NONE',  ( 5.405949406249999534, 9.363379034771803333, -158.5937500020483810 ) ) ;
#20576 = DIRECTION ( 'NONE',  ( 0.000000000000000000, 0.000000000000000000, 1.000000000000000000 ) ) ;
#20577 = CARTESIAN_POINT ( 'NONE',  ( 9.999999999999998224, 0.000000000000000000, -36.49999999999997868 ) ) ;
#20578 = CARTESIAN_POINT ( 'NONE',  ( -5.000000000000003553, -8.660254037844383745, -176.5000000000000000 ) ) ;
#20579 = CARTESIAN_POINT ( 'NONE',  ( -10.81189881249999729, 1.324075727343319199E-15, -90.59375000204838102 ) ) ;
#20580 = DIRECTION ( 'NONE',  ( 0.000000000000000000, 0.000000000000000000, -1.000000000000000000 ) ) ;
#20581 = CARTESIAN_POINT ( 'NONE',  ( 7.644554776091147741E-16, 12.48450537969573659, -64.15625000204838102 ) ) ;
#20582 = CARTESIAN_POINT ( 'NONE',  ( 10.00000000000025402, -5.773502691896113426, -124.0000000040967620 ) ) ;
#20583 = ADVANCED_FACE ( 'NONE', ( #42382 ), #38950, .T. ) ;
#20584 = CARTESIAN_POINT ( 'NONE',  ( -10.81189881249999729, 1.324075727343319199E-15, -180.5937500020484094 ) ) ;
#20585 = CARTESIAN_POINT ( 'NONE',  ( 5.405949406249999534, 9.363379034771803333, -122.7812500020483952 ) ) ;
#20586 = CIRCLE ( 'NONE', #41943, 20.00000000000000355 ) ;
#20587 = CARTESIAN_POINT ( 'NONE',  ( -10.81189881249999729, 6.242252689847871849, -152.4062500020483810 ) ) ;
#20588 = CARTESIAN_POINT ( 'NONE',  ( -10.81189881249999907, -6.242252689847864744, -53.15625000204837391 ) ) ;
#20589 = CARTESIAN_POINT ( 'NONE',  ( -4.999999999999996447, 8.660254037844387298, -126.3750000040967905 ) ) ;
#20590 = CARTESIAN_POINT ( 'NONE',  ( 4.999999999999992006, -8.660254037844389075, -108.7499999999999858 ) ) ;
#20591 = ORIENTED_EDGE ( 'NONE', *, *, #1854, .T. ) ;
#20592 = CARTESIAN_POINT ( 'NONE',  ( 5.405949406249999534, 9.363379034771803333, -131.7812500020483810 ) ) ;
#20593 = CARTESIAN_POINT ( 'NONE',  ( -9.999999999999998224, 5.773502691896259087, -157.7500000040967905 ) ) ;
#20594 = CARTESIAN_POINT ( 'NONE',  ( -10.81189881249999729, 6.242252689847871849, -150.9062500020484094 ) ) ;
#20595 = AXIS2_PLACEMENT_3D ( 'NONE', #27351, #40486, #7716 ) ;
#20596 = CARTESIAN_POINT ( 'NONE',  ( -10.81189881249999907, -6.242252689847864744, -191.1562500020484094 ) ) ;
#20597 = CARTESIAN_POINT ( 'NONE',  ( 5.405949406249992428, -9.363379034771808662, -81.09375000204838102 ) ) ;
#20598 = ORIENTED_EDGE ( 'NONE', *, *, #19755, .T. ) ;
#20599 = CARTESIAN_POINT ( 'NONE',  ( 10.00000000000000000, 5.773502691896255534, -48.37499999999997158 ) ) ;
#20600 = CARTESIAN_POINT ( 'NONE',  ( -10.81189881249999907, -6.242252689847864744, -178.9687500020484094 ) ) ;
#20601 = CARTESIAN_POINT ( 'NONE',  ( 5.000000000000000000, 8.660254037844385522, -68.12500000409677625 ) ) ;
#20602 = CARTESIAN_POINT ( 'NONE',  ( -10.00000000000019362, -5.773502691896140959, -179.6250000000000568 ) ) ;
#20603 = CARTESIAN_POINT ( 'NONE',  ( -9.999999999999998224, 1.224646799147353059E-15, -166.2500000000000000 ) ) ;
#20604 = CARTESIAN_POINT ( 'NONE',  ( -10.81189881249999907, -6.242252689847864744, -72.65625000204836681 ) ) ;
#20605 = CARTESIAN_POINT ( 'NONE',  ( -2.293366432827344421E-15, -12.48450537969573659, -60.40625000204838813 ) ) ;
#20606 = CARTESIAN_POINT ( 'NONE',  ( 10.00000000000000000, 5.773502691896255534, -48.75000000409676204 ) ) ;
#20607 = CIRCLE ( 'NONE', #34440, 60.00000000000000711 ) ;
#20608 = CARTESIAN_POINT ( 'NONE',  ( -10.81189881249999907, -6.242252689847864744, -6.468750002048357040 ) ) ;
#20609 = FACE_OUTER_BOUND ( 'NONE', #17958, .T. ) ;
#20610 = CARTESIAN_POINT ( 'NONE',  ( 10.81189881249999551, -6.242252689847874514, -175.6562500020484094 ) ) ;
#20611 = CARTESIAN_POINT ( 'NONE',  ( -5.405949406249996869, 9.363379034771805109, -4.031250002048375691 ) ) ;
#20612 = CARTESIAN_POINT ( 'NONE',  ( 7.070501591499376803E-16, 11.54700538379251284, -147.5000000040967905 ) ) ;
#20613 = CARTESIAN_POINT ( 'NONE',  ( -2.121150477449813534E-15, -11.54700538379251284, -148.2500000040968189 ) ) ;
#20614 = DIRECTION ( 'NONE',  ( -0.000000000000000000, -0.000000000000000000, 1.000000000000000000 ) ) ;
#20615 = DIRECTION ( 'NONE',  ( -0.000000000000000000, -0.000000000000000000, 1.000000000000000000 ) ) ;
#20617 = ORIENTED_EDGE ( 'NONE', *, *, #42299, .F. ) ;
#20616 = CARTESIAN_POINT ( 'NONE',  ( 5.405949406249992428, -9.363379034771808662, -87.28125000204838102 ) ) ;
#20619 = ORIENTED_EDGE ( 'NONE', *, *, #33818, .T. ) ;
#20618 = CARTESIAN_POINT ( 'NONE',  ( -9.999999999999998224, 1.224646799147353059E-15, -91.62500000409677625 ) ) ;
#20620 = ORIENTED_EDGE ( 'NONE', *, *, #24095, .F. ) ;
#20621 = CARTESIAN_POINT ( 'NONE',  ( -5.405949406249996869, 9.363379034771805109, -23.34375000204835970 ) ) ;
#20622 = CARTESIAN_POINT ( 'NONE',  ( -5.405949406249996869, 9.363379034771805109, -16.03125000204835970 ) ) ;
#20623 = DATE_TIME_ROLE ( 'classification_date' ) ;
#20624 = CIRCLE ( 'NONE', #7546, 20.00000000000000000 ) ;
#20625 = CARTESIAN_POINT ( 'NONE',  ( -5.405949406249996869, 9.363379034771805109, -68.34375000204836681 ) ) ;
#20626 = CARTESIAN_POINT ( 'NONE',  ( -4.999999999999996447, 8.660254037844387298, -92.99999999999998579 ) ) ;
#20627 = CARTESIAN_POINT ( 'NONE',  ( -10.00000000000000000, -5.773502691896251982, -43.12499999999997158 ) ) ;
#20628 = CARTESIAN_POINT ( 'NONE',  ( 5.405949406249992428, -9.363379034771808662, -189.0937500020483810 ) ) ;
#20629 = CARTESIAN_POINT ( 'NONE',  ( -10.81189881249999729, 1.324075727343319199E-15, -164.0937500020484094 ) ) ;
#20630 = CARTESIAN_POINT ( 'NONE',  ( 9.999999999999998224, 0.000000000000000000, -119.0000000000000000 ) ) ;
#20631 = CARTESIAN_POINT ( 'NONE',  ( -9.999999999999998224, 1.224646799147353059E-15, -200.0000000000000000 ) ) ;
#20632 = AXIS2_PLACEMENT_3D ( 'NONE', #28801, #42146, #22102 ) ;
#20633 = CARTESIAN_POINT ( 'NONE',  ( -4.999999999999996447, 8.660254037844387298, -70.87500000409677625 ) ) ;
#20634 = CARTESIAN_POINT ( 'NONE',  ( -4.999999999999996447, 8.660254037844387298, 1.124999995903236405 ) ) ;
#20635 = CARTESIAN_POINT ( 'NONE',  ( -2.121150477449813534E-15, -11.54700538379251284, -89.75000000409677625 ) ) ;
#20636 = CARTESIAN_POINT ( 'NONE',  ( -5.405949406250003975, -9.363379034771801557, -114.3437500020483810 ) ) ;
#20637 = LINE ( 'NONE', #7276, #30091 ) ;
#20638 = CARTESIAN_POINT ( 'NONE',  ( -10.81189881249999729, 1.324075727343319199E-15, -89.28125000204838102 ) ) ;
#20639 = EDGE_CURVE ( 'NONE', #30470, #10633, #1212, .T. ) ;
#20640 = CARTESIAN_POINT ( 'NONE',  ( 5.405949406249992428, -9.363379034771808662, -102.0937500020483810 ) ) ;
#20641 = CARTESIAN_POINT ( 'NONE',  ( 5.405949406249999534, 9.363379034771803333, -71.59375000204836681 ) ) ;
#20642 = ADVANCED_FACE ( 'NONE', ( #12814 ), #42173, .T. ) ;
#20643 = CARTESIAN_POINT ( 'NONE',  ( 10.81189881249999729, 0.000000000000000000, -78.03125000204838102 ) ) ;
#20644 = CARTESIAN_POINT ( 'NONE',  ( -5.000000000000003553, -8.660254037844383745, -163.3750000040967905 ) ) ;
#20645 = EDGE_CURVE ( 'NONE', #5415, #25371, #26538, .T. ) ;
#20646 = CARTESIAN_POINT ( 'NONE',  ( -5.405949406249996869, 9.363379034771805109, -158.5312500020484094 ) ) ;
#20647 = CARTESIAN_POINT ( 'NONE',  ( -5.405949406249996869, 9.363379034771805109, -172.0312500020484094 ) ) ;
#20648 = CARTESIAN_POINT ( 'NONE',  ( -5.405949406249996869, 9.363379034771805109, 0.6562499979516356330 ) ) ;
#20649 = CARTESIAN_POINT ( 'NONE',  ( -9.999999999999998224, 1.224646799147353059E-15, -0.1250000040967647053 ) ) ;
#20650 = CARTESIAN_POINT ( 'NONE',  ( -10.81189881249999907, -6.242252689847864744, -108.4687500020483810 ) ) ;
#20651 = CARTESIAN_POINT ( 'NONE',  ( 9.999999999999998224, 0.000000000000000000, -70.99999999999998579 ) ) ;
#20652 = CARTESIAN_POINT ( 'NONE',  ( -10.81189881249999729, 6.242252689847871849, -6.906250002048365033 ) ) ;
#20653 = CARTESIAN_POINT ( 'NONE',  ( -10.00000000000000000, -5.773502691896251982, -88.50000000409679046 ) ) ;
#20654 = DIRECTION ( 'NONE',  ( -0.4999999999999997224, -0.8660254037844388186, 0.000000000000000000 ) ) ;
#20655 = PRODUCT_DEFINITION ( 'UNKNOWN', '', #36620, #42507 ) ;
#20656 = CARTESIAN_POINT ( 'NONE',  ( 5.405949406249992428, -9.363379034771808662, -103.7812500020483810 ) ) ;
#20657 = CARTESIAN_POINT ( 'NONE',  ( -2.293366432827344421E-15, -12.48450537969573659, -85.90625000204839523 ) ) ;
#20658 = CARTESIAN_POINT ( 'NONE',  ( -9.999999999999998224, 5.773502691896259087, -78.25000000409677625 ) ) ;
#20659 = LINE ( 'NONE', #1038, #213 ) ;
#20660 = CARTESIAN_POINT ( 'NONE',  ( -5.405949406250003975, -9.363379034771801557, -33.34375000204836681 ) ) ;
#20661 = ORIENTED_EDGE ( 'NONE', *, *, #16145, .F. ) ;
#20662 = CARTESIAN_POINT ( 'NONE',  ( -10.81189881249999729, 6.242252689847871849, -197.4062500020484379 ) ) ;
#20663 = CARTESIAN_POINT ( 'NONE',  ( 10.81189881249999729, 0.000000000000000000, -28.53125000204837036 ) ) ;
#20664 = CARTESIAN_POINT ( 'NONE',  ( -2.293366432827344421E-15, -12.48450537969573659, -15.21875000204835615 ) ) ;
#20665 = CARTESIAN_POINT ( 'NONE',  ( 0.000000000000000000, 0.000000000000000000, -200.0000000000000000 ) ) ;
#20666 = EDGE_CURVE ( 'NONE', #38366, #27040, #7368, .T. ) ;
#20667 = CARTESIAN_POINT ( 'NONE',  ( -9.999999999999998224, 5.773502691896259087, -6.250000004096755823 ) ) ;
#20668 = CARTESIAN_POINT ( 'NONE',  ( 5.405949406249999534, 9.363379034771803333, -134.7812500020483810 ) ) ;
#20669 = EDGE_CURVE ( 'NONE', #24317, #4916, #5624, .T. ) ;
#20670 = CARTESIAN_POINT ( 'NONE',  ( 9.999999999999998224, 0.000000000000000000, -192.5000000000000000 ) ) ;
#20671 = LINE ( 'NONE', #17423, #38570 ) ;
#20673 = ORIENTED_EDGE ( 'NONE', *, *, #40453, .F. ) ;
#20672 = CARTESIAN_POINT ( 'NONE',  ( -10.81189881249999729, 6.242252689847871849, -108.9062500020483810 ) ) ;
#20674 = CARTESIAN_POINT ( 'NONE',  ( -9.999999999999998224, 1.224646799147353059E-15, -48.12500000409677625 ) ) ;
#20675 = ORIENTED_EDGE ( 'NONE', *, *, #24808, .F. ) ;
#20676 =( BOUNDED_CURVE ( )  B_SPLINE_CURVE ( 2, ( #23583, #29629, #39121, #72, #10184, #36731, #29206 ),
 .UNSPECIFIED., .F., .F. ) 
 B_SPLINE_CURVE_WITH_KNOTS ( ( 3, 2, 2, 3 ),
 ( 0.9067164179104481025, 0.9079601990049754878, 0.9092039800995028731, 0.9104477611940301474 ),
 .UNSPECIFIED. ) 
 CURVE ( )  GEOMETRIC_REPRESENTATION_ITEM ( )  RATIONAL_B_SPLINE_CURVE ( ( 0.9999999999999641398, 0.8660254037844745678, 1.000000000000000000, 0.8660254037844387076, 1.000000000000000000, 0.8660254037844028474, 1.000000000000035971 ) ) 
 REPRESENTATION_ITEM ( '' )  );
#20677 = ORIENTED_EDGE ( 'NONE', *, *, #30325, .T. ) ;
#20678 = CARTESIAN_POINT ( 'NONE',  ( -10.81189881249999729, 6.242252689847871849, -36.90625000204835970 ) ) ;
#20679 = PERSON_AND_ORGANIZATION ( #11915, #17965 ) ;
#20680 = CARTESIAN_POINT ( 'NONE',  ( -2.293366432827344421E-15, -12.48450537969573659, -94.71875000204838102 ) ) ;
#20681 = CARTESIAN_POINT ( 'NONE',  ( 9.999999999999998224, 0.000000000000000000, -115.9999999999999858 ) ) ;
#20682 = EDGE_CURVE ( 'NONE', #21356, #20412, #24546, .T. ) ;
#20683 = CARTESIAN_POINT ( 'NONE',  ( -9.999999999999998224, 1.224646799147353059E-15, -136.2499999999999716 ) ) ;
#20684 = EDGE_CURVE ( 'NONE', #9826, #6419, #10007, .T. ) ;
#20685 = CARTESIAN_POINT ( 'NONE',  ( -10.81189881249999729, 1.324075727343319199E-15, -192.5937500020484094 ) ) ;
#20686 = CARTESIAN_POINT ( 'NONE',  ( 10.81189881249999907, 6.242252689847868297, -173.9062500020484094 ) ) ;
#20687 = CARTESIAN_POINT ( 'NONE',  ( -10.00000000000076916, 5.773502691895813221, -137.8750000000000000 ) ) ;
#20688 = VECTOR ( 'NONE', #39469, 1000.000000000000000 ) ;
#20689 = CARTESIAN_POINT ( 'NONE',  ( -10.81189881249999729, 6.242252689847871849, -126.7187500020483810 ) ) ;
#20690 = CARTESIAN_POINT ( 'NONE',  ( -5.405949406249996869, 9.363379034771805109, -95.34375000204838102 ) ) ;
#20691 = DIRECTION ( 'NONE',  ( 0.000000000000000000, 0.000000000000000000, -1.000000000000000000 ) ) ;
#20692 = CARTESIAN_POINT ( 'NONE',  ( 10.81189881249999729, 0.000000000000000000, -102.0312500020483952 ) ) ;
#20693 = CARTESIAN_POINT ( 'NONE',  ( -5.000000000000003553, -8.660254037844383745, -188.8750000040967905 ) ) ;
#20694 = CARTESIAN_POINT ( 'NONE',  ( 5.405949406249999534, 9.363379034771803333, -109.0937500020483810 ) ) ;
#20695 = CARTESIAN_POINT ( 'NONE',  ( -10.81189881249999729, 6.242252689847871849, -176.4062500020484094 ) ) ;
#20696 = CARTESIAN_POINT ( 'NONE',  ( -9.999999999999804601, 5.773502691896371886, -179.8750000000000000 ) ) ;
#20697 = DIRECTION ( 'NONE',  ( -0.000000000000000000, -0.000000000000000000, 1.000000000000000000 ) ) ;
#20698 = CARTESIAN_POINT ( 'NONE',  ( 10.81189881249999907, 6.242252689847868297, -196.4062500020484379 ) ) ;
#20699 = CARTESIAN_POINT ( 'NONE',  ( -5.405949406250003975, -9.363379034771801557, -49.84375000204838102 ) ) ;
#20700 = CARTESIAN_POINT ( 'NONE',  ( 7.644554776091147741E-16, 12.48450537969573659, -38.46875000204835260 ) ) ;
#20701 = CARTESIAN_POINT ( 'NONE',  ( -5.000000000000003553, -8.660254037844383745, -173.8750000040968189 ) ) ;
#20702 = CARTESIAN_POINT ( 'NONE',  ( 10.81189881249999551, -6.242252689847874514, -13.65625000204836503 ) ) ;
#20703 = CARTESIAN_POINT ( 'NONE',  ( 5.405949406249999534, 9.363379034771803333, -19.09375000204835260 ) ) ;
#20704 = CARTESIAN_POINT ( 'NONE',  ( 9.999999999999998224, 0.000000000000000000, -27.49999999999996803 ) ) ;
#20705 = CARTESIAN_POINT ( 'NONE',  ( -10.81189881249999729, 1.324075727343319199E-15, -132.5937500020483810 ) ) ;
#20706 = CARTESIAN_POINT ( 'NONE',  ( 10.00000000000000000, 5.773502691896255534, -94.87499999999998579 ) ) ;
#20707 = CARTESIAN_POINT ( 'NONE',  ( 7.644554776091147741E-16, 12.48450537969573659, -28.15625000204838102 ) ) ;
#20708 = CARTESIAN_POINT ( 'NONE',  ( 10.00000000000000000, 5.773502691896255534, -113.2500000040967905 ) ) ;
#20709 = CARTESIAN_POINT ( 'NONE',  ( -9.999999999999998224, 1.224646799147353059E-15, -152.7500000000000000 ) ) ;
#20710 = CARTESIAN_POINT ( 'NONE',  ( 9.999999999999996447, -5.773502691896262640, -62.12499999999998579 ) ) ;
#20711 = CARTESIAN_POINT ( 'NONE',  ( -10.81189881249999907, -6.242252689847864744, -120.6562500020483810 ) ) ;
#20712 = CARTESIAN_POINT ( 'NONE',  ( -10.81189881249999729, -6.242252689847864744, -104.1562500020483952 ) ) ;
#20713 = ORIENTED_EDGE ( 'NONE', *, *, #8063, .F. ) ;
#20714 = CARTESIAN_POINT ( 'NONE',  ( -4.999999999999996447, 8.660254037844387298, -100.8750000040967905 ) ) ;
#20715 = DIRECTION ( 'NONE',  ( 0.000000000000000000, 0.000000000000000000, 1.000000000000000000 ) ) ;
#20716 = CARTESIAN_POINT ( 'NONE',  ( -10.81189881249999729, 1.324075727343319199E-15, -56.09375000204835970 ) ) ;
#20717 = ORIENTED_EDGE ( 'NONE', *, *, #10069, .T. ) ;
#20718 = CARTESIAN_POINT ( 'NONE',  ( 4.999999999999992006, -8.660254037844389075, -35.24999999999997868 ) ) ;
#20719 = EDGE_CURVE ( 'NONE', #26093, #14015, #30956, .T. ) ;
#20720 = CARTESIAN_POINT ( 'NONE',  ( 10.81189881249999729, 6.242252689847867408, -32.90625000204835970 ) ) ;
#20721 = CARTESIAN_POINT ( 'NONE',  ( 9.999999999999996447, -5.773502691896262640, -158.1250000000000284 ) ) ;
#20722 = CARTESIAN_POINT ( 'NONE',  ( -10.00000000000102496, 5.773502691895664007, -34.75000000409671941 ) ) ;
#20723 = CARTESIAN_POINT ( 'NONE',  ( 10.00000000000000000, 5.773502691896255534, -27.75000000409677625 ) ) ;
#20724 =( BOUNDED_CURVE ( )  B_SPLINE_CURVE ( 2, ( #18790, #17924, #31121, #5429, #2196, #31552, #27875 ),
 .UNSPECIFIED., .F., .F. ) 
 B_SPLINE_CURVE_WITH_KNOTS ( ( 3, 2, 2, 3 ),
 ( 0.03731343283582092690, 0.03855721393034829136, 0.03980099502487565583, 0.04104477611940302029 ),
 .UNSPECIFIED. ) 
 CURVE ( )  GEOMETRIC_REPRESENTATION_ITEM ( )  RATIONAL_B_SPLINE_CURVE ( ( 0.9999999999999963363, 0.8660254037844424824, 1.000000000000000000, 0.8660254037844387076, 1.000000000000000000, 0.8660254037844349329, 1.000000000000003775 ) ) 
 REPRESENTATION_ITEM ( '' )  );
#20725 = LOCAL_TIME ( 11, 57, 6.000000000000000000, #12082 ) ;
#20726 = CARTESIAN_POINT ( 'NONE',  ( 10.81189881249999551, -6.242252689847874514, -135.1562500020484094 ) ) ;
#20727 = VECTOR ( 'NONE', #30563, 1000.000000000000000 ) ;
#20728 = CARTESIAN_POINT ( 'NONE',  ( 9.999999999999998224, 0.000000000000000000, -162.8750000040967905 ) ) ;
#20729 = EDGE_LOOP ( 'NONE', ( #2892, #27580, #11968, #25064 ) ) ;
#20730 =( BOUNDED_CURVE ( )  B_SPLINE_CURVE ( 2, ( #9259, #25260, #22427, #11852, #8638, #21793, #34973 ),
 .UNSPECIFIED., .F., .F. ) 
 B_SPLINE_CURVE_WITH_KNOTS ( ( 3, 2, 2, 3 ),
 ( 0.8432835820895525636, 0.8445273631840799489, 0.8457711442786073341, 0.8470149253731346084 ),
 .UNSPECIFIED. ) 
 CURVE ( )  GEOMETRIC_REPRESENTATION_ITEM ( )  RATIONAL_B_SPLINE_CURVE ( ( 0.9999999999999641398, 0.8660254037844745678, 1.000000000000000000, 0.8660254037844387076, 1.000000000000000000, 0.8660254037844028474, 1.000000000000035971 ) ) 
 REPRESENTATION_ITEM ( '' )  );
#20732 = ORIENTED_EDGE ( 'NONE', *, *, #26583, .T. ) ;
#20731 = ORIENTED_EDGE ( 'NONE', *, *, #30729, .F. ) ;
#20733 = CARTESIAN_POINT ( 'NONE',  ( 0.000000000000000000, 0.000000000000000000, -99.99999999999998579 ) ) ;
#20734 = CARTESIAN_POINT ( 'NONE',  ( -9.999999999999998224, 1.224646799147353059E-15, -155.7500000000000000 ) ) ;
#20735 = CARTESIAN_POINT ( 'NONE',  ( 7.644554776091147741E-16, 12.48450537969573659, -165.9687500020483810 ) ) ;
#20736 = CARTESIAN_POINT ( 'NONE',  ( -10.81189881249999907, -6.242252689847864744, -194.1562500020484094 ) ) ;
#20737 = CARTESIAN_POINT ( 'NONE',  ( 10.81189881249999729, 0.000000000000000000, -13.34375000204834905 ) ) ;
#20738 = DIRECTION ( 'NONE',  ( -0.000000000000000000, -0.000000000000000000, 1.000000000000000000 ) ) ;
#20739 = CARTESIAN_POINT ( 'NONE',  ( -10.81189881249999729, -6.242252689847864744, -150.4687500020484094 ) ) ;
#20740 = CARTESIAN_POINT ( 'NONE',  ( 10.81189881249999551, -6.242252689847874514, -134.9687500020483810 ) ) ;
#20741 = CARTESIAN_POINT ( 'NONE',  ( -10.81189881249999729, 1.324075727343319199E-15, -110.2812500020483810 ) ) ;
#20742 = CARTESIAN_POINT ( 'NONE',  ( -10.81189881249999729, 6.242252689847871849, -117.7187500020483952 ) ) ;
#20743 = CARTESIAN_POINT ( 'NONE',  ( -10.00000000000000000, -5.773502691896251982, -198.0000000040968189 ) ) ;
#20744 = CARTESIAN_POINT ( 'NONE',  ( -10.81189881249999729, 6.242252689847871849, -128.4062500020484094 ) ) ;
#20746 = CARTESIAN_POINT ( 'NONE',  ( -10.81189881249999729, 6.242252689847871849, -8.218750002048354375 ) ) ;
#20745 = B_SPLINE_CURVE_WITH_KNOTS ( 'NONE', 3,
 ( #1165, #3973, #27703, #30946, #40841, #34192, #7419, #4820, #21003, #17967, #27270, #31167, #34400, #4610, #30313, #37186, #1379, #40409, #37626, #1597, #24475, #10854, #20569, #14725, #7634, #13870, #33975, #14509, #27917, #17534, #36983, #10433 ),
 .UNSPECIFIED., .F., .F.,
 ( 4, 2, 2, 2, 2, 2, 2, 2, 2, 2, 2, 2, 2, 2, 2, 4 ),
 ( 0.002038875896278021741, 0.004610120927203064864, 0.005895743442665587510, 0.007181365958128110155, 0.008466988473590628464, 0.009752610989053148507, 0.01103823350451566855, 0.01232385601997818859, 0.01360947853544071037, 0.01489510105090322868, 0.01618072356636575046, 0.01746634608182826703, 0.01875196859729078708, 0.02003759111275331059, 0.02132321362821582716, 0.02260883614367834721 ),
 .UNSPECIFIED. ) ;
#20747 = CARTESIAN_POINT ( 'NONE',  ( 10.81189881249999729, 0.000000000000000000, -128.8437500020484094 ) ) ;
#20748 = CARTESIAN_POINT ( 'NONE',  ( -9.999999999999998224, 1.224646799147353059E-15, -200.0000000000000000 ) ) ;
#20749 = CARTESIAN_POINT ( 'NONE',  ( -9.999999999999998224, 1.224646799147353059E-15, -196.6250000040967905 ) ) ;
#20750 = CARTESIAN_POINT ( 'NONE',  ( -9.999999999999998224, 1.224646799147353059E-15, -154.2500000000000000 ) ) ;
#20751 = CARTESIAN_POINT ( 'NONE',  ( 7.070501591499377789E-16, 11.54700538379251284, -21.12499999999997513 ) ) ;
#20752 = CC_DESIGN_APPROVAL ( #38361, ( #14057 ) ) ;
#20753 = CARTESIAN_POINT ( 'NONE',  ( -10.81189881249999729, 1.324075727343319199E-15, -72.59375000204838102 ) ) ;
#20754 = CARTESIAN_POINT ( 'NONE',  ( -10.81189881249999907, -6.242252689847864744, -61.96875000204838813 ) ) ;
#20755 = CARTESIAN_POINT ( 'NONE',  ( 5.405949406249992428, -9.363379034771808662, -37.78125000204838102 ) ) ;
#20756 = CARTESIAN_POINT ( 'NONE',  ( 5.405949406249992428, -9.363379034771808662, -42.09375000204837391 ) ) ;
#20757 = DIRECTION ( 'NONE',  ( -0.000000000000000000, -0.000000000000000000, 1.000000000000000000 ) ) ;
#20758 = CARTESIAN_POINT ( 'NONE',  ( 10.81189881249999907, 6.242252689847868297, -154.2187500020483810 ) ) ;
#20759 = CARTESIAN_POINT ( 'NONE',  ( 7.070501591499377789E-16, 11.54700538379251284, -118.6250000000000142 ) ) ;
#20760 = CARTESIAN_POINT ( 'NONE',  ( -10.81189881249999729, -6.242252689847864744, -134.1562500020483810 ) ) ;
#20761 = CARTESIAN_POINT ( 'NONE',  ( -9.999999999998969713, -5.773502691896847949, -67.50000000409676204 ) ) ;
#20762 = CARTESIAN_POINT ( 'NONE',  ( -9.999999999999998224, 5.773502691896259087, -80.87499999999998579 ) ) ;
#20763 = CARTESIAN_POINT ( 'NONE',  ( 5.405949406249992428, -9.363379034771808662, -19.78125000204836326 ) ) ;
#20764 = ORIENTED_EDGE ( 'NONE', *, *, #33818, .F. ) ;
#20765 = CARTESIAN_POINT ( 'NONE',  ( -6.058704384512919816, 8.986510772356837151, -100.0161565621822319 ) ) ;
#20766 = CARTESIAN_POINT ( 'NONE',  ( 9.999999999999998224, 0.000000000000000000, -123.8750000040967905 ) ) ;
#20767 = CARTESIAN_POINT ( 'NONE',  ( 9.999999999999998224, 0.000000000000000000, -9.499999999999953815 ) ) ;
#20768 = ADVANCED_FACE ( 'NONE', ( #14234 ), #17484, .F. ) ;
#20769 = CARTESIAN_POINT ( 'NONE',  ( 9.999999999999996447, -5.773502691896262640, -32.50000000409675494 ) ) ;
#20770 = CARTESIAN_POINT ( 'NONE',  ( -9.999999999999998224, 0.000000000000000000, -99.99999999999998579 ) ) ;
#20771 = CARTESIAN_POINT ( 'NONE',  ( 5.405949406249999534, 9.363379034771803333, -52.28125000204835970 ) ) ;
#20772 = CARTESIAN_POINT ( 'NONE',  ( -9.999999999999998224, 1.224646799147353059E-15, -146.7500000000000000 ) ) ;
#20773 = CARTESIAN_POINT ( 'NONE',  ( 7.644554776091147741E-16, 12.48450537969573659, -155.6562500020484094 ) ) ;
#20774 = CARTESIAN_POINT ( 'NONE',  ( -5.405949406250003975, -9.363379034771801557, -135.3437500020484094 ) ) ;
#20775 = ORIENTED_EDGE ( 'NONE', *, *, #39145, .F. ) ;
#20776 = CARTESIAN_POINT ( 'NONE',  ( -9.999999999999998224, 1.224646799147353059E-15, -163.6250000040967905 ) ) ;
#20778 = ADVANCED_FACE ( 'NONE', ( #18134 ), #40571, .F. ) ;
#20777 = ORIENTED_EDGE ( 'NONE', *, *, #30448, .T. ) ;
#20779 = LOCAL_TIME ( 11, 57, 6.000000000000000000, #22606 ) ;
#20780 = ORIENTED_EDGE ( 'NONE', *, *, #17738, .T. ) ;
#20782 = ORIENTED_EDGE ( 'NONE', *, *, #15145, .F. ) ;
#20781 = CARTESIAN_POINT ( 'NONE',  ( -2.293366432827344421E-15, -12.48450537969573659, -114.2187500020483668 ) ) ;
#20783 = CARTESIAN_POINT ( 'NONE',  ( -9.999999999999998224, 1.224646799147353059E-15, -52.24999999999996447 ) ) ;
#20784 = CARTESIAN_POINT ( 'NONE',  ( 5.405949406249992428, -9.363379034771808662, -187.5937500020483810 ) ) ;
#20785 = VECTOR ( 'NONE', #25116, 1000.000000000000000 ) ;
#20786 = CARTESIAN_POINT ( 'NONE',  ( -10.81189881249999729, 1.324075727343319199E-15, -41.09375000204837391 ) ) ;
#20787 = CARTESIAN_POINT ( 'NONE',  ( -2.293366432827344421E-15, -12.48450537969573659, -175.7187500020483810 ) ) ;
#20788 = CARTESIAN_POINT ( 'NONE',  ( 5.405949406249992428, -9.363379034771808662, -165.0937500020484094 ) ) ;
#20789 =( BOUNDED_CURVE ( )  B_SPLINE_CURVE ( 2, ( #18918, #26454, #32101, #22371, #2534, #16287, #19329 ),
 .UNSPECIFIED., .F., .F. ) 
 B_SPLINE_CURVE_WITH_KNOTS ( ( 3, 2, 2, 3 ),
 ( 0.1716417910447761430, 0.1728855721393035005, 0.1741293532338308858, 0.1753731343283582433 ),
 .UNSPECIFIED. ) 
 CURVE ( )  GEOMETRIC_REPRESENTATION_ITEM ( )  RATIONAL_B_SPLINE_CURVE ( ( 0.9999999999999970024, 0.8660254037844417052, 1.000000000000000000, 0.8660254037844387076, 1.000000000000000000, 0.8660254037844357100, 1.000000000000003109 ) ) 
 REPRESENTATION_ITEM ( '' )  );
#20790 = CARTESIAN_POINT ( 'NONE',  ( 10.00000000000102318, -5.773502691895667560, -65.50000000409674783 ) ) ;
#20791 = CARTESIAN_POINT ( 'NONE',  ( -10.81189881249999729, 6.242252689847871849, -141.7187500020483810 ) ) ;
#20792 = CARTESIAN_POINT ( 'NONE',  ( 7.644554776091147741E-16, 12.48450537969573659, -152.4687500020484094 ) ) ;
#20793 = FACE_OUTER_BOUND ( 'NONE', #25894, .T. ) ;
#20794 = CARTESIAN_POINT ( 'NONE',  ( -10.00000000000154188, 5.773502691895366468, -66.25000000409673362 ) ) ;
#20795 = CARTESIAN_POINT ( 'NONE',  ( 10.00000000000000000, 5.773502691896255534, -183.3750000000000000 ) ) ;
#20796 = CARTESIAN_POINT ( 'NONE',  ( 10.81189881249999907, 6.242252689847868297, -91.21875000204838102 ) ) ;
#20797 = CARTESIAN_POINT ( 'NONE',  ( -9.999999999999998224, 1.224646799147353059E-15, -198.1250000040967905 ) ) ;
#20798 = CARTESIAN_POINT ( 'NONE',  ( 5.405949406249992428, -9.363379034771808662, -55.78125000204836681 ) ) ;
#20799 = CARTESIAN_POINT ( 'NONE',  ( 5.000000000000000000, 8.660254037844385522, -87.62500000409677625 ) ) ;
#20800 = CARTESIAN_POINT ( 'NONE',  ( -5.405949406249996869, 9.363379034771805109, -177.8437500020483810 ) ) ;
#20801 = CARTESIAN_POINT ( 'NONE',  ( -10.81189881249999907, -6.242252689847864744, -120.6562500020483810 ) ) ;
#20802 = CARTESIAN_POINT ( 'NONE',  ( 7.644554776091147741E-16, 12.48450537969573659, -151.1562500020484094 ) ) ;
#20803 = CARTESIAN_POINT ( 'NONE',  ( -10.00000000000076916, 5.773502691895813221, -115.3749999999999716 ) ) ;
#20804 = CARTESIAN_POINT ( 'NONE',  ( -10.81189881249999907, -6.242252689847864744, -56.15625000204838102 ) ) ;
#20805 = CARTESIAN_POINT ( 'NONE',  ( -10.00000000000000000, -5.773502691896251982, -133.5000000040967905 ) ) ;
#20806 = CARTESIAN_POINT ( 'NONE',  ( 9.999999999999998224, 0.000000000000000000, -106.9999999999999858 ) ) ;
#20807 = CIRCLE ( 'NONE', #27048, 31.99999999999997158 ) ;
#20808 = EDGE_CURVE ( 'NONE', #40108, #31308, #30677, .T. ) ;
#20809 = ORIENTED_EDGE ( 'NONE', *, *, #42227, .T. ) ;
#20810 = CARTESIAN_POINT ( 'NONE',  ( 10.81189881249999729, 6.242252689847867408, -131.9062500020483810 ) ) ;
#20811 = CARTESIAN_POINT ( 'NONE',  ( -9.999999999999998224, 5.773502691896259087, -148.7500000040967905 ) ) ;
#20812 = CARTESIAN_POINT ( 'NONE',  ( 10.81189881249999729, 0.000000000000000000, -148.5312500020483810 ) ) ;
#20813 = CARTESIAN_POINT ( 'NONE',  ( -5.405949406249996869, 9.363379034771805109, -190.0312500020484094 ) ) ;
#20814 = ORIENTED_EDGE ( 'NONE', *, *, #15002, .T. ) ;
#20815 = CARTESIAN_POINT ( 'NONE',  ( -9.999999999999998224, 5.773502691896259087, -49.37499999999997868 ) ) ;
#20816 = CARTESIAN_POINT ( 'NONE',  ( 5.405949406249992428, -9.363379034771808662, -178.5937500020484094 ) ) ;
#20817 = CARTESIAN_POINT ( 'NONE',  ( -9.999999999999998224, 5.773502691896259087, -58.75000000409676915 ) ) ;
#20818 = CARTESIAN_POINT ( 'NONE',  ( 9.999999999999998224, 0.000000000000000000, -179.0000000000000000 ) ) ;
#20819 = CARTESIAN_POINT ( 'NONE',  ( -5.000000000000003553, -8.660254037844383745, -166.0000000000000000 ) ) ;
#20820 = CARTESIAN_POINT ( 'NONE',  ( 5.405949406249999534, 9.363379034771803333, -77.78125000204838102 ) ) ;
#20821 = CARTESIAN_POINT ( 'NONE',  ( -10.81189881249999729, 1.324075727343319199E-15, -48.78125000204838813 ) ) ;
#20822 = CARTESIAN_POINT ( 'NONE',  ( 5.000000000000000000, 8.660254037844385522, -56.12500000409676204 ) ) ;
#20823 = CARTESIAN_POINT ( 'NONE',  ( -10.81189881249999729, 6.242252689847871849, -9.718750002048361480 ) ) ;
#20824 = DIRECTION ( 'NONE',  ( -0.000000000000000000, -0.000000000000000000, 1.000000000000000000 ) ) ;
#20825 = CARTESIAN_POINT ( 'NONE',  ( -2.293366432827344421E-15, -12.48450537969573659, -177.4062500020483810 ) ) ;
#20826 = AXIS2_PLACEMENT_3D ( 'NONE', #37652, #21456, #17992 ) ;
#20827 = CARTESIAN_POINT ( 'NONE',  ( 5.405949406249999534, 9.363379034771803333, -4.281250002048375691 ) ) ;
#20828 = LINE ( 'NONE', #31208, #36662 ) ;
#20829 = CARTESIAN_POINT ( 'NONE',  ( 9.999999999999742428, 5.773502691896404748, -138.7500000040967905 ) ) ;
#20830 = CARTESIAN_POINT ( 'NONE',  ( 9.999999999999998224, 0.000000000000000000, -70.99999999999998579 ) ) ;
#20831 = PLANE ( 'NONE',  #38306 ) ;
#20832 = CARTESIAN_POINT ( 'NONE',  ( -9.999999999999998224, 1.224646799147353059E-15, -195.1250000040967905 ) ) ;
#20834 = VERTEX_POINT ( 'NONE', #28087 ) ;
#20833 = CARTESIAN_POINT ( 'NONE',  ( -10.81189881249999907, -6.242252689847864744, -83.15625000204836681 ) ) ;
#20835 = EDGE_CURVE ( 'NONE', #35094, #38971, #14405, .T. ) ;
#20837 = ORIENTED_EDGE ( 'NONE', *, *, #33703, .T. ) ;
#20836 = CARTESIAN_POINT ( 'NONE',  ( 9.999999999999998224, 0.000000000000000000, -69.49999999999997158 ) ) ;
#20838 = ORIENTED_EDGE ( 'NONE', *, *, #33336, .F. ) ;
#20839 = VECTOR ( 'NONE', #23866, 1000.000000000000000 ) ;
#20840 =( BOUNDED_CURVE ( )  B_SPLINE_CURVE ( 2, ( #37540, #40759, #11201, #34962, #2156, #27836, #4736 ),
 .UNSPECIFIED., .F., .F. ) 
 B_SPLINE_CURVE_WITH_KNOTS ( ( 3, 2, 2, 3 ),
 ( 0.02611940298507465369, 0.02736318407960201815, 0.02860696517412938261, 0.02985074626865674360 ),
 .UNSPECIFIED. ) 
 CURVE ( )  GEOMETRIC_REPRESENTATION_ITEM ( )  RATIONAL_B_SPLINE_CURVE ( ( 0.9999999999999970024, 0.8660254037844417052, 1.000000000000000000, 0.8660254037844387076, 1.000000000000000000, 0.8660254037844357100, 1.000000000000003109 ) ) 
 REPRESENTATION_ITEM ( '' )  );
#20841 = CARTESIAN_POINT ( 'NONE',  ( -5.405949406249996869, 9.363379034771805109, -38.34375000204837391 ) ) ;
#20842 = CARTESIAN_POINT ( 'NONE',  ( 10.81189881249999729, 0.000000000000000000, -28.34375000204836326 ) ) ;
#20843 = CARTESIAN_POINT ( 'NONE',  ( -10.81189881249999729, 6.242252689847871849, -12.90625000204835970 ) ) ;
#20844 = CARTESIAN_POINT ( 'NONE',  ( 10.81189881249999907, 6.242252689847868297, -65.71875000204836681 ) ) ;
#20845 = CARTESIAN_POINT ( 'NONE',  ( 9.999999999999998224, 0.000000000000000000, -131.0000000000000000 ) ) ;
#20846 = CARTESIAN_POINT ( 'NONE',  ( 9.999999999999998224, 0.000000000000000000, -45.49999999999998579 ) ) ;
#20847 = CARTESIAN_POINT ( 'NONE',  ( 10.81189881249999729, 0.000000000000000000, -185.8437500020483810 ) ) ;
#20848 = CARTESIAN_POINT ( 'NONE',  ( -5.405949406249996869, 9.363379034771805109, -165.8437500020484094 ) ) ;
#20849 = CARTESIAN_POINT ( 'NONE',  ( 10.81189881249999729, 6.242252689847867408, -175.2187500020484094 ) ) ;
#20850 = LINE ( 'NONE', #31012, #13609 ) ;
#20851 = DIRECTION ( 'NONE',  ( -0.000000000000000000, -0.000000000000000000, -1.000000000000000000 ) ) ;
#20852 = CARTESIAN_POINT ( 'NONE',  ( 9.999999999999742428, 5.773502691896404748, -126.3749999999999858 ) ) ;
#20853 = CARTESIAN_POINT ( 'NONE',  ( -4.999999999999996447, 8.660254037844387298, -199.5000000000000000 ) ) ;
#20854 = CARTESIAN_POINT ( 'NONE',  ( 5.405949406249999534, 9.363379034771803333, -110.5937500020483810 ) ) ;
#20855 = CARTESIAN_POINT ( 'NONE',  ( 5.000000000000000000, 8.660254037844385522, -109.7499999999999858 ) ) ;
#20856 = CARTESIAN_POINT ( 'NONE',  ( -10.81189881249999907, -6.242252689847864744, -92.15625000204839523 ) ) ;
#20857 = CARTESIAN_POINT ( 'NONE',  ( -2.293366432827344421E-15, -12.48450537969573659, -97.71875000204838102 ) ) ;
#20858 = CARTESIAN_POINT ( 'NONE',  ( -2.293366432827344421E-15, -12.48450537969573659, -69.21875000204839523 ) ) ;
#20859 = CARTESIAN_POINT ( 'NONE',  ( -5.405949406250003975, -9.363379034771801557, -77.03125000204838102 ) ) ;
#20860 = CARTESIAN_POINT ( 'NONE',  ( 7.070501591499377789E-16, 11.54700538379251284, -155.0000000040968189 ) ) ;
#20861 = CARTESIAN_POINT ( 'NONE',  ( 10.00000000000000000, 5.773502691896255534, -135.3750000000000000 ) ) ;
#20862 = CARTESIAN_POINT ( 'NONE',  ( 5.405949406249992428, -9.363379034771808662, -160.7812500020484094 ) ) ;
#20863 = CARTESIAN_POINT ( 'NONE',  ( 10.81189881249999551, -6.242252689847874514, -174.1562500020484094 ) ) ;
#20864 = CARTESIAN_POINT ( 'NONE',  ( 5.000000000000000000, 8.660254037844385522, -153.6250000040967905 ) ) ;
#20865 = CARTESIAN_POINT ( 'NONE',  ( -9.999999999999998224, 1.224646799147353059E-15, -38.74999999999997868 ) ) ;
#20866 = CARTESIAN_POINT ( 'NONE',  ( 7.644554776091147741E-16, 12.48450537969573659, -105.9687500020483668 ) ) ;
#20867 = CARTESIAN_POINT ( 'NONE',  ( -9.999999999999998224, 1.224646799147353059E-15, -120.1250000040967905 ) ) ;
#20868 = CARTESIAN_POINT ( 'NONE',  ( 9.999999999999996447, -5.773502691896262640, -77.12499999999998579 ) ) ;
#20869 = CARTESIAN_POINT ( 'NONE',  ( 10.81189881249999907, 6.242252689847868297, -1.406250002048359260 ) ) ;
#20870 = CARTESIAN_POINT ( 'NONE',  ( -4.999999999999996447, 8.660254037844387298, -79.87500000409677625 ) ) ;
#20871 = CARTESIAN_POINT ( 'NONE',  ( 5.405949406249999534, 9.363379034771803333, -98.78125000204839523 ) ) ;
#20872 = CARTESIAN_POINT ( 'NONE',  ( 10.81189881249999729, 6.242252689847867408, -80.90625000204839523 ) ) ;
#20873 = CARTESIAN_POINT ( 'NONE',  ( 9.999999999999996447, -5.773502691896262640, -76.00000000409677625 ) ) ;
#20874 = CARTESIAN_POINT ( 'NONE',  ( -5.000000000000003553, -8.660254037844383745, -59.49999999999997158 ) ) ;
#20875 = CARTESIAN_POINT ( 'NONE',  ( 7.644554776091147741E-16, 12.48450537969573659, -32.46875000204835260 ) ) ;
#20876 = VERTEX_POINT ( 'NONE', #40998 ) ;
#20877 = CARTESIAN_POINT ( 'NONE',  ( -10.00000000000000000, -5.773502691896251982, -4.124999999999955591 ) ) ;
#20878 = CARTESIAN_POINT ( 'NONE',  ( 5.405949406249999534, 9.363379034771803333, -29.78125000204837036 ) ) ;
#20879 = CARTESIAN_POINT ( 'NONE',  ( 5.405949406249999534, 9.363379034771803333, -16.09375000204835260 ) ) ;
#20880 = CARTESIAN_POINT ( 'NONE',  ( 4.999999999999992006, -8.660254037844389075, -118.1250000040967905 ) ) ;
#20881 = CARTESIAN_POINT ( 'NONE',  ( -4.999999999999996447, 8.660254037844387298, -0.3750000040967649273 ) ) ;
#20882 = CARTESIAN_POINT ( 'NONE',  ( -5.405949406249996869, 9.363379034771805109, -131.5312500020484094 ) ) ;
#20883 = CARTESIAN_POINT ( 'NONE',  ( -2.121150477449813534E-15, -11.54700538379251284, -179.3750000000000284 ) ) ;
#20884 = DIRECTION ( 'NONE',  ( -0.000000000000000000, -0.000000000000000000, -1.000000000000000000 ) ) ;
#20886 = VERTEX_POINT ( 'NONE', #17694 ) ;
#20885 = CARTESIAN_POINT ( 'NONE',  ( 10.81189881249999729, 0.000000000000000000, -109.5312500020483810 ) ) ;
#20887 = DIRECTION ( 'NONE',  ( -0.000000000000000000, -0.000000000000000000, 1.000000000000000000 ) ) ;
#20888 = EDGE_CURVE ( 'NONE', #30784, #38354, #18850, .T. ) ;
#20889 = ORIENTED_EDGE ( 'NONE', *, *, #6146, .F. ) ;
#20890 = ADVANCED_FACE ( 'NONE', ( #7802 ), #24209, .F. ) ;
#20891 = ORIENTED_EDGE ( 'NONE', *, *, #24376, .T. ) ;
#20892 = CARTESIAN_POINT ( 'NONE',  ( -10.81189881249999907, -6.242252689847864744, -36.65625000204835970 ) ) ;
#20893 = DATE_AND_TIME ( #24373, #26284 ) ;
#20894 = CARTESIAN_POINT ( 'NONE',  ( 10.81189881249999907, 6.242252689847868297, -86.71875000204836681 ) ) ;
#20895 = DIRECTION ( 'NONE',  ( 0.000000000000000000, 0.000000000000000000, -1.000000000000000000 ) ) ;
#20896 = CARTESIAN_POINT ( 'NONE',  ( -10.00000000000051337, 5.773502691895962435, -113.8749999999999858 ) ) ;
#20897 = CARTESIAN_POINT ( 'NONE',  ( -9.999999999999998224, 1.224646799147353059E-15, -33.12500000409676915 ) ) ;
#20898 = CARTESIAN_POINT ( 'NONE',  ( -10.81189881249999729, 6.242252689847871849, -173.4062500020483810 ) ) ;
#20899 = CARTESIAN_POINT ( 'NONE',  ( 9.999999999999998224, 0.000000000000000000, -110.3750000040967763 ) ) ;
#20900 = ADVANCED_FACE ( 'NONE', ( #34133 ), #37785, .F. ) ;
#20901 = CARTESIAN_POINT ( 'NONE',  ( -5.405949406249996869, 9.363379034771805109, -122.3437500020483952 ) ) ;
#20902 = CARTESIAN_POINT ( 'NONE',  ( 7.644554776091147741E-16, 12.48450537969573659, -90.96875000204838102 ) ) ;
#20903 = CARTESIAN_POINT ( 'NONE',  ( 10.81189881249999551, -6.242252689847874514, -3.156250002048347270 ) ) ;
#20904 = CARTESIAN_POINT ( 'NONE',  ( 10.81189881249999729, 0.000000000000000000, -199.3437500020484094 ) ) ;
#20905 = CARTESIAN_POINT ( 'NONE',  ( 7.644554776091147741E-16, 12.48450537969573659, -97.15625000204839523 ) ) ;
#20906 = CARTESIAN_POINT ( 'NONE',  ( -5.000000000000003553, -8.660254037844383745, -181.3750000040967905 ) ) ;
#20907 = CARTESIAN_POINT ( 'NONE',  ( 7.644554776091147741E-16, 12.48450537969573659, -105.9687500020483668 ) ) ;
#20908 = CARTESIAN_POINT ( 'NONE',  ( -10.81189881249999729, -6.242252689847864744, -182.1562500020483810 ) ) ;
#20909 = DIRECTION ( 'NONE',  ( -1.000000000000000000, 0.000000000000000000, 0.000000000000000000 ) ) ;
#20910 = CARTESIAN_POINT ( 'NONE',  ( -10.81189881249999729, 1.324075727343319199E-15, -179.2812500020484094 ) ) ;
#20911 = CARTESIAN_POINT ( 'NONE',  ( -10.81189881249999907, -6.242252689847864744, -195.6562500020484094 ) ) ;
#20912 = CARTESIAN_POINT ( 'NONE',  ( 5.405949406249999534, 9.363379034771803333, -49.09375000204838102 ) ) ;
#20913 = CARTESIAN_POINT ( 'NONE',  ( 5.405949406249999534, 9.363379034771803333, -44.59375000204837391 ) ) ;
#20914 = CARTESIAN_POINT ( 'NONE',  ( -4.999999999999996447, 8.660254037844387298, -172.8750000040968189 ) ) ;
#20915 = CARTESIAN_POINT ( 'NONE',  ( 10.81189881249999729, 0.000000000000000000, -9.031250002048352599 ) ) ;
#20916 = CARTESIAN_POINT ( 'NONE',  ( -10.81189881249999729, 1.324075727343319199E-15, -18.59375000204835260 ) ) ;
#20917 = CARTESIAN_POINT ( 'NONE',  ( -10.00000000000051337, 5.773502691895962435, -145.3750000000000000 ) ) ;
#20918 = CARTESIAN_POINT ( 'NONE',  ( -2.293366432827344421E-15, -12.48450537969573659, -132.2187500020483810 ) ) ;
#20919 = CARTESIAN_POINT ( 'NONE',  ( 5.000000000000000000, 8.660254037844385522, -97.74999999999998579 ) ) ;
#20920 = CARTESIAN_POINT ( 'NONE',  ( -5.405949406250003975, -9.363379034771801557, -26.03125000204836681 ) ) ;
#20921 = CARTESIAN_POINT ( 'NONE',  ( -10.00000000000000000, -5.773502691896251982, -114.0000000040967905 ) ) ;
#20922 = ADVANCED_FACE ( 'NONE', ( #8448 ), #1325, .F. ) ;
#20923 = CARTESIAN_POINT ( 'NONE',  ( -10.00000000000025580, 5.773502691896109873, -101.8750000000000000 ) ) ;
#20924 = CARTESIAN_POINT ( 'NONE',  ( 9.999999999999998224, 0.000000000000000000, -60.49999999999997158 ) ) ;
#20925 = CARTESIAN_POINT ( 'NONE',  ( -10.81189881249999729, 1.324075727343319199E-15, -123.7812500020483952 ) ) ;
#20926 = CARTESIAN_POINT ( 'NONE',  ( 10.81189881249999729, 0.000000000000000000, -111.0312500020483810 ) ) ;
#20927 = ORIENTED_EDGE ( 'NONE', *, *, #9831, .T. ) ;
#20928 = CARTESIAN_POINT ( 'NONE',  ( -9.999999999999479527, -5.773502691896549521, -145.1250000000000000 ) ) ;
#20929 = CARTESIAN_POINT ( 'NONE',  ( -9.999999999999998224, 5.773502691896259087, -99.25000000409677625 ) ) ;
#20930 = CARTESIAN_POINT ( 'NONE',  ( -9.999999999999998224, 1.224646799147353059E-15, -151.6250000040967905 ) ) ;
#20931 = CARTESIAN_POINT ( 'NONE',  ( 10.81189881249999729, 0.000000000000000000, -163.5312500020484094 ) ) ;
#20932 = CARTESIAN_POINT ( 'NONE',  ( -5.405949406250003975, -9.363379034771801557, -55.84375000204835970 ) ) ;
#20933 = ORIENTED_EDGE ( 'NONE', *, *, #18864, .F. ) ;
#20934 = CARTESIAN_POINT ( 'NONE',  ( 7.070501591499377789E-16, 11.54700538379251284, -25.62499999999997513 ) ) ;
#20935 = CARTESIAN_POINT ( 'NONE',  ( 5.405949406249999534, 9.363379034771803333, -37.28125000204837391 ) ) ;
#20936 = CARTESIAN_POINT ( 'NONE',  ( 10.00000000000000000, 5.773502691896255534, -160.8750000000000000 ) ) ;
#20937 = CARTESIAN_POINT ( 'NONE',  ( -2.121150477449813534E-15, -11.54700538379251284, -92.37500000000000000 ) ) ;
#20938 =( BOUNDED_CURVE ( )  B_SPLINE_CURVE ( 2, ( #9574, #9787, #29651, #93, #23169, #37610, #33535 ),
 .UNSPECIFIED., .F., .F. ) 
 B_SPLINE_CURVE_WITH_KNOTS ( ( 3, 2, 2, 3 ),
 ( 0.4850746268656717652, 0.4863184079601990950, 0.4875621890547264248, 0.4888059701492538101 ),
 .UNSPECIFIED. ) 
 CURVE ( )  GEOMETRIC_REPRESENTATION_ITEM ( )  RATIONAL_B_SPLINE_CURVE ( ( 0.9999999999999880096, 0.8660254037844506980, 1.000000000000000000, 0.8660254037844387076, 1.000000000000000000, 0.8660254037844327124, 1.000000000000005995 ) ) 
 REPRESENTATION_ITEM ( '' )  );
#20939 = CARTESIAN_POINT ( 'NONE',  ( 4.999999999999992006, -8.660254037844389075, -25.12500000409675849 ) ) ;
#20940 = DIRECTION ( 'NONE',  ( -0.000000000000000000, -0.000000000000000000, 1.000000000000000000 ) ) ;
#20941 = CARTESIAN_POINT ( 'NONE',  ( -10.81189881249999907, -6.242252689847864744, -137.1562500020483810 ) ) ;
#20942 = CARTESIAN_POINT ( 'NONE',  ( 3.989097665506361245, 9.623024927554942209, -1.486633740873807397E-14 ) ) ;
#20943 = EDGE_CURVE ( 'NONE', #419, #21453, #1786, .T. ) ;
#20944 = CARTESIAN_POINT ( 'NONE',  ( -9.999999999999998224, 1.224646799147353059E-15, -166.6250000040967905 ) ) ;
#20945 = ORIENTED_EDGE ( 'NONE', *, *, #39140, .T. ) ;
#20946 = EDGE_CURVE ( 'NONE', #37673, #38469, #11229, .T. ) ;
#20947 = ADVANCED_FACE ( 'NONE', ( #8014 ), #33919, .F. ) ;
#20949 = EDGE_LOOP ( 'NONE', ( #36400, #13631, #34541, #2725 ) ) ;
#20948 = EDGE_LOOP ( 'NONE', ( #5755, #38517, #8544, #5395 ) ) ;
#20950 = CARTESIAN_POINT ( 'NONE',  ( -99.99999999999994316, 39.99999999999999289, -160.0000000000000000 ) ) ;
#20951 = CARTESIAN_POINT ( 'NONE',  ( -2.121150477449813534E-15, -11.54700538379251284, -134.3750000000000000 ) ) ;
#20952 = CARTESIAN_POINT ( 'NONE',  ( -10.81189881249999729, 1.324075727343319199E-15, -162.5937500020484094 ) ) ;
#20953 = CARTESIAN_POINT ( 'NONE',  ( 5.405949406249992428, -9.363379034771808662, -196.7812500020484094 ) ) ;
#20954 = CARTESIAN_POINT ( 'NONE',  ( 10.81189881249999551, -6.242252689847874514, -14.96875000204837036 ) ) ;
#20955 = CARTESIAN_POINT ( 'NONE',  ( -9.999999999999996447, 5.773502691896259975, -170.8750000000000000 ) ) ;
#20956 = CARTESIAN_POINT ( 'NONE',  ( 10.81189881249999729, 6.242252689847867408, -146.7187500020484094 ) ) ;
#20957 = CARTESIAN_POINT ( 'NONE',  ( 7.644554776091147741E-16, 12.48450537969573659, -137.4687500020483810 ) ) ;
#20958 = CARTESIAN_POINT ( 'NONE',  ( 10.81189881249999907, 6.242252689847868297, -103.4062500020483952 ) ) ;
#20959 = CARTESIAN_POINT ( 'NONE',  ( 5.405949406249992428, -9.363379034771808662, -117.0937500020483810 ) ) ;
#20960 = CARTESIAN_POINT ( 'NONE',  ( -5.000000000000003553, -8.660254037844383745, -196.3750000040967905 ) ) ;
#20961 = CARTESIAN_POINT ( 'NONE',  ( 10.81189881249999907, 6.242252689847868297, -122.9062500020484094 ) ) ;
#20962 = CARTESIAN_POINT ( 'NONE',  ( 7.070501591499377789E-16, 11.54700538379251284, -198.5000000040968189 ) ) ;
#20964 = ADVANCED_FACE ( 'NONE', ( #22241 ), #8868, .T. ) ;
#20963 = CARTESIAN_POINT ( 'NONE',  ( -10.81189881249999729, 6.242252689847871849, -134.2187500020483810 ) ) ;
#20965 = CARTESIAN_POINT ( 'NONE',  ( -9.999999999999998224, 1.224646799147353059E-15, -200.0000000000000000 ) ) ;
#20966 = CARTESIAN_POINT ( 'NONE',  ( 5.000000000000000000, 8.660254037844385522, -157.7500000000000000 ) ) ;
#20967 = CARTESIAN_POINT ( 'NONE',  ( -10.00000000000000000, -5.773502691896251982, -23.62499999999997868 ) ) ;
#20968 = CARTESIAN_POINT ( 'NONE',  ( 5.405949406249992428, -9.363379034771808662, -79.59375000204838102 ) ) ;
#20969 = CARTESIAN_POINT ( 'NONE',  ( -2.293366432827344421E-15, -12.48450537969573659, -66.21875000204836681 ) ) ;
#20970 = FACE_OUTER_BOUND ( 'NONE', #27807, .T. ) ;
#20971 = CARTESIAN_POINT ( 'NONE',  ( -2.293366432827344421E-15, -12.48450537969573659, -36.40625000204835970 ) ) ;
#20972 = CARTESIAN_POINT ( 'NONE',  ( -10.81189881249999729, 1.324075727343319199E-15, -45.59375000204838102 ) ) ;
#20973 = CARTESIAN_POINT ( 'NONE',  ( 10.00000000000076916, -5.773502691895816774, -110.5000000040967763 ) ) ;
#20974 = CARTESIAN_POINT ( 'NONE',  ( -10.81189881249999729, 6.242252689847871849, -156.7187500020483810 ) ) ;
#20975 = CARTESIAN_POINT ( 'NONE',  ( 9.999999999999996447, -5.773502691896262640, -122.1250000000000000 ) ) ;
#20976 = CARTESIAN_POINT ( 'NONE',  ( 5.405949406249999534, 9.363379034771803333, -130.2812500020483810 ) ) ;
#20977 = CARTESIAN_POINT ( 'NONE',  ( 9.999999999999479527, 5.773502691896553074, -94.87499999999997158 ) ) ;
#20978 = CARTESIAN_POINT ( 'NONE',  ( -9.999999999999998224, 1.224646799147353059E-15, -86.74999999999998579 ) ) ;
#20979 = CARTESIAN_POINT ( 'NONE',  ( -5.405949406249996869, 9.363379034771805109, -14.53125000204835615 ) ) ;
#20980 = EDGE_LOOP ( 'NONE', ( #18453, #31809, #32746, #10165 ) ) ;
#20981 =( BOUNDED_CURVE ( )  B_SPLINE_CURVE ( 2, ( #17877, #13568, #7335, #10342, #34313, #10767, #23956 ),
 .UNSPECIFIED., .F., .F. ) 
 B_SPLINE_CURVE_WITH_KNOTS ( ( 3, 2, 2, 3 ),
 ( 0.08955223880597024122, 0.09079601990049755711, 0.09203980099502487300, 0.09328358208955218889 ),
 .UNSPECIFIED. ) 
 CURVE ( )  GEOMETRIC_REPRESENTATION_ITEM ( )  RATIONAL_B_SPLINE_CURVE ( ( 0.9999999999999895639, 0.8660254037844491437, 1.000000000000000000, 0.8660254037844387076, 1.000000000000000000, 0.8660254037844447028, 0.9999999999999940048 ) ) 
 REPRESENTATION_ITEM ( '' )  );
#20982 = CARTESIAN_POINT ( 'NONE',  ( 7.644554776091147741E-16, 12.48450537969573659, -106.1562500020483810 ) ) ;
#20983 = CARTESIAN_POINT ( 'NONE',  ( 9.999999999999998224, 0.000000000000000000, -120.8750000040967905 ) ) ;
#20984 = CARTESIAN_POINT ( 'NONE',  ( -9.999999999999998224, 1.224646799147353059E-15, -180.1250000040968189 ) ) ;
#20985 = CARTESIAN_POINT ( 'NONE',  ( 7.070501591499377789E-16, 11.54700538379251284, -32.00000000409674783 ) ) ;
#20986 = CARTESIAN_POINT ( 'NONE',  ( -4.999999999999996447, 8.660254037844387298, -148.5000000000000000 ) ) ;
#20987 = CARTESIAN_POINT ( 'NONE',  ( -10.81189881249999907, -6.242252689847864744, -42.65625000204836681 ) ) ;
#20988 =( BOUNDED_CURVE ( )  B_SPLINE_CURVE ( 2, ( #7581, #4992, #33704, #24642, #7803, #17695, #37786 ),
 .UNSPECIFIED., .F., .F. ) 
 B_SPLINE_CURVE_WITH_KNOTS ( ( 3, 2, 2, 3 ),
 ( 0.7126865671641793298, 0.7139303482587067151, 0.7151741293532342114, 0.7164179104477614857 ),
 .UNSPECIFIED. ) 
 CURVE ( )  GEOMETRIC_REPRESENTATION_ITEM ( )  RATIONAL_B_SPLINE_CURVE ( ( 0.9999999999999761302, 0.8660254037844625774, 1.000000000000000000, 0.8660254037844387076, 1.000000000000000000, 0.8660254037844028474, 1.000000000000035971 ) ) 
 REPRESENTATION_ITEM ( '' )  );
#20989 = CARTESIAN_POINT ( 'NONE',  ( 4.999999999999992006, -8.660254037844389075, -40.12500000409676915 ) ) ;
#20990 = CARTESIAN_POINT ( 'NONE',  ( -10.81189881249999729, 1.324075727343319199E-15, -153.7812500020484094 ) ) ;
#20991 = CARTESIAN_POINT ( 'NONE',  ( 10.81189881249999551, -6.242252689847874514, -130.4687500020483810 ) ) ;
#20992 = CARTESIAN_POINT ( 'NONE',  ( 7.070501591499376803E-16, 11.54700538379251284, -165.5000000040967905 ) ) ;
#20993 = ORIENTED_EDGE ( 'NONE', *, *, #15632, .T. ) ;
#20994 = CARTESIAN_POINT ( 'NONE',  ( -9.999999999999998224, 0.000000000000000000, -99.99999999999998579 ) ) ;
#20995 = ORIENTED_EDGE ( 'NONE', *, *, #7249, .T. ) ;
#20996 = ORIENTED_EDGE ( 'NONE', *, *, #12691, .F. ) ;
#20998 = ORIENTED_EDGE ( 'NONE', *, *, #32021, .F. ) ;
#20997 = CARTESIAN_POINT ( 'NONE',  ( 10.81189881249999729, 0.000000000000000000, -110.8437500020483810 ) ) ;
#20999 = CARTESIAN_POINT ( 'NONE',  ( 9.999999999999998224, 0.000000000000000000, -200.0000000000000000 ) ) ;
#21000 = CARTESIAN_POINT ( 'NONE',  ( 10.81189881249999551, -6.242252689847874514, -190.4687500020484094 ) ) ;
#21002 = ADVANCED_FACE ( 'NONE', ( #32179 ), #2398, .T. ) ;
#21001 = CARTESIAN_POINT ( 'NONE',  ( 5.405949406249992428, -9.363379034771808662, -40.59375000204837391 ) ) ;
#21003 = CARTESIAN_POINT ( 'NONE',  ( 3.768369288276942619, -9.903100897459154339, -1.167351363741238987E-15 ) ) ;
#21004 = CARTESIAN_POINT ( 'NONE',  ( 9.999999999999998224, 0.000000000000000000, -30.87500000409676559 ) ) ;
#21005 = CARTESIAN_POINT ( 'NONE',  ( 5.405949406249999534, 9.363379034771803333, -169.0937500020484094 ) ) ;
#21006 = CARTESIAN_POINT ( 'NONE',  ( -10.81189881249999729, 6.242252689847871849, -161.2187500020483526 ) ) ;
#21007 = CARTESIAN_POINT ( 'NONE',  ( -9.999999999999998224, 1.224646799147353059E-15, -93.12500000409677625 ) ) ;
#21008 = CARTESIAN_POINT ( 'NONE',  ( 5.405949406249999534, 9.363379034771803333, -145.0937500020483810 ) ) ;
#21009 = CARTESIAN_POINT ( 'NONE',  ( -10.81189881249999729, 1.324075727343319199E-15, -150.7812500020483810 ) ) ;
#21010 = CARTESIAN_POINT ( 'NONE',  ( 10.81189881249999551, -6.242252689847874514, -151.4687500020484094 ) ) ;
#21011 = DIRECTION ( 'NONE',  ( -1.000000000000000000, 0.000000000000000000, 0.000000000000000000 ) ) ;
#21012 = CARTESIAN_POINT ( 'NONE',  ( 5.000000000000000000, 8.660254037844385522, -180.2500000000000284 ) ) ;
#21013 = CARTESIAN_POINT ( 'NONE',  ( 10.81189881249999551, -6.242252689847874514, -85.46875000204836681 ) ) ;
#21014 = CARTESIAN_POINT ( 'NONE',  ( -1.470112319795894296, 10.71737856626141827, -100.0000000000000142 ) ) ;
#21015 = CARTESIAN_POINT ( 'NONE',  ( -2.293366432827344421E-15, -12.48450537969573659, -60.40625000204839523 ) ) ;
#21016 = CARTESIAN_POINT ( 'NONE',  ( 0.000000000000000000, 0.000000000000000000, -223.0000000000000000 ) ) ;
#21017 = CARTESIAN_POINT ( 'NONE',  ( 10.81189881249999907, 6.242252689847868297, -181.2187500020484094 ) ) ;
#21018 = CARTESIAN_POINT ( 'NONE',  ( 5.405949406249999534, 9.363379034771803333, -115.2812500020483952 ) ) ;
#21019 = CARTESIAN_POINT ( 'NONE',  ( 10.81189881249999729, 6.242252689847867408, -151.4062500020484094 ) ) ;
#21020 = CARTESIAN_POINT ( 'NONE',  ( 5.405949406249999534, 9.363379034771803333, -44.78125000204838102 ) ) ;
#21021 = CARTESIAN_POINT ( 'NONE',  ( 9.999999999999996447, -5.773502691896262640, -128.5000000040967905 ) ) ;
#21022 = CARTESIAN_POINT ( 'NONE',  ( -2.121150477449813534E-15, -11.54700538379251284, -110.3749999999999858 ) ) ;
#21023 = ORIENTED_EDGE ( 'NONE', *, *, #11679, .F. ) ;
#21024 = AXIS2_PLACEMENT_3D ( 'NONE', #15242, #1894, #28222 ) ;
#21025 = CARTESIAN_POINT ( 'NONE',  ( 10.81189881249999729, 6.242252689847867408, -128.9062500020483810 ) ) ;
#21026 = CARTESIAN_POINT ( 'NONE',  ( 9.999999999999996447, -5.773502691896262640, -145.0000000040967905 ) ) ;
#21027 = CARTESIAN_POINT ( 'NONE',  ( 9.999999999999998224, 0.000000000000000000, -167.0000000000000000 ) ) ;
#21028 = CARTESIAN_POINT ( 'NONE',  ( -10.81189881249999729, 1.324075727343319199E-15, -179.2812500020484094 ) ) ;
#21029 = ORIENTED_EDGE ( 'NONE', *, *, #2242, .F. ) ;
#21030 = CARTESIAN_POINT ( 'NONE',  ( -2.121150477449813534E-15, -11.54700538379251284, -53.37499999999997868 ) ) ;
#21031 = CARTESIAN_POINT ( 'NONE',  ( -10.81189881249999729, 1.324075727343319199E-15, -170.0937500020484094 ) ) ;
#21032 = CARTESIAN_POINT ( 'NONE',  ( 5.000000000000000000, 8.660254037844385522, -56.12500000409676204 ) ) ;
#21033 = CARTESIAN_POINT ( 'NONE',  ( -5.000000000000003553, -8.660254037844383745, -18.99999999999996092 ) ) ;
#21034 = CARTESIAN_POINT ( 'NONE',  ( 0.000000000000000000, 0.000000000000000000, -99.99999999999998579 ) ) ;
#21035 = CARTESIAN_POINT ( 'NONE',  ( -10.81189881249999729, 1.324075727343319199E-15, -77.28125000204838102 ) ) ;
#21036 = CARTESIAN_POINT ( 'NONE',  ( -10.81189881249999729, -6.242252689847864744, -48.65625000204837391 ) ) ;
#21037 = CARTESIAN_POINT ( 'NONE',  ( 4.999999999999992006, -8.660254037844389075, -50.62500000409675494 ) ) ;
#21038 = CARTESIAN_POINT ( 'NONE',  ( -10.81189881249999907, -6.242252689847864744, -10.96875000204835970 ) ) ;
#21039 = CARTESIAN_POINT ( 'NONE',  ( 10.00000000000051159, -5.773502691895965988, -35.12499999999995026 ) ) ;
#21040 = CARTESIAN_POINT ( 'NONE',  ( 5.405949406249999534, 9.363379034771803333, -178.2812500020484094 ) ) ;
#21041 = DIRECTION ( 'NONE',  ( -0.000000000000000000, -0.000000000000000000, -1.000000000000000000 ) ) ;
#21042 = CARTESIAN_POINT ( 'NONE',  ( 7.071067811865472841, -7.071067811865472841, -200.0000000000000000 ) ) ;
#21043 = CARTESIAN_POINT ( 'NONE',  ( 7.070501591499376803E-16, 11.54700538379251284, -117.1249999999999858 ) ) ;
#21044 = LINE ( 'NONE', #14767, #1101 ) ;
#21045 = CARTESIAN_POINT ( 'NONE',  ( -5.000000000000003553, -8.660254037844383745, -163.3750000040967905 ) ) ;
#21047 = ORIENTED_EDGE ( 'NONE', *, *, #41656, .F. ) ;
#21046 = CARTESIAN_POINT ( 'NONE',  ( -2.293366432827344421E-15, -12.48450537969573659, -87.40625000204838102 ) ) ;
#21048 =( NAMED_UNIT ( * ) SI_UNIT ( $, .STERADIAN. ) SOLID_ANGLE_UNIT ( ) );
#21050 = ORIENTED_EDGE ( 'NONE', *, *, #19327, .T. ) ;
#21049 = CARTESIAN_POINT ( 'NONE',  ( -10.00000000000051337, 5.773502691895962435, -91.75000000409676204 ) ) ;
#21051 =( BOUNDED_CURVE ( )  B_SPLINE_CURVE ( 2, ( #32869, #12567, #39119, #35687, #32453, #6956, #20113 ),
 .UNSPECIFIED., .F., .F. ) 
 B_SPLINE_CURVE_WITH_KNOTS ( ( 3, 2, 2, 3 ),
 ( 0.2835820895522389029, 0.2848258706467662882, 0.2860696517412936180, 0.2873134328358210032 ),
 .UNSPECIFIED. ) 
 CURVE ( )  GEOMETRIC_REPRESENTATION_ITEM ( )  RATIONAL_B_SPLINE_CURVE ( ( 0.9999999999999880096, 0.8660254037844506980, 1.000000000000000000, 0.8660254037844387076, 1.000000000000000000, 0.8660254037844267172, 1.000000000000011990 ) ) 
 REPRESENTATION_ITEM ( '' )  );
#21052 = ORIENTED_EDGE ( 'NONE', *, *, #7755, .F. ) ;
#21053 = CARTESIAN_POINT ( 'NONE',  ( 5.405949406249999534, 9.363379034771803333, -37.09375000204836681 ) ) ;
#21054 = CARTESIAN_POINT ( 'NONE',  ( -10.81189881249999729, 6.242252689847871849, -29.21875000204835615 ) ) ;
#21055 = CARTESIAN_POINT ( 'NONE',  ( 10.81189881249999729, 0.000000000000000000, -12.03125000204835438 ) ) ;
#21056 = CARTESIAN_POINT ( 'NONE',  ( -10.81189881249999729, 1.324075727343319199E-15, -63.59375000204836681 ) ) ;
#21057 = CARTESIAN_POINT ( 'NONE',  ( 5.000000000000000000, 8.660254037844385522, -93.24999999999998579 ) ) ;
#21058 = CARTESIAN_POINT ( 'NONE',  ( -10.00000000000000000, -5.773502691896251982, -44.62499999999997158 ) ) ;
#21059 = CARTESIAN_POINT ( 'NONE',  ( -5.405949406250003975, -9.363379034771801557, -184.8437500020483810 ) ) ;
#21060 = CARTESIAN_POINT ( 'NONE',  ( 5.405949406249992428, -9.363379034771808662, -162.0937500020484094 ) ) ;
#21061 = LINE ( 'NONE', #31230, #16455 ) ;
#21062 = CARTESIAN_POINT ( 'NONE',  ( -9.999999999999483080, -5.773502691897144601, -100.1249999999999574 ) ) ;
#21063 = DIRECTION ( 'NONE',  ( -0.000000000000000000, -0.000000000000000000, -1.000000000000000000 ) ) ;
#21064 = CARTESIAN_POINT ( 'NONE',  ( -9.999999999999998224, 1.224646799147353059E-15, -103.6250000040967763 ) ) ;
#21065 = FACE_OUTER_BOUND ( 'NONE', #6769, .T. ) ;
#21066 = CARTESIAN_POINT ( 'NONE',  ( 5.405949406249992428, -9.363379034771808662, -111.0937500020483810 ) ) ;
#21067 = FACE_OUTER_BOUND ( 'NONE', #42073, .T. ) ;
#21068 = CARTESIAN_POINT ( 'NONE',  ( 10.81189881249999729, 0.000000000000000000, -81.03125000204839523 ) ) ;
#21069 = CARTESIAN_POINT ( 'NONE',  ( 5.405949406249992428, -9.363379034771808662, -100.5937500020483810 ) ) ;
#21070 = ADVANCED_FACE ( 'NONE', ( #15527 ), #15322, .T. ) ;
#21071 = CARTESIAN_POINT ( 'NONE',  ( 7.644554776091147741E-16, 12.48450537969573659, -60.96875000204838102 ) ) ;
#21072 = VECTOR ( 'NONE', #24049, 1000.000000000000114 ) ;
#21073 = CARTESIAN_POINT ( 'NONE',  ( 10.81189881249999551, -6.242252689847874514, -64.65625000204839523 ) ) ;
#21074 = CARTESIAN_POINT ( 'NONE',  ( -2.121150477449813534E-15, -11.54700538379251284, -155.7500000040967620 ) ) ;
#21075 = CARTESIAN_POINT ( 'NONE',  ( 7.070501591499377789E-16, 11.54700538379251284, -130.6250000000000000 ) ) ;
#21076 = VECTOR ( 'NONE', #37454, 1000.000000000000000 ) ;
#21077 = CARTESIAN_POINT ( 'NONE',  ( 10.81189881249999551, -6.242252689847874514, -147.1562500020484379 ) ) ;
#21078 = CARTESIAN_POINT ( 'NONE',  ( 10.81189881249999907, 6.242252689847868297, -163.4062500020484094 ) ) ;
#21079 = CARTESIAN_POINT ( 'NONE',  ( -5.000000000000003553, -8.660254037844383745, -145.3750000040967905 ) ) ;
#21080 = CARTESIAN_POINT ( 'NONE',  ( -9.999999999999998224, 1.224646799147353059E-15, -197.7500000000000000 ) ) ;
#21081 = CARTESIAN_POINT ( 'NONE',  ( 10.81189881249999551, -6.242252689847874514, -95.96875000204838102 ) ) ;
#21082 = DIRECTION ( 'NONE',  ( -0.000000000000000000, -0.000000000000000000, 1.000000000000000000 ) ) ;
#21083 = CARTESIAN_POINT ( 'NONE',  ( 4.999999999999992006, -8.660254037844389075, -69.74999999999997158 ) ) ;
#21084 = CARTESIAN_POINT ( 'NONE',  ( -10.81189881249999729, 1.324075727343319199E-15, -0.7812500020483725827 ) ) ;
#21085 = CARTESIAN_POINT ( 'NONE',  ( -9.999999999999998224, 5.773502691896259087, -84.25000000409677625 ) ) ;
#21086 = CARTESIAN_POINT ( 'NONE',  ( 4.162302680423837664, -9.761226838701102082, -180.0000000000000284 ) ) ;
#21087 = CARTESIAN_POINT ( 'NONE',  ( -2.293366432827344421E-15, -12.48450537969573659, -97.90625000204839523 ) ) ;
#21088 = CARTESIAN_POINT ( 'NONE',  ( 10.81189881249999729, 6.242252689847867408, -74.90625000204836681 ) ) ;
#21089 = CARTESIAN_POINT ( 'NONE',  ( -10.00000000000000000, -5.773502691896251982, -78.00000000409677625 ) ) ;
#21090 = CARTESIAN_POINT ( 'NONE',  ( -4.999999999999996447, 8.660254037844387298, -135.0000000000000000 ) ) ;
#21091 = CARTESIAN_POINT ( 'NONE',  ( -10.81189881249999729, 1.324075727343319199E-15, -35.09375000204836681 ) ) ;
#21092 = ORIENTED_EDGE ( 'NONE', *, *, #40401, .F. ) ;
#21093 = CARTESIAN_POINT ( 'NONE',  ( 9.999999999999996447, -5.773502691896262640, -5.124999999999960032 ) ) ;
#21094 = CARTESIAN_POINT ( 'NONE',  ( 7.644554776091147741E-16, 12.48450537969573659, -29.65625000204835615 ) ) ;
#21095 = CARTESIAN_POINT ( 'NONE',  ( 10.81189881249999729, 0.000000000000000000, -16.34375000204835260 ) ) ;
#21096 = CARTESIAN_POINT ( 'NONE',  ( 10.00000000000051159, -5.773502691895965988, -94.00000000409677625 ) ) ;
#21097 = CARTESIAN_POINT ( 'NONE',  ( -4.999999999999996447, 8.660254037844387298, -4.875000004096769146 ) ) ;
#21098 = CARTESIAN_POINT ( 'NONE',  ( -5.405949406249996869, 9.363379034771805109, -130.0312500020484094 ) ) ;
#21099 =( BOUNDED_CURVE ( )  B_SPLINE_CURVE ( 2, ( #33946, #24232, #37383, #7826, #36950, #20973, #17081 ),
 .UNSPECIFIED., .F., .F. ) 
 B_SPLINE_CURVE_WITH_KNOTS ( ( 3, 2, 2, 3 ),
 ( 0.4365671641791046276, 0.4378109452736320129, 0.4390547263681593981, 0.4402985074626867279 ),
 .UNSPECIFIED. ) 
 CURVE ( )  GEOMETRIC_REPRESENTATION_ITEM ( )  RATIONAL_B_SPLINE_CURVE ( ( 0.9999999999999820144, 0.8660254037844566932, 1.000000000000000000, 0.8660254037844387076, 1.000000000000000000, 0.8660254037844207220, 1.000000000000017986 ) ) 
 REPRESENTATION_ITEM ( '' )  );
#21100 = CARTESIAN_POINT ( 'NONE',  ( -2.121150477449813534E-15, -11.54700538379251284, -182.3750000000000000 ) ) ;
#21101 = LINE ( 'NONE', #21316, #37196 ) ;
#21103 = ORIENTED_EDGE ( 'NONE', *, *, #23720, .F. ) ;
#21102 = CARTESIAN_POINT ( 'NONE',  ( -10.81189881249999907, -6.242252689847864744, -107.1562500020483952 ) ) ;
#21104 = LINE ( 'NONE', #17856, #8331 ) ;
#21105 = ORIENTED_EDGE ( 'NONE', *, *, #4603, .T. ) ;
#21106 = VERTEX_POINT ( 'NONE', #2608 ) ;
#21107 = CARTESIAN_POINT ( 'NONE',  ( 10.81189881249999729, 0.000000000000000000, -37.53125000204838102 ) ) ;
#21108 = COORDINATED_UNIVERSAL_TIME_OFFSET ( 6, 0, .AHEAD. ) ;
#21109 = CARTESIAN_POINT ( 'NONE',  ( 7.644554776091147741E-16, 12.48450537969573659, -84.96875000204835260 ) ) ;
#21110 = PLANE ( 'NONE',  #7735 ) ;
#21111 = CARTESIAN_POINT ( 'NONE',  ( 0.000000000000000000, 0.000000000000000000, -200.0000000000000000 ) ) ;
#21112 = CARTESIAN_POINT ( 'NONE',  ( -10.00000000000025580, 5.773502691896109873, -122.8750000000000000 ) ) ;
#21113 = CARTESIAN_POINT ( 'NONE',  ( 10.81189881249999551, -6.242252689847874514, -160.6562500020484379 ) ) ;
#21114 = DIRECTION ( 'NONE',  ( -0.000000000000000000, -0.000000000000000000, 1.000000000000000000 ) ) ;
#21115 = CARTESIAN_POINT ( 'NONE',  ( 5.405949406249999534, 9.363379034771803333, -127.0937500020483668 ) ) ;
#21116 = CARTESIAN_POINT ( 'NONE',  ( -10.81189881249999729, 1.324075727343319199E-15, -90.59375000204838102 ) ) ;
#21117 = CARTESIAN_POINT ( 'NONE',  ( 10.81189881249999729, 0.000000000000000000, -0.03125000204837191653 ) ) ;
#21118 = CARTESIAN_POINT ( 'NONE',  ( 10.81189881249999729, 0.000000000000000000, -197.8437500020484094 ) ) ;
#21119 = CARTESIAN_POINT ( 'NONE',  ( 10.81189881249999551, -6.242252689847874514, -99.15625000204838102 ) ) ;
#21120 = CARTESIAN_POINT ( 'NONE',  ( -10.00000000000000000, -5.773502691896251982, -178.5000000040967905 ) ) ;
#21121 = CARTESIAN_POINT ( 'NONE',  ( -10.81189881249999729, 6.242252689847871849, -105.7187500020483668 ) ) ;
#21122 = CARTESIAN_POINT ( 'NONE',  ( -10.81189881249999729, 6.242252689847871849, -174.9062500020484094 ) ) ;
#21123 = CARTESIAN_POINT ( 'NONE',  ( -9.999999999999998224, 1.224646799147353059E-15, -109.6250000040967763 ) ) ;
#21124 = CARTESIAN_POINT ( 'NONE',  ( -10.00000000000025580, 5.773502691896109873, -121.7500000040967905 ) ) ;
#21125 = CARTESIAN_POINT ( 'NONE',  ( 9.999999999999998224, 0.000000000000000000, -0.4999999999999726885 ) ) ;
#21126 = CARTESIAN_POINT ( 'NONE',  ( -5.405949406250003975, -9.363379034771801557, -48.34375000204838102 ) ) ;
#21127 = CARTESIAN_POINT ( 'NONE',  ( -9.999999999999998224, 5.773502691896259087, -171.2500000040967905 ) ) ;
#21128 = CARTESIAN_POINT ( 'NONE',  ( 7.644554776091147741E-16, 12.48450537969573659, -13.15625000204836148 ) ) ;
#21129 = CARTESIAN_POINT ( 'NONE',  ( 10.81189881249999729, 0.000000000000000000, -22.34375000204835615 ) ) ;
#21130 = DIRECTION ( 'NONE',  ( -0.000000000000000000, -0.000000000000000000, 1.000000000000000000 ) ) ;
#21131 = CARTESIAN_POINT ( 'NONE',  ( -10.81189881249999729, 1.324075727343319199E-15, -131.0937500020483810 ) ) ;
#21132 = ADVANCED_FACE ( 'NONE', ( #19201 ), #16151, .T. ) ;
#21133 = CARTESIAN_POINT ( 'NONE',  ( -9.999999999999998224, 5.773502691896259087, -94.37499999999998579 ) ) ;
#21134 = CARTESIAN_POINT ( 'NONE',  ( 10.81189881249999907, 6.242252689847868297, -29.90625000204835970 ) ) ;
#21135 = CARTESIAN_POINT ( 'NONE',  ( 9.999999999999998224, 0.000000000000000000, -104.3750000040967763 ) ) ;
#21136 = CARTESIAN_POINT ( 'NONE',  ( 9.999999999999998224, 0.000000000000000000, -168.5000000000000000 ) ) ;
#21137 = EDGE_CURVE ( 'NONE', #34823, #6210, #39762, .T. ) ;
#21138 = CARTESIAN_POINT ( 'NONE',  ( -9.999999999999998224, 5.773502691896259087, -49.37499999999997868 ) ) ;
#21139 = CARTESIAN_POINT ( 'NONE',  ( -2.293366432827344421E-15, -12.48450537969573659, -124.9062500020483810 ) ) ;
#21140 = CARTESIAN_POINT ( 'NONE',  ( 7.644554776091147741E-16, 12.48450537969573659, -97.15625000204839523 ) ) ;
#21141 = ORIENTED_EDGE ( 'NONE', *, *, #33499, .T. ) ;
#21142 = CARTESIAN_POINT ( 'NONE',  ( -9.999999999999998224, 5.773502691896259087, -97.75000000409677625 ) ) ;
#21143 = LINE ( 'NONE', #8211, #40146 ) ;
#21144 = CARTESIAN_POINT ( 'NONE',  ( -10.81189881249999907, -6.242252689847864744, -161.1562500020484094 ) ) ;
#21145 = CARTESIAN_POINT ( 'NONE',  ( 5.405949406249992428, -9.363379034771808662, -60.09375000204835970 ) ) ;
#21146 = VERTEX_POINT ( 'NONE', #38213 ) ;
#21147 = CARTESIAN_POINT ( 'NONE',  ( 9.999999999999998224, 0.000000000000000000, -22.99999999999996447 ) ) ;
#21148 = CARTESIAN_POINT ( 'NONE',  ( 5.405949406249992428, -9.363379034771808662, -33.28125000204837391 ) ) ;
#21149 = CARTESIAN_POINT ( 'NONE',  ( -5.000000000000003553, -8.660254037844383745, -160.0000000000000000 ) ) ;
#21150 = DIRECTION ( 'NONE',  ( -0.000000000000000000, -0.000000000000000000, -1.000000000000000000 ) ) ;
#21151 = CARTESIAN_POINT ( 'NONE',  ( -5.000000000000003553, -8.660254037844383745, -31.37500000409676559 ) ) ;
#21152 = LINE ( 'NONE', #25060, #40780 ) ;
#21153 = CARTESIAN_POINT ( 'NONE',  ( 10.81189881249999907, 6.242252689847868297, -133.4062500020483810 ) ) ;
#21154 = CARTESIAN_POINT ( 'NONE',  ( 0.000000000000000000, 0.000000000000000000, -200.0000000000000000 ) ) ;
#21155 = CARTESIAN_POINT ( 'NONE',  ( 7.070501591499376803E-16, 11.54700538379251284, -174.5000000040967905 ) ) ;
#21156 = ORIENTED_EDGE ( 'NONE', *, *, #16390, .F. ) ;
#21157 = CARTESIAN_POINT ( 'NONE',  ( -10.81189881249999907, -6.242252689847864744, -59.15625000204838813 ) ) ;
#21159 = ORIENTED_EDGE ( 'NONE', *, *, #40949, .T. ) ;
#21158 = VERTEX_POINT ( 'NONE', #32391 ) ;
#21160 = CARTESIAN_POINT ( 'NONE',  ( -9.999999999999998224, 1.224646799147353059E-15, -121.2500000000000000 ) ) ;
#21161 = FACE_OUTER_BOUND ( 'NONE', #7577, .T. ) ;
#21162 = CARTESIAN_POINT ( 'NONE',  ( -5.405949406249996869, 9.363379034771805109, -164.3437500020484094 ) ) ;
#21163 = CARTESIAN_POINT ( 'NONE',  ( 10.81189881249999551, -6.242252689847874514, -196.6562500020484379 ) ) ;
#21164 = CARTESIAN_POINT ( 'NONE',  ( 10.81189881249999907, 6.242252689847868297, -11.71875000204837214 ) ) ;
#21165 = CARTESIAN_POINT ( 'NONE',  ( -11.54700538379251817, 20.00000000000000355, 0.000000000000000000 ) ) ;
#21166 = CARTESIAN_POINT ( 'NONE',  ( 5.405949406249999534, 9.363379034771803333, -148.0937500020483810 ) ) ;
#21167 = CARTESIAN_POINT ( 'NONE',  ( 5.405949406249999534, 9.363379034771803333, -131.5937500020483810 ) ) ;
#21168 = CARTESIAN_POINT ( 'NONE',  ( -10.81189881249999907, -6.242252689847864744, -108.6562500020483952 ) ) ;
#21169 = CARTESIAN_POINT ( 'NONE',  ( 10.81189881249999907, 6.242252689847868297, -115.2187500020483810 ) ) ;
#21170 = CARTESIAN_POINT ( 'NONE',  ( 10.00000000000000000, 5.773502691896255534, -194.2500000040968189 ) ) ;
#21171 = CARTESIAN_POINT ( 'NONE',  ( -10.81189881249999907, -6.242252689847864744, -120.6562500020483810 ) ) ;
#21172 = CARTESIAN_POINT ( 'NONE',  ( 10.81189881249999729, 0.000000000000000000, -1.343750002048366143 ) ) ;
#21173 = CARTESIAN_POINT ( 'NONE',  ( 10.81189881249999729, 6.242252689847867408, -128.7187500020483810 ) ) ;
#21174 = CARTESIAN_POINT ( 'NONE',  ( 9.999999999999998224, 0.000000000000000000, -165.8750000040967905 ) ) ;
#21175 = CARTESIAN_POINT ( 'NONE',  ( -9.999999999999998224, 1.224646799147353059E-15, -114.1250000040967763 ) ) ;
#21176 = CARTESIAN_POINT ( 'NONE',  ( 9.999999999999996447, -5.773502691896262640, -146.1250000000000000 ) ) ;
#21177 = CARTESIAN_POINT ( 'NONE',  ( 7.070501591499377789E-16, 11.54700538379251284, -22.62499999999997868 ) ) ;
#21178 = CARTESIAN_POINT ( 'NONE',  ( -5.405949406250003975, -9.363379034771801557, -72.34375000204836681 ) ) ;
#21179 = CARTESIAN_POINT ( 'NONE',  ( 5.405949406249992428, -9.363379034771808662, -69.09375000204836681 ) ) ;
#21180 = CARTESIAN_POINT ( 'NONE',  ( -5.000000000000003553, -8.660254037844383745, -158.8750000040967905 ) ) ;
#21181 = CARTESIAN_POINT ( 'NONE',  ( 5.405949406249999534, 9.363379034771803333, -32.78125000204837391 ) ) ;
#21182 = CARTESIAN_POINT ( 'NONE',  ( -10.81189881249999729, 1.324075727343319199E-15, -44.09375000204837391 ) ) ;
#21183 = CARTESIAN_POINT ( 'NONE',  ( 9.999999999998969713, 5.773502691896851502, -32.25000000409673362 ) ) ;
#21184 = CARTESIAN_POINT ( 'NONE',  ( 5.405949406249992428, -9.363379034771808662, -154.5937500020483810 ) ) ;
#21185 = EDGE_CURVE ( 'NONE', #17257, #19459, #25698, .T. ) ;
#21186 = CARTESIAN_POINT ( 'NONE',  ( -5.000000000000003553, -8.660254037844383745, -122.5000000000000000 ) ) ;
#21187 = CARTESIAN_POINT ( 'NONE',  ( -5.405949406250003975, -9.363379034771801557, -132.5312500020484094 ) ) ;
#21188 =( BOUNDED_CURVE ( )  B_SPLINE_CURVE ( 2, ( #20136, #19496, #33323, #39770, #26198, #22749, #10204 ),
 .UNSPECIFIED., .F., .F. ) 
 B_SPLINE_CURVE_WITH_KNOTS ( ( 3, 2, 2, 3 ),
 ( 0.6753731343283584376, 0.6766169154228858229, 0.6778606965174133192, 0.6791044776119405935 ),
 .UNSPECIFIED. ) 
 CURVE ( )  GEOMETRIC_REPRESENTATION_ITEM ( )  RATIONAL_B_SPLINE_CURVE ( ( 0.9999999999999761302, 0.8660254037844625774, 1.000000000000000000, 0.8660254037844387076, 1.000000000000000000, 0.8660254037844028474, 1.000000000000035971 ) ) 
 REPRESENTATION_ITEM ( '' )  );
#21189 = CARTESIAN_POINT ( 'NONE',  ( 9.999999999999998224, 0.000000000000000000, -66.87500000409676204 ) ) ;
#21190 = CARTESIAN_POINT ( 'NONE',  ( 5.000000000000000000, 8.660254037844385522, -76.74999999999998579 ) ) ;
#21191 = CARTESIAN_POINT ( 'NONE',  ( 7.644554776091147741E-16, 12.48450537969573659, -19.15625000204837391 ) ) ;
#21192 = EDGE_CURVE ( 'NONE', #1054, #19531, #28520, .T. ) ;
#21193 = ORIENTED_EDGE ( 'NONE', *, *, #29446, .T. ) ;
#21194 = CARTESIAN_POINT ( 'NONE',  ( 10.81189881249999729, 6.242252689847867408, -104.9062500020483952 ) ) ;
#21195 = CARTESIAN_POINT ( 'NONE',  ( -4.999999999999996447, 8.660254037844387298, -123.3750000040967905 ) ) ;
#21196 = CARTESIAN_POINT ( 'NONE',  ( -5.000000000000003553, -8.660254037844383745, -179.8750000040967905 ) ) ;
#21197 = CARTESIAN_POINT ( 'NONE',  ( 4.999999999999992006, -8.660254037844389075, -35.62500000409676915 ) ) ;
#21198 = CARTESIAN_POINT ( 'NONE',  ( -9.999999999998969713, -5.773502691896847949, -14.62499999999995026 ) ) ;
#21199 = APPROVAL ( #23295, 'UNSPECIFIED' ) ;
#21200 = CARTESIAN_POINT ( 'NONE',  ( 5.405949406249992428, -9.363379034771808662, -45.28125000204838102 ) ) ;
#21201 = CARTESIAN_POINT ( 'NONE',  ( -2.121150477449813534E-15, -11.54700538379251284, -191.3750000000000284 ) ) ;
#21202 = CARTESIAN_POINT ( 'NONE',  ( 7.644554776091147741E-16, 12.48450537969573659, -154.1562500020484094 ) ) ;
#21203 = CARTESIAN_POINT ( 'NONE',  ( -5.405949406249996869, 9.363379034771805109, -129.8437500020484094 ) ) ;
#21204 = CARTESIAN_POINT ( 'NONE',  ( 7.070501591499376803E-16, 11.54700538379251284, -109.6249999999999858 ) ) ;
#21205 = ORIENTED_EDGE ( 'NONE', *, *, #34924, .F. ) ;
#21206 = CARTESIAN_POINT ( 'NONE',  ( 9.999999999999998224, 0.000000000000000000, -185.3750000040967905 ) ) ;
#21207 = ORIENTED_EDGE ( 'NONE', *, *, #9126, .T. ) ;
#21208 = EDGE_CURVE ( 'NONE', #12734, #31643, #1468, .T. ) ;
#21209 = VERTEX_POINT ( 'NONE', #12294 ) ;
#21210 = VECTOR ( 'NONE', #16320, 1000.000000000000000 ) ;
#21211 = ORIENTED_EDGE ( 'NONE', *, *, #382, .T. ) ;
#21212 =( BOUNDED_CURVE ( )  B_SPLINE_CURVE ( 2, ( #22818, #7050, #20201, #16947, #584, #27967, #33807 ),
 .UNSPECIFIED., .F., .F. ) 
 B_SPLINE_CURVE_WITH_KNOTS ( ( 3, 2, 2, 3 ),
 ( 0.8656716417910450545, 0.8669154228855724398, 0.8681592039800998251, 0.8694029850746272103 ),
 .UNSPECIFIED. ) 
 CURVE ( )  GEOMETRIC_REPRESENTATION_ITEM ( )  RATIONAL_B_SPLINE_CURVE ( ( 0.9999999999999641398, 0.8660254037844745678, 1.000000000000000000, 0.8660254037844387076, 1.000000000000000000, 0.8660254037844028474, 1.000000000000035971 ) ) 
 REPRESENTATION_ITEM ( '' )  );
#21213 = CARTESIAN_POINT ( 'NONE',  ( 10.00000000000051159, -5.773502691895965988, -145.0000000040967620 ) ) ;
#21214 = CARTESIAN_POINT ( 'NONE',  ( -5.405949406250003975, -9.363379034771801557, -187.8437500020483810 ) ) ;
#21215 = CARTESIAN_POINT ( 'NONE',  ( 10.81189881249999551, -6.242252689847874514, -40.46875000204835260 ) ) ;
#21216 = CARTESIAN_POINT ( 'NONE',  ( -10.00000000000038547, 5.773502691896036154, -153.2500000040967905 ) ) ;
#21217 = CARTESIAN_POINT ( 'NONE',  ( 0.000000000000000000, 0.000000000000000000, -200.0000000000000000 ) ) ;
#21218 = CARTESIAN_POINT ( 'NONE',  ( 10.81189881249999729, 0.000000000000000000, -173.8437500020484094 ) ) ;
#21219 = CARTESIAN_POINT ( 'NONE',  ( 7.644554776091147741E-16, 12.48450537969573659, -161.4687500020484094 ) ) ;
#21220 = LINE ( 'NONE', #24479, #10042 ) ;
#21221 = CARTESIAN_POINT ( 'NONE',  ( -10.81189881249999729, 6.242252689847871849, -143.2187500020484094 ) ) ;
#21222 = CARTESIAN_POINT ( 'NONE',  ( 10.81189881249999907, 6.242252689847868297, -145.4062500020484094 ) ) ;
#21223 = CARTESIAN_POINT ( 'NONE',  ( -2.293366432827344421E-15, -12.48450537969573659, -151.7187500020483810 ) ) ;
#21224 = CARTESIAN_POINT ( 'NONE',  ( -11.54700538379251817, 20.00000000000000355, 45.00000000000009237 ) ) ;
#21225 =( BOUNDED_CURVE ( )  B_SPLINE_CURVE ( 2, ( #40689, #20852, #34036, #24539, #37046, #11552, #40472 ),
 .UNSPECIFIED., .F., .F. ) 
 B_SPLINE_CURVE_WITH_KNOTS ( ( 3, 2, 2, 3 ),
 ( 0.3656716417910448325, 0.3669154228855722732, 0.3681592039800996030, 0.3694029850746270438 ),
 .UNSPECIFIED. ) 
 CURVE ( )  GEOMETRIC_REPRESENTATION_ITEM ( )  RATIONAL_B_SPLINE_CURVE ( ( 0.9999999999999940048, 0.8660254037844447028, 1.000000000000000000, 0.8660254037844387076, 1.000000000000000000, 0.8660254037844207220, 1.000000000000017986 ) ) 
 REPRESENTATION_ITEM ( '' )  );
#21226 = LINE ( 'NONE', #14519, #3877 ) ;
#21227 = CARTESIAN_POINT ( 'NONE',  ( -9.999999999999998224, 1.224646799147353059E-15, -167.7500000000000000 ) ) ;
#21228 = CARTESIAN_POINT ( 'NONE',  ( -10.81189881249999729, 1.324075727343319199E-15, -87.59375000204836681 ) ) ;
#21229 = CARTESIAN_POINT ( 'NONE',  ( -9.999999999998456346, -5.773502691897145489, -82.50000000409673362 ) ) ;
#21230 = CARTESIAN_POINT ( 'NONE',  ( -2.293366432827344421E-15, -12.48450537969573659, -55.90625000204837391 ) ) ;
#21231 = CARTESIAN_POINT ( 'NONE',  ( -5.741579586894616227, -8.238110979333516326, -99.99999999999995737 ) ) ;
#21232 = CARTESIAN_POINT ( 'NONE',  ( 5.405949406249999534, 9.363379034771803333, -176.5937500020484094 ) ) ;
#21233 = CARTESIAN_POINT ( 'NONE',  ( 10.81189881249999729, 0.000000000000000000, -112.5312500020483952 ) ) ;
#21234 = CARTESIAN_POINT ( 'NONE',  ( -5.405949406250003975, -9.363379034771801557, -158.0312500020484094 ) ) ;
#21235 = DIRECTION ( 'NONE',  ( -0.000000000000000000, -0.000000000000000000, 1.000000000000000000 ) ) ;
#21236 = CARTESIAN_POINT ( 'NONE',  ( -5.405949406249996869, 9.363379034771805109, -41.53125000204838102 ) ) ;
#21237 = CARTESIAN_POINT ( 'NONE',  ( -9.999999999999998224, 5.773502691896259087, -127.7500000040967905 ) ) ;
#21238 = CARTESIAN_POINT ( 'NONE',  ( 5.000000000000000000, 8.660254037844385522, -105.2499999999999858 ) ) ;
#21239 = ORIENTED_EDGE ( 'NONE', *, *, #18864, .T. ) ;
#21240 =( BOUNDED_CURVE ( )  B_SPLINE_CURVE ( 2, ( #22530, #35703, #15606, #25355, #28808, #32471, #12793 ),
 .UNSPECIFIED., .F., .F. ) 
 B_SPLINE_CURVE_WITH_KNOTS ( ( 3, 2, 2, 3 ),
 ( 0.7313432835820897759, 0.7325870646766171612, 0.7338308457711446575, 0.7350746268656719318 ),
 .UNSPECIFIED. ) 
 CURVE ( )  GEOMETRIC_REPRESENTATION_ITEM ( )  RATIONAL_B_SPLINE_CURVE ( ( 0.9999999999999761302, 0.8660254037844625774, 1.000000000000000000, 0.8660254037844387076, 1.000000000000000000, 0.8660254037844028474, 1.000000000000035971 ) ) 
 REPRESENTATION_ITEM ( '' )  );
#21241 = CARTESIAN_POINT ( 'NONE',  ( 5.405949406249999534, 9.363379034771803333, -124.2812500020483952 ) ) ;
#21242 = CARTESIAN_POINT ( 'NONE',  ( 5.000000000000000000, 8.660254037844385522, -152.1250000040967905 ) ) ;
#21243 = CARTESIAN_POINT ( 'NONE',  ( 5.321294541346989426, -5.321294541346989426, -219.9999999999999716 ) ) ;
#21244 = CARTESIAN_POINT ( 'NONE',  ( -10.81189881249999729, 1.324075727343319199E-15, -180.7812500020484094 ) ) ;
#21245 = ORIENTED_EDGE ( 'NONE', *, *, #40425, .T. ) ;
#21246 = CARTESIAN_POINT ( 'NONE',  ( -5.405949406250003975, -9.363379034771801557, -175.8437500020483810 ) ) ;
#21247 = CARTESIAN_POINT ( 'NONE',  ( -9.999999999999998224, 1.224646799147353059E-15, -60.12500000409676204 ) ) ;
#21248 = CARTESIAN_POINT ( 'NONE',  ( 9.999999999999998224, 0.000000000000000000, -18.49999999999996092 ) ) ;
#21249 = CARTESIAN_POINT ( 'NONE',  ( 7.070501591499376803E-16, 11.54700538379251284, -135.5000000040967905 ) ) ;
#21250 = CARTESIAN_POINT ( 'NONE',  ( 5.405949406249999534, 9.363379034771803333, -71.78125000204838102 ) ) ;
#21251 = CARTESIAN_POINT ( 'NONE',  ( 5.405949406249992428, -9.363379034771808662, -49.78125000204838813 ) ) ;
#21252 = CARTESIAN_POINT ( 'NONE',  ( -5.000000000000003553, -8.660254037844383745, -41.87500000409677625 ) ) ;
#21253 = CARTESIAN_POINT ( 'NONE',  ( 5.405949406249992428, -9.363379034771808662, -4.593750002048368586 ) ) ;
#21254 = LINE ( 'NONE', #34442, #20727 ) ;
#21255 = CARTESIAN_POINT ( 'NONE',  ( 10.81189881249999551, -6.242252689847874514, -178.6562500020484094 ) ) ;
#21256 = EDGE_CURVE ( 'NONE', #7028, #318, #29143, .T. ) ;
#21257 = CARTESIAN_POINT ( 'NONE',  ( -9.999999999999998224, 1.224646799147353059E-15, -159.1250000040967905 ) ) ;
#21258 = CARTESIAN_POINT ( 'NONE',  ( -10.00000000000076916, 5.773502691895813221, -138.2500000040967905 ) ) ;
#21259 = B_SPLINE_CURVE_WITH_KNOTS ( 'NONE', 3,
 ( #31179, #28366, #41505, #37198, #7646, #4406, #30747, #21014, #3458, #12149, #26550, #2669 ),
 .UNSPECIFIED., .F., .F.,
 ( 4, 2, 2, 2, 2, 4 ),
 ( 4.985610057939991272E-16, 0.002144051117877697737, 0.004288102235754896741, 0.005360127794693496026, 0.006432153353632096178, 0.008576204471509293881 ),
 .UNSPECIFIED. ) ;
#21260 = ORIENTED_EDGE ( 'NONE', *, *, #42062, .F. ) ;
#21261 = CARTESIAN_POINT ( 'NONE',  ( -4.999999999999996447, 8.660254037844387298, -117.0000000000000000 ) ) ;
#21262 = CARTESIAN_POINT ( 'NONE',  ( 9.999999999999998224, 0.000000000000000000, -59.37500000409676204 ) ) ;
#21263 = CARTESIAN_POINT ( 'NONE',  ( -9.999999999999998224, 0.000000000000000000, -99.99999999999998579 ) ) ;
#21265 = ORIENTED_EDGE ( 'NONE', *, *, #15138, .T. ) ;
#21264 = CARTESIAN_POINT ( 'NONE',  ( -10.81189881249999729, 1.324075727343319199E-15, -86.28125000204838102 ) ) ;
#21267 = VERTEX_POINT ( 'NONE', #38426 ) ;
#21266 = CARTESIAN_POINT ( 'NONE',  ( -23.09401076758503280, 0.000000000000000000, 49.99999999999998579 ) ) ;
#21268 = EDGE_LOOP ( 'NONE', ( #31542, #16069, #4337, #38987 ) ) ;
#21269 = CARTESIAN_POINT ( 'NONE',  ( -10.81189881249999729, 6.242252689847871849, -41.21875000204834549 ) ) ;
#21270 = CARTESIAN_POINT ( 'NONE',  ( 10.81189881249999551, -6.242252689847874514, -23.96875000204836681 ) ) ;
#21271 = CARTESIAN_POINT ( 'NONE',  ( 5.405949406249992428, -9.363379034771808662, -10.78125000204835438 ) ) ;
#21273 = ORIENTED_EDGE ( 'NONE', *, *, #27256, .T. ) ;
#21272 = CARTESIAN_POINT ( 'NONE',  ( 7.644554776091147741E-16, 12.48450537969573659, -63.96875000204837391 ) ) ;
#21274 = DIRECTION ( 'NONE',  ( 1.000000000000000000, 0.000000000000000000, 0.000000000000000000 ) ) ;
#21275 = CARTESIAN_POINT ( 'NONE',  ( -10.00000000000000000, -5.773502691896251982, -38.62499999999996447 ) ) ;
#21276 = AXIS2_PLACEMENT_3D ( 'NONE', #29585, #2835, #25721 ) ;
#21277 = CARTESIAN_POINT ( 'NONE',  ( 10.81189881249999551, -6.242252689847874514, -188.9687500020484094 ) ) ;
#21278 = CARTESIAN_POINT ( 'NONE',  ( -5.405949406250003975, -9.363379034771801557, -166.8437500020484094 ) ) ;
#21279 = CARTESIAN_POINT ( 'NONE',  ( 9.999999999999998224, 0.000000000000000000, -59.37500000409676204 ) ) ;
#21280 = DIRECTION ( 'NONE',  ( -1.000000000000000000, 0.000000000000000000, 0.000000000000000000 ) ) ;
#21281 = CARTESIAN_POINT ( 'NONE',  ( -1.040834085586084257E-14, 125.0000000000000000, 22.49999999999999289 ) ) ;
#21282 = CARTESIAN_POINT ( 'NONE',  ( -9.999999999999998224, 1.224646799147353059E-15, -60.12500000409676204 ) ) ;
#21283 = CARTESIAN_POINT ( 'NONE',  ( 10.81189881249999907, 6.242252689847868297, -113.7187500020483810 ) ) ;
#21284 = DIRECTION ( 'NONE',  ( 1.000000000000000000, 0.000000000000000000, 0.000000000000000000 ) ) ;
#21285 = CARTESIAN_POINT ( 'NONE',  ( 5.405949406249999534, 9.363379034771803333, -85.28125000204838102 ) ) ;
#21286 = CARTESIAN_POINT ( 'NONE',  ( -10.81189881249999729, 1.324075727343319199E-15, -104.0937500020483810 ) ) ;
#21287 = CARTESIAN_POINT ( 'NONE',  ( -10.81189881249999729, 6.242252689847871849, -62.21875000204838102 ) ) ;
#21288 = CARTESIAN_POINT ( 'NONE',  ( -2.293366432827344421E-15, -12.48450537969573659, -70.90625000204839523 ) ) ;
#21289 = CARTESIAN_POINT ( 'NONE',  ( 5.000000000000000000, 8.660254037844385522, -153.6250000040967905 ) ) ;
#21290 = CARTESIAN_POINT ( 'NONE',  ( 9.999999999999998224, 0.000000000000000000, -129.5000000000000000 ) ) ;
#21291 = CARTESIAN_POINT ( 'NONE',  ( -2.293366432827344421E-15, -12.48450537969573659, -148.9062500020484379 ) ) ;
#21292 = CARTESIAN_POINT ( 'NONE',  ( 5.405949406249999534, 9.363379034771803333, -167.7812500020484094 ) ) ;
#21293 = CARTESIAN_POINT ( 'NONE',  ( 4.999999999999992006, -8.660254037844389075, -174.7500000000000284 ) ) ;
#21294 = DIRECTION ( 'NONE',  ( -0.000000000000000000, -0.000000000000000000, 1.000000000000000000 ) ) ;
#21295 = CARTESIAN_POINT ( 'NONE',  ( 10.81189881249999729, 0.000000000000000000, -97.34375000204838102 ) ) ;
#21296 = CARTESIAN_POINT ( 'NONE',  ( 7.070501591499376803E-16, 11.54700538379251284, -120.5000000040967905 ) ) ;
#21297 = CARTESIAN_POINT ( 'NONE',  ( 5.000000000000000000, 8.660254037844385522, -75.24999999999998579 ) ) ;
#21298 = CARTESIAN_POINT ( 'NONE',  ( 7.644554776091147741E-16, 12.48450537969573659, 0.3437499979516422943 ) ) ;
#21299 = CARTESIAN_POINT ( 'NONE',  ( 10.00000000000000000, 5.773502691896255534, -83.25000000409677625 ) ) ;
#21300 = CYLINDRICAL_SURFACE ( 'NONE', #21024, 9.999999999999998224 ) ;
#21301 = CARTESIAN_POINT ( 'NONE',  ( 7.644554776091147741E-16, 12.48450537969573659, -91.15625000204838102 ) ) ;
#21302 = CARTESIAN_POINT ( 'NONE',  ( 10.81189881249999729, 0.000000000000000000, -78.03125000204838102 ) ) ;
#21303 = CARTESIAN_POINT ( 'NONE',  ( -9.999999999999998224, 1.224646799147353059E-15, -66.12500000409676204 ) ) ;
#21304 = CARTESIAN_POINT ( 'NONE',  ( -2.121150477449813534E-15, -11.54700538379251284, -59.37500000000001421 ) ) ;
#21305 = CARTESIAN_POINT ( 'NONE',  ( -5.405949406249996869, 9.363379034771805109, -26.34375000204835970 ) ) ;
#21306 = ORIENTED_EDGE ( 'NONE', *, *, #6173, .T. ) ;
#21307 = CARTESIAN_POINT ( 'NONE',  ( 4.999999999999992006, -8.660254037844389075, -5.249999999999976907 ) ) ;
#21308 = CARTESIAN_POINT ( 'NONE',  ( -2.293366432827344421E-15, -12.48450537969573659, -24.40625000204838102 ) ) ;
#21309 = CARTESIAN_POINT ( 'NONE',  ( 10.81189881249999551, -6.242252689847874514, -14.96875000204837214 ) ) ;
#21310 = CARTESIAN_POINT ( 'NONE',  ( -9.999999999999998224, 1.224646799147353059E-15, -149.7500000000000000 ) ) ;
#21311 =( BOUNDED_CURVE ( )  B_SPLINE_CURVE ( 2, ( #10227, #3561, #19944, #23414, #22775, #36563, #16479 ),
 .UNSPECIFIED., .F., .F. ) 
 B_SPLINE_CURVE_WITH_KNOTS ( ( 3, 2, 2, 3 ),
 ( 0.02238805970149256030, 0.02363184079601992477, 0.02487562189054729270, 0.02611940298507465369 ),
 .UNSPECIFIED. ) 
 CURVE ( )  GEOMETRIC_REPRESENTATION_ITEM ( )  RATIONAL_B_SPLINE_CURVE ( ( 0.9999999999999973355, 0.8660254037844413721, 1.000000000000000000, 0.8660254037844387076, 1.000000000000000000, 0.8660254037844357100, 1.000000000000003109 ) ) 
 REPRESENTATION_ITEM ( '' )  );
#21312 = CARTESIAN_POINT ( 'NONE',  ( -9.999999999999998224, 1.224646799147353059E-15, -6.125000004096770034 ) ) ;
#21313 = CARTESIAN_POINT ( 'NONE',  ( 9.999999999999998224, 0.000000000000000000, -152.3750000040967905 ) ) ;
#21314 = CARTESIAN_POINT ( 'NONE',  ( -10.81189881249999729, 6.242252689847871849, -128.4062500020484094 ) ) ;
#21315 = CARTESIAN_POINT ( 'NONE',  ( 9.999999999999998224, 0.000000000000000000, -183.5000000000000000 ) ) ;
#21316 = CARTESIAN_POINT ( 'NONE',  ( -9.999999999999998224, 1.224646799147353059E-15, -200.0000000000000000 ) ) ;
#21318 = EDGE_LOOP ( 'NONE', ( #8208, #41075 ) ) ;
#21317 = CARTESIAN_POINT ( 'NONE',  ( -2.293366432827344421E-15, -12.48450537969573659, -108.4062500020483810 ) ) ;
#21319 = VERTEX_POINT ( 'NONE', #38639 ) ;
#21320 = VERTEX_POINT ( 'NONE', #12705 ) ;
#21321 = ADVANCED_FACE ( 'NONE', ( #25902 ), #39054, .T. ) ;
#21322 = CIRCLE ( 'NONE', #18558, 20.00000000000000355 ) ;
#21323 = CARTESIAN_POINT ( 'NONE',  ( 10.81189881249999551, -6.242252689847874514, -36.15625000204835970 ) ) ;
#21324 = CALENDAR_DATE ( 2026, 28, 9 ) ;
#21325 = CARTESIAN_POINT ( 'NONE',  ( -5.405949406249996869, 9.363379034771805109, -89.34375000204838102 ) ) ;
#21326 = FACE_OUTER_BOUND ( 'NONE', #15364, .T. ) ;
#21327 = CARTESIAN_POINT ( 'NONE',  ( -9.999999999999227285, -5.773502691896698735, -129.0000000040967620 ) ) ;
#21328 = CARTESIAN_POINT ( 'NONE',  ( -9.999999999999998224, 1.224646799147353059E-15, -105.1250000040967763 ) ) ;
#21329 = CARTESIAN_POINT ( 'NONE',  ( 5.405949406249999534, 9.363379034771803333, -163.2812500020484094 ) ) ;
#21330 = DIRECTION ( 'NONE',  ( -0.5000000000000008882, 0.8660254037844382635, 0.000000000000000000 ) ) ;
#21331 = CARTESIAN_POINT ( 'NONE',  ( 10.81189881249999551, -6.242252689847874514, -121.4687500020484237 ) ) ;
#21332 = CARTESIAN_POINT ( 'NONE',  ( 5.405949406249992428, -9.363379034771808662, -84.09375000204836681 ) ) ;
#21333 = CARTESIAN_POINT ( 'NONE',  ( -5.405949406250003975, -9.363379034771801557, -0.5312500020483723606 ) ) ;
#21334 = CARTESIAN_POINT ( 'NONE',  ( -10.81189881249999907, -6.242252689847864744, -193.9687500020484094 ) ) ;
#21335 = CARTESIAN_POINT ( 'NONE',  ( 5.405949406249992428, -9.363379034771808662, -91.78125000204838102 ) ) ;
#21336 = CARTESIAN_POINT ( 'NONE',  ( 10.00000000000000000, 5.773502691896255534, -176.2500000040968189 ) ) ;
#21337 = CARTESIAN_POINT ( 'NONE',  ( -2.293366432827344421E-15, -12.48450537969573659, -169.9062500020484379 ) ) ;
#21338 = DIRECTION ( 'NONE',  ( -0.000000000000000000, -0.000000000000000000, 1.000000000000000000 ) ) ;
#21339 = CARTESIAN_POINT ( 'NONE',  ( -5.405949406249996869, 9.363379034771805109, -178.0312500020483810 ) ) ;
#21340 = CARTESIAN_POINT ( 'NONE',  ( -10.81189881249999907, -6.242252689847864744, -188.1562500020484094 ) ) ;
#21341 = CARTESIAN_POINT ( 'NONE',  ( -10.81189881249999729, 1.324075727343319199E-15, -56.09375000204835970 ) ) ;
#21342 = VECTOR ( 'NONE', #7677, 1000.000000000000000 ) ;
#21343 = EDGE_CURVE ( 'NONE', #12803, #17345, #5880, .T. ) ;
#21344 = CARTESIAN_POINT ( 'NONE',  ( 7.070501591499377789E-16, 11.54700538379251284, -162.5000000040967905 ) ) ;
#21345 = CARTESIAN_POINT ( 'NONE',  ( -10.81189881249999729, 6.242252689847871849, -9.906250002048379244 ) ) ;
#21346 = CARTESIAN_POINT ( 'NONE',  ( 10.81189881249999551, -6.242252689847874514, -10.46875000204835793 ) ) ;
#21347 = DIRECTION ( 'NONE',  ( -1.000000000000000000, 0.000000000000000000, 0.000000000000000000 ) ) ;
#21348 = CARTESIAN_POINT ( 'NONE',  ( 5.405949406249992428, -9.363379034771808662, -123.0937500020483952 ) ) ;
#21349 = CARTESIAN_POINT ( 'NONE',  ( -10.00000000000000000, -5.773502691896251982, -100.1249999999999858 ) ) ;
#21350 = CARTESIAN_POINT ( 'NONE',  ( -10.81189881249999729, 6.242252689847871849, -23.40625000204837747 ) ) ;
#21351 = CARTESIAN_POINT ( 'NONE',  ( 9.999999999999996447, -5.773502691896262640, -104.5000000040967763 ) ) ;
#21352 = CARTESIAN_POINT ( 'NONE',  ( -9.999999999999998224, 1.224646799147353059E-15, -115.2499999999999858 ) ) ;
#21353 = CARTESIAN_POINT ( 'NONE',  ( 7.070501591499377789E-16, 11.54700538379251284, -52.62499999999997868 ) ) ;
#21354 = CARTESIAN_POINT ( 'NONE',  ( -10.81189881249999729, 6.242252689847871849, -125.4062500020483810 ) ) ;
#21355 = CARTESIAN_POINT ( 'NONE',  ( 10.81189881249999551, -6.242252689847874514, -96.15625000204838102 ) ) ;
#21356 = VERTEX_POINT ( 'NONE', #10540 ) ;
#21357 =( BOUNDED_CURVE ( )  B_SPLINE_CURVE ( 2, ( #14074, #37412, #8067, #24045, #23831, #21216, #7854 ),
 .UNSPECIFIED., .F., .F. ) 
 B_SPLINE_CURVE_WITH_KNOTS ( ( 3, 2, 2, 3 ),
 ( 0.2238805970149254365, 0.2251243781094527940, 0.2263681592039801793, 0.2276119402985075368 ),
 .UNSPECIFIED. ) 
 CURVE ( )  GEOMETRIC_REPRESENTATION_ITEM ( )  RATIONAL_B_SPLINE_CURVE ( ( 0.9999999999999940048, 0.8660254037844447028, 1.000000000000000000, 0.8660254037844387076, 1.000000000000000000, 0.8660254037844297148, 1.000000000000008882 ) ) 
 REPRESENTATION_ITEM ( '' )  );
#21358 = ADVANCED_FACE ( 'NONE', ( #23726 ), #19618, .T. ) ;
#21359 = CARTESIAN_POINT ( 'NONE',  ( -9.999999999999998224, 1.224646799147353059E-15, -99.12500000409677625 ) ) ;
#21360 = CARTESIAN_POINT ( 'NONE',  ( -9.999999999999998224, 1.224646799147353059E-15, -139.6250000040967905 ) ) ;
#21361 = CARTESIAN_POINT ( 'NONE',  ( -10.81189881249999907, -6.242252689847864744, -162.6562500020483810 ) ) ;
#21362 = CARTESIAN_POINT ( 'NONE',  ( -10.81189881249999729, 6.242252689847871849, -47.21875000204836681 ) ) ;
#21363 = ORIENTED_EDGE ( 'NONE', *, *, #11142, .T. ) ;
#21364 = CARTESIAN_POINT ( 'NONE',  ( -2.121150477449813534E-15, -11.54700538379251284, -21.87499999999997513 ) ) ;
#21365 = CARTESIAN_POINT ( 'NONE',  ( -10.81189881249999729, -6.242252689847864744, -27.65625000204838102 ) ) ;
#21366 = CARTESIAN_POINT ( 'NONE',  ( 7.070501591499377789E-16, 11.54700538379251284, -157.6250000000000000 ) ) ;
#21367 = DIRECTION ( 'NONE',  ( 1.000000000000000000, 0.000000000000000000, 0.000000000000000000 ) ) ;
#21368 = CARTESIAN_POINT ( 'NONE',  ( -4.999999999999996447, 8.660254037844387298, -31.87500000409676559 ) ) ;
#21369 = DIRECTION ( 'NONE',  ( -0.000000000000000000, -0.000000000000000000, 1.000000000000000000 ) ) ;
#21370 = CARTESIAN_POINT ( 'NONE',  ( -5.405949406249996869, 9.363379034771805109, -134.5312500020484094 ) ) ;
#21371 = CARTESIAN_POINT ( 'NONE',  ( 5.504483976897049047, 8.886403137384359496, -8.678191841965556968E-15 ) ) ;
#21372 = ORIENTED_EDGE ( 'NONE', *, *, #32223, .T. ) ;
#21373 = CARTESIAN_POINT ( 'NONE',  ( 5.405949406249999534, 9.363379034771803333, -62.78125000204837391 ) ) ;
#21374 = COORDINATED_UNIVERSAL_TIME_OFFSET ( 6, 0, .AHEAD. ) ;
#21375 = VECTOR ( 'NONE', #1267, 1000.000000000000000 ) ;
#21376 = EDGE_CURVE ( 'NONE', #23028, #33859, #6129, .T. ) ;
#21378 = ORIENTED_EDGE ( 'NONE', *, *, #11028, .F. ) ;
#21377 = ORIENTED_EDGE ( 'NONE', *, *, #19093, .F. ) ;
#21379 = DIRECTION ( 'NONE',  ( -0.000000000000000000, -0.000000000000000000, -1.000000000000000000 ) ) ;
#21380 = CARTESIAN_POINT ( 'NONE',  ( -7.071067811865477282, -7.071067811865471064, -200.0000000000000000 ) ) ;
#21381 = CARTESIAN_POINT ( 'NONE',  ( 10.81189881249999551, -6.242252689847874514, -160.4687500020484094 ) ) ;
#21382 = CARTESIAN_POINT ( 'NONE',  ( -10.81189881249999907, -6.242252689847864744, -185.1562500020484094 ) ) ;
#21383 = CARTESIAN_POINT ( 'NONE',  ( -10.81189881249999729, 6.242252689847871849, -14.21875000204836681 ) ) ;
#21384 = DIRECTION ( 'NONE',  ( 0.7071067811865459074, 8.659560562354911904E-17, -0.7071067811865491270 ) ) ;
#21385 = CARTESIAN_POINT ( 'NONE',  ( -10.81189881249999729, 6.242252689847871849, -150.7187500020483810 ) ) ;
#21386 = CARTESIAN_POINT ( 'NONE',  ( -5.405949406249996869, 9.363379034771805109, -106.0312500020483810 ) ) ;
#21387 = CARTESIAN_POINT ( 'NONE',  ( -5.405949406249996869, 9.363379034771805109, -110.3437500020483810 ) ) ;
#21388 = DIRECTION ( 'NONE',  ( 1.000000000000000000, 0.000000000000000000, 0.000000000000000000 ) ) ;
#21389 = CARTESIAN_POINT ( 'NONE',  ( 5.405949406249992428, -9.363379034771808662, -112.7812500020483952 ) ) ;
#21390 = CARTESIAN_POINT ( 'NONE',  ( -2.293366432827344421E-15, -12.48450537969573659, -6.218750002048345493 ) ) ;
#21391 = CARTESIAN_POINT ( 'NONE',  ( -5.405949406249996869, 9.363379034771805109, -128.3437500020484094 ) ) ;
#21392 = CARTESIAN_POINT ( 'NONE',  ( 7.644554776091147741E-16, 12.48450537969573659, -191.6562500020484094 ) ) ;
#21393 = DIRECTION ( 'NONE',  ( -0.000000000000000000, -0.000000000000000000, 1.000000000000000000 ) ) ;
#21394 = CARTESIAN_POINT ( 'NONE',  ( 9.999999999999998224, 0.000000000000000000, -146.0000000000000000 ) ) ;
#21395 = CARTESIAN_POINT ( 'NONE',  ( 9.999999999999996447, -5.773502691896262640, -9.624999999999968026 ) ) ;
#21396 = CARTESIAN_POINT ( 'NONE',  ( 7.644554776091147741E-16, 12.48450537969573659, -75.96875000204838102 ) ) ;
#21397 = CARTESIAN_POINT ( 'NONE',  ( 10.81189881249999907, 6.242252689847868297, -55.21875000204836681 ) ) ;
#21398 = CARTESIAN_POINT ( 'NONE',  ( -10.00000000000000000, -5.773502691896252870, -170.6249999999999716 ) ) ;
#21399 = CARTESIAN_POINT ( 'NONE',  ( -2.293366432827344421E-15, -12.48450537969573659, -34.90625000204836681 ) ) ;
#21400 = CARTESIAN_POINT ( 'NONE',  ( 7.644554776091147741E-16, 12.48450537969573659, -42.96875000204835970 ) ) ;
#21401 = CARTESIAN_POINT ( 'NONE',  ( -10.81189881249999907, -6.242252689847864744, -144.4687500020484094 ) ) ;
#21402 = CARTESIAN_POINT ( 'NONE',  ( -4.999999999999996447, 8.660254037844387298, -121.5000000000000000 ) ) ;
#21403 = FACE_OUTER_BOUND ( 'NONE', #13471, .T. ) ;
#21404 = CARTESIAN_POINT ( 'NONE',  ( 5.000000000000000000, 8.660254037844385522, -72.24999999999998579 ) ) ;
#21405 = CARTESIAN_POINT ( 'NONE',  ( 5.405949406249999534, 9.363379034771803333, -7.281250002048378356 ) ) ;
#21406 = VERTEX_POINT ( 'NONE', #36666 ) ;
#21407 = CARTESIAN_POINT ( 'NONE',  ( -5.405949406250003975, -9.363379034771801557, -104.0312500020483810 ) ) ;
#21408 = CARTESIAN_POINT ( 'NONE',  ( -4.999999999999996447, 8.660254037844387298, -126.3750000040967905 ) ) ;
#21409 = CARTESIAN_POINT ( 'NONE',  ( -10.00000000000025757, -5.773502691896102768, -180.0000000040968189 ) ) ;
#21410 = CARTESIAN_POINT ( 'NONE',  ( -2.293366432827344421E-15, -12.48450537969573659, -79.71875000204838102 ) ) ;
#21411 = AXIS2_PLACEMENT_3D ( 'NONE', #34932, #38573, #5996 ) ;
#21412 = CARTESIAN_POINT ( 'NONE',  ( -9.999999999999998224, 5.773502691896259087, -31.75000000409675138 ) ) ;
#21413 = VECTOR ( 'NONE', #12853, 1000.000000000000000 ) ;
#21414 = CARTESIAN_POINT ( 'NONE',  ( -9.999999999999998224, 1.224646799147353059E-15, -3.125000004096767370 ) ) ;
#21415 = CARTESIAN_POINT ( 'NONE',  ( 5.405949406249992428, -9.363379034771808662, -42.28125000204838102 ) ) ;
#21416 = CARTESIAN_POINT ( 'NONE',  ( -2.121150477449813534E-15, -11.54700538379251284, -137.3750000000000000 ) ) ;
#21417 = CARTESIAN_POINT ( 'NONE',  ( -5.405949406250003975, -9.363379034771801557, -141.5312500020483810 ) ) ;
#21418 = CARTESIAN_POINT ( 'NONE',  ( -10.81189881249999729, 6.242252689847871849, -123.7187500020483952 ) ) ;
#21419 = CARTESIAN_POINT ( 'NONE',  ( 9.999999999999479527, 5.773502691896553074, -144.3750000000000000 ) ) ;
#21420 = CARTESIAN_POINT ( 'NONE',  ( -9.999999999999868550, 5.773502691896333694, -176.8750000000000000 ) ) ;
#21421 = ORIENTED_EDGE ( 'NONE', *, *, #14872, .F. ) ;
#21422 = EDGE_CURVE ( 'NONE', #19092, #40867, #10517, .T. ) ;
#21423 = ORIENTED_EDGE ( 'NONE', *, *, #33597, .T. ) ;
#21424 = ADVANCED_FACE ( 'NONE', ( #13765 ), #3236, .F. ) ;
#21425 = VERTEX_POINT ( 'NONE', #7107 ) ;
#21426 = EDGE_CURVE ( 'NONE', #23854, #11337, #10264, .T. ) ;
#21427 = LINE ( 'NONE', #1376, #23774 ) ;
#21428 = CARTESIAN_POINT ( 'NONE',  ( -10.81189881249999907, -6.242252689847864744, -180.4687500020484094 ) ) ;
#21429 = CC_DESIGN_SECURITY_CLASSIFICATION ( #10394, ( #36593 ) ) ;
#21430 = CARTESIAN_POINT ( 'NONE',  ( -5.405949406250003975, -9.363379034771801557, -36.34375000204836681 ) ) ;
#21431 = CARTESIAN_POINT ( 'NONE',  ( -5.000000000000003553, -8.660254037844383745, -41.49999999999997868 ) ) ;
#21432 = CARTESIAN_POINT ( 'NONE',  ( -10.81189881249999729, -6.242252689847864744, -171.4687500020483526 ) ) ;
#21433 = CARTESIAN_POINT ( 'NONE',  ( 5.405949406249992428, -9.363379034771808662, -156.0937500020483810 ) ) ;
#21434 = CARTESIAN_POINT ( 'NONE',  ( 0.000000000000000000, 0.000000000000000000, -200.0000000000000000 ) ) ;
#21435 = CARTESIAN_POINT ( 'NONE',  ( -10.81189881249999729, 1.324075727343319199E-15, -140.0937500020483810 ) ) ;
#21436 = CARTESIAN_POINT ( 'NONE',  ( -10.81189881249999907, -6.242252689847864744, -144.6562500020484094 ) ) ;
#21437 = CARTESIAN_POINT ( 'NONE',  ( -10.81189881249999729, 1.324075727343319199E-15, -158.0937500020483810 ) ) ;
#21438 = CARTESIAN_POINT ( 'NONE',  ( 10.00000000000025402, -5.773502691896113426, -155.1250000000000000 ) ) ;
#21439 = CARTESIAN_POINT ( 'NONE',  ( 5.000000000000000000, 8.660254037844385522, -11.12500000409674605 ) ) ;
#21440 = CARTESIAN_POINT ( 'NONE',  ( -5.000000000000003553, -8.660254037844383745, -170.5000000000000000 ) ) ;
#21441 = CARTESIAN_POINT ( 'NONE',  ( 7.644554776091147741E-16, 12.48450537969573659, -80.46875000204838102 ) ) ;
#21442 = FACE_OUTER_BOUND ( 'NONE', #37406, .T. ) ;
#21443 = CARTESIAN_POINT ( 'NONE',  ( -5.405949406250003975, -9.363379034771801557, -56.03125000204836681 ) ) ;
#21444 = CARTESIAN_POINT ( 'NONE',  ( -10.37936602110037931, 1.593253728262159941, -99.99999999999994316 ) ) ;
#21445 = CARTESIAN_POINT ( 'NONE',  ( 7.644554776091147741E-16, 12.48450537969573659, -176.4687500020483810 ) ) ;
#21446 = EDGE_CURVE ( 'NONE', #4273, #40023, #14674, .T. ) ;
#21447 = CARTESIAN_POINT ( 'NONE',  ( 5.405949406249999534, 9.363379034771803333, -116.7812500020483952 ) ) ;
#21448 = CARTESIAN_POINT ( 'NONE',  ( -2.293366432827344421E-15, -12.48450537969573659, -157.9062500020483810 ) ) ;
#21449 = CARTESIAN_POINT ( 'NONE',  ( 10.00000000000102318, -5.773502691895667560, -11.12499999999993072 ) ) ;
#21450 = CARTESIAN_POINT ( 'NONE',  ( 10.81189881249999551, -6.242252689847874514, -40.65625000204835970 ) ) ;
#21451 = CARTESIAN_POINT ( 'NONE',  ( 9.999999999999996447, -5.773502691896262640, -127.0000000040967763 ) ) ;
#21452 = CARTESIAN_POINT ( 'NONE',  ( -9.999999999999998224, 5.773502691896259087, -98.87499999999998579 ) ) ;
#21453 = VERTEX_POINT ( 'NONE', #6679 ) ;
#21454 = CARTESIAN_POINT ( 'NONE',  ( 10.81189881249999551, -6.242252689847874514, -126.1562500020483810 ) ) ;
#21455 = CARTESIAN_POINT ( 'NONE',  ( -5.000000000000003553, -8.660254037844383745, -149.8750000040967905 ) ) ;
#21456 = DIRECTION ( 'NONE',  ( 0.000000000000000000, 1.000000000000000000, 0.000000000000000000 ) ) ;
#21457 = CARTESIAN_POINT ( 'NONE',  ( 10.81189881249999907, 6.242252689847868297, -184.4062500020484094 ) ) ;
#21458 = VERTEX_POINT ( 'NONE', #30211 ) ;
#21459 = CARTESIAN_POINT ( 'NONE',  ( -10.81189881249999729, 6.242252689847871849, -173.2187500020483810 ) ) ;
#21460 = CARTESIAN_POINT ( 'NONE',  ( 4.999999999999992006, -8.660254037844389075, -59.62500000409676204 ) ) ;
#21461 = ADVANCED_FACE ( 'NONE', ( #33239 ), #20044, .F. ) ;
#21462 = CARTESIAN_POINT ( 'NONE',  ( -9.999999999999998224, 1.224646799147353059E-15, -121.6250000040967905 ) ) ;
#21463 = CARTESIAN_POINT ( 'NONE',  ( 10.81189881249999729, 0.000000000000000000, -69.03125000204838102 ) ) ;
#21464 = CARTESIAN_POINT ( 'NONE',  ( -10.81189881249999729, -6.242252689847864744, -51.65625000204838102 ) ) ;
#21465 = VECTOR ( 'NONE', #12376, 1000.000000000000000 ) ;
#21466 = CARTESIAN_POINT ( 'NONE',  ( 10.00000000000000000, 5.773502691896255534, -41.25000000409676204 ) ) ;
#21467 = CARTESIAN_POINT ( 'NONE',  ( 10.81189881249999729, 0.000000000000000000, -2.843750002048367698 ) ) ;
#21468 = CARTESIAN_POINT ( 'NONE',  ( -9.999999999999998224, 1.224646799147353059E-15, -9.125000004096744277 ) ) ;
#21469 = CARTESIAN_POINT ( 'NONE',  ( 7.644554776091147741E-16, 12.48450537969573659, -181.1562500020484094 ) ) ;
#21470 = LOCAL_TIME ( 11, 57, 6.000000000000000000, #434 ) ;
#21471 = CARTESIAN_POINT ( 'NONE',  ( -5.000000000000003553, -8.660254037844383745, -106.3750000040967763 ) ) ;
#21472 = CARTESIAN_POINT ( 'NONE',  ( 9.999999999999998224, 0.000000000000000000, -137.0000000000000000 ) ) ;
#21473 = ORIENTED_EDGE ( 'NONE', *, *, #20639, .T. ) ;
#21474 = LINE ( 'NONE', #38513, #18724 ) ;
#21475 = CARTESIAN_POINT ( 'NONE',  ( -9.999999999999998224, 1.224646799147353059E-15, -105.1250000040967763 ) ) ;
#21476 =( BOUNDED_CURVE ( )  B_SPLINE_CURVE ( 2, ( #422, #33853, #9898, #23073, #30194, #20030, #630 ),
 .UNSPECIFIED., .F., .F. ) 
 B_SPLINE_CURVE_WITH_KNOTS ( ( 3, 2, 2, 3 ),
 ( 0.2985074626865671932, 0.2997512437810946340, 0.3009950248756220192, 0.3022388059701494045 ),
 .UNSPECIFIED. ) 
 CURVE ( )  GEOMETRIC_REPRESENTATION_ITEM ( )  RATIONAL_B_SPLINE_CURVE ( ( 0.9999999999999940048, 0.8660254037844447028, 1.000000000000000000, 0.8660254037844387076, 1.000000000000000000, 0.8660254037844207220, 1.000000000000017986 ) ) 
 REPRESENTATION_ITEM ( '' )  );
#21477 = CARTESIAN_POINT ( 'NONE',  ( 7.070501591499376803E-16, 11.54700538379251284, -195.5000000040968189 ) ) ;
#21478 = AXIS2_PLACEMENT_3D ( 'NONE', #19670, #9541, #30257 ) ;
#21480 = ORIENTED_EDGE ( 'NONE', *, *, #8857, .F. ) ;
#21479 = CARTESIAN_POINT ( 'NONE',  ( 5.405949406249992428, -9.363379034771808662, -75.28125000204838102 ) ) ;
#21481 = CARTESIAN_POINT ( 'NONE',  ( 0.000000000000000000, 0.000000000000000000, -200.0000000000000000 ) ) ;
#21483 = ORIENTED_EDGE ( 'NONE', *, *, #11704, .T. ) ;
#21482 = CARTESIAN_POINT ( 'NONE',  ( -7.423074889580956182, -12.85714285714295890, 52.14285714285716011 ) ) ;
#21484 = VERTEX_POINT ( 'NONE', #19830 ) ;
#21485 = EDGE_CURVE ( 'NONE', #38772, #25832, #13557, .T. ) ;
#21486 = CARTESIAN_POINT ( 'NONE',  ( 10.81189881249999551, -6.242252689847874514, -38.96875000204835970 ) ) ;
#21488 = CARTESIAN_POINT ( 'NONE',  ( 5.000000000000000000, 8.660254037844385522, -74.12500000409677625 ) ) ;
#21487 =( BOUNDED_CURVE ( )  B_SPLINE_CURVE ( 2, ( #17253, #3475, #38, #19652, #13161, #19863, #26355 ),
 .UNSPECIFIED., .F., .F. ) 
 B_SPLINE_CURVE_WITH_KNOTS ( ( 3, 2, 2, 3 ),
 ( 0.3544776119402986980, 0.3557213930348260278, 0.3569651741293533576, 0.3582089552238806873 ),
 .UNSPECIFIED. ) 
 CURVE ( )  GEOMETRIC_REPRESENTATION_ITEM ( )  RATIONAL_B_SPLINE_CURVE ( ( 0.9999999999999820144, 0.8660254037844566932, 1.000000000000000000, 0.8660254037844387076, 1.000000000000000000, 0.8660254037844267172, 1.000000000000011990 ) ) 
 REPRESENTATION_ITEM ( '' )  );
#21489 = CARTESIAN_POINT ( 'NONE',  ( 10.81189881249999907, 6.242252689847868297, -17.90625000204837036 ) ) ;
#21492 = EDGE_CURVE ( 'NONE', #31836, #3056, #14927, .T. ) ;
#21491 = ORIENTED_EDGE ( 'NONE', *, *, #25736, .T. ) ;
#21490 = CARTESIAN_POINT ( 'NONE',  ( -5.405949406250003975, -9.363379034771801557, -60.34375000204835970 ) ) ;
#21493 = CARTESIAN_POINT ( 'NONE',  ( 0.000000000000000000, 20.00000000000000000, -232.0000000000000000 ) ) ;
#21494 = CARTESIAN_POINT ( 'NONE',  ( -9.999999999999998224, 1.224646799147353059E-15, -38.74999999999997868 ) ) ;
#21495 = CARTESIAN_POINT ( 'NONE',  ( 10.81189881249999729, 6.242252689847867408, -193.2187500020484094 ) ) ;
#21496 = CARTESIAN_POINT ( 'NONE',  ( -10.81189881249999729, 6.242252689847871849, -179.2187500020483810 ) ) ;
#21497 = CARTESIAN_POINT ( 'NONE',  ( 10.81189881249999729, 0.000000000000000000, -169.3437500020484094 ) ) ;
#21498 = CONICAL_SURFACE ( 'NONE', #40096, 15.00000000000001421, 0.7853981633974469467 ) ;
#21499 = CARTESIAN_POINT ( 'NONE',  ( 5.405949406249999534, 9.363379034771803333, -175.0937500020484094 ) ) ;
#21500 = CARTESIAN_POINT ( 'NONE',  ( 10.00000000000015632, -5.773502691896169381, -192.6250000000000568 ) ) ;
#21501 = DIRECTION ( 'NONE',  ( -0.000000000000000000, -0.000000000000000000, 1.000000000000000000 ) ) ;
#21502 = CARTESIAN_POINT ( 'NONE',  ( -4.999999999999996447, 8.660254037844387298, -193.5000000000000000 ) ) ;
#21503 = CARTESIAN_POINT ( 'NONE',  ( 5.405949406249992428, -9.363379034771808662, -115.5937500020483810 ) ) ;
#21504 = DIRECTION ( 'NONE',  ( 1.000000000000000000, 0.000000000000000000, 0.000000000000000000 ) ) ;
#21505 = CARTESIAN_POINT ( 'NONE',  ( 5.405949406249999534, 9.363379034771803333, -82.28125000204838102 ) ) ;
#21506 = CARTESIAN_POINT ( 'NONE',  ( 5.405949406249992428, -9.363379034771808662, -93.09375000204838102 ) ) ;
#21507 = CARTESIAN_POINT ( 'NONE',  ( -5.405949406250003975, -9.363379034771801557, -58.84375000204835970 ) ) ;
#21508 = CARTESIAN_POINT ( 'NONE',  ( 5.405949406249999534, 9.363379034771803333, -71.78125000204838102 ) ) ;
#21509 = CARTESIAN_POINT ( 'NONE',  ( 5.000000000000000000, 8.660254037844385522, -156.6250000040967905 ) ) ;
#21510 = CARTESIAN_POINT ( 'NONE',  ( -9.999999999999998224, 1.224646799147353059E-15, -121.2500000000000000 ) ) ;
#21511 = EDGE_CURVE ( 'NONE', #10167, #2239, #24588, .T. ) ;
#21512 = CARTESIAN_POINT ( 'NONE',  ( 5.405949406249999534, 9.363379034771803333, -149.7812500020483810 ) ) ;
#21513 = CARTESIAN_POINT ( 'NONE',  ( -5.405949406249996869, 9.363379034771805109, -161.5312500020484094 ) ) ;
#21514 = CARTESIAN_POINT ( 'NONE',  ( 4.999999999999992006, -8.660254037844389075, -13.12500000409674783 ) ) ;
#21515 = CARTESIAN_POINT ( 'NONE',  ( -4.999999999999996447, 8.660254037844387298, -159.3750000040967905 ) ) ;
#21516 = CARTESIAN_POINT ( 'NONE',  ( 7.644554776091147741E-16, 12.48450537969573659, -98.46875000204839523 ) ) ;
#21517 = ORIENTED_EDGE ( 'NONE', *, *, #37405, .T. ) ;
#21518 = CARTESIAN_POINT ( 'NONE',  ( 9.999999999999996447, -5.773502691896262640, -68.12500000000000000 ) ) ;
#21519 = CARTESIAN_POINT ( 'NONE',  ( 5.405949406249992428, -9.363379034771808662, -196.5937500020484094 ) ) ;
#21520 = CARTESIAN_POINT ( 'NONE',  ( 9.999999999999998224, 0.000000000000000000, -83.37500000409677625 ) ) ;
#21521 = CARTESIAN_POINT ( 'NONE',  ( -5.950676495627904572, -8.268445900970100126, -180.0000000000000000 ) ) ;
#21522 = CARTESIAN_POINT ( 'NONE',  ( -10.81189881249999729, 6.242252689847871849, -89.40625000204838102 ) ) ;
#21523 = CARTESIAN_POINT ( 'NONE',  ( -10.81189881249999729, -6.242252689847864744, -74.15625000204836681 ) ) ;
#21524 = CARTESIAN_POINT ( 'NONE',  ( 9.999999999999996447, -5.773502691896262640, -67.00000000409677625 ) ) ;
#21525 = CARTESIAN_POINT ( 'NONE',  ( 0.000000000000000000, 0.000000000000000000, -200.0000000000000000 ) ) ;
#21526 = CARTESIAN_POINT ( 'NONE',  ( 5.405949406249992428, -9.363379034771808662, -25.59375000204835970 ) ) ;
#21527 = ORIENTED_EDGE ( 'NONE', *, *, #9863, .F. ) ;
#21528 = CARTESIAN_POINT ( 'NONE',  ( 7.644554776091147741E-16, 12.48450537969573659, -199.1562500020484094 ) ) ;
#21529 = CARTESIAN_POINT ( 'NONE',  ( -10.81189881249999907, -6.242252689847864744, -23.15625000204837747 ) ) ;
#21530 = CARTESIAN_POINT ( 'NONE',  ( -2.293366432827344421E-15, -12.48450537969573659, -10.71875000204836503 ) ) ;
#21531 = CARTESIAN_POINT ( 'NONE',  ( -2.121150477449813534E-15, -11.54700538379251284, -118.2500000040968189 ) ) ;
#21532 = CARTESIAN_POINT ( 'NONE',  ( -2.293366432827344421E-15, -12.48450537969573659, -142.7187500020484094 ) ) ;
#21533 = CARTESIAN_POINT ( 'NONE',  ( 9.999999999999998224, 0.000000000000000000, -49.99999999999998579 ) ) ;
#21534 = CARTESIAN_POINT ( 'NONE',  ( 7.071067811865472841, -7.071067811865472841, -200.0000000000000000 ) ) ;
#21535 = CARTESIAN_POINT ( 'NONE',  ( 5.405949406249999534, 9.363379034771803333, -128.7812500020483810 ) ) ;
#21536 = AXIS2_PLACEMENT_3D ( 'NONE', #18461, #11766, #32282 ) ;
#21537 = CARTESIAN_POINT ( 'NONE',  ( -9.999999999999998224, 1.224646799147353059E-15, -182.7500000000000000 ) ) ;
#21538 = CARTESIAN_POINT ( 'NONE',  ( 7.070501591499376803E-16, 11.54700538379251284, -120.1249999999999858 ) ) ;
#21540 = EDGE_LOOP ( 'NONE', ( #24073, #39988, #976, #5247 ) ) ;
#21539 = CARTESIAN_POINT ( 'NONE',  ( -10.81189881249999729, 1.324075727343319199E-15, -108.7812500020483810 ) ) ;
#21541 = CARTESIAN_POINT ( 'NONE',  ( 10.00000000000025402, -5.773502691896113426, -154.0000000040967905 ) ) ;
#21542 = ORIENTED_EDGE ( 'NONE', *, *, #30976, .T. ) ;
#21543 = ORIENTED_EDGE ( 'NONE', *, *, #42108, .F. ) ;
#21544 = CARTESIAN_POINT ( 'NONE',  ( 7.644554776091147741E-16, 12.48450537969573659, -37.15625000204836681 ) ) ;
#21545 = DATE_AND_TIME ( #21324, #39355 ) ;
#21546 = VECTOR ( 'NONE', #30188, 1000.000000000000000 ) ;
#21547 = CARTESIAN_POINT ( 'NONE',  ( 5.405949406249992428, -9.363379034771808662, -90.09375000204838102 ) ) ;
#21548 = DIRECTION ( 'NONE',  ( 0.000000000000000000, -0.000000000000000000, -1.000000000000000000 ) ) ;
#21549 = CARTESIAN_POINT ( 'NONE',  ( -4.999999999999996447, 8.660254037844387298, -113.9999999999999858 ) ) ;
#21550 = CARTESIAN_POINT ( 'NONE',  ( -4.999999999999996447, 8.660254037844387298, -123.0000000000000000 ) ) ;
#21551 = CARTESIAN_POINT ( 'NONE',  ( 10.81189881249999551, -6.242252689847874514, -163.6562500020484094 ) ) ;
#21552 = CARTESIAN_POINT ( 'NONE',  ( -2.121150477449813534E-15, -11.54700538379251284, -77.37500000000000000 ) ) ;
#21553 = ADVANCED_FACE ( 'NONE', ( #24161 ), #34080, .T. ) ;
#21554 = CARTESIAN_POINT ( 'NONE',  ( -5.405949406249996869, 9.363379034771805109, -117.8437500020483810 ) ) ;
#21555 = CARTESIAN_POINT ( 'NONE',  ( 5.405949406249992428, -9.363379034771808662, -88.59375000204838102 ) ) ;
#21556 = CARTESIAN_POINT ( 'NONE',  ( 5.405949406249992428, -9.363379034771808662, -0.2812500020483721386 ) ) ;
#21557 = CARTESIAN_POINT ( 'NONE',  ( 5.405949406249992428, -9.363379034771808662, -190.5937500020484094 ) ) ;
#21558 = CARTESIAN_POINT ( 'NONE',  ( -10.81189881249999729, 6.242252689847871849, -93.90625000204839523 ) ) ;
#21559 = CARTESIAN_POINT ( 'NONE',  ( 10.00000000000000000, 5.773502691896255534, -177.7500000040967905 ) ) ;
#21560 = CARTESIAN_POINT ( 'NONE',  ( 10.81189881249999729, 6.242252689847867408, -173.9062500020483810 ) ) ;
#21561 = CARTESIAN_POINT ( 'NONE',  ( -9.999999999999479527, -5.773502691896549521, -70.50000000409677625 ) ) ;
#21562 = CARTESIAN_POINT ( 'NONE',  ( -5.405949406250003975, -9.363379034771801557, -173.0312500020484094 ) ) ;
#21563 = CARTESIAN_POINT ( 'NONE',  ( 7.644554776091147741E-16, 12.48450537969573659, -188.6562500020484379 ) ) ;
#21564 = CARTESIAN_POINT ( 'NONE',  ( -5.405949406249996869, 9.363379034771805109, -54.84375000204835970 ) ) ;
#21565 = CARTESIAN_POINT ( 'NONE',  ( 9.999999999999998224, 0.000000000000000000, -167.3750000040967905 ) ) ;
#21566 = CARTESIAN_POINT ( 'NONE',  ( 10.81189881249999551, -6.242252689847874514, -0.1562500020483646446 ) ) ;
#21567 = CARTESIAN_POINT ( 'NONE',  ( -5.405949406249996869, 9.363379034771805109, -17.34375000204835260 ) ) ;
#21568 = FACE_OUTER_BOUND ( 'NONE', #32335, .T. ) ;
#21569 = CARTESIAN_POINT ( 'NONE',  ( 7.644554776091147741E-16, 12.48450537969573659, -120.9687500020483952 ) ) ;
#21570 = CARTESIAN_POINT ( 'NONE',  ( -9.999999999999998224, 5.773502691896259087, -95.87499999999998579 ) ) ;
#21571 = CARTESIAN_POINT ( 'NONE',  ( -2.293366432827344421E-15, -12.48450537969573659, -18.40625000204837391 ) ) ;
#21572 = CARTESIAN_POINT ( 'NONE',  ( -4.999999999999996447, 8.660254037844387298, -102.3750000040967905 ) ) ;
#21573 =( BOUNDED_CURVE ( )  B_SPLINE_CURVE ( 2, ( #23581, #36729, #17499, #7167, #20319, #30272, #33720 ),
 .UNSPECIFIED., .F., .F. ) 
 B_SPLINE_CURVE_WITH_KNOTS ( ( 3, 2, 2, 3 ),
 ( 0.3656716417910448325, 0.3669154228855722177, 0.3681592039800996030, 0.3694029850746269883 ),
 .UNSPECIFIED. ) 
 CURVE ( )  GEOMETRIC_REPRESENTATION_ITEM ( )  RATIONAL_B_SPLINE_CURVE ( ( 0.9999999999999940048, 0.8660254037844447028, 1.000000000000000000, 0.8660254037844387076, 1.000000000000000000, 0.8660254037844267172, 1.000000000000011990 ) ) 
 REPRESENTATION_ITEM ( '' )  );
#21574 = CARTESIAN_POINT ( 'NONE',  ( 9.999999999999998224, 0.000000000000000000, -149.3750000040967905 ) ) ;
#21575 = CARTESIAN_POINT ( 'NONE',  ( -2.121150477449813534E-15, -11.54700538379251284, -53.37499999999997868 ) ) ;
#21576 = CARTESIAN_POINT ( 'NONE',  ( -10.81189881249999729, 6.242252689847871849, -116.4062500020483810 ) ) ;
#21577 = CARTESIAN_POINT ( 'NONE',  ( -10.81189881249999729, -6.242252689847864744, -98.15625000204840944 ) ) ;
#21578 = EDGE_CURVE ( 'NONE', #10744, #900, #7749, .T. ) ;
#21579 = ORIENTED_EDGE ( 'NONE', *, *, #34123, .F. ) ;
#21580 = CARTESIAN_POINT ( 'NONE',  ( 4.999999999999992006, -8.660254037844389075, -89.62500000409677625 ) ) ;
#21581 = DIRECTION ( 'NONE',  ( -0.000000000000000000, 1.000000000000000000, -0.000000000000000000 ) ) ;
#21582 = CARTESIAN_POINT ( 'NONE',  ( 5.405949406249999534, 9.363379034771803333, -155.7812500020484094 ) ) ;
#21583 = CARTESIAN_POINT ( 'NONE',  ( 10.81189881249999551, -6.242252689847874514, -53.96875000204837391 ) ) ;
#21584 = ORIENTED_EDGE ( 'NONE', *, *, #37047, .F. ) ;
#21585 = CARTESIAN_POINT ( 'NONE',  ( -9.999999999999998224, 5.773502691896259087, -25.37499999999997868 ) ) ;
#21586 = CARTESIAN_POINT ( 'NONE',  ( -2.293366432827344421E-15, -12.48450537969573659, -28.90625000204835615 ) ) ;
#21587 = CARTESIAN_POINT ( 'NONE',  ( 10.00000000000000000, 5.773502691896255534, -162.3750000000000000 ) ) ;
#21588 = CARTESIAN_POINT ( 'NONE',  ( 0.000000000000000000, 0.000000000000000000, -200.0000000000000000 ) ) ;
#21589 = CARTESIAN_POINT ( 'NONE',  ( 4.999999999999992006, -8.660254037844389075, -20.62500000409675494 ) ) ;
#21590 = DIRECTION ( 'NONE',  ( 1.000000000000000000, 0.000000000000000000, 0.000000000000000000 ) ) ;
#21591 = CARTESIAN_POINT ( 'NONE',  ( 10.81189881249999551, -6.242252689847874514, -136.6562500020484094 ) ) ;
#21592 = CARTESIAN_POINT ( 'NONE',  ( 6.569145736382243861, 8.192416893213705364, -5.257032284683799044E-15 ) ) ;
#21593 = DIRECTION ( 'NONE',  ( -0.000000000000000000, -0.000000000000000000, 1.000000000000000000 ) ) ;
#21594 = ORIENTED_EDGE ( 'NONE', *, *, #7221, .T. ) ;
#21595 = CARTESIAN_POINT ( 'NONE',  ( 10.81189881249999551, -6.242252689847874514, -58.65625000204838813 ) ) ;
#21596 = PERSON_AND_ORGANIZATION_ROLE ( 'creator' ) ;
#21598 = ORIENTED_EDGE ( 'NONE', *, *, #24376, .F. ) ;
#21597 = ORIENTED_EDGE ( 'NONE', *, *, #18843, .T. ) ;
#21599 = DIRECTION ( 'NONE',  ( 0.000000000000000000, -0.000000000000000000, -1.000000000000000000 ) ) ;
#21600 = CARTESIAN_POINT ( 'NONE',  ( -5.000000000000003553, -8.660254037844383745, -197.8750000040967905 ) ) ;
#21602 = EDGE_CURVE ( 'NONE', #13677, #23116, #19348, .T. ) ;
#21601 = CARTESIAN_POINT ( 'NONE',  ( -5.405949406249996869, 9.363379034771805109, -155.3437500020483810 ) ) ;
#21603 = CARTESIAN_POINT ( 'NONE',  ( 7.644554776091147741E-16, 12.48450537969573659, -190.1562500020484094 ) ) ;
#21604 = CARTESIAN_POINT ( 'NONE',  ( -5.405949406250003975, -9.363379034771801557, -3.343750002048367698 ) ) ;
#21605 = CARTESIAN_POINT ( 'NONE',  ( -2.293366432827344421E-15, -12.48450537969573659, -136.7187500020483810 ) ) ;
#21606 = CARTESIAN_POINT ( 'NONE',  ( -5.405949406250003975, -9.363379034771801557, -99.53125000204839523 ) ) ;
#21607 = CARTESIAN_POINT ( 'NONE',  ( 5.405949406249992428, -9.363379034771808662, -112.5937500020483810 ) ) ;
#21608 = CARTESIAN_POINT ( 'NONE',  ( 9.999999999999998224, 0.000000000000000000, -161.0000000000000000 ) ) ;
#21609 = CARTESIAN_POINT ( 'NONE',  ( 10.81189881249999551, -6.242252689847874514, -120.1562500020483810 ) ) ;
#21610 = CARTESIAN_POINT ( 'NONE',  ( -5.405949406249996869, 9.363379034771805109, -5.343750002048369474 ) ) ;
#21611 = CARTESIAN_POINT ( 'NONE',  ( -5.405949406249996869, 9.363379034771805109, -122.3437500020483952 ) ) ;
#21612 = CARTESIAN_POINT ( 'NONE',  ( 10.81189881249999551, -6.242252689847874514, -196.6562500020484094 ) ) ;
#21613 =( BOUNDED_CURVE ( )  B_SPLINE_CURVE ( 2, ( #34731, #492, #14629, #1494, #24589, #25022, #18087 ),
 .UNSPECIFIED., .F., .F. ) 
 B_SPLINE_CURVE_WITH_KNOTS ( ( 3, 2, 2, 3 ),
 ( 0.1417910447761193959, 0.1430348258706467535, 0.1442786069651741387, 0.1455223880597014963 ),
 .UNSPECIFIED. ) 
 CURVE ( )  GEOMETRIC_REPRESENTATION_ITEM ( )  RATIONAL_B_SPLINE_CURVE ( ( 1.000000000000000000, 0.8660254037844387076, 1.000000000000000000, 0.8660254037844387076, 1.000000000000000000, 0.8660254037844387076, 1.000000000000000000 ) ) 
 REPRESENTATION_ITEM ( '' )  );
#21614 = CYLINDRICAL_SURFACE ( 'NONE', #13014, 9.999999999999998224 ) ;
#21615 = CARTESIAN_POINT ( 'NONE',  ( -9.999999999999998224, 5.773502691896259087, -145.3750000000000000 ) ) ;
#21616 = CARTESIAN_POINT ( 'NONE',  ( 10.00000000000000000, 5.773502691896255534, -12.37499999999996803 ) ) ;
#21617 = CARTESIAN_POINT ( 'NONE',  ( 5.405949406249992428, -9.363379034771808662, -78.09375000204838102 ) ) ;
#21618 = CARTESIAN_POINT ( 'NONE',  ( -10.81189881249999729, 1.324075727343319199E-15, -57.59375000204835970 ) ) ;
#21619 = CARTESIAN_POINT ( 'NONE',  ( -5.000000000000003553, -8.660254037844383745, -188.8750000040967905 ) ) ;
#21620 = CARTESIAN_POINT ( 'NONE',  ( 10.81189881249999907, 6.242252689847868297, -34.40625000204836681 ) ) ;
#21621 = CARTESIAN_POINT ( 'NONE',  ( 7.644554776091147741E-16, 12.48450537969573659, -33.96875000204835260 ) ) ;
#21622 = DIRECTION ( 'NONE',  ( -0.000000000000000000, -0.000000000000000000, 1.000000000000000000 ) ) ;
#21623 = CARTESIAN_POINT ( 'NONE',  ( 10.81189881249999907, 6.242252689847868297, -149.7187500020483810 ) ) ;
#21624 = CARTESIAN_POINT ( 'NONE',  ( -2.121150477449813534E-15, -11.54700538379251284, -120.8749999999999858 ) ) ;
#21625 = ADVANCED_FACE ( 'NONE', ( #10964 ), #37660, .T. ) ;
#21626 = CARTESIAN_POINT ( 'NONE',  ( 10.00000000000051159, -5.773502691895965988, -101.5000000040967763 ) ) ;
#21627 = CARTESIAN_POINT ( 'NONE',  ( 7.070501591499377789E-16, 11.54700538379251284, -73.62499999999995737 ) ) ;
#21628 = CARTESIAN_POINT ( 'NONE',  ( -5.405949406249996869, 9.363379034771805109, -143.5312500020483810 ) ) ;
#21629 = CARTESIAN_POINT ( 'NONE',  ( -2.293366432827344421E-15, -12.48450537969573659, -6.406250002048362369 ) ) ;
#21630 = ORIENTED_EDGE ( 'NONE', *, *, #37289, .F. ) ;
#21631 = CARTESIAN_POINT ( 'NONE',  ( -10.81189881249999729, 6.242252689847871849, -105.9062500020483810 ) ) ;
#21632 = CARTESIAN_POINT ( 'NONE',  ( 9.999999999999998224, 0.000000000000000000, -117.8750000040967905 ) ) ;
#21633 = CARTESIAN_POINT ( 'NONE',  ( 9.999999999999998224, 0.000000000000000000, -55.99999999999996447 ) ) ;
#21634 = CARTESIAN_POINT ( 'NONE',  ( 10.81189881249999551, -6.242252689847874514, -77.96875000204838102 ) ) ;
#21635 = CARTESIAN_POINT ( 'NONE',  ( -4.999999999999996447, 8.660254037844387298, -24.37500000409675849 ) ) ;
#21636 = CARTESIAN_POINT ( 'NONE',  ( 5.405949406249999534, 9.363379034771803333, -46.28125000204838813 ) ) ;
#21637 = CARTESIAN_POINT ( 'NONE',  ( 0.000000000000000000, 0.000000000000000000, -200.0000000000000000 ) ) ;
#21638 = CARTESIAN_POINT ( 'NONE',  ( 7.644554776091147741E-16, 12.48450537969573659, -145.1562500020484094 ) ) ;
#21639 = CARTESIAN_POINT ( 'NONE',  ( 10.81189881249999551, -6.242252689847874514, -127.4687500020483810 ) ) ;
#21640 = CARTESIAN_POINT ( 'NONE',  ( 4.999999999999992006, -8.660254037844389075, -164.6250000040967905 ) ) ;
#21641 = FACE_OUTER_BOUND ( 'NONE', #5682, .T. ) ;
#21642 = ORIENTED_EDGE ( 'NONE', *, *, #38786, .T. ) ;
#21643 = VERTEX_POINT ( 'NONE', #37953 ) ;
#21644 = ORIENTED_EDGE ( 'NONE', *, *, #26989, .F. ) ;
#21645 = CARTESIAN_POINT ( 'NONE',  ( 9.999999999999998224, 0.000000000000000000, -200.0000000000000000 ) ) ;
#21646 = CARTESIAN_POINT ( 'NONE',  ( -5.405949406250003975, -9.363379034771801557, -180.3437500020483810 ) ) ;
#21647 = CARTESIAN_POINT ( 'NONE',  ( 7.644554776091147741E-16, 12.48450537969573659, -33.96875000204834549 ) ) ;
#21648 = CARTESIAN_POINT ( 'NONE',  ( 4.999999999999992006, -8.660254037844389075, -130.1250000040967620 ) ) ;
#21649 = CARTESIAN_POINT ( 'NONE',  ( 5.405949406249992428, -9.363379034771808662, -172.5937500020484094 ) ) ;
#21650 = CARTESIAN_POINT ( 'NONE',  ( -2.293366432827344421E-15, -12.48450537969573659, -151.7187500020483810 ) ) ;
#21651 = CARTESIAN_POINT ( 'NONE',  ( -4.999999999999996447, 8.660254037844387298, -178.5000000000000000 ) ) ;
#21652 = CARTESIAN_POINT ( 'NONE',  ( 5.405949406249999534, 9.363379034771803333, -131.5937500020483810 ) ) ;
#21653 = CARTESIAN_POINT ( 'NONE',  ( -10.81189881249999729, 6.242252689847871849, -138.9062500020484094 ) ) ;
#21654 = CARTESIAN_POINT ( 'NONE',  ( -10.81189881249999729, -6.242252689847864744, -154.9687500020484094 ) ) ;
#21655 = CARTESIAN_POINT ( 'NONE',  ( 7.070501591499376803E-16, 11.54700538379251284, -127.6249999999999858 ) ) ;
#21656 = CARTESIAN_POINT ( 'NONE',  ( -9.999999999999998224, 1.224646799147353059E-15, -33.12500000409676915 ) ) ;
#21657 = CARTESIAN_POINT ( 'NONE',  ( 9.999999999999996447, -5.773502691896262640, -173.1250000000000000 ) ) ;
#21658 = SHAPE_REPRESENTATION ( 'BR-597', ( #3510, #11063, #35920, #13124, #29709, #42107, #26949 ), #41425 ) ;
#21659 = CARTESIAN_POINT ( 'NONE',  ( -2.293366432827344421E-15, -12.48450537969573659, -82.71875000204838102 ) ) ;
#21660 = CARTESIAN_POINT ( 'NONE',  ( -2.121150477449813534E-15, -11.54700538379251284, -82.25000000409676204 ) ) ;
#21661 = CARTESIAN_POINT ( 'NONE',  ( -10.81189881249999729, 6.242252689847871849, -56.40625000204837391 ) ) ;
#21662 = CARTESIAN_POINT ( 'NONE',  ( -4.999999999999996447, 8.660254037844387298, -133.5000000000000000 ) ) ;
#21663 = CARTESIAN_POINT ( 'NONE',  ( 10.81189881249999729, 0.000000000000000000, -172.3437500020484094 ) ) ;
#21664 = CARTESIAN_POINT ( 'NONE',  ( 7.644554776091147741E-16, 12.48450537969573659, -116.6562500020483952 ) ) ;
#21665 = CARTESIAN_POINT ( 'NONE',  ( -5.405949406250003975, -9.363379034771801557, -146.0312500020483810 ) ) ;
#21666 = CARTESIAN_POINT ( 'NONE',  ( -2.293366432827344421E-15, -12.48450537969573659, -48.40625000204838102 ) ) ;
#21667 = CARTESIAN_POINT ( 'NONE',  ( 4.999999999999992006, -8.660254037844389075, -118.1250000040967905 ) ) ;
#21668 = CARTESIAN_POINT ( 'NONE',  ( -5.000000000000003553, -8.660254037844383745, -99.99999999999998579 ) ) ;
#21669 = VERTEX_POINT ( 'NONE', #40310 ) ;
#21670 = CARTESIAN_POINT ( 'NONE',  ( -10.81189881249999729, -6.242252689847864744, -125.1562500020483810 ) ) ;
#21671 = CARTESIAN_POINT ( 'NONE',  ( -5.000000000000003553, -8.660254037844383745, -146.8750000040967905 ) ) ;
#21672 = CARTESIAN_POINT ( 'NONE',  ( 7.070501591499376803E-16, 11.54700538379251284, -192.5000000040968189 ) ) ;
#21673 = CARTESIAN_POINT ( 'NONE',  ( -2.293366432827344421E-15, -12.48450537969573659, -178.9062500020484379 ) ) ;
#21674 = EDGE_LOOP ( 'NONE', ( #1855, #23816, #18661, #15019 ) ) ;
#21675 = CARTESIAN_POINT ( 'NONE',  ( -10.81189881249999729, 6.242252689847871849, -170.2187500020483810 ) ) ;
#21676 = CARTESIAN_POINT ( 'NONE',  ( -9.999999999999998224, 5.773502691896259087, -57.25000000409677625 ) ) ;
#21677 = EDGE_CURVE ( 'NONE', #27421, #31328, #23768, .T. ) ;
#21678 = CARTESIAN_POINT ( 'NONE',  ( 0.000000000000000000, 20.00000000000000000, -232.0000000000000000 ) ) ;
#21679 = CARTESIAN_POINT ( 'NONE',  ( 9.999999999999998224, 0.000000000000000000, -155.0000000000000000 ) ) ;
#21680 = ADVANCED_FACE ( 'NONE', ( #8179 ), #4714, .T. ) ;
#21681 = CARTESIAN_POINT ( 'NONE',  ( -10.81189881249999907, -6.242252689847864744, -68.15625000204839523 ) ) ;
#21682 = CARTESIAN_POINT ( 'NONE',  ( -9.999999999999998224, 1.224646799147353059E-15, -43.62500000409677625 ) ) ;
#21683 = CARTESIAN_POINT ( 'NONE',  ( -2.293366432827344421E-15, -12.48450537969573659, -1.718750002048352377 ) ) ;
#21684 = CARTESIAN_POINT ( 'NONE',  ( 10.00000000000051159, -5.773502691895965988, -148.0000000040967905 ) ) ;
#21685 = CARTESIAN_POINT ( 'NONE',  ( 5.405949406249992428, -9.363379034771808662, -168.2812500020484094 ) ) ;
#21686 = DIRECTION ( 'NONE',  ( -0.000000000000000000, -0.000000000000000000, 1.000000000000000000 ) ) ;
#21687 = CARTESIAN_POINT ( 'NONE',  ( 7.070501591499376803E-16, 11.54700538379251284, -148.6250000000000000 ) ) ;
#21688 = EDGE_LOOP ( 'NONE', ( #2813, #39943, #10374, #35405 ) ) ;
#21689 = CARTESIAN_POINT ( 'NONE',  ( -9.999999999999998224, 1.224646799147353059E-15, -13.24999999999995559 ) ) ;
#21690 = CARTESIAN_POINT ( 'NONE',  ( 9.999999999999998224, 0.000000000000000000, -194.0000000000000000 ) ) ;
#21691 = DIRECTION ( 'NONE',  ( 1.000000000000000000, 0.000000000000000000, 0.000000000000000000 ) ) ;
#21693 = VERTEX_POINT ( 'NONE', #20683 ) ;
#21692 = CARTESIAN_POINT ( 'NONE',  ( -10.81189881249999729, 1.324075727343319199E-15, -80.28125000204838102 ) ) ;
#21694 = DIRECTION ( 'NONE',  ( 0.000000000000000000, 0.000000000000000000, 1.000000000000000000 ) ) ;
#21696 = ORIENTED_EDGE ( 'NONE', *, *, #22141, .T. ) ;
#21695 = CARTESIAN_POINT ( 'NONE',  ( 4.999999999999992006, -8.660254037844389075, -119.2500000000000000 ) ) ;
#21697 = ORIENTED_EDGE ( 'NONE', *, *, #4064, .T. ) ;
#21698 = CARTESIAN_POINT ( 'NONE',  ( -5.405949406249996869, 9.363379034771805109, -35.34375000204836681 ) ) ;
#21699 = CARTESIAN_POINT ( 'NONE',  ( 0.000000000000000000, 0.000000000000000000, -99.99999999999998579 ) ) ;
#21700 = CARTESIAN_POINT ( 'NONE',  ( 5.405949406249992428, -9.363379034771808662, -9.281250002048352599 ) ) ;
#21702 = VERTEX_POINT ( 'NONE', #40520 ) ;
#21701 = CARTESIAN_POINT ( 'NONE',  ( -5.405949406249996869, 9.363379034771805109, -59.34375000204835970 ) ) ;
#21703 = CARTESIAN_POINT ( 'NONE',  ( 9.999999999999998224, 0.000000000000000000, -108.8750000040967763 ) ) ;
#21704 = CARTESIAN_POINT ( 'NONE',  ( 9.999999999999996447, -5.773502691896262640, -35.12499999999996447 ) ) ;
#21705 = CARTESIAN_POINT ( 'NONE',  ( -10.81189881249999729, 1.324075727343319199E-15, -198.5937500020484094 ) ) ;
#21706 = CARTESIAN_POINT ( 'NONE',  ( -5.405949406250003975, -9.363379034771801557, -175.8437500020483810 ) ) ;
#21707 = CARTESIAN_POINT ( 'NONE',  ( 7.644554776091147741E-16, 12.48450537969573659, -153.9687500020484094 ) ) ;
#21708 = CARTESIAN_POINT ( 'NONE',  ( 5.000000000000000000, 8.660254037844385522, -43.74999999999998579 ) ) ;
#21709 = CARTESIAN_POINT ( 'NONE',  ( 9.999999999999998224, 0.000000000000000000, -75.49999999999998579 ) ) ;
#21710 = VECTOR ( 'NONE', #17997, 1000.000000000000114 ) ;
#21711 = FACE_OUTER_BOUND ( 'NONE', #18028, .T. ) ;
#21712 = CARTESIAN_POINT ( 'NONE',  ( -10.00000000000000000, -5.773502691896251982, -191.6250000000000284 ) ) ;
#21713 = CARTESIAN_POINT ( 'NONE',  ( -5.405949406250003975, -9.363379034771801557, -103.8437500020483810 ) ) ;
#21714 = CARTESIAN_POINT ( 'NONE',  ( -9.999999999999998224, 1.224646799147353059E-15, -140.7500000000000000 ) ) ;
#21715 = CARTESIAN_POINT ( 'NONE',  ( 10.81189881249999551, -6.242252689847874514, -82.65625000204836681 ) ) ;
#21716 = CARTESIAN_POINT ( 'NONE',  ( 10.81189881249999551, -6.242252689847874514, -94.46875000204838102 ) ) ;
#21717 = CARTESIAN_POINT ( 'NONE',  ( 5.405949406249992428, -9.363379034771808662, -72.28125000204838102 ) ) ;
#21718 = CARTESIAN_POINT ( 'NONE',  ( 5.000000000000000000, 8.660254037844385522, -147.6250000040967905 ) ) ;
#21719 = CARTESIAN_POINT ( 'NONE',  ( -4.999999999999996447, 8.660254037844387298, -123.0000000000000000 ) ) ;
#21720 = CARTESIAN_POINT ( 'NONE',  ( 5.405949406249992428, -9.363379034771808662, -148.7812500020483810 ) ) ;
#21721 = CARTESIAN_POINT ( 'NONE',  ( -10.81189881249999907, -6.242252689847864744, -167.1562500020483810 ) ) ;
#21722 = LINE ( 'NONE', #15235, #18554 ) ;
#21723 = CARTESIAN_POINT ( 'NONE',  ( 10.00000000000006040, -5.773502691896226224, -197.1250000000000284 ) ) ;
#21724 = CARTESIAN_POINT ( 'NONE',  ( 10.81189881249999729, 0.000000000000000000, -100.3437500020483810 ) ) ;
#21725 = ORIENTED_EDGE ( 'NONE', *, *, #836, .T. ) ;
#21726 = CARTESIAN_POINT ( 'NONE',  ( -5.000000000000003553, -8.660254037844383745, -65.49999999999997158 ) ) ;
#21727 = CARTESIAN_POINT ( 'NONE',  ( -5.405949406249996869, 9.363379034771805109, -194.3437500020484094 ) ) ;
#21728 = CARTESIAN_POINT ( 'NONE',  ( 7.070501591499377789E-16, 11.54700538379251284, -86.00000000409676204 ) ) ;
#21729 = EDGE_CURVE ( 'NONE', #39897, #30831, #580, .T. ) ;
#21730 = CARTESIAN_POINT ( 'NONE',  ( 6.072958700806868393, -8.826036754033463438, -180.0000000000000853 ) ) ;
#21731 = FACE_OUTER_BOUND ( 'NONE', #35280, .T. ) ;
#21732 = CARTESIAN_POINT ( 'NONE',  ( 5.405949406249992428, -9.363379034771808662, -93.28125000204838102 ) ) ;
#21733 = CONICAL_SURFACE ( 'NONE', #36204, 14.99999999999998579, 0.7853981633974466137 ) ;
#21734 = CARTESIAN_POINT ( 'NONE',  ( -2.293366432827344421E-15, -12.48450537969573659, -75.40625000204838102 ) ) ;
#21735 =( BOUNDED_CURVE ( )  B_SPLINE_CURVE ( 2, ( #27255, #8273, #17737, #31155, #37830, #40395, #14931 ),
 .UNSPECIFIED., .F., .F. ) 
 B_SPLINE_CURVE_WITH_KNOTS ( ( 3, 2, 2, 3 ),
 ( 0.9701492537313435305, 0.9713930348258709158, 0.9726368159203981900, 0.9738805970149255753 ),
 .UNSPECIFIED. ) 
 CURVE ( )  GEOMETRIC_REPRESENTATION_ITEM ( )  RATIONAL_B_SPLINE_CURVE ( ( 0.9999999999999761302, 0.8660254037844625774, 1.000000000000000000, 0.8660254037844387076, 1.000000000000000000, 0.8660254037844148378, 1.000000000000023981 ) ) 
 REPRESENTATION_ITEM ( '' )  );
#21736 = EDGE_CURVE ( 'NONE', #6545, #5513, #14016, .T. ) ;
#21737 = CARTESIAN_POINT ( 'NONE',  ( 9.999999999999998224, 0.000000000000000000, -65.37500000409676204 ) ) ;
#21738 = CYLINDRICAL_SURFACE ( 'NONE', #8001, 9.999999999999998224 ) ;
#21739 = CARTESIAN_POINT ( 'NONE',  ( 10.81189881249999729, 0.000000000000000000, -29.84375000204836326 ) ) ;
#21740 = CARTESIAN_POINT ( 'NONE',  ( -5.405949406249996869, 9.363379034771805109, -194.5312500020484094 ) ) ;
#21741 = EDGE_CURVE ( 'NONE', #5570, #36180, #8209, .T. ) ;
#21742 = CARTESIAN_POINT ( 'NONE',  ( 5.405949406249999534, 9.363379034771803333, -19.28125000204835970 ) ) ;
#21743 = CARTESIAN_POINT ( 'NONE',  ( 10.81189881249999551, -6.242252689847874514, -7.468750002048351710 ) ) ;
#21744 = CARTESIAN_POINT ( 'NONE',  ( 9.999999999999998224, 0.000000000000000000, -161.0000000000000000 ) ) ;
#21745 = CARTESIAN_POINT ( 'NONE',  ( -10.81189881249999729, 1.324075727343319199E-15, -144.5937500020483810 ) ) ;
#21746 = CARTESIAN_POINT ( 'NONE',  ( 10.00000000000051159, -5.773502691895965988, -50.12499999999997158 ) ) ;
#21747 = CC_DESIGN_DATE_AND_TIME_ASSIGNMENT ( #34775, #13863, ( #10394 ) ) ;
#21748 = CARTESIAN_POINT ( 'NONE',  ( 9.999999999999998224, 0.000000000000000000, -111.8750000040967763 ) ) ;
#21749 = AXIS2_PLACEMENT_3D ( 'NONE', #29589, #6706, #3051 ) ;
#21750 = CARTESIAN_POINT ( 'NONE',  ( -10.00000000000000000, -5.773502691896251982, -175.1249999999999716 ) ) ;
#21752 = VERTEX_POINT ( 'NONE', #22399 ) ;
#21751 = CARTESIAN_POINT ( 'NONE',  ( -5.405949406250003975, -9.363379034771801557, -98.03125000204839523 ) ) ;
#21753 = CARTESIAN_POINT ( 'NONE',  ( -9.999999999999998224, 1.224646799147353059E-15, -115.6250000040967905 ) ) ;
#21754 = EDGE_CURVE ( 'NONE', #5836, #2425, #12647, .T. ) ;
#21755 = EDGE_LOOP ( 'NONE', ( #15655, #29540, #32370, #36130 ) ) ;
#21756 = VERTEX_POINT ( 'NONE', #2767 ) ;
#21757 = CARTESIAN_POINT ( 'NONE',  ( -10.81189881249999729, 1.324075727343319199E-15, -30.78125000204837036 ) ) ;
#21758 = PERSON_AND_ORGANIZATION_ROLE ( 'creator' ) ;
#21759 = EDGE_CURVE ( 'NONE', #34823, #24099, #2561, .T. ) ;
#21760 = CARTESIAN_POINT ( 'NONE',  ( 5.405949406249999534, 9.363379034771803333, -89.59375000204838102 ) ) ;
#21761 = CARTESIAN_POINT ( 'NONE',  ( 0.000000000000000000, 0.000000000000000000, -200.0000000000000000 ) ) ;
#21762 = CARTESIAN_POINT ( 'NONE',  ( 9.600329599501245426, 4.034346693190136612, -99.99999999999994316 ) ) ;
#21763 = CARTESIAN_POINT ( 'NONE',  ( 7.070501591499376803E-16, 11.54700538379251284, -105.5000000040967763 ) ) ;
#21764 = CARTESIAN_POINT ( 'NONE',  ( 5.405949406249992428, -9.363379034771808662, -165.2812500020484094 ) ) ;
#21765 = CARTESIAN_POINT ( 'NONE',  ( 10.00000000000000000, 5.773502691896255534, -9.750000004096756712 ) ) ;
#21766 = CARTESIAN_POINT ( 'NONE',  ( 9.999999999999998224, 0.000000000000000000, -198.5000000000000000 ) ) ;
#21767 = CARTESIAN_POINT ( 'NONE',  ( -5.405949406250003975, -9.363379034771801557, -115.8437500020483810 ) ) ;
#21768 = AXIS2_PLACEMENT_3D ( 'NONE', #1461, #824, #27570 ) ;
#21769 = CARTESIAN_POINT ( 'NONE',  ( 5.405949406249992428, -9.363379034771808662, -87.09375000204836681 ) ) ;
#21770 = CARTESIAN_POINT ( 'NONE',  ( -10.81189881249999729, -6.242252689847864744, -5.156250002048356151 ) ) ;
#21771 = CARTESIAN_POINT ( 'NONE',  ( 5.405949406249992428, -9.363379034771808662, -193.5937500020484094 ) ) ;
#21772 = CARTESIAN_POINT ( 'NONE',  ( -5.405949406250003975, -9.363379034771801557, -95.03125000204838102 ) ) ;
#21773 = CARTESIAN_POINT ( 'NONE',  ( -4.999999999999996447, 8.660254037844387298, -175.8750000040967905 ) ) ;
#21774 = CARTESIAN_POINT ( 'NONE',  ( -5.405949406250003975, -9.363379034771801557, -173.0312500020484094 ) ) ;
#21775 = CARTESIAN_POINT ( 'NONE',  ( 9.999999999998969713, 5.773502691896851502, -102.7500000040967620 ) ) ;
#21776 = CARTESIAN_POINT ( 'NONE',  ( 5.405949406249992428, -9.363379034771808662, -174.2812500020484094 ) ) ;
#21777 = CARTESIAN_POINT ( 'NONE',  ( 7.644554776091147741E-16, 12.48450537969573659, -185.6562500020484094 ) ) ;
#21778 = CARTESIAN_POINT ( 'NONE',  ( 5.405949406249999534, 9.363379034771803333, -43.09375000204837391 ) ) ;
#21779 = CARTESIAN_POINT ( 'NONE',  ( 5.000000000000000000, 8.660254037844385522, -161.1250000040967905 ) ) ;
#21780 = CARTESIAN_POINT ( 'NONE',  ( 5.405949406249992428, -9.363379034771808662, -4.781250002048375691 ) ) ;
#21781 = CARTESIAN_POINT ( 'NONE',  ( 10.81189881249999729, 0.000000000000000000, -13.34375000204834905 ) ) ;
#21782 = CARTESIAN_POINT ( 'NONE',  ( 5.000000000000000000, 8.660254037844385522, -54.24999999999996447 ) ) ;
#21783 = CARTESIAN_POINT ( 'NONE',  ( 5.405949406249999534, 9.363379034771803333, -121.0937500020483952 ) ) ;
#21784 = CARTESIAN_POINT ( 'NONE',  ( -5.000000000000003553, -8.660254037844383745, -89.49999999999998579 ) ) ;
#21785 = CARTESIAN_POINT ( 'NONE',  ( -10.81189881249999729, 1.324075727343319199E-15, -23.28125000204836326 ) ) ;
#21786 = CARTESIAN_POINT ( 'NONE',  ( 4.999999999999992006, -8.660254037844389075, -106.1250000040967763 ) ) ;
#21787 = CARTESIAN_POINT ( 'NONE',  ( 4.999999999999992006, -8.660254037844389075, -149.6250000040967905 ) ) ;
#21788 = CARTESIAN_POINT ( 'NONE',  ( -2.121150477449813534E-15, -11.54700538379251284, -51.87499999999997158 ) ) ;
#21789 = CARTESIAN_POINT ( 'NONE',  ( 10.81189881249999907, 6.242252689847868297, -113.9062500020483952 ) ) ;
#21790 = CARTESIAN_POINT ( 'NONE',  ( 10.81189881249999729, 6.242252689847867408, -98.90625000204839523 ) ) ;
#21791 = VERTEX_POINT ( 'NONE', #12035 ) ;
#21792 = CARTESIAN_POINT ( 'NONE',  ( 9.999999999999998224, 0.000000000000000000, -90.87500000409677625 ) ) ;
#21793 = CARTESIAN_POINT ( 'NONE',  ( -10.00000000000154188, 5.773502691895366468, -28.75000000409670520 ) ) ;
#21794 = CARTESIAN_POINT ( 'NONE',  ( -5.405949406250003975, -9.363379034771801557, -155.0312500020484094 ) ) ;
#21795 = CARTESIAN_POINT ( 'NONE',  ( -10.81189881249999729, 6.242252689847871849, -53.21875000204836681 ) ) ;
#21796 = ORIENTED_EDGE ( 'NONE', *, *, #36841, .F. ) ;
#21797 = CARTESIAN_POINT ( 'NONE',  ( -9.999999999999998224, 1.224646799147353059E-15, -23.74999999999996447 ) ) ;
#21798 = CARTESIAN_POINT ( 'NONE',  ( 10.81189881249999729, 0.000000000000000000, -25.53125000204836681 ) ) ;
#21799 = CARTESIAN_POINT ( 'NONE',  ( -9.999999999999998224, 5.773502691896259087, -151.3750000000000000 ) ) ;
#21800 = CARTESIAN_POINT ( 'NONE',  ( -4.999999999999996447, 8.660254037844387298, -16.87500000409675138 ) ) ;
#21801 = AXIS2_PLACEMENT_3D ( 'NONE', #9493, #2189, #22660 ) ;
#21802 = CARTESIAN_POINT ( 'NONE',  ( 9.999999999999998224, 0.000000000000000000, -80.37500000409677625 ) ) ;
#21803 = ADVANCED_FACE ( 'NONE', ( #9229 ), #25228, .T. ) ;
#21804 = CARTESIAN_POINT ( 'NONE',  ( -10.81189881249999729, 1.324075727343319199E-15, -126.7812500020483668 ) ) ;
#21805 = CARTESIAN_POINT ( 'NONE',  ( -4.999999999999996447, 8.660254037844387298, -75.37500000409677625 ) ) ;
#21806 = VERTEX_POINT ( 'NONE', #38375 ) ;
#21807 = CARTESIAN_POINT ( 'NONE',  ( -5.405949406249996869, 9.363379034771805109, -62.53125000204837391 ) ) ;
#21808 = DATE_TIME_ROLE ( 'creation_date' ) ;
#21809 = CARTESIAN_POINT ( 'NONE',  ( 5.405949406249999534, 9.363379034771803333, -107.5937500020483810 ) ) ;
#21811 = ORIENTED_EDGE ( 'NONE', *, *, #34843, .F. ) ;
#21810 = EDGE_LOOP ( 'NONE', ( #32585, #19195, #15574, #25474 ) ) ;
#21812 = CARTESIAN_POINT ( 'NONE',  ( -9.999999999998969713, -5.773502691896847949, -85.50000000409674783 ) ) ;
#21813 = CARTESIAN_POINT ( 'NONE',  ( -9.999999999999998224, 1.224646799147353059E-15, -116.7499999999999858 ) ) ;
#21814 = CARTESIAN_POINT ( 'NONE',  ( 5.405949406249992428, -9.363379034771808662, -157.5937500020483810 ) ) ;
#21815 = CARTESIAN_POINT ( 'NONE',  ( -10.81189881249999729, 1.324075727343319199E-15, -185.2812500020484094 ) ) ;
#21816 = CARTESIAN_POINT ( 'NONE',  ( 5.405949406249999534, 9.363379034771803333, -10.09375000204834549 ) ) ;
#21817 = CARTESIAN_POINT ( 'NONE',  ( -10.81189881249999729, 6.242252689847871849, -140.2187500020483810 ) ) ;
#21818 =( BOUNDED_CURVE ( )  B_SPLINE_CURVE ( 2, ( #20728, #27431, #8007, #40354, #23985, #30252, #7363 ),
 .UNSPECIFIED., .F., .F. ) 
 B_SPLINE_CURVE_WITH_KNOTS ( ( 3, 2, 2, 3 ),
 ( 0.1791044776119403437, 0.1803482587064677289, 0.1815920398009950587, 0.1828358208955224162 ),
 .UNSPECIFIED. ) 
 CURVE ( )  GEOMETRIC_REPRESENTATION_ITEM ( )  RATIONAL_B_SPLINE_CURVE ( ( 0.9999999999999940048, 0.8660254037844447028, 1.000000000000000000, 0.8660254037844387076, 1.000000000000000000, 0.8660254037844357100, 1.000000000000003109 ) ) 
 REPRESENTATION_ITEM ( '' )  );
#21819 = CARTESIAN_POINT ( 'NONE',  ( 7.644554776091147741E-16, 12.48450537969573659, -110.4687500020483668 ) ) ;
#21820 = CARTESIAN_POINT ( 'NONE',  ( 9.999999999999998224, 0.000000000000000000, -149.3750000040967905 ) ) ;
#21821 = CARTESIAN_POINT ( 'NONE',  ( -10.81189881249999907, -6.242252689847864744, -116.1562500020483952 ) ) ;
#21822 = CARTESIAN_POINT ( 'NONE',  ( 10.00000000000000000, 5.773502691896255534, -198.7500000040968189 ) ) ;
#21823 = CARTESIAN_POINT ( 'NONE',  ( -10.81189881249999729, -6.242252689847864744, -123.4687500020483952 ) ) ;
#21824 = CARTESIAN_POINT ( 'NONE',  ( 10.81189881249999729, 0.000000000000000000, -190.5312500020484094 ) ) ;
#21825 = CARTESIAN_POINT ( 'NONE',  ( 0.000000000000000000, 0.000000000000000000, -99.99999999999998579 ) ) ;
#21826 = CC_DESIGN_APPROVAL ( #2230, ( #16278 ) ) ;
#21827 = CARTESIAN_POINT ( 'NONE',  ( 9.999999999999996447, -5.773502691896262640, -149.1250000000000000 ) ) ;
#21828 = CARTESIAN_POINT ( 'NONE',  ( -9.999999999999998224, 5.773502691896259087, -16.37499999999997158 ) ) ;
#21829 = CARTESIAN_POINT ( 'NONE',  ( 7.644554776091147741E-16, 12.48450537969573659, -68.46875000204838102 ) ) ;
#21830 = CARTESIAN_POINT ( 'NONE',  ( -5.405949406249996869, 9.363379034771805109, -60.84375000204836681 ) ) ;
#21831 = CARTESIAN_POINT ( 'NONE',  ( -9.999999999999998224, 1.224646799147353059E-15, -184.6250000040967905 ) ) ;
#21832 = CARTESIAN_POINT ( 'NONE',  ( -10.81189881249999729, 1.324075727343319199E-15, -27.78125000204837036 ) ) ;
#21833 = CARTESIAN_POINT ( 'NONE',  ( 7.644554776091147741E-16, 12.48450537969573659, -41.46875000204835970 ) ) ;
#21834 = CARTESIAN_POINT ( 'NONE',  ( 7.070501591499376803E-16, 11.54700538379251284, -95.00000000409677625 ) ) ;
#21835 = CARTESIAN_POINT ( 'NONE',  ( 10.81189881249999551, -6.242252689847874514, -149.9687500020483810 ) ) ;
#21836 = CARTESIAN_POINT ( 'NONE',  ( -9.999999999999998224, 1.224646799147353059E-15, -112.2499999999999858 ) ) ;
#21837 = DIRECTION ( 'NONE',  ( 1.000000000000000000, 0.000000000000000000, 0.000000000000000000 ) ) ;
#21838 = CARTESIAN_POINT ( 'NONE',  ( -5.000000000000003553, -8.660254037844383745, -72.99999999999998579 ) ) ;
#21839 = CARTESIAN_POINT ( 'NONE',  ( -10.81189881249999729, 6.242252689847871849, -141.9062500020484094 ) ) ;
#21840 = CARTESIAN_POINT ( 'NONE',  ( -10.81189881249999729, -6.242252689847864744, -11.15625000204838457 ) ) ;
#21841 = ORIENTED_EDGE ( 'NONE', *, *, #15733, .T. ) ;
#21842 = CARTESIAN_POINT ( 'NONE',  ( 0.000000000000000000, 20.00000000000000000, -235.0000000000000000 ) ) ;
#21843 = CARTESIAN_POINT ( 'NONE',  ( 9.999999999999996447, -5.773502691896262640, -119.5000000040967763 ) ) ;
#21844 = CARTESIAN_POINT ( 'NONE',  ( 0.000000000000000000, 0.000000000000000000, -240.0000000000000000 ) ) ;
#21845 = CARTESIAN_POINT ( 'NONE',  ( -5.405949406250003975, -9.363379034771801557, -76.84375000204838102 ) ) ;
#21846 = CARTESIAN_POINT ( 'NONE',  ( 10.00000000000000000, 5.773502691896255534, -52.87499999999997868 ) ) ;
#21847 = CARTESIAN_POINT ( 'NONE',  ( 10.00000000000000000, 5.773502691896255534, -27.75000000409677980 ) ) ;
#21848 = PRODUCT ( 'retaining plate', 'retaining plate', '', ( #9272 ) ) ;
#21849 = CARTESIAN_POINT ( 'NONE',  ( -4.999999999999996447, 8.660254037844387298, -61.49999999999997158 ) ) ;
#21850 = CARTESIAN_POINT ( 'NONE',  ( -10.81189881249999729, 6.242252689847871849, -41.40625000204836681 ) ) ;
#21851 = LINE ( 'NONE', #24893, #29003 ) ;
#21852 = CARTESIAN_POINT ( 'NONE',  ( -10.81189881249999729, 1.324075727343319199E-15, -144.7812500020483810 ) ) ;
#21853 = CARTESIAN_POINT ( 'NONE',  ( 10.81189881249999729, 0.000000000000000000, -130.3437500020484094 ) ) ;
#21854 = CARTESIAN_POINT ( 'NONE',  ( 4.999999999999992006, -8.660254037844389075, -65.24999999999997158 ) ) ;
#21855 = CARTESIAN_POINT ( 'NONE',  ( -5.000000000000003553, -8.660254037844383745, -127.3750000040967905 ) ) ;
#21856 = ORIENTED_EDGE ( 'NONE', *, *, #8284, .F. ) ;
#21857 = VERTEX_POINT ( 'NONE', #15689 ) ;
#21858 = ORIENTED_EDGE ( 'NONE', *, *, #23848, .F. ) ;
#21859 = EDGE_CURVE ( 'NONE', #36790, #41954, #28678, .T. ) ;
#21860 = CARTESIAN_POINT ( 'NONE',  ( -2.121150477449813534E-15, -11.54700538379251284, -7.250000004096746054 ) ) ;
#21861 =( BOUNDED_CURVE ( )  B_SPLINE_CURVE ( 2, ( #35787, #18730, #22829, #2351, #12660, #2138, #39010 ),
 .UNSPECIFIED., .F., .F. ) 
 B_SPLINE_CURVE_WITH_KNOTS ( ( 3, 2, 2, 3 ),
 ( 0.3731343283582090331, 0.3743781094527363629, 0.3756218905472638037, 0.3768656716417911334 ),
 .UNSPECIFIED. ) 
 CURVE ( )  GEOMETRIC_REPRESENTATION_ITEM ( )  RATIONAL_B_SPLINE_CURVE ( ( 0.9999999999999940048, 0.8660254037844447028, 1.000000000000000000, 0.8660254037844387076, 1.000000000000000000, 0.8660254037844267172, 1.000000000000011990 ) ) 
 REPRESENTATION_ITEM ( '' )  );
#21862 = CARTESIAN_POINT ( 'NONE',  ( 7.644554776091147741E-16, 12.48450537969573659, -182.4687500020484094 ) ) ;
#21863 = CARTESIAN_POINT ( 'NONE',  ( 10.81189881249999551, -6.242252689847874514, -34.46875000204835260 ) ) ;
#21864 = DIRECTION ( 'NONE',  ( -0.000000000000000000, -0.000000000000000000, 1.000000000000000000 ) ) ;
#21865 = CARTESIAN_POINT ( 'NONE',  ( -10.81189881249999729, -6.242252689847864744, -166.9687500020484094 ) ) ;
#21866 = CARTESIAN_POINT ( 'NONE',  ( 10.81189881249999729, 0.000000000000000000, -154.3437500020483810 ) ) ;
#21867 = CARTESIAN_POINT ( 'NONE',  ( -10.00000000000012790, -5.773502691896177375, -176.6250000000000284 ) ) ;
#21868 = CARTESIAN_POINT ( 'NONE',  ( 10.81189881249999729, 0.000000000000000000, -133.3437500020484094 ) ) ;
#21869 = CARTESIAN_POINT ( 'NONE',  ( -10.81189881249999907, -6.242252689847864744, -140.1562500020484094 ) ) ;
#21870 = CARTESIAN_POINT ( 'NONE',  ( -10.81189881249999729, 6.242252689847871849, -143.2187500020483810 ) ) ;
#21871 = CARTESIAN_POINT ( 'NONE',  ( 0.000000000000000000, 0.000000000000000000, -200.0000000000000000 ) ) ;
#21872 =( BOUNDED_CURVE ( )  B_SPLINE_CURVE ( 2, ( #38104, #9171, #28829, #5304, #12393, #18457, #22342 ),
 .UNSPECIFIED., .F., .F. ) 
 B_SPLINE_CURVE_WITH_KNOTS ( ( 3, 2, 2, 3 ),
 ( 0.1380597014925373234, 0.1393034825870646809, 0.1405472636815920384, 0.1417910447761193959 ),
 .UNSPECIFIED. ) 
 CURVE ( )  GEOMETRIC_REPRESENTATION_ITEM ( )  RATIONAL_B_SPLINE_CURVE ( ( 1.000000000000000000, 0.8660254037844387076, 1.000000000000000000, 0.8660254037844387076, 1.000000000000000000, 0.8660254037844387076, 1.000000000000000000 ) ) 
 REPRESENTATION_ITEM ( '' )  );
#21873 = CARTESIAN_POINT ( 'NONE',  ( 9.999999999999872102, 5.773502691896329253, -169.8750000000000000 ) ) ;
#21874 = CARTESIAN_POINT ( 'NONE',  ( -9.999999999999998224, 1.224646799147353059E-15, -175.2500000000000284 ) ) ;
#21875 = CARTESIAN_POINT ( 'NONE',  ( -2.293366432827344421E-15, -12.48450537969573659, -78.21875000204838102 ) ) ;
#21876 = DIRECTION ( 'NONE',  ( -0.000000000000000000, -0.000000000000000000, 1.000000000000000000 ) ) ;
#21877 = CARTESIAN_POINT ( 'NONE',  ( 5.405949406249992428, -9.363379034771808662, -46.78125000204838813 ) ) ;
#21878 = CARTESIAN_POINT ( 'NONE',  ( 0.000000000000000000, 0.000000000000000000, -200.0000000000000000 ) ) ;
#21879 = CARTESIAN_POINT ( 'NONE',  ( -10.81189881249999907, -6.242252689847864744, -166.9687500020484094 ) ) ;
#21880 = CARTESIAN_POINT ( 'NONE',  ( -10.81189881249999907, -6.242252689847864744, -113.1562500020483952 ) ) ;
#21881 = CARTESIAN_POINT ( 'NONE',  ( 5.405949406249992428, -9.363379034771808662, -147.2812500020483810 ) ) ;
#21882 = CARTESIAN_POINT ( 'NONE',  ( 10.00000000000102318, -5.773502691895667560, -29.12499999999995381 ) ) ;
#21883 = CARTESIAN_POINT ( 'NONE',  ( -5.405949406249996869, 9.363379034771805109, -43.03125000204838102 ) ) ;
#21884 = CARTESIAN_POINT ( 'NONE',  ( -9.999999999999998224, 1.224646799147353059E-15, -124.6250000040967763 ) ) ;
#21885 = CARTESIAN_POINT ( 'NONE',  ( 9.999999999999998224, 0.000000000000000000, -100.9999999999999858 ) ) ;
#21886 = ORIENTED_EDGE ( 'NONE', *, *, #23947, .F. ) ;
#21887 = CARTESIAN_POINT ( 'NONE',  ( 5.405949406249999534, 9.363379034771803333, -130.2812500020483810 ) ) ;
#21888 = CARTESIAN_POINT ( 'NONE',  ( -9.999999999999998224, 5.773502691896259087, -142.7500000040967905 ) ) ;
#21889 = ADVANCED_FACE ( 'NONE', ( #42022 ), #4985, .F. ) ;
#21890 = CARTESIAN_POINT ( 'NONE',  ( -10.81189881249999729, 1.324075727343319199E-15, -183.7812500020484094 ) ) ;
#21891 = ORIENTED_EDGE ( 'NONE', *, *, #35192, .F. ) ;
#21892 = CARTESIAN_POINT ( 'NONE',  ( 5.405949406249999534, 9.363379034771803333, -170.5937500020484094 ) ) ;
#21893 = CARTESIAN_POINT ( 'NONE',  ( 7.070501591499377789E-16, 11.54700538379251284, -53.00000000409676915 ) ) ;
#21894 = CARTESIAN_POINT ( 'NONE',  ( 4.999999999999992006, -8.660254037844389075, -155.2500000000000000 ) ) ;
#21895 = CARTESIAN_POINT ( 'NONE',  ( 5.405949406249992428, -9.363379034771808662, -70.78125000204838102 ) ) ;
#21896 = CARTESIAN_POINT ( 'NONE',  ( 9.999999999998969713, 5.773502691896851502, -9.750000004096735395 ) ) ;
#21897 = CARTESIAN_POINT ( 'NONE',  ( 5.405949406249992428, -9.363379034771808662, -166.7812500020484094 ) ) ;
#21898 = VECTOR ( 'NONE', #27556, 1000.000000000000000 ) ;
#21899 = CARTESIAN_POINT ( 'NONE',  ( 7.070501591499376803E-16, 11.54700538379251284, -64.62499999999998579 ) ) ;
#21900 = VECTOR ( 'NONE', #11183, 1000.000000000000000 ) ;
#21901 = ORIENTED_EDGE ( 'NONE', *, *, #8538, .F. ) ;
#21902 = DIRECTION ( 'NONE',  ( 0.000000000000000000, 0.000000000000000000, 1.000000000000000000 ) ) ;
#21903 = CARTESIAN_POINT ( 'NONE',  ( -9.999999999999998224, 1.224646799147353059E-15, -52.62500000409675494 ) ) ;
#21904 = CARTESIAN_POINT ( 'NONE',  ( 9.999999999999998224, 0.000000000000000000, -117.8750000040967905 ) ) ;
#21906 = ORIENTED_EDGE ( 'NONE', *, *, #39107, .T. ) ;
#21905 = CARTESIAN_POINT ( 'NONE',  ( 10.81189881249999551, -6.242252689847874514, -81.15625000204839523 ) ) ;
#21908 = ORIENTED_EDGE ( 'NONE', *, *, #27480, .F. ) ;
#21907 = CARTESIAN_POINT ( 'NONE',  ( -10.00000000000019362, -5.773502691896140959, -178.5000000040968189 ) ) ;
#21909 = ORIENTED_EDGE ( 'NONE', *, *, #12806, .F. ) ;
#21910 = CARTESIAN_POINT ( 'NONE',  ( 10.81189881249999729, 6.242252689847867408, -29.71875000204834549 ) ) ;
#21911 = CARTESIAN_POINT ( 'NONE',  ( -9.999999999999998224, 1.224646799147353059E-15, -122.7500000000000000 ) ) ;
#21912 = CARTESIAN_POINT ( 'NONE',  ( -10.81189881249999729, 1.324075727343319199E-15, -3.781250002048375247 ) ) ;
#21914 = ORIENTED_EDGE ( 'NONE', *, *, #38889, .T. ) ;
#21913 = CARTESIAN_POINT ( 'NONE',  ( -5.405949406249996869, 9.363379034771805109, -53.34375000204835970 ) ) ;
#21915 = CARTESIAN_POINT ( 'NONE',  ( 9.999999999999998224, 0.000000000000000000, -51.49999999999996447 ) ) ;
#21916 = EDGE_CURVE ( 'NONE', #24037, #10798, #31718, .T. ) ;
#21917 = CARTESIAN_POINT ( 'NONE',  ( -10.00000000000000000, -5.773502691896251982, -35.62499999999996447 ) ) ;
#21918 = CARTESIAN_POINT ( 'NONE',  ( 5.405949406249992428, -9.363379034771808662, -184.5937500020483810 ) ) ;
#21919 = CARTESIAN_POINT ( 'NONE',  ( -5.405949406250003975, -9.363379034771801557, -177.3437500020483810 ) ) ;
#21920 = CARTESIAN_POINT ( 'NONE',  ( 7.644554776091147741E-16, 12.48450537969573659, -158.4687500020483810 ) ) ;
#21921 = CARTESIAN_POINT ( 'NONE',  ( 10.81189881249999551, -6.242252689847874514, -167.9687500020483810 ) ) ;
#21922 = CARTESIAN_POINT ( 'NONE',  ( 9.999999999999998224, 0.000000000000000000, -200.0000000000000000 ) ) ;
#21923 = CARTESIAN_POINT ( 'NONE',  ( 5.000000000000000000, 8.660254037844385522, -132.2499999999999716 ) ) ;
#21924 = CARTESIAN_POINT ( 'NONE',  ( 10.00000000000000000, 5.773502691896255534, -198.3750000000000000 ) ) ;
#21925 = CARTESIAN_POINT ( 'NONE',  ( -2.293366432827344421E-15, -12.48450537969573659, -102.2187500020483952 ) ) ;
#21926 = CARTESIAN_POINT ( 'NONE',  ( 0.000000000000000000, 0.000000000000000000, -200.0000000000000000 ) ) ;
#21927 = VECTOR ( 'NONE', #11773, 1000.000000000000000 ) ;
#21928 = CARTESIAN_POINT ( 'NONE',  ( 5.405949406249999534, 9.363379034771803333, -79.28125000204838102 ) ) ;
#21929 = CARTESIAN_POINT ( 'NONE',  ( 10.81189881249999729, 0.000000000000000000, -94.34375000204838102 ) ) ;
#21930 = AXIS2_PLACEMENT_3D ( 'NONE', #24483, #34410, #30319 ) ;
#21931 = CARTESIAN_POINT ( 'NONE',  ( 10.81189881249999729, 0.000000000000000000, -70.53125000204838102 ) ) ;
#21932 = CARTESIAN_POINT ( 'NONE',  ( -9.999999999999998224, 5.773502691896259087, -148.7500000040967905 ) ) ;
#21933 = CARTESIAN_POINT ( 'NONE',  ( 5.000000000000000000, 8.660254037844385522, -124.7500000000000000 ) ) ;
#21934 = ORIENTED_EDGE ( 'NONE', *, *, #5893, .F. ) ;
#21935 = CARTESIAN_POINT ( 'NONE',  ( -10.81189881249999729, 1.324075727343319199E-15, -150.7812500020483810 ) ) ;
#21936 = CARTESIAN_POINT ( 'NONE',  ( -10.81189881249999907, -6.242252689847864744, -162.6562500020483810 ) ) ;
#21937 = CARTESIAN_POINT ( 'NONE',  ( 7.070501591499376803E-16, 11.54700538379251284, -98.00000000409677625 ) ) ;
#21938 = LINE ( 'NONE', #25402, #1330 ) ;
#21939 = CARTESIAN_POINT ( 'NONE',  ( 10.81189881249999907, 6.242252689847868297, -98.71875000204838102 ) ) ;
#21940 = ORIENTED_EDGE ( 'NONE', *, *, #41105, .T. ) ;
#21941 = CARTESIAN_POINT ( 'NONE',  ( -9.999999999999998224, 5.773502691896259087, -62.87499999999996447 ) ) ;
#21942 = CARTESIAN_POINT ( 'NONE',  ( 10.81189881249999907, 6.242252689847868297, 0.09374999795164208616 ) ) ;
#21943 = CARTESIAN_POINT ( 'NONE',  ( 4.999999999999992006, -8.660254037844389075, -74.62500000409677625 ) ) ;
#21944 = CARTESIAN_POINT ( 'NONE',  ( -9.999999999999998224, 1.224646799147353059E-15, -85.62500000409677625 ) ) ;
#21945 = CARTESIAN_POINT ( 'NONE',  ( 4.999999999999992006, -8.660254037844389075, -144.7500000000000000 ) ) ;
#21946 = CARTESIAN_POINT ( 'NONE',  ( -10.81189881249999907, -6.242252689847864744, -92.15625000204839523 ) ) ;
#21947 = CARTESIAN_POINT ( 'NONE',  ( -10.81189881249999729, 1.324075727343319199E-15, -77.28125000204838102 ) ) ;
#21948 = CARTESIAN_POINT ( 'NONE',  ( -4.999999999999996447, 8.660254037844387298, -67.87500000409677625 ) ) ;
#21949 = CARTESIAN_POINT ( 'NONE',  ( -11.54700538379251817, 20.00000000000000355, 45.00000000000009237 ) ) ;
#21950 = CARTESIAN_POINT ( 'NONE',  ( 5.405949406249999534, 9.363379034771803333, -23.59375000204835970 ) ) ;
#21951 = EDGE_LOOP ( 'NONE', ( #10956, #27895, #32795, #14442 ) ) ;
#21952 = CARTESIAN_POINT ( 'NONE',  ( -5.405949406249996869, 9.363379034771805109, -196.0312500020484094 ) ) ;
#21953 = CARTESIAN_POINT ( 'NONE',  ( 5.405949406249992428, -9.363379034771808662, -16.78125000204835970 ) ) ;
#21954 = CARTESIAN_POINT ( 'NONE',  ( 10.81189881249999551, -6.242252689847874514, -2.968750002048361925 ) ) ;
#21955 = CARTESIAN_POINT ( 'NONE',  ( 9.999999999999742428, 5.773502691896404748, -186.7500000040967905 ) ) ;
#21956 = CARTESIAN_POINT ( 'NONE',  ( 7.070501591499376803E-16, 11.54700538379251284, -192.1250000000000284 ) ) ;
#21957 = LINE ( 'NONE', #35772, #39679 ) ;
#21958 = CARTESIAN_POINT ( 'NONE',  ( -4.999999999999996447, 8.660254037844387298, -177.0000000000000000 ) ) ;
#21959 = CARTESIAN_POINT ( 'NONE',  ( 9.999999999999998224, 0.000000000000000000, -106.9999999999999858 ) ) ;
#21961 = VERTEX_POINT ( 'NONE', #34255 ) ;
#21960 = CARTESIAN_POINT ( 'NONE',  ( -10.81189881249999729, 6.242252689847871849, -105.9062500020483810 ) ) ;
#21962 = CARTESIAN_POINT ( 'NONE',  ( -9.999999999999872102, -5.773502691896326589, -162.0000000040967620 ) ) ;
#21963 = ORIENTED_EDGE ( 'NONE', *, *, #31149, .F. ) ;
#21964 = VERTEX_POINT ( 'NONE', #38482 ) ;
#21965 = CARTESIAN_POINT ( 'NONE',  ( -10.81189881249999729, 1.324075727343319199E-15, -32.28125000204837391 ) ) ;
#21966 = APPROVAL_STATUS ( 'not_yet_approved' ) ;
#21967 = CARTESIAN_POINT ( 'NONE',  ( 5.405949406249992428, -9.363379034771808662, -78.09375000204838102 ) ) ;
#21968 = DIRECTION ( 'NONE',  ( -0.000000000000000000, -0.000000000000000000, 1.000000000000000000 ) ) ;
#21969 = EDGE_CURVE ( 'NONE', #35880, #18233, #19581, .T. ) ;
#21970 = EDGE_CURVE ( 'NONE', #36790, #1002, #5963, .T. ) ;
#21971 = ADVANCED_FACE ( 'NONE', ( #4668 ), #8131, .T. ) ;
#21972 = EDGE_CURVE ( 'NONE', #34874, #16149, #36112, .T. ) ;
#21973 = CARTESIAN_POINT ( 'NONE',  ( 9.999999999999998224, 0.000000000000000000, -156.8750000040967905 ) ) ;
#21974 = CARTESIAN_POINT ( 'NONE',  ( -5.405949406249996869, 9.363379034771805109, -161.5312500020484094 ) ) ;
#21975 = CARTESIAN_POINT ( 'NONE',  ( 9.999999999999996447, -5.773502691896262640, -13.00000000409675849 ) ) ;
#21976 = CARTESIAN_POINT ( 'NONE',  ( 0.000000000000000000, 0.000000000000000000, -176.9999999999999432 ) ) ;
#21977 = CARTESIAN_POINT ( 'NONE',  ( -5.405949406249996869, 9.363379034771805109, -126.8437500020483952 ) ) ;
#21978 = CARTESIAN_POINT ( 'NONE',  ( 5.405949406249992428, -9.363379034771808662, -117.0937500020483810 ) ) ;
#21979 = CC_DESIGN_PERSON_AND_ORGANIZATION_ASSIGNMENT ( #16741, #13708, ( #25992 ) ) ;
#21980 = CARTESIAN_POINT ( 'NONE',  ( -2.293366432827344421E-15, -12.48450537969573659, -87.21875000204838102 ) ) ;
#21981 = CARTESIAN_POINT ( 'NONE',  ( -10.81189881249999729, 6.242252689847871849, -192.7187500020483810 ) ) ;
#21982 = CARTESIAN_POINT ( 'NONE',  ( -5.405949406250003975, -9.363379034771801557, -93.53125000204838102 ) ) ;
#21983 = CARTESIAN_POINT ( 'NONE',  ( -5.000000000000003553, -8.660254037844383745, -172.3750000040968189 ) ) ;
#21984 = CARTESIAN_POINT ( 'NONE',  ( -2.293366432827344421E-15, -12.48450537969573659, -168.4062500020484379 ) ) ;
#21985 =( BOUNDED_CURVE ( )  B_SPLINE_CURVE ( 2, ( #8802, #11808, #1910, #5350, #41592, #14391, #28459 ),
 .UNSPECIFIED., .F., .F. ) 
 B_SPLINE_CURVE_WITH_KNOTS ( ( 3, 2, 2, 3 ),
 ( 0.1119402985074627876, 0.1131840796019901035, 0.1144278606965174333, 0.1156716417910447492 ),
 .UNSPECIFIED. ) 
 CURVE ( )  GEOMETRIC_REPRESENTATION_ITEM ( )  RATIONAL_B_SPLINE_CURVE ( ( 0.9999999999999894529, 0.8660254037844491437, 1.000000000000000000, 0.8660254037844387076, 1.000000000000000000, 0.8660254037844417052, 0.9999999999999970024 ) ) 
 REPRESENTATION_ITEM ( '' )  );
#21986 = CARTESIAN_POINT ( 'NONE',  ( -5.000000000000003553, -8.660254037844383745, -151.0000000000000000 ) ) ;
#21987 = CARTESIAN_POINT ( 'NONE',  ( -10.81189881249999729, 1.324075727343319199E-15, -177.7812500020484094 ) ) ;
#21988 = CARTESIAN_POINT ( 'NONE',  ( 10.81189881249999729, 0.000000000000000000, -189.0312500020484094 ) ) ;
#21989 = CARTESIAN_POINT ( 'NONE',  ( 5.405949406249999534, 9.363379034771803333, -41.59375000204837391 ) ) ;
#21990 = CARTESIAN_POINT ( 'NONE',  ( 10.00000000000000000, 5.773502691896255534, -165.7500000040967905 ) ) ;
#21991 = CARTESIAN_POINT ( 'NONE',  ( -5.405949406249996869, 9.363379034771805109, -1.031250002048372805 ) ) ;
#21992 = CARTESIAN_POINT ( 'NONE',  ( 5.405949406249992428, -9.363379034771808662, -12.09375000204834727 ) ) ;
#21993 = CARTESIAN_POINT ( 'NONE',  ( -9.999999999999998224, 1.224646799147353059E-15, -162.1250000040967905 ) ) ;
#21994 = CARTESIAN_POINT ( 'NONE',  ( -10.81189881249999729, 6.242252689847871849, -123.7187500020483952 ) ) ;
#21995 = CARTESIAN_POINT ( 'NONE',  ( -2.121150477449813534E-15, -11.54700538379251284, -86.37499999999997158 ) ) ;
#21996 = CARTESIAN_POINT ( 'NONE',  ( -5.405949406250003975, -9.363379034771801557, -20.03125000204836326 ) ) ;
#21997 = CARTESIAN_POINT ( 'NONE',  ( -9.999999999999998224, 1.224646799147353059E-15, -103.6250000040967763 ) ) ;
#21998 = EDGE_CURVE ( 'NONE', #8116, #35398, #21225, .T. ) ;
#21999 = AXIS2_PLACEMENT_3D ( 'NONE', #21878, #41712, #14740 ) ;
#22000 = CARTESIAN_POINT ( 'NONE',  ( 9.999999999999998224, 0.000000000000000000, -200.0000000000000000 ) ) ;
#22001 = CARTESIAN_POINT ( 'NONE',  ( -10.81189881249999907, -6.242252689847864744, -114.6562500020483952 ) ) ;
#22002 = CARTESIAN_POINT ( 'NONE',  ( 10.81189881249999729, 0.000000000000000000, -97.53125000204839523 ) ) ;
#22003 = ORIENTED_EDGE ( 'NONE', *, *, #948, .F. ) ;
#22004 = CARTESIAN_POINT ( 'NONE',  ( 9.999999999999998224, 0.000000000000000000, -95.37500000409677625 ) ) ;
#22005 = LINE ( 'NONE', #32583, #13930 ) ;
#22006 = CARTESIAN_POINT ( 'NONE',  ( 7.644554776091147741E-16, 12.48450537969573659, -154.1562500020484094 ) ) ;
#22007 = CARTESIAN_POINT ( 'NONE',  ( -5.405949406249996869, 9.363379034771805109, -53.34375000204835970 ) ) ;
#22009 = ADVANCED_FACE ( 'NONE', ( #27338 ), #4456, .T. ) ;
#22008 = VERTEX_POINT ( 'NONE', #11129 ) ;
#22010 = CARTESIAN_POINT ( 'NONE',  ( -4.999999999999996447, 8.660254037844387298, -14.99999999999995737 ) ) ;
#22011 = VECTOR ( 'NONE', #37919, 1000.000000000000000 ) ;
#22012 = CARTESIAN_POINT ( 'NONE',  ( -10.81189881249999729, 6.242252689847871849, -27.90625000204838102 ) ) ;
#22013 = CARTESIAN_POINT ( 'NONE',  ( 4.999999999999992006, -8.660254037844389075, -152.2500000000000000 ) ) ;
#22014 = EDGE_CURVE ( 'NONE', #9407, #4172, #1121, .T. ) ;
#22015 = CARTESIAN_POINT ( 'NONE',  ( 4.999999999999992006, -8.660254037844389075, -19.12500000409675494 ) ) ;
#22016 = VECTOR ( 'NONE', #26598, 1000.000000000000000 ) ;
#22017 = CARTESIAN_POINT ( 'NONE',  ( -9.999999999999998224, 1.224646799147353059E-15, -199.2500000000000000 ) ) ;
#22019 = ORIENTED_EDGE ( 'NONE', *, *, #25715, .F. ) ;
#22018 = CARTESIAN_POINT ( 'NONE',  ( -10.81189881249999907, -6.242252689847864744, -129.6562500020483810 ) ) ;
#22020 = PLANE ( 'NONE',  #15167 ) ;
#22021 = EDGE_CURVE ( 'NONE', #7904, #30038, #30320, .T. ) ;
#22022 = CARTESIAN_POINT ( 'NONE',  ( 5.000000000000000000, 8.660254037844385522, -143.1250000040967905 ) ) ;
#22023 = EDGE_CURVE ( 'NONE', #30574, #39730, #12145, .T. ) ;
#22024 = ORIENTED_EDGE ( 'NONE', *, *, #21208, .F. ) ;
#22025 = CARTESIAN_POINT ( 'NONE',  ( -5.405949406250003975, -9.363379034771801557, -54.53125000204836681 ) ) ;
#22026 = PERSON_AND_ORGANIZATION_ROLE ( 'creator' ) ;
#22027 = CARTESIAN_POINT ( 'NONE',  ( 10.81189881249999551, -6.242252689847874514, -112.4687500020483810 ) ) ;
#22029 = ORIENTED_EDGE ( 'NONE', *, *, #8605, .T. ) ;
#22028 = ORIENTED_EDGE ( 'NONE', *, *, #8296, .T. ) ;
#22030 = CARTESIAN_POINT ( 'NONE',  ( 9.999999999999998224, 1.224646799147353059E-15, -99.99999999999998579 ) ) ;
#22031 = CARTESIAN_POINT ( 'NONE',  ( 11.54700538379250396, 20.00000000000000711, 45.00000000000009237 ) ) ;
#22032 = CARTESIAN_POINT ( 'NONE',  ( 7.644554776091147741E-16, 12.48450537969573659, -161.4687500020484094 ) ) ;
#22033 = CARTESIAN_POINT ( 'NONE',  ( 10.81189881249999907, 6.242252689847868297, -191.9062500020484094 ) ) ;
#22034 = CARTESIAN_POINT ( 'NONE',  ( -10.81189881249999907, -6.242252689847864744, -7.968750002048352599 ) ) ;
#22035 = CARTESIAN_POINT ( 'NONE',  ( -5.000000000000003553, -8.660254037844383745, -133.0000000000000000 ) ) ;
#22036 = AXIS2_PLACEMENT_3D ( 'NONE', #10742, #33857, #843 ) ;
#22037 = CARTESIAN_POINT ( 'NONE',  ( 5.405949406249999534, 9.363379034771803333, -140.5937500020483810 ) ) ;
#22038 = CARTESIAN_POINT ( 'NONE',  ( -2.293366432827344421E-15, -12.48450537969573659, -106.7187500020483668 ) ) ;
#22039 = CARTESIAN_POINT ( 'NONE',  ( 0.000000000000000000, 0.000000000000000000, -240.0000000000000000 ) ) ;
#22040 = CARTESIAN_POINT ( 'NONE',  ( -10.81189881249999907, -6.242252689847864744, -119.1562500020484237 ) ) ;
#22041 = CARTESIAN_POINT ( 'NONE',  ( -10.00000000000000000, -5.773502691896251982, -196.5000000040967905 ) ) ;
#22042 = CARTESIAN_POINT ( 'NONE',  ( -10.81189881249999729, -6.242252689847864744, -124.9687500020483810 ) ) ;
#22043 = CARTESIAN_POINT ( 'NONE',  ( 10.81189881249999729, 0.000000000000000000, -193.5312500020484094 ) ) ;
#22044 = CARTESIAN_POINT ( 'NONE',  ( -4.999999999999996447, 8.660254037844387298, -165.3750000040967905 ) ) ;
#22045 = CARTESIAN_POINT ( 'NONE',  ( -9.999999999999998224, 1.224646799147353059E-15, -143.7500000000000000 ) ) ;
#22046 = CARTESIAN_POINT ( 'NONE',  ( 4.999999999999992006, -8.660254037844389075, -15.74999999999995914 ) ) ;
#22047 = CARTESIAN_POINT ( 'NONE',  ( -10.81189881249999729, 1.324075727343319199E-15, -69.59375000204836681 ) ) ;
#22048 = CARTESIAN_POINT ( 'NONE',  ( -5.405949406249996869, 9.363379034771805109, -54.84375000204835970 ) ) ;
#22049 = CARTESIAN_POINT ( 'NONE',  ( 10.00000000000000000, 5.773502691896255534, -188.2500000040968189 ) ) ;
#22050 = CARTESIAN_POINT ( 'NONE',  ( 10.81189881249999729, 0.000000000000000000, -30.03125000204837036 ) ) ;
#22051 = CARTESIAN_POINT ( 'NONE',  ( -5.405949406250003975, -9.363379034771801557, -39.34375000204837391 ) ) ;
#22052 = CARTESIAN_POINT ( 'NONE',  ( -4.999999999999996447, 8.660254037844387298, -52.87500000409675494 ) ) ;
#22053 = CARTESIAN_POINT ( 'NONE',  ( -10.81189881249999729, 6.242252689847871849, -146.2187500020483810 ) ) ;
#22054 = CARTESIAN_POINT ( 'NONE',  ( -4.999999999999996447, 8.660254037844387298, -115.4999999999999858 ) ) ;
#22055 = DIRECTION ( 'NONE',  ( -0.000000000000000000, -0.000000000000000000, 1.000000000000000000 ) ) ;
#22056 = CARTESIAN_POINT ( 'NONE',  ( -9.999999999999998224, 1.224646799147353059E-15, -76.24999999999998579 ) ) ;
#22057 = CARTESIAN_POINT ( 'NONE',  ( -10.81189881249999729, 6.242252689847871849, -137.4062500020484094 ) ) ;
#22058 = CARTESIAN_POINT ( 'NONE',  ( 7.644554776091147741E-16, 12.48450537969573659, -10.15625000204837924 ) ) ;
#22059 = EDGE_CURVE ( 'NONE', #41040, #25114, #39853, .T. ) ;
#22060 = VERTEX_POINT ( 'NONE', #13304 ) ;
#22061 = CARTESIAN_POINT ( 'NONE',  ( 0.000000000000000000, 0.000000000000000000, -200.0000000000000000 ) ) ;
#22062 = CARTESIAN_POINT ( 'NONE',  ( 4.999999999999992006, -8.660254037844389075, -116.6250000040967905 ) ) ;
#22063 = CARTESIAN_POINT ( 'NONE',  ( -9.999999999999479527, -5.773502691896549521, -39.00000000409675494 ) ) ;
#22064 = CARTESIAN_POINT ( 'NONE',  ( -2.293366432827344421E-15, -12.48450537969573659, -75.21875000204839523 ) ) ;
#22065 = CARTESIAN_POINT ( 'NONE',  ( -2.121150477449813534E-15, -11.54700538379251284, -38.37499999999995737 ) ) ;
#22066 = CARTESIAN_POINT ( 'NONE',  ( -4.999999999999996447, 8.660254037844387298, -22.87500000409675849 ) ) ;
#22067 = FACE_OUTER_BOUND ( 'NONE', #23070, .T. ) ;
#22068 = CARTESIAN_POINT ( 'NONE',  ( -10.81189881249999729, 6.242252689847871849, -36.90625000204835970 ) ) ;
#22069 = DIRECTION ( 'NONE',  ( -1.000000000000000000, 0.000000000000000000, 0.000000000000000000 ) ) ;
#22070 = CARTESIAN_POINT ( 'NONE',  ( -2.293366432827344421E-15, -12.48450537969573659, -144.4062500020484094 ) ) ;
#22071 = VECTOR ( 'NONE', #3861, 1000.000000000000000 ) ;
#22072 = CARTESIAN_POINT ( 'NONE',  ( -5.405949406250003975, -9.363379034771801557, -150.5312500020483810 ) ) ;
#22073 = CARTESIAN_POINT ( 'NONE',  ( -9.999999999999998224, 1.224646799147353059E-15, -65.74999999999997158 ) ) ;
#22074 = CYLINDRICAL_SURFACE ( 'NONE', #7293, 9.999999999999998224 ) ;
#22075 = ORIENTED_EDGE ( 'NONE', *, *, #22890, .T. ) ;
#22076 = ORIENTED_EDGE ( 'NONE', *, *, #32093, .T. ) ;
#22077 = EDGE_LOOP ( 'NONE', ( #27259, #430, #6772, #38977 ) ) ;
#22078 =( BOUNDED_CURVE ( )  B_SPLINE_CURVE ( 2, ( #34051, #7289, #31248, #27354, #7498, #37706, #10935 ),
 .UNSPECIFIED., .F., .F. ) 
 B_SPLINE_CURVE_WITH_KNOTS ( ( 3, 2, 2, 3 ),
 ( 0.6791044776119405935, 0.6803482587064679787, 0.6815920398009952530, 0.6828358208955226383 ),
 .UNSPECIFIED. ) 
 CURVE ( )  GEOMETRIC_REPRESENTATION_ITEM ( )  RATIONAL_B_SPLINE_CURVE ( ( 0.9999999999999641398, 0.8660254037844745678, 1.000000000000000000, 0.8660254037844387076, 1.000000000000000000, 0.8660254037844148378, 1.000000000000023981 ) ) 
 REPRESENTATION_ITEM ( '' )  );
#22079 = FACE_OUTER_BOUND ( 'NONE', #24140, .T. ) ;
#22080 = CARTESIAN_POINT ( 'NONE',  ( -10.81189881249999729, 1.324075727343319199E-15, -183.5937500020483810 ) ) ;
#22081 = CARTESIAN_POINT ( 'NONE',  ( 10.81189881249999551, -6.242252689847874514, -31.46875000204835260 ) ) ;
#22082 = CARTESIAN_POINT ( 'NONE',  ( -10.00000000000076916, 5.773502691895813221, -109.7500000040967620 ) ) ;
#22083 = CARTESIAN_POINT ( 'NONE',  ( 5.405949406249992428, -9.363379034771808662, -163.5937500020484094 ) ) ;
#22084 = CARTESIAN_POINT ( 'NONE',  ( 10.81189881249999729, 0.000000000000000000, -155.8437500020483810 ) ) ;
#22085 = CYLINDRICAL_SURFACE ( 'NONE', #27264, 9.999999999999998224 ) ;
#22086 = CARTESIAN_POINT ( 'NONE',  ( -10.81189881249999729, 6.242252689847871849, -137.2187500020483810 ) ) ;
#22087 = CARTESIAN_POINT ( 'NONE',  ( -2.293366432827344421E-15, -12.48450537969573659, -141.4062500020483810 ) ) ;
#22088 = CARTESIAN_POINT ( 'NONE',  ( 0.000000000000000000, 0.000000000000000000, -99.99999999999998579 ) ) ;
#22089 = CARTESIAN_POINT ( 'NONE',  ( 10.81189881249999551, -6.242252689847874514, -149.9687500020483810 ) ) ;
#22090 = CARTESIAN_POINT ( 'NONE',  ( -9.999999999999998224, 1.224646799147353059E-15, -152.7500000000000000 ) ) ;
#22091 = CARTESIAN_POINT ( 'NONE',  ( 9.999999999999998224, 0.000000000000000000, -33.87500000409676915 ) ) ;
#22092 = CARTESIAN_POINT ( 'NONE',  ( -9.999999999999998224, 1.224646799147353059E-15, -173.7500000000000284 ) ) ;
#22093 = VECTOR ( 'NONE', #27377, 1000.000000000000000 ) ;
#22094 = EDGE_CURVE ( 'NONE', #6996, #8228, #40270, .T. ) ;
#22095 = CARTESIAN_POINT ( 'NONE',  ( -5.405949406249996869, 9.363379034771805109, -77.34375000204838102 ) ) ;
#22096 = DIRECTION ( 'NONE',  ( -0.000000000000000000, -0.000000000000000000, 1.000000000000000000 ) ) ;
#22097 = CARTESIAN_POINT ( 'NONE',  ( -5.405949406249996869, 9.363379034771805109, -50.53125000204835970 ) ) ;
#22098 = CARTESIAN_POINT ( 'NONE',  ( -9.187887513909968717, -4.550206982411138412, -99.99999999999997158 ) ) ;
#22099 = CARTESIAN_POINT ( 'NONE',  ( -5.405949406250003975, -9.363379034771801557, -171.3437500020484094 ) ) ;
#22100 = CARTESIAN_POINT ( 'NONE',  ( 7.070501591499377789E-16, 11.54700538379251284, -138.1250000000000000 ) ) ;
#22101 = CARTESIAN_POINT ( 'NONE',  ( 10.81189881249999729, 6.242252689847867408, -145.4062500020484094 ) ) ;
#22102 = DIRECTION ( 'NONE',  ( 1.000000000000000000, 0.000000000000000000, 0.000000000000000000 ) ) ;
#22103 = CARTESIAN_POINT ( 'NONE',  ( -2.293366432827344421E-15, -12.48450537969573659, -36.40625000204835970 ) ) ;
#22104 = CARTESIAN_POINT ( 'NONE',  ( -9.999999999999998224, 1.224646799147353059E-15, -121.6250000040967905 ) ) ;
#22105 = CARTESIAN_POINT ( 'NONE',  ( 5.000000000000000000, 8.660254037844385522, -97.74999999999998579 ) ) ;
#22106 = EDGE_LOOP ( 'NONE', ( #27485, #38101, #37616, #32384 ) ) ;
#22107 = CARTESIAN_POINT ( 'NONE',  ( -2.293366432827344421E-15, -12.48450537969573659, -121.9062500020483952 ) ) ;
#22108 = CARTESIAN_POINT ( 'NONE',  ( -2.121150477449813534E-15, -11.54700538379251284, -140.7500000040967905 ) ) ;
#22109 = CARTESIAN_POINT ( 'NONE',  ( 9.999999999999998224, 0.000000000000000000, -140.3750000040967905 ) ) ;
#22110 = CARTESIAN_POINT ( 'NONE',  ( -5.405949406249996869, 9.363379034771805109, -175.0312500020484094 ) ) ;
#22111 = CARTESIAN_POINT ( 'NONE',  ( 7.070501591499377789E-16, 11.54700538379251284, -51.50000000409676204 ) ) ;
#22112 = CARTESIAN_POINT ( 'NONE',  ( 5.000000000000000000, 8.660254037844385522, -48.62500000409678336 ) ) ;
#22113 = CARTESIAN_POINT ( 'NONE',  ( 5.405949406249999534, 9.363379034771803333, -70.28125000204838102 ) ) ;
#22114 = EDGE_CURVE ( 'NONE', #4599, #4329, #3625, .T. ) ;
#22115 = DIRECTION ( 'NONE',  ( 1.000000000000000000, 0.000000000000000000, 0.000000000000000000 ) ) ;
#22116 = CARTESIAN_POINT ( 'NONE',  ( -10.81189881249999729, 6.242252689847871849, -165.9062500020483810 ) ) ;
#22117 = CARTESIAN_POINT ( 'NONE',  ( 0.000000000000000000, 0.000000000000000000, -200.0000000000000000 ) ) ;
#22118 = DIRECTION ( 'NONE',  ( -0.000000000000000000, -0.000000000000000000, 1.000000000000000000 ) ) ;
#22119 = VERTEX_POINT ( 'NONE', #26493 ) ;
#22120 = CYLINDRICAL_SURFACE ( 'NONE', #13215, 9.999999999999998224 ) ;
#22121 = DIRECTION ( 'NONE',  ( -0.000000000000000000, -0.000000000000000000, 1.000000000000000000 ) ) ;
#22122 =( BOUNDED_CURVE ( )  B_SPLINE_CURVE ( 2, ( #31636, #5726, #41091, #18447, #34447, #31418, #18011 ),
 .UNSPECIFIED., .F., .F. ) 
 B_SPLINE_CURVE_WITH_KNOTS ( ( 3, 2, 2, 3 ),
 ( 0.9888059701492539766, 0.9900497512437813619, 0.9912935323383086361, 0.9925373134328360214 ),
 .UNSPECIFIED. ) 
 CURVE ( )  GEOMETRIC_REPRESENTATION_ITEM ( )  RATIONAL_B_SPLINE_CURVE ( ( 0.9999999999999761302, 0.8660254037844625774, 1.000000000000000000, 0.8660254037844387076, 1.000000000000000000, 0.8660254037844148378, 1.000000000000023981 ) ) 
 REPRESENTATION_ITEM ( '' )  );
#22123 = CARTESIAN_POINT ( 'NONE',  ( -9.999999999999998224, 1.224646799147353059E-15, -71.74999999999998579 ) ) ;
#22125 = VERTEX_POINT ( 'NONE', #27127 ) ;
#22124 = CARTESIAN_POINT ( 'NONE',  ( -10.81189881249999907, -6.242252689847864744, -81.65625000204839523 ) ) ;
#22127 = ORIENTED_EDGE ( 'NONE', *, *, #29145, .F. ) ;
#22126 = CARTESIAN_POINT ( 'NONE',  ( -9.999999999999742428, -5.773502691896402084, -100.5000000040967905 ) ) ;
#22128 = EDGE_LOOP ( 'NONE', ( #12076, #38318, #23767, #483 ) ) ;
#22129 = CARTESIAN_POINT ( 'NONE',  ( -5.405949406250003975, -9.363379034771801557, -33.34375000204836681 ) ) ;
#22130 = CARTESIAN_POINT ( 'NONE',  ( 4.999999999999992006, -8.660254037844389075, -53.24999999999996447 ) ) ;
#22131 = CARTESIAN_POINT ( 'NONE',  ( -10.81189881249999729, 6.242252689847871849, -2.406250002048375247 ) ) ;
#22132 =( BOUNDED_CURVE ( )  B_SPLINE_CURVE ( 2, ( #34881, #18239, #35305, #31429, #41324, #41546, #24748 ),
 .UNSPECIFIED., .F., .F. ) 
 B_SPLINE_CURVE_WITH_KNOTS ( ( 3, 2, 2, 3 ),
 ( 0.06343283582089558059, 0.06467661691542293811, 0.06592039800995032339, 0.06716417910447768091 ),
 .UNSPECIFIED. ) 
 CURVE ( )  GEOMETRIC_REPRESENTATION_ITEM ( )  RATIONAL_B_SPLINE_CURVE ( ( 0.9999999999999940048, 0.8660254037844447028, 1.000000000000000000, 0.8660254037844387076, 1.000000000000000000, 0.8660254037844312691, 1.000000000000007550 ) ) 
 REPRESENTATION_ITEM ( '' )  );
#22134 = ORIENTED_EDGE ( 'NONE', *, *, #32284, .T. ) ;
#22133 = CARTESIAN_POINT ( 'NONE',  ( 5.405949406249999534, 9.363379034771803333, -53.59375000204835970 ) ) ;
#22135 = CARTESIAN_POINT ( 'NONE',  ( -9.999999999999479527, -5.773502691896549521, -112.5000000040967478 ) ) ;
#22136 = CARTESIAN_POINT ( 'NONE',  ( 5.000000000000000000, 8.660254037844385522, -33.24999999999997158 ) ) ;
#22137 = CARTESIAN_POINT ( 'NONE',  ( 5.405949406249992428, -9.363379034771808662, -189.0937500020483810 ) ) ;
#22138 = CARTESIAN_POINT ( 'NONE',  ( 10.81189881249999551, -6.242252689847874514, -176.9687500020483810 ) ) ;
#22139 = CARTESIAN_POINT ( 'NONE',  ( 5.405949406249999534, 9.363379034771803333, -157.0937500020483810 ) ) ;
#22141 = EDGE_CURVE ( 'NONE', #36280, #15509, #37495, .T. ) ;
#22140 = CARTESIAN_POINT ( 'NONE',  ( 7.644554776091147741E-16, 12.48450537969573659, -173.4687500020483810 ) ) ;
#22142 = DIRECTION ( 'NONE',  ( -0.000000000000000000, -0.000000000000000000, 1.000000000000000000 ) ) ;
#22143 = CARTESIAN_POINT ( 'NONE',  ( 7.070501591499376803E-16, 11.54700538379251284, -132.1250000000000000 ) ) ;
#22144 = CARTESIAN_POINT ( 'NONE',  ( -2.121150477449813534E-15, -11.54700538379251284, -194.3750000000000284 ) ) ;
#22145 = CARTESIAN_POINT ( 'NONE',  ( -2.293366432827344421E-15, -12.48450537969573659, -106.7187500020483668 ) ) ;
#22146 = CARTESIAN_POINT ( 'NONE',  ( -9.999999999999998224, 1.224646799147353059E-15, -17.74999999999996092 ) ) ;
#22147 = CARTESIAN_POINT ( 'NONE',  ( 10.81189881249999907, 6.242252689847868297, -77.90625000204836681 ) ) ;
#22148 = CARTESIAN_POINT ( 'NONE',  ( -5.405949406250003975, -9.363379034771801557, -93.34375000204838102 ) ) ;
#22149 = CARTESIAN_POINT ( 'NONE',  ( 10.81189881249999551, -6.242252689847874514, -58.65625000204838813 ) ) ;
#22150 = CARTESIAN_POINT ( 'NONE',  ( -5.000000000000003553, -8.660254037844383745, -146.8750000040967905 ) ) ;
#22151 = CARTESIAN_POINT ( 'NONE',  ( 9.999999999999996447, -5.773502691896262640, -120.6250000000000000 ) ) ;
#22152 = VECTOR ( 'NONE', #18342, 1000.000000000000000 ) ;
#22153 = VERTEX_POINT ( 'NONE', #7486 ) ;
#22154 = CARTESIAN_POINT ( 'NONE',  ( 10.81189881249999729, 6.242252689847867408, -139.4062500020484094 ) ) ;
#22155 = CARTESIAN_POINT ( 'NONE',  ( -10.81189881249999729, 1.324075727343319199E-15, -158.2812500020484094 ) ) ;
#22156 = LOCAL_TIME ( 11, 57, 6.000000000000000000, #30421 ) ;
#22157 = CARTESIAN_POINT ( 'NONE',  ( -9.999999999999998224, 1.224646799147353059E-15, -118.2500000000000000 ) ) ;
#22158 = CARTESIAN_POINT ( 'NONE',  ( -10.81189881249999907, -6.242252689847864744, -91.96875000204838102 ) ) ;
#22159 = ORIENTED_EDGE ( 'NONE', *, *, #20529, .F. ) ;
#22160 = CARTESIAN_POINT ( 'NONE',  ( 5.000000000000000000, 8.660254037844385522, -61.74999999999997158 ) ) ;
#22161 = CARTESIAN_POINT ( 'NONE',  ( 10.81189881249999551, -6.242252689847874514, -0.1562500020483581498 ) ) ;
#22162 = CARTESIAN_POINT ( 'NONE',  ( -9.999999999999998224, 1.224646799147353059E-15, -72.12500000409677625 ) ) ;
#22163 = CARTESIAN_POINT ( 'NONE',  ( -5.000000000000003553, -8.660254037844383745, -169.3750000040967905 ) ) ;
#22164 = CARTESIAN_POINT ( 'NONE',  ( -9.999999999999998224, 1.224646799147353059E-15, -200.0000000000000000 ) ) ;
#22165 = CARTESIAN_POINT ( 'NONE',  ( 7.644554776091147741E-16, 12.48450537969573659, -89.65625000204839523 ) ) ;
#22166 = CARTESIAN_POINT ( 'NONE',  ( -5.405949406250003975, -9.363379034771801557, -68.03125000204838102 ) ) ;
#22167 = CARTESIAN_POINT ( 'NONE',  ( -4.999999999999996447, 8.660254037844387298, -70.87500000409677625 ) ) ;
#22168 = CARTESIAN_POINT ( 'NONE',  ( -9.999999999999998224, 0.000000000000000000, -99.99999999999998579 ) ) ;
#22169 = CARTESIAN_POINT ( 'NONE',  ( -5.405949406250003975, -9.363379034771801557, -22.84375000204835615 ) ) ;
#22170 = ORIENTED_EDGE ( 'NONE', *, *, #20888, .T. ) ;
#22171 = CARTESIAN_POINT ( 'NONE',  ( 5.405949406249992428, -9.363379034771808662, -196.7812500020484094 ) ) ;
#22172 = VECTOR ( 'NONE', #34994, 1000.000000000000000 ) ;
#22173 = CARTESIAN_POINT ( 'NONE',  ( -5.405949406249996869, 9.363379034771805109, -22.03125000204836326 ) ) ;
#22174 = EDGE_CURVE ( 'NONE', #317, #14499, #20637, .T. ) ;
#22175 = CARTESIAN_POINT ( 'NONE',  ( 10.81189881249999729, 6.242252689847867408, -8.718750002048357928 ) ) ;
#22176 = DIRECTION ( 'NONE',  ( -0.000000000000000000, -0.000000000000000000, 1.000000000000000000 ) ) ;
#22177 = CARTESIAN_POINT ( 'NONE',  ( -9.999999999998969713, -5.773502691896847949, -63.00000000409676915 ) ) ;
#22178 = LINE ( 'NONE', #42429, #10044 ) ;
#22179 = CARTESIAN_POINT ( 'NONE',  ( -10.00000000000000000, -5.773502691896251982, -178.1250000000000284 ) ) ;
#22180 = CARTESIAN_POINT ( 'NONE',  ( 0.000000000000000000, 0.000000000000000000, -200.0000000000000000 ) ) ;
#22182 = VERTEX_POINT ( 'NONE', #10923 ) ;
#22181 = CARTESIAN_POINT ( 'NONE',  ( -5.405949406250003975, -9.363379034771801557, -102.5312500020483952 ) ) ;
#22183 = EDGE_LOOP ( 'NONE', ( #16443, #19669, #8866, #1322 ) ) ;
#22184 = VERTEX_POINT ( 'NONE', #17392 ) ;
#22185 = CARTESIAN_POINT ( 'NONE',  ( -2.293366432827344421E-15, -12.48450537969573659, -27.40625000204838102 ) ) ;
#22186 = DATE_AND_TIME ( #32338, #14580 ) ;
#22187 = CC_DESIGN_SECURITY_CLASSIFICATION ( #37345, ( #42693 ) ) ;
#22188 = CARTESIAN_POINT ( 'NONE',  ( -10.81189881249999907, -6.242252689847864744, -79.96875000204836681 ) ) ;
#22189 = DIRECTION ( 'NONE',  ( -0.000000000000000000, -0.000000000000000000, -1.000000000000000000 ) ) ;
#22190 = CARTESIAN_POINT ( 'NONE',  ( 9.876501204336495476, -2.277692215602485692, -100.0000000000000142 ) ) ;
#22191 = CARTESIAN_POINT ( 'NONE',  ( 9.999999999999998224, 0.000000000000000000, -200.0000000000000000 ) ) ;
#22192 = FACE_OUTER_BOUND ( 'NONE', #846, .T. ) ;
#22193 = CARTESIAN_POINT ( 'NONE',  ( 5.405949406249999534, 9.363379034771803333, -155.7812500020484094 ) ) ;
#22194 = CARTESIAN_POINT ( 'NONE',  ( 9.999999999999996447, -5.773502691896262640, -8.500000004096751383 ) ) ;
#22195 = CARTESIAN_POINT ( 'NONE',  ( 10.81189881249999729, 0.000000000000000000, -131.8437500020484094 ) ) ;
#22196 = CARTESIAN_POINT ( 'NONE',  ( -10.81189881249999729, 6.242252689847871849, -119.2187500020483810 ) ) ;
#22197 =( BOUNDED_CURVE ( )  B_SPLINE_CURVE ( 2, ( #20234, #40493, #13736, #26926, #13949, #26717, #10727 ),
 .UNSPECIFIED., .F., .F. ) 
 B_SPLINE_CURVE_WITH_KNOTS ( ( 3, 2, 2, 3 ),
 ( 0.1492537313432835966, 0.1504975124378109819, 0.1517412935323383116, 0.1529850746268656692 ),
 .UNSPECIFIED. ) 
 CURVE ( )  GEOMETRIC_REPRESENTATION_ITEM ( )  RATIONAL_B_SPLINE_CURVE ( ( 0.9999999999999970024, 0.8660254037844417052, 1.000000000000000000, 0.8660254037844387076, 1.000000000000000000, 0.8660254037844387076, 1.000000000000000000 ) ) 
 REPRESENTATION_ITEM ( '' )  );
#22198 = CARTESIAN_POINT ( 'NONE',  ( -2.293366432827344421E-15, -12.48450537969573659, -82.71875000204838102 ) ) ;
#22199 = CARTESIAN_POINT ( 'NONE',  ( -10.81189881249999729, 1.324075727343319199E-15, -89.28125000204838102 ) ) ;
#22200 = CARTESIAN_POINT ( 'NONE',  ( 9.999999999999996447, -5.773502691896262640, -170.5000000040967905 ) ) ;
#22201 = CARTESIAN_POINT ( 'NONE',  ( 7.644554776091147741E-16, 12.48450537969573659, -167.6562500020484094 ) ) ;
#22202 = CARTESIAN_POINT ( 'NONE',  ( 9.999999999999998224, 0.000000000000000000, -155.0000000000000000 ) ) ;
#22203 = CARTESIAN_POINT ( 'NONE',  ( -10.81189881249999729, 6.242252689847871849, -176.4062500020484094 ) ) ;
#22204 = CARTESIAN_POINT ( 'NONE',  ( -10.81189881249999907, -6.242252689847864744, -191.1562500020484094 ) ) ;
#22205 = CARTESIAN_POINT ( 'NONE',  ( 10.81189881249999729, 6.242252689847867408, -43.21875000204835970 ) ) ;
#22206 = CARTESIAN_POINT ( 'NONE',  ( -4.999999999999996447, 8.660254037844387298, -166.8750000040967905 ) ) ;
#22207 = CARTESIAN_POINT ( 'NONE',  ( 5.405949406249999534, 9.363379034771803333, -5.781250002048377468 ) ) ;
#22208 = CARTESIAN_POINT ( 'NONE',  ( -10.81189881249999907, -6.242252689847864744, -10.96875000204835970 ) ) ;
#22209 = CARTESIAN_POINT ( 'NONE',  ( 7.070501591499376803E-16, 11.54700538379251284, -162.5000000040967905 ) ) ;
#22210 = CARTESIAN_POINT ( 'NONE',  ( 10.81189881249999551, -6.242252689847874514, -122.9687500020483810 ) ) ;
#22211 = CARTESIAN_POINT ( 'NONE',  ( 9.999999999999998224, 0.000000000000000000, -93.49999999999998579 ) ) ;
#22212 = CARTESIAN_POINT ( 'NONE',  ( 5.405949406249999534, 9.363379034771803333, -22.28125000204836326 ) ) ;
#22213 = CARTESIAN_POINT ( 'NONE',  ( 7.070501591499377789E-16, 11.54700538379251284, -101.0000000040967905 ) ) ;
#22214 = LINE ( 'NONE', #12269, #19667 ) ;
#22215 = CARTESIAN_POINT ( 'NONE',  ( -5.405949406249996869, 9.363379034771805109, -118.0312500020483952 ) ) ;
#22216 = CARTESIAN_POINT ( 'NONE',  ( 5.405949406249992428, -9.363379034771808662, -91.78125000204838102 ) ) ;
#22217 = VERTEX_POINT ( 'NONE', #30589 ) ;
#22218 = VECTOR ( 'NONE', #24752, 1000.000000000000000 ) ;
#22219 = CARTESIAN_POINT ( 'NONE',  ( 7.070501591499377789E-16, 11.54700538379251284, -93.50000000409677625 ) ) ;
#22220 = CARTESIAN_POINT ( 'NONE',  ( 0.000000000000000000, 0.000000000000000000, -240.0000000000000000 ) ) ;
#22221 = CARTESIAN_POINT ( 'NONE',  ( -10.81189881249999729, 6.242252689847871849, -158.4062500020483810 ) ) ;
#22222 = CARTESIAN_POINT ( 'NONE',  ( -5.405949406249996869, 9.363379034771805109, -48.84375000204838102 ) ) ;
#22223 = ORIENTED_EDGE ( 'NONE', *, *, #24858, .T. ) ;
#22224 = CARTESIAN_POINT ( 'NONE',  ( -10.00000000000000000, -5.773502691896251982, -20.62499999999997158 ) ) ;
#22225 = ADVANCED_FACE ( 'NONE', ( #36622 ), #40067, .T. ) ;
#22226 = CARTESIAN_POINT ( 'NONE',  ( 7.644554776091147741E-16, 12.48450537969573659, -28.15625000204838813 ) ) ;
#22227 = CARTESIAN_POINT ( 'NONE',  ( -2.121150477449813534E-15, -11.54700538379251284, -156.8750000000000000 ) ) ;
#22228 = CARTESIAN_POINT ( 'NONE',  ( -5.000000000000003553, -8.660254037844383745, -22.37500000409675494 ) ) ;
#22229 = EDGE_CURVE ( 'NONE', #26657, #39297, #9384, .T. ) ;
#22230 = AXIS2_PLACEMENT_3D ( 'NONE', #14751, #5066, #18214 ) ;
#22231 = CARTESIAN_POINT ( 'NONE',  ( 9.999999999999998224, 0.000000000000000000, -198.5000000000000000 ) ) ;
#22233 = ORIENTED_EDGE ( 'NONE', *, *, #41110, .F. ) ;
#22232 = CARTESIAN_POINT ( 'NONE',  ( -5.405949406250003975, -9.363379034771801557, -126.5312500020483952 ) ) ;
#22234 = CARTESIAN_POINT ( 'NONE',  ( -10.00000000000025580, 5.773502691896109873, -117.2500000040968047 ) ) ;
#22235 = ORIENTED_EDGE ( 'NONE', *, *, #29704, .F. ) ;
#22236 = CARTESIAN_POINT ( 'NONE',  ( 5.405949406249992428, -9.363379034771808662, -51.28125000204835970 ) ) ;
#22237 = COORDINATED_UNIVERSAL_TIME_OFFSET ( 6, 0, .AHEAD. ) ;
#22238 = CARTESIAN_POINT ( 'NONE',  ( 10.81189881249999729, 0.000000000000000000, -106.3437500020483810 ) ) ;
#22240 = ORIENTED_EDGE ( 'NONE', *, *, #30325, .F. ) ;
#22239 = EDGE_LOOP ( 'NONE', ( #35516, #8942, #7318, #21886 ) ) ;
#22241 = FACE_OUTER_BOUND ( 'NONE', #14622, .T. ) ;
#22242 = CARTESIAN_POINT ( 'NONE',  ( -9.999999999999996447, 5.773502691896259975, -170.8750000000000000 ) ) ;
#22243 =( BOUNDED_CURVE ( )  B_SPLINE_CURVE ( 2, ( #29964, #7496, #404, #16552, #13731, #20013, #26920 ),
 .UNSPECIFIED., .F., .F. ) 
 B_SPLINE_CURVE_WITH_KNOTS ( ( 3, 2, 2, 3 ),
 ( 0.4514925373134329734, 0.4527363184079603031, 0.4539800995024877439, 0.4552238805970150737 ),
 .UNSPECIFIED. ) 
 CURVE ( )  GEOMETRIC_REPRESENTATION_ITEM ( )  RATIONAL_B_SPLINE_CURVE ( ( 0.9999999999999880096, 0.8660254037844506980, 1.000000000000000000, 0.8660254037844387076, 1.000000000000000000, 0.8660254037844207220, 1.000000000000017986 ) ) 
 REPRESENTATION_ITEM ( '' )  );
#22244 = CARTESIAN_POINT ( 'NONE',  ( -5.405949406249996869, 9.363379034771805109, -156.8437500020483810 ) ) ;
#22245 = CARTESIAN_POINT ( 'NONE',  ( -10.81189881249999729, 1.324075727343319199E-15, -177.7812500020484094 ) ) ;
#22246 = CARTESIAN_POINT ( 'NONE',  ( 10.81189881249999551, -6.242252689847874514, -10.46875000204836503 ) ) ;
#22247 = CARTESIAN_POINT ( 'NONE',  ( -4.999999999999996447, 8.660254037844387298, -139.5000000000000000 ) ) ;
#22248 = ADVANCED_FACE ( 'NONE', ( #393 ), #7705, .F. ) ;
#22249 = CARTESIAN_POINT ( 'NONE',  ( 5.405949406249992428, -9.363379034771808662, -144.0937500020483810 ) ) ;
#22250 = CARTESIAN_POINT ( 'NONE',  ( 7.644554776091147741E-16, 12.48450537969573659, -108.9687500020483952 ) ) ;
#22251 = CARTESIAN_POINT ( 'NONE',  ( -7.071067811865472841, -7.071067811865472841, -200.0000000000000000 ) ) ;
#22252 = CARTESIAN_POINT ( 'NONE',  ( 5.405949406249992428, -9.363379034771808662, -117.2812500020483952 ) ) ;
#22253 = CARTESIAN_POINT ( 'NONE',  ( -5.000000000000003553, -8.660254037844383745, -197.8750000040967905 ) ) ;
#22254 = CARTESIAN_POINT ( 'NONE',  ( 7.644554776091147741E-16, 12.48450537969573659, -119.4687500020483668 ) ) ;
#22255 = CARTESIAN_POINT ( 'NONE',  ( -10.81189881249999729, 1.324075727343319199E-15, -194.2812500020484094 ) ) ;
#22256 = CARTESIAN_POINT ( 'NONE',  ( 5.000000000000000000, 8.660254037844385522, -157.7500000000000000 ) ) ;
#22257 = CARTESIAN_POINT ( 'NONE',  ( 4.999999999999992006, -8.660254037844389075, -137.2499999999999716 ) ) ;
#22258 = CARTESIAN_POINT ( 'NONE',  ( -9.999999999999998224, 1.224646799147353059E-15, -14.74999999999995737 ) ) ;
#22259 = VECTOR ( 'NONE', #34917, 1000.000000000000114 ) ;
#22260 = CARTESIAN_POINT ( 'NONE',  ( 5.405949406249992428, -9.363379034771808662, -72.09375000204836681 ) ) ;
#22261 = CARTESIAN_POINT ( 'NONE',  ( -5.405949406249996869, 9.363379034771805109, -53.34375000204835970 ) ) ;
#22262 = CARTESIAN_POINT ( 'NONE',  ( 5.000000000000000000, 8.660254037844385522, -189.6250000040967905 ) ) ;
#22263 = CARTESIAN_POINT ( 'NONE',  ( -5.405949406250003975, -9.363379034771801557, -24.53125000204836681 ) ) ;
#22264 = CARTESIAN_POINT ( 'NONE',  ( -10.81189881249999729, 1.324075727343319199E-15, -41.09375000204837391 ) ) ;
#22265 = CARTESIAN_POINT ( 'NONE',  ( 9.999999999999479527, 5.773502691896553074, -149.2500000040967905 ) ) ;
#22266 = CARTESIAN_POINT ( 'NONE',  ( -2.293366432827344421E-15, -12.48450537969573659, -148.7187500020484094 ) ) ;
#22267 = CARTESIAN_POINT ( 'NONE',  ( 4.999999999999992006, -8.660254037844389075, -114.7499999999999858 ) ) ;
#22268 = CARTESIAN_POINT ( 'NONE',  ( 0.000000000000000000, 0.000000000000000000, -240.0000000000000000 ) ) ;
#22269 = CARTESIAN_POINT ( 'NONE',  ( 9.999999999999998224, 0.000000000000000000, -66.49999999999997158 ) ) ;
#22270 = CARTESIAN_POINT ( 'NONE',  ( -5.405949406249996869, 9.363379034771805109, -139.0312500020484094 ) ) ;
#22271 = CARTESIAN_POINT ( 'NONE',  ( -2.293366432827344421E-15, -12.48450537969573659, -7.906250002048370362 ) ) ;
#22272 = VERTEX_POINT ( 'NONE', #29953 ) ;
#22273 = LINE ( 'NONE', #32000, #12079 ) ;
#22274 = CARTESIAN_POINT ( 'NONE',  ( -4.999999999999996447, 8.660254037844387298, -112.8750000040967763 ) ) ;
#22275 = CARTESIAN_POINT ( 'NONE',  ( 9.999999999999998224, 0.000000000000000000, -38.37500000409676915 ) ) ;
#22276 = CARTESIAN_POINT ( 'NONE',  ( 7.644554776091147741E-16, 12.48450537969573659, -71.46875000204835260 ) ) ;
#22277 = CARTESIAN_POINT ( 'NONE',  ( 4.999999999999992006, -8.660254037844389075, -42.74999999999998579 ) ) ;
#22278 = CARTESIAN_POINT ( 'NONE',  ( 9.999999999999998224, 0.000000000000000000, -23.37500000409675849 ) ) ;
#22279 = EDGE_CURVE ( 'NONE', #21961, #36222, #4459, .T. ) ;
#22280 = CARTESIAN_POINT ( 'NONE',  ( 10.81189881249999729, 6.242252689847867408, -52.40625000204838813 ) ) ;
#22281 = CARTESIAN_POINT ( 'NONE',  ( -9.999999999999998224, 1.224646799147353059E-15, -121.2500000000000000 ) ) ;
#22282 = CARTESIAN_POINT ( 'NONE',  ( -5.405949406250003975, -9.363379034771801557, -36.53125000204837391 ) ) ;
#22283 = EDGE_CURVE ( 'NONE', #1789, #22578, #830, .T. ) ;
#22284 = CYLINDRICAL_SURFACE ( 'NONE', #749, 9.999999999999998224 ) ;
#22285 = CARTESIAN_POINT ( 'NONE',  ( 5.405949406249999534, 9.363379034771803333, -148.2812500020483810 ) ) ;
#22286 = ADVANCED_FACE ( 'NONE', ( #21067 ), #37476, .T. ) ;
#22287 = CARTESIAN_POINT ( 'NONE',  ( -10.81189881249999729, 1.324075727343319199E-15, -150.7812500020483810 ) ) ;
#22288 = CARTESIAN_POINT ( 'NONE',  ( -9.999999999999998224, 1.224646799147353059E-15, -165.1250000040967905 ) ) ;
#22289 = DIRECTION ( 'NONE',  ( -0.000000000000000000, -0.000000000000000000, 1.000000000000000000 ) ) ;
#22290 = ORIENTED_EDGE ( 'NONE', *, *, #3804, .T. ) ;
#22291 = ORIENTED_EDGE ( 'NONE', *, *, #7325, .T. ) ;
#22292 = EDGE_LOOP ( 'NONE', ( #29553, #31699, #5302, #38878, #32600, #35955 ) ) ;
#22293 = EDGE_CURVE ( 'NONE', #10615, #3056, #31444, .T. ) ;
#22294 = CARTESIAN_POINT ( 'NONE',  ( -10.00000000000019185, -5.773502691896140071, -177.0000000040967620 ) ) ;
#22295 = CARTESIAN_POINT ( 'NONE',  ( 5.405949406249999534, 9.363379034771803333, -184.0937500020483810 ) ) ;
#22296 = CARTESIAN_POINT ( 'NONE',  ( -10.81189881249999729, 6.242252689847871849, -32.21875000204835970 ) ) ;
#22297 = CARTESIAN_POINT ( 'NONE',  ( -9.999999999998969713, -5.773502691896847949, -41.62499999999995737 ) ) ;
#22298 = CARTESIAN_POINT ( 'NONE',  ( 10.81189881249999729, 0.000000000000000000, -161.8437500020484094 ) ) ;
#22299 = CARTESIAN_POINT ( 'NONE',  ( 10.81189881249999729, 0.000000000000000000, -151.3437500020483810 ) ) ;
#22300 = DIRECTION ( 'NONE',  ( 1.000000000000000000, 0.000000000000000000, 0.000000000000000000 ) ) ;
#22301 = CARTESIAN_POINT ( 'NONE',  ( 10.81189881249999907, 6.242252689847868297, -137.7187500020484094 ) ) ;
#22302 = CARTESIAN_POINT ( 'NONE',  ( 5.405949406249999534, 9.363379034771803333, -139.2812500020483810 ) ) ;
#22303 = CARTESIAN_POINT ( 'NONE',  ( 7.644554776091147741E-16, 12.48450537969573659, -20.46875000204836326 ) ) ;
#22304 = CARTESIAN_POINT ( 'NONE',  ( 10.81189881249999729, 6.242252689847867408, -143.7187500020484094 ) ) ;
#22305 = DIRECTION ( 'NONE',  ( -0.000000000000000000, -0.000000000000000000, -1.000000000000000000 ) ) ;
#22306 = CARTESIAN_POINT ( 'NONE',  ( 5.000000000000000000, 8.660254037844385522, -163.7500000000000000 ) ) ;
#22307 = CARTESIAN_POINT ( 'NONE',  ( -10.81189881249999729, 6.242252689847871849, -83.21875000204838102 ) ) ;
#22308 = CARTESIAN_POINT ( 'NONE',  ( 9.999999999999998224, 0.000000000000000000, -153.8750000040967905 ) ) ;
#22309 = CARTESIAN_POINT ( 'NONE',  ( -10.81189881249999729, 1.324075727343319199E-15, -47.28125000204838813 ) ) ;
#22310 = CARTESIAN_POINT ( 'NONE',  ( -5.405949406249996869, 9.363379034771805109, -63.84375000204836681 ) ) ;
#22311 = CARTESIAN_POINT ( 'NONE',  ( -9.999999999999998224, 1.224646799147353059E-15, -77.74999999999998579 ) ) ;
#22312 = CARTESIAN_POINT ( 'NONE',  ( -5.405949406250003975, -9.363379034771801557, -169.8437500020484094 ) ) ;
#22313 = CARTESIAN_POINT ( 'NONE',  ( 5.000000000000000000, 8.660254037844385522, -136.7499999999999716 ) ) ;
#22314 = CARTESIAN_POINT ( 'NONE',  ( 5.405949406249992428, -9.363379034771808662, -142.7812500020483810 ) ) ;
#22315 = CARTESIAN_POINT ( 'NONE',  ( 0.000000000000000000, 0.000000000000000000, -200.0000000000000000 ) ) ;
#22316 = CARTESIAN_POINT ( 'NONE',  ( -10.81189881249999729, 6.242252689847871849, -38.40625000204835970 ) ) ;
#22317 = CARTESIAN_POINT ( 'NONE',  ( 5.000000000000000000, 8.660254037844385522, -120.6250000040967905 ) ) ;
#22318 = CARTESIAN_POINT ( 'NONE',  ( -4.999999999999996447, 8.660254037844387298, -97.49999999999998579 ) ) ;
#22319 = EDGE_LOOP ( 'NONE', ( #7956, #11921, #25586, #38050 ) ) ;
#22320 = CARTESIAN_POINT ( 'NONE',  ( 10.81189881249999729, 0.000000000000000000, -117.0312500020483952 ) ) ;
#22321 = CARTESIAN_POINT ( 'NONE',  ( -9.999999999999998224, 5.773502691896259087, -138.2500000040967905 ) ) ;
#22322 = CARTESIAN_POINT ( 'NONE',  ( -9.999999999999998224, 1.224646799147353059E-15, -145.6250000040967905 ) ) ;
#22323 = CARTESIAN_POINT ( 'NONE',  ( -5.405949406249996869, 9.363379034771805109, -170.5312500020484094 ) ) ;
#22324 = CARTESIAN_POINT ( 'NONE',  ( 4.999999999999992006, -8.660254037844389075, -53.62500000409675494 ) ) ;
#22325 = CARTESIAN_POINT ( 'NONE',  ( 9.999999999999998224, 0.000000000000000000, -159.5000000000000000 ) ) ;
#22326 = CARTESIAN_POINT ( 'NONE',  ( -2.293366432827344421E-15, -12.48450537969573659, -63.40625000204838813 ) ) ;
#22327 = CARTESIAN_POINT ( 'NONE',  ( 4.999999999999992006, -8.660254037844389075, -134.6250000040967620 ) ) ;
#22328 = CARTESIAN_POINT ( 'NONE',  ( -10.81189881249999907, -6.242252689847864744, -171.6562500020484094 ) ) ;
#22329 = CARTESIAN_POINT ( 'NONE',  ( 9.999999999999678479, 5.773502691896442940, -183.7500000040967905 ) ) ;
#22330 = CARTESIAN_POINT ( 'NONE',  ( -10.00000000000102496, 5.773502691895664007, -64.37499999999994316 ) ) ;
#22331 = VERTEX_POINT ( 'NONE', #31017 ) ;
#22332 = CARTESIAN_POINT ( 'NONE',  ( 9.999999999999998224, 0.000000000000000000, -105.4999999999999858 ) ) ;
#22333 = CARTESIAN_POINT ( 'NONE',  ( 0.000000000000000000, 20.00000000000000000, -235.0000000000000000 ) ) ;
#22334 = ADVANCED_FACE ( 'NONE', ( #1879 ), #34258, .T. ) ;
#22336 = ORIENTED_EDGE ( 'NONE', *, *, #24629, .F. ) ;
#22335 = CARTESIAN_POINT ( 'NONE',  ( -2.293366432827344421E-15, -12.48450537969573659, -79.90625000204839523 ) ) ;
#22337 = CARTESIAN_POINT ( 'NONE',  ( 0.000000000000000000, 0.000000000000000000, 0.000000000000000000 ) ) ;
#22339 = ORIENTED_EDGE ( 'NONE', *, *, #6671, .F. ) ;
#22338 = CARTESIAN_POINT ( 'NONE',  ( 4.999999999999992006, -8.660254037844389075, -100.1250000040967905 ) ) ;
#22340 = VERTEX_POINT ( 'NONE', #31660 ) ;
#22341 = CARTESIAN_POINT ( 'NONE',  ( -5.405949406250003975, -9.363379034771801557, -28.84375000204836326 ) ) ;
#22342 = CARTESIAN_POINT ( 'NONE',  ( 9.999999999999998224, 0.000000000000000000, -170.3750000040968189 ) ) ;
#22343 = CARTESIAN_POINT ( 'NONE',  ( -10.81189881249999729, 1.324075727343319199E-15, -9.781250002048352599 ) ) ;
#22345 = ORIENTED_EDGE ( 'NONE', *, *, #29898, .F. ) ;
#22344 = CARTESIAN_POINT ( 'NONE',  ( 7.644554776091147741E-16, 12.48450537969573659, -53.46875000204837391 ) ) ;
#22346 = CYLINDRICAL_SURFACE ( 'NONE', #21536, 9.999999999999998224 ) ;
#22347 = CARTESIAN_POINT ( 'NONE',  ( 10.00000000000000000, 5.773502691896255534, -31.87499999999995737 ) ) ;
#22348 = CARTESIAN_POINT ( 'NONE',  ( 10.81189881249999551, -6.242252689847874514, -185.9687500020484094 ) ) ;
#22349 = CARTESIAN_POINT ( 'NONE',  ( 7.644554776091147741E-16, 12.48450537969573659, -179.4687500020483810 ) ) ;
#22350 = CARTESIAN_POINT ( 'NONE',  ( -10.81189881249999729, 6.242252689847871849, -155.2187500020483810 ) ) ;
#22351 = CARTESIAN_POINT ( 'NONE',  ( 10.81189881249999551, -6.242252689847874514, -170.9687500020483810 ) ) ;
#22352 = CARTESIAN_POINT ( 'NONE',  ( 7.070501591499376803E-16, 11.54700538379251284, -41.00000000409676204 ) ) ;
#22353 = DIRECTION ( 'NONE',  ( 1.000000000000000000, 0.000000000000000000, 0.000000000000000000 ) ) ;
#22354 = CARTESIAN_POINT ( 'NONE',  ( -9.999999999999998224, 5.773502691896259087, -196.3750000000000568 ) ) ;
#22355 = CARTESIAN_POINT ( 'NONE',  ( 5.405949406249992428, -9.363379034771808662, -103.5937500020483668 ) ) ;
#22356 = CARTESIAN_POINT ( 'NONE',  ( 10.00000000000102318, -5.773502691895667560, -84.62499999999995737 ) ) ;
#22357 = CARTESIAN_POINT ( 'NONE',  ( -5.405949406250003975, -9.363379034771801557, -72.53125000204838102 ) ) ;
#22358 = CARTESIAN_POINT ( 'NONE',  ( 7.644554776091147741E-16, 12.48450537969573659, -80.46875000204838102 ) ) ;
#22359 = CARTESIAN_POINT ( 'NONE',  ( -5.405949406249996869, 9.363379034771805109, -59.53125000204836681 ) ) ;
#22360 = CARTESIAN_POINT ( 'NONE',  ( 4.999999999999992006, -8.660254037844389075, -149.6250000040967905 ) ) ;
#22361 = CARTESIAN_POINT ( 'NONE',  ( -5.000000000000003553, -8.660254037844383745, -119.5000000000000000 ) ) ;
#22362 = ORIENTED_EDGE ( 'NONE', *, *, #15152, .F. ) ;
#22363 = CARTESIAN_POINT ( 'NONE',  ( -10.81189881249999729, -6.242252689847864744, -143.1562500020484094 ) ) ;
#22364 = CARTESIAN_POINT ( 'NONE',  ( -10.81189881249999729, 1.324075727343319199E-15, -155.2812500020484094 ) ) ;
#22365 = CARTESIAN_POINT ( 'NONE',  ( -10.81189881249999729, 1.324075727343319199E-15, -194.2812500020484094 ) ) ;
#22366 = CARTESIAN_POINT ( 'NONE',  ( 5.405949406249992428, -9.363379034771808662, -88.59375000204838102 ) ) ;
#22367 = ORIENTED_EDGE ( 'NONE', *, *, #36507, .T. ) ;
#22368 = CARTESIAN_POINT ( 'NONE',  ( 9.999999999999996447, -5.773502691896262640, -65.12499999999998579 ) ) ;
#22369 = CARTESIAN_POINT ( 'NONE',  ( -2.293366432827344421E-15, -12.48450537969573659, -186.2187500020484094 ) ) ;
#22370 = CARTESIAN_POINT ( 'NONE',  ( 4.999999999999992006, -8.660254037844389075, -73.12500000409677625 ) ) ;
#22371 = CARTESIAN_POINT ( 'NONE',  ( 7.070501591499376803E-16, 11.54700538379251284, -165.1250000000000000 ) ) ;
#22372 = PLANE ( 'NONE',  #33751 ) ;
#22373 = CARTESIAN_POINT ( 'NONE',  ( 10.81189881249999729, 0.000000000000000000, -82.53125000204838102 ) ) ;
#22374 = CARTESIAN_POINT ( 'NONE',  ( -2.293366432827344421E-15, -12.48450537969573659, -64.90625000204838102 ) ) ;
#22375 =( BOUNDED_CURVE ( )  B_SPLINE_CURVE ( 2, ( #2136, #41600, #15476, #18728, #18943, #9228, #25437 ),
 .UNSPECIFIED., .F., .F. ) 
 B_SPLINE_CURVE_WITH_KNOTS ( ( 3, 2, 2, 3 ),
 ( 0.1305970149253731227, 0.1318407960199005080, 0.1330845771144278378, 0.1343283582089551953 ),
 .UNSPECIFIED. ) 
 CURVE ( )  GEOMETRIC_REPRESENTATION_ITEM ( )  RATIONAL_B_SPLINE_CURVE ( ( 1.000000000000000000, 0.8660254037844387076, 1.000000000000000000, 0.8660254037844387076, 1.000000000000000000, 0.8660254037844417052, 0.9999999999999970024 ) ) 
 REPRESENTATION_ITEM ( '' )  );
#22376 = CARTESIAN_POINT ( 'NONE',  ( 5.000000000000000000, 8.660254037844385522, -59.12500000409676204 ) ) ;
#22377 = CARTESIAN_POINT ( 'NONE',  ( 9.999999999999998224, 0.000000000000000000, -158.3750000040967905 ) ) ;
#22378 = CARTESIAN_POINT ( 'NONE',  ( -2.293366432827344421E-15, -12.48450537969573659, -15.21875000204836326 ) ) ;
#22379 = CARTESIAN_POINT ( 'NONE',  ( -9.999999999999998224, 1.224646799147353059E-15, -0.1250000040967647053 ) ) ;
#22380 = CARTESIAN_POINT ( 'NONE',  ( -10.81189881249999907, -6.242252689847864744, -192.6562500020484094 ) ) ;
#22381 = CARTESIAN_POINT ( 'NONE',  ( 10.81189881249999551, -6.242252689847874514, -18.15625000204837391 ) ) ;
#22382 = CARTESIAN_POINT ( 'NONE',  ( -10.81189881249999729, -6.242252689847864744, -1.968750002048357262 ) ) ;
#22383 = CARTESIAN_POINT ( 'NONE',  ( -79.99999999999992895, 19.99999999999998934, -160.0000000000000000 ) ) ;
#22384 = CARTESIAN_POINT ( 'NONE',  ( -5.000000000000003553, -8.660254037844383745, -107.8750000040967763 ) ) ;
#22385 =( BOUNDED_CURVE ( )  B_SPLINE_CURVE ( 2, ( #42284, #7108, #32392, #2816, #15948, #29351, #29144 ),
 .UNSPECIFIED., .F., .F. ) 
 B_SPLINE_CURVE_WITH_KNOTS ( ( 3, 2, 2, 3 ),
 ( 0.8283582089552240513, 0.8296019900497514366, 0.8308457711442787108, 0.8320895522388060961 ),
 .UNSPECIFIED. ) 
 CURVE ( )  GEOMETRIC_REPRESENTATION_ITEM ( )  RATIONAL_B_SPLINE_CURVE ( ( 0.9999999999999761302, 0.8660254037844625774, 1.000000000000000000, 0.8660254037844387076, 1.000000000000000000, 0.8660254037844267172, 1.000000000000011990 ) ) 
 REPRESENTATION_ITEM ( '' )  );
#22386 = CARTESIAN_POINT ( 'NONE',  ( -10.00000000000000000, -5.773502691896251982, -173.6249999999999716 ) ) ;
#22387 = CARTESIAN_POINT ( 'NONE',  ( 7.070501591499376803E-16, 11.54700538379251284, -166.6250000000000000 ) ) ;
#22389 = VERTEX_POINT ( 'NONE', #35107 ) ;
#22388 = CARTESIAN_POINT ( 'NONE',  ( -10.81189881249999907, -6.242252689847864744, -102.6562500020483952 ) ) ;
#22390 = CARTESIAN_POINT ( 'NONE',  ( 7.070501591499376803E-16, 11.54700538379251284, -37.62499999999995737 ) ) ;
#22391 = ORIENTED_EDGE ( 'NONE', *, *, #8821, .F. ) ;
#22392 = ORIENTED_EDGE ( 'NONE', *, *, #8605, .F. ) ;
#22393 = VECTOR ( 'NONE', #2951, 1000.000000000000000 ) ;
#22394 = CARTESIAN_POINT ( 'NONE',  ( -10.81189881249999907, -6.242252689847864744, -26.15625000204837391 ) ) ;
#22395 = SECURITY_CLASSIFICATION_LEVEL ( 'unclassified' ) ;
#22396 = CARTESIAN_POINT ( 'NONE',  ( 5.405949406249999534, 9.363379034771803333, -77.59375000204838102 ) ) ;
#22397 = CARTESIAN_POINT ( 'NONE',  ( 57.00000000000002132, 0.000000000000000000, -240.0000000000000000 ) ) ;
#22398 = ADVANCED_FACE ( 'NONE', ( #41559 ), #7920, .T. ) ;
#22399 = CARTESIAN_POINT ( 'NONE',  ( 9.999999999999998224, 0.000000000000000000, -138.8750000040968189 ) ) ;
#22400 = CARTESIAN_POINT ( 'NONE',  ( 5.000000000000000000, 8.660254037844385522, -30.62500000409676559 ) ) ;
#22401 = CARTESIAN_POINT ( 'NONE',  ( 10.81189881249999551, -6.242252689847874514, -159.1562500020484094 ) ) ;
#22402 = CARTESIAN_POINT ( 'NONE',  ( 9.999999999999998224, 0.000000000000000000, -14.37500000409674961 ) ) ;
#22403 = CARTESIAN_POINT ( 'NONE',  ( -9.999999999999998224, 1.224646799147353059E-15, -125.7499999999999716 ) ) ;
#22404 = CARTESIAN_POINT ( 'NONE',  ( 5.405949406249999534, 9.363379034771803333, -130.0937500020483810 ) ) ;
#22405 = CARTESIAN_POINT ( 'NONE',  ( -10.81189881249999729, 1.324075727343319199E-15, -96.78125000204839523 ) ) ;
#22406 = CARTESIAN_POINT ( 'NONE',  ( 7.644554776091147741E-16, 12.48450537969573659, -119.4687500020483668 ) ) ;
#22407 = CARTESIAN_POINT ( 'NONE',  ( -5.405949406250003975, -9.363379034771801557, -78.34375000204838102 ) ) ;
#22408 = CARTESIAN_POINT ( 'NONE',  ( -5.405949406250003975, -9.363379034771801557, -83.03125000204838102 ) ) ;
#22409 = CARTESIAN_POINT ( 'NONE',  ( 10.00000000000000000, 5.773502691896255534, -168.7500000040967905 ) ) ;
#22410 = LINE ( 'NONE', #29526, #14399 ) ;
#22411 = CARTESIAN_POINT ( 'NONE',  ( -2.293366432827344421E-15, -12.48450537969573659, -163.9062500020483810 ) ) ;
#22412 = CARTESIAN_POINT ( 'NONE',  ( -2.293366432827344421E-15, -12.48450537969573659, -178.9062500020484379 ) ) ;
#22413 = CARTESIAN_POINT ( 'NONE',  ( -10.81189881249999729, 1.324075727343319199E-15, -47.09375000204838102 ) ) ;
#22414 = CARTESIAN_POINT ( 'NONE',  ( 10.00000000000000000, 5.773502691896255534, -153.7500000040967905 ) ) ;
#22415 = CARTESIAN_POINT ( 'NONE',  ( -5.405949406250003975, -9.363379034771801557, -0.5312500020483723606 ) ) ;
#22416 = CARTESIAN_POINT ( 'NONE',  ( -10.81189881249999907, -6.242252689847864744, -3.468750002048353931 ) ) ;
#22417 = CARTESIAN_POINT ( 'NONE',  ( 5.000000000000000000, 8.660254037844385522, -6.249999999999977796 ) ) ;
#22418 = CARTESIAN_POINT ( 'NONE',  ( 10.81189881249999551, -6.242252689847874514, -110.9687500020483810 ) ) ;
#22419 = CARTESIAN_POINT ( 'NONE',  ( -4.999999999999996447, 8.660254037844387298, -91.49999999999998579 ) ) ;
#22420 = CARTESIAN_POINT ( 'NONE',  ( -10.81189881249999729, 6.242252689847871849, -12.90625000204836859 ) ) ;
#22421 = CARTESIAN_POINT ( 'NONE',  ( -10.00000000000000000, -5.773502691896251982, -100.5000000040967905 ) ) ;
#22422 = CARTESIAN_POINT ( 'NONE',  ( -4.999999999999996447, 8.660254037844387298, -150.3750000040967905 ) ) ;
#22423 = CARTESIAN_POINT ( 'NONE',  ( -5.405949406250003975, -9.363379034771801557, -111.5312500020483810 ) ) ;
#22424 = CARTESIAN_POINT ( 'NONE',  ( -10.81189881249999729, 6.242252689847871849, -89.40625000204838102 ) ) ;
#22425 = ORIENTED_EDGE ( 'NONE', *, *, #3654, .T. ) ;
#22426 = CARTESIAN_POINT ( 'NONE',  ( 10.00000000000000000, 5.773502691896255534, -93.75000000409677625 ) ) ;
#22427 = CARTESIAN_POINT ( 'NONE',  ( 5.000000000000000000, 8.660254037844385522, -29.12500000409676204 ) ) ;
#22428 = CARTESIAN_POINT ( 'NONE',  ( 10.81189881249999729, 0.000000000000000000, -43.34375000204837391 ) ) ;
#22429 = EDGE_LOOP ( 'NONE', ( #33484, #726, #20407, #32789 ) ) ;
#22430 = CARTESIAN_POINT ( 'NONE',  ( 10.00000000000000000, 5.773502691896255534, -15.37499999999997691 ) ) ;
#22431 = CARTESIAN_POINT ( 'NONE',  ( 7.644554776091147741E-16, 12.48450537969573659, -23.65625000204837747 ) ) ;
#22432 = CARTESIAN_POINT ( 'NONE',  ( 7.070501591499377789E-16, 11.54700538379251284, -156.1250000000000000 ) ) ;
#22433 = CARTESIAN_POINT ( 'NONE',  ( 9.999999999999996447, -5.773502691896262640, -20.50000000409676915 ) ) ;
#22434 = CARTESIAN_POINT ( 'NONE',  ( 4.999999999999992006, -8.660254037844389075, -197.2500000000000000 ) ) ;
#22436 = ORIENTED_EDGE ( 'NONE', *, *, #1201, .F. ) ;
#22435 = CARTESIAN_POINT ( 'NONE',  ( -2.293366432827344421E-15, -12.48450537969573659, -123.4062500020484094 ) ) ;
#22437 = CARTESIAN_POINT ( 'NONE',  ( -5.000000000000003553, -8.660254037844383745, -152.5000000000000000 ) ) ;
#22438 = AXIS2_PLACEMENT_3D ( 'NONE', #12357, #22096, #23313 ) ;
#22439 = EDGE_LOOP ( 'NONE', ( #34280, #8446, #20559, #24155 ) ) ;
#22440 = CARTESIAN_POINT ( 'NONE',  ( 5.405949406249999534, 9.363379034771803333, -50.78125000204835970 ) ) ;
#22441 = APPROVAL_ROLE ( '' ) ;
#22442 = CARTESIAN_POINT ( 'NONE',  ( -2.293366432827344421E-15, -12.48450537969573659, -100.7187500020483952 ) ) ;
#22444 = EDGE_LOOP ( 'NONE', ( #17268, #41777 ) ) ;
#22443 = EDGE_LOOP ( 'NONE', ( #42264, #39564, #14504, #20562 ) ) ;
#22445 = AXIS2_PLACEMENT_3D ( 'NONE', #25744, #15148, #2649 ) ;
#22446 =( BOUNDED_CURVE ( )  B_SPLINE_CURVE ( 2, ( #30525, #17531, #10851, #11488, #24902, #40406, #8279 ),
 .UNSPECIFIED., .F., .F. ) 
 B_SPLINE_CURVE_WITH_KNOTS ( ( 3, 2, 2, 3 ),
 ( 0.4776119402985076756, 0.4788557213930350054, 0.4800995024875623352, 0.4813432835820896649 ),
 .UNSPECIFIED. ) 
 CURVE ( )  GEOMETRIC_REPRESENTATION_ITEM ( )  RATIONAL_B_SPLINE_CURVE ( ( 0.9999999999999761302, 0.8660254037844625774, 1.000000000000000000, 0.8660254037844387076, 1.000000000000000000, 0.8660254037844267172, 1.000000000000011990 ) ) 
 REPRESENTATION_ITEM ( '' )  );
#22447 = DIRECTION ( 'NONE',  ( 1.000000000000000000, 0.000000000000000000, 0.000000000000000000 ) ) ;
#22448 = CARTESIAN_POINT ( 'NONE',  ( -2.121150477449813534E-15, -11.54700538379251284, -197.7500000040967905 ) ) ;
#22449 = CARTESIAN_POINT ( 'NONE',  ( -10.81189881249999907, -6.242252689847864744, -150.4687500020484094 ) ) ;
#22450 = CARTESIAN_POINT ( 'NONE',  ( 10.81189881249999907, 6.242252689847868297, -179.9062500020484094 ) ) ;
#22451 = CARTESIAN_POINT ( 'NONE',  ( -2.293366432827344421E-15, -12.48450537969573659, -6.218750002048345493 ) ) ;
#22452 = CARTESIAN_POINT ( 'NONE',  ( 9.999999999999998224, 0.000000000000000000, -132.5000000000000000 ) ) ;
#22453 = EDGE_CURVE ( 'NONE', #740, #40819, #10073, .T. ) ;
#22454 = CARTESIAN_POINT ( 'NONE',  ( -5.405949406250003975, -9.363379034771801557, -138.3437500020484094 ) ) ;
#22455 = CARTESIAN_POINT ( 'NONE',  ( -10.81189881249999729, 1.324075727343319199E-15, -99.59375000204838102 ) ) ;
#22456 = CARTESIAN_POINT ( 'NONE',  ( 9.999999999999998224, 0.000000000000000000, -200.0000000000000000 ) ) ;
#22457 = CARTESIAN_POINT ( 'NONE',  ( 10.81189881249999907, 6.242252689847868297, -112.4062500020483952 ) ) ;
#22458 = CARTESIAN_POINT ( 'NONE',  ( 4.999999999999992006, -8.660254037844389075, -190.1250000040967905 ) ) ;
#22459 = CARTESIAN_POINT ( 'NONE',  ( -2.293366432827344421E-15, -12.48450537969573659, -118.7187500020483668 ) ) ;
#22460 = CARTESIAN_POINT ( 'NONE',  ( -5.405949406250003975, -9.363379034771801557, -186.5312500020484094 ) ) ;
#22461 = CARTESIAN_POINT ( 'NONE',  ( 4.999999999999992006, -8.660254037844389075, -95.24999999999998579 ) ) ;
#22462 = CARTESIAN_POINT ( 'NONE',  ( 4.999999999999992006, -8.660254037844389075, -135.7499999999999716 ) ) ;
#22463 = CARTESIAN_POINT ( 'NONE',  ( -2.121150477449813534E-15, -11.54700538379251284, -0.8749999999999591438 ) ) ;
#22464 = CARTESIAN_POINT ( 'NONE',  ( 5.405949406249992428, -9.363379034771808662, -66.09375000204836681 ) ) ;
#22465 = CARTESIAN_POINT ( 'NONE',  ( 5.405949406249992428, -9.363379034771808662, -52.59375000204835260 ) ) ;
#22466 = CARTESIAN_POINT ( 'NONE',  ( 5.000000000000000000, 8.660254037844385522, -185.1250000040967905 ) ) ;
#22467 = CARTESIAN_POINT ( 'NONE',  ( 5.405949406249992428, -9.363379034771808662, -25.78125000204836681 ) ) ;
#22468 = CARTESIAN_POINT ( 'NONE',  ( 5.405949406249992428, -9.363379034771808662, -34.59375000204836681 ) ) ;
#22469 = CARTESIAN_POINT ( 'NONE',  ( 10.00000000000051159, -5.773502691895965988, -142.0000000040967905 ) ) ;
#22470 = CARTESIAN_POINT ( 'NONE',  ( 5.405949406249999534, 9.363379034771803333, -140.5937500020483810 ) ) ;
#22471 = CARTESIAN_POINT ( 'NONE',  ( -2.121150477449813534E-15, -11.54700538379251284, -111.8749999999999858 ) ) ;
#22472 = CARTESIAN_POINT ( 'NONE',  ( 0.000000000000000000, 0.000000000000000000, -200.0000000000000000 ) ) ;
#22473 = AXIS2_PLACEMENT_3D ( 'NONE', #2078, #2296, #18025 ) ;
#22474 = CARTESIAN_POINT ( 'NONE',  ( -2.121150477449813534E-15, -11.54700538379251284, -68.37499999999998579 ) ) ;
#22475 = CARTESIAN_POINT ( 'NONE',  ( -5.405949406250003975, -9.363379034771801557, -138.5312500020484094 ) ) ;
#22476 = CARTESIAN_POINT ( 'NONE',  ( 10.81189881249999729, 0.000000000000000000, -114.0312500020483952 ) ) ;
#22477 = VERTEX_POINT ( 'NONE', #34470 ) ;
#22478 = CARTESIAN_POINT ( 'NONE',  ( -10.00000000000012790, -5.773502691896177375, -176.6250000000000284 ) ) ;
#22479 = CARTESIAN_POINT ( 'NONE',  ( -5.000000000000003553, -8.660254037844383745, -115.3750000040967905 ) ) ;
#22480 = CARTESIAN_POINT ( 'NONE',  ( 0.000000000000000000, 0.000000000000000000, -240.0000000000000000 ) ) ;
#22481 = CARTESIAN_POINT ( 'NONE',  ( 5.405949406249992428, -9.363379034771808662, -75.09375000204838102 ) ) ;
#22482 = CARTESIAN_POINT ( 'NONE',  ( -2.121150477449813534E-15, -11.54700538379251284, -41.37499999999997158 ) ) ;
#22483 = CARTESIAN_POINT ( 'NONE',  ( -10.00000000000000000, -5.773502691896251982, -28.50000000409675138 ) ) ;
#22484 = CARTESIAN_POINT ( 'NONE',  ( 10.81189881249999729, 6.242252689847867408, -46.40625000204835970 ) ) ;
#22485 = VECTOR ( 'NONE', #39058, 1000.000000000000114 ) ;
#22486 = CARTESIAN_POINT ( 'NONE',  ( 9.999999999999998224, 0.000000000000000000, -141.5000000000000000 ) ) ;
#22487 = CARTESIAN_POINT ( 'NONE',  ( 5.000000000000000000, 8.660254037844385522, -42.62500000409677625 ) ) ;
#22488 = CARTESIAN_POINT ( 'NONE',  ( -2.293366432827344421E-15, -12.48450537969573659, -33.40625000204835970 ) ) ;
#22489 = CARTESIAN_POINT ( 'NONE',  ( 7.070501591499376803E-16, 11.54700538379251284, -156.5000000040968189 ) ) ;
#22490 = CARTESIAN_POINT ( 'NONE',  ( -5.405949406249996869, 9.363379034771805109, -137.5312500020484094 ) ) ;
#22491 = CARTESIAN_POINT ( 'NONE',  ( -10.81189881249999907, -6.242252689847864744, -150.6562500020484094 ) ) ;
#22492 = CARTESIAN_POINT ( 'NONE',  ( -4.999999999999996447, 8.660254037844387298, -153.0000000000000000 ) ) ;
#22493 = DIRECTION ( 'NONE',  ( 0.000000000000000000, 1.000000000000000000, 0.000000000000000000 ) ) ;
#22494 = VERTEX_POINT ( 'NONE', #4671 ) ;
#22495 =( BOUNDED_CURVE ( )  B_SPLINE_CURVE ( 2, ( #20065, #7774, #29804, #24180, #37327, #20917, #3466 ),
 .UNSPECIFIED., .F., .F. ) 
 B_SPLINE_CURVE_WITH_KNOTS ( ( 3, 2, 2, 3 ),
 ( 0.2686567164179105571, 0.2699004975124379424, 0.2711442786069652722, 0.2723880597014926574 ),
 .UNSPECIFIED. ) 
 CURVE ( )  GEOMETRIC_REPRESENTATION_ITEM ( )  RATIONAL_B_SPLINE_CURVE ( ( 0.9999999999999880096, 0.8660254037844506980, 1.000000000000000000, 0.8660254037844387076, 1.000000000000000000, 0.8660254037844267172, 1.000000000000011990 ) ) 
 REPRESENTATION_ITEM ( '' )  );
#22496 = ORIENTED_EDGE ( 'NONE', *, *, #20405, .T. ) ;
#22497 = EDGE_LOOP ( 'NONE', ( #6562, #42012, #2076, #30402 ) ) ;
#22498 = AXIS2_PLACEMENT_3D ( 'NONE', #21926, #24978, #11349 ) ;
#22499 = CYLINDRICAL_SURFACE ( 'NONE', #28401, 9.999999999999998224 ) ;
#22500 = CARTESIAN_POINT ( 'NONE',  ( -5.405949406250003975, -9.363379034771801557, -177.3437500020483810 ) ) ;
#22501 = CARTESIAN_POINT ( 'NONE',  ( -2.293366432827344421E-15, -12.48450537969573659, -31.71875000204834905 ) ) ;
#22502 = ADVANCED_FACE ( 'NONE', ( #11992 ), #41769, .T. ) ;
#22503 = ADVANCED_FACE ( 'NONE', ( #18040 ), #31236, .T. ) ;
#22504 = CARTESIAN_POINT ( 'NONE',  ( -10.81189881249999729, 6.242252689847871849, -164.2187500020483810 ) ) ;
#22505 = CARTESIAN_POINT ( 'NONE',  ( -10.81189881249999729, 6.242252689847871849, -146.2187500020483810 ) ) ;
#22506 = EDGE_CURVE ( 'NONE', #40819, #740, #1847, .T. ) ;
#22507 = DIRECTION ( 'NONE',  ( 0.000000000000000000, 0.000000000000000000, -1.000000000000000000 ) ) ;
#22508 = CARTESIAN_POINT ( 'NONE',  ( 5.405949406249992428, -9.363379034771808662, -129.0937500020483810 ) ) ;
#22509 = CARTESIAN_POINT ( 'NONE',  ( -10.81189881249999729, 6.242252689847871849, -143.4062500020484094 ) ) ;
#22510 = CARTESIAN_POINT ( 'NONE',  ( 5.405949406249999534, 9.363379034771803333, -19.09375000204835260 ) ) ;
#22512 = ADVANCED_FACE ( 'NONE', ( #8353 ), #1660, .T. ) ;
#22511 = CARTESIAN_POINT ( 'NONE',  ( -5.405949406250003975, -9.363379034771801557, -147.3437500020483810 ) ) ;
#22513 = CARTESIAN_POINT ( 'NONE',  ( -1.040834085586084257E-14, -145.0000000000000000, 37.50000000000000711 ) ) ;
#22514 = DIRECTION ( 'NONE',  ( -0.000000000000000000, -0.000000000000000000, 1.000000000000000000 ) ) ;
#22515 = CARTESIAN_POINT ( 'NONE',  ( -9.999999999999998224, 5.773502691896259087, -166.3749999999999716 ) ) ;
#22516 = CARTESIAN_POINT ( 'NONE',  ( 10.81189881249999551, -6.242252689847874514, -76.46875000204838102 ) ) ;
#22517 = CARTESIAN_POINT ( 'NONE',  ( 5.405949406249992428, -9.363379034771808662, -54.28125000204836681 ) ) ;
#22518 = CARTESIAN_POINT ( 'NONE',  ( 7.644554776091147741E-16, 12.48450537969573659, -57.96875000204837391 ) ) ;
#22519 = CYLINDRICAL_SURFACE ( 'NONE', #29567, 9.999999999999998224 ) ;
#22520 = CARTESIAN_POINT ( 'NONE',  ( -10.81189881249999729, 1.324075727343319199E-15, -170.0937500020484094 ) ) ;
#22521 = CARTESIAN_POINT ( 'NONE',  ( -4.999999999999996447, 8.660254037844387298, -136.5000000000000000 ) ) ;
#22522 = CARTESIAN_POINT ( 'NONE',  ( 5.405949406249999534, 9.363379034771803333, -149.7812500020483810 ) ) ;
#22523 = CC_DESIGN_PERSON_AND_ORGANIZATION_ASSIGNMENT ( #27261, #10847, ( #8303 ) ) ;
#22524 = CARTESIAN_POINT ( 'NONE',  ( 7.070501591499376803E-16, 11.54700538379251284, -15.50000000409676915 ) ) ;
#22525 = CARTESIAN_POINT ( 'NONE',  ( -5.000000000000003553, -8.660254037844383745, -122.8750000040967905 ) ) ;
#22526 = CARTESIAN_POINT ( 'NONE',  ( -4.999999999999996447, 8.660254037844387298, -91.49999999999998579 ) ) ;
#22527 = ORIENTED_EDGE ( 'NONE', *, *, #18315, .T. ) ;
#22528 = CARTESIAN_POINT ( 'NONE',  ( 10.81189881249999551, -6.242252689847874514, -121.6562500020483952 ) ) ;
#22529 = CARTESIAN_POINT ( 'NONE',  ( -9.999999999999998224, 1.224646799147353059E-15, -144.1250000040967905 ) ) ;
#22530 = CARTESIAN_POINT ( 'NONE',  ( 9.999999999999998224, 0.000000000000000000, -52.99999999999996447 ) ) ;
#22531 = CARTESIAN_POINT ( 'NONE',  ( -10.81189881249999729, 6.242252689847871849, -174.9062500020483810 ) ) ;
#22532 = CARTESIAN_POINT ( 'NONE',  ( 9.999999999999996447, -5.773502691896262640, -49.00000000409676915 ) ) ;
#22533 = CARTESIAN_POINT ( 'NONE',  ( -9.999999999999998224, 1.224646799147353059E-15, -160.2500000000000000 ) ) ;
#22534 = CARTESIAN_POINT ( 'NONE',  ( -5.405949406250003975, -9.363379034771801557, -60.53125000204836681 ) ) ;
#22535 = CARTESIAN_POINT ( 'NONE',  ( -9.999999999999998224, 1.224646799147353059E-15, -44.74999999999998579 ) ) ;
#22536 = CARTESIAN_POINT ( 'NONE',  ( 10.81189881249999551, -6.242252689847874514, -169.6562500020484094 ) ) ;
#22537 = EDGE_CURVE ( 'NONE', #28346, #17318, #14360, .T. ) ;
#22538 = CARTESIAN_POINT ( 'NONE',  ( -10.81189881249999907, -6.242252689847864744, -141.4687500020484094 ) ) ;
#22539 = CARTESIAN_POINT ( 'NONE',  ( 0.000000000000000000, 0.000000000000000000, -200.0000000000000000 ) ) ;
#22540 = CARTESIAN_POINT ( 'NONE',  ( 5.000000000000000000, 8.660254037844385522, -80.12500000409677625 ) ) ;
#22541 = EDGE_LOOP ( 'NONE', ( #9198, #28882, #15940, #41991 ) ) ;
#22542 = CARTESIAN_POINT ( 'NONE',  ( 9.999999999999998224, 1.224646799147353059E-15, -99.99999999999998579 ) ) ;
#22544 = ORIENTED_EDGE ( 'NONE', *, *, #12569, .F. ) ;
#22543 = CARTESIAN_POINT ( 'NONE',  ( 10.81189881249999551, -6.242252689847874514, -72.15625000204836681 ) ) ;
#22545 = DIRECTION ( 'NONE',  ( 0.000000000000000000, 0.000000000000000000, 1.000000000000000000 ) ) ;
#22546 = ORIENTED_EDGE ( 'NONE', *, *, #26483, .F. ) ;
#22547 = EDGE_CURVE ( 'NONE', #5178, #21158, #41116, .T. ) ;
#22548 = VERTEX_POINT ( 'NONE', #24765 ) ;
#22549 = CARTESIAN_POINT ( 'NONE',  ( 5.405949406249992428, -9.363379034771808662, -30.09375000204836326 ) ) ;
#22550 = CARTESIAN_POINT ( 'NONE',  ( -7.071067811865472841, -7.071067811865472841, -200.0000000000000000 ) ) ;
#22551 = CARTESIAN_POINT ( 'NONE',  ( 5.405949406249999534, 9.363379034771803333, -2.781250002048374359 ) ) ;
#22552 = CARTESIAN_POINT ( 'NONE',  ( 5.405949406249992428, -9.363379034771808662, -58.59375000204835970 ) ) ;
#22553 = DIRECTION ( 'NONE',  ( -1.000000000000000000, 0.000000000000000000, 0.000000000000000000 ) ) ;
#22554 = CARTESIAN_POINT ( 'NONE',  ( 10.00000000000000000, 5.773502691896255534, -28.87499999999998579 ) ) ;
#22555 = CARTESIAN_POINT ( 'NONE',  ( 5.405949406249999534, 9.363379034771803333, -188.5937500020483810 ) ) ;
#22556 = CARTESIAN_POINT ( 'NONE',  ( -5.405949406250003975, -9.363379034771801557, -169.8437500020484094 ) ) ;
#22557 = CARTESIAN_POINT ( 'NONE',  ( 10.81189881249999551, -6.242252689847874514, -160.4687500020484094 ) ) ;
#22558 = CARTESIAN_POINT ( 'NONE',  ( -10.81189881249999729, 6.242252689847871849, -167.2187500020484379 ) ) ;
#22559 = LINE ( 'NONE', #25183, #19822 ) ;
#22560 = CARTESIAN_POINT ( 'NONE',  ( -5.000000000000003553, -8.660254037844383745, -127.0000000000000000 ) ) ;
#22561 = CARTESIAN_POINT ( 'NONE',  ( -9.999999999999998224, 5.773502691896259087, -188.8750000000000568 ) ) ;
#22562 = CARTESIAN_POINT ( 'NONE',  ( 10.81189881249999551, -6.242252689847874514, -104.9687500020483810 ) ) ;
#22563 = CARTESIAN_POINT ( 'NONE',  ( 10.00000000000102318, -5.773502691895667560, -47.50000000409674783 ) ) ;
#22564 = CARTESIAN_POINT ( 'NONE',  ( -5.405949406249996869, 9.363379034771805109, -74.53125000204838102 ) ) ;
#22565 = DIRECTION ( 'NONE',  ( -1.000000000000000000, 0.000000000000000000, 0.000000000000000000 ) ) ;
#22566 = CARTESIAN_POINT ( 'NONE',  ( 10.81189881249999551, -6.242252689847874514, -83.96875000204838102 ) ) ;
#22567 = CARTESIAN_POINT ( 'NONE',  ( -10.81189881249999907, -6.242252689847864744, -57.65625000204838102 ) ) ;
#22568 = CARTESIAN_POINT ( 'NONE',  ( 5.000000000000000000, 8.660254037844385522, -143.1250000040967905 ) ) ;
#22569 = CARTESIAN_POINT ( 'NONE',  ( 5.000000000000000000, 8.660254037844385522, -117.2500000000000000 ) ) ;
#22570 = ORIENTED_EDGE ( 'NONE', *, *, #23848, .T. ) ;
#22571 = CARTESIAN_POINT ( 'NONE',  ( -10.81189881249999729, 6.242252689847871849, -143.4062500020484094 ) ) ;
#22572 = CARTESIAN_POINT ( 'NONE',  ( -10.81189881249999907, -6.242252689847864744, -155.1562500020484094 ) ) ;
#22573 = EDGE_CURVE ( 'NONE', #5984, #26792, #27769, .T. ) ;
#22574 = CARTESIAN_POINT ( 'NONE',  ( 5.405949406249992428, -9.363379034771808662, -193.7812500020484094 ) ) ;
#22575 = CARTESIAN_POINT ( 'NONE',  ( 10.00000000000051159, -5.773502691895965988, -179.1250000000000000 ) ) ;
#22576 = CARTESIAN_POINT ( 'NONE',  ( -10.81189881249999729, 6.242252689847871849, -89.21875000204836681 ) ) ;
#22577 = VECTOR ( 'NONE', #1549, 1000.000000000000000 ) ;
#22578 = VERTEX_POINT ( 'NONE', #21714 ) ;
#22579 = CARTESIAN_POINT ( 'NONE',  ( -2.121150477449813534E-15, -11.54700538379251284, -56.37499999999997868 ) ) ;
#22580 = CARTESIAN_POINT ( 'NONE',  ( -2.293366432827344421E-15, -12.48450537969573659, -192.2187500020484379 ) ) ;
#22581 = CARTESIAN_POINT ( 'NONE',  ( 10.00000000000000000, 5.773502691896255534, -75.75000000409679046 ) ) ;
#22582 = CARTESIAN_POINT ( 'NONE',  ( -9.999999999999998224, 1.224646799147353059E-15, -117.1250000040967905 ) ) ;
#22583 =( BOUNDED_CURVE ( )  B_SPLINE_CURVE ( 2, ( #16621, #29825, #23127, #22489, #25946, #35664, #39095 ),
 .UNSPECIFIED., .F., .F. ) 
 B_SPLINE_CURVE_WITH_KNOTS ( ( 3, 2, 2, 3 ),
 ( 0.2089552238805970630, 0.2101990049751244205, 0.2114427860696518058, 0.2126865671641791633 ),
 .UNSPECIFIED. ) 
 CURVE ( )  GEOMETRIC_REPRESENTATION_ITEM ( )  RATIONAL_B_SPLINE_CURVE ( ( 0.9999999999999940048, 0.8660254037844447028, 1.000000000000000000, 0.8660254037844387076, 1.000000000000000000, 0.8660254037844327124, 1.000000000000005995 ) ) 
 REPRESENTATION_ITEM ( '' )  );
#22584 = CARTESIAN_POINT ( 'NONE',  ( 9.999999999998456346, 5.773502691897149042, -12.75000000409671941 ) ) ;
#22585 = CARTESIAN_POINT ( 'NONE',  ( 5.405949406249999534, 9.363379034771803333, -85.28125000204838102 ) ) ;
#22586 = CARTESIAN_POINT ( 'NONE',  ( 7.644554776091147741E-16, 12.48450537969573659, -70.15625000204839523 ) ) ;
#22587 = CARTESIAN_POINT ( 'NONE',  ( -9.999999999999998224, 1.224646799147353059E-15, -61.62500000409676204 ) ) ;
#22588 = CARTESIAN_POINT ( 'NONE',  ( -10.81189881249999729, 1.324075727343319199E-15, -17.09375000204835260 ) ) ;
#22589 = CARTESIAN_POINT ( 'NONE',  ( 9.999999999999479527, 5.773502691896553074, -100.8749999999999716 ) ) ;
#22590 = CARTESIAN_POINT ( 'NONE',  ( -2.293366432827344421E-15, -12.48450537969573659, -193.9062500020484094 ) ) ;
#22591 = CARTESIAN_POINT ( 'NONE',  ( -10.81189881249999729, 6.242252689847871849, -15.90625000204837036 ) ) ;
#22592 = CARTESIAN_POINT ( 'NONE',  ( 5.405949406249992428, -9.363379034771808662, -3.093750002048367698 ) ) ;
#22593 = CYLINDRICAL_SURFACE ( 'NONE', #18630, 20.00000000000000355 ) ;
#22594 = LINE ( 'NONE', #12645, #28388 ) ;
#22595 = CARTESIAN_POINT ( 'NONE',  ( -9.999999999999998224, 1.224646799147353059E-15, -173.7500000000000284 ) ) ;
#22596 = CARTESIAN_POINT ( 'NONE',  ( 9.999999999999998224, 0.000000000000000000, -171.5000000000000000 ) ) ;
#22597 = CARTESIAN_POINT ( 'NONE',  ( 7.070501591499376803E-16, 11.54700538379251284, -97.62499999999997158 ) ) ;
#22599 = ORIENTED_EDGE ( 'NONE', *, *, #10123, .T. ) ;
#22598 = CARTESIAN_POINT ( 'NONE',  ( -10.81189881249999729, 6.242252689847871849, -98.40625000204838102 ) ) ;
#22600 = CARTESIAN_POINT ( 'NONE',  ( -9.999999999999998224, 1.224646799147353059E-15, -200.0000000000000000 ) ) ;
#22601 = VERTEX_POINT ( 'NONE', #11776 ) ;
#22602 = VERTEX_POINT ( 'NONE', #37909 ) ;
#22603 = B_SPLINE_CURVE_WITH_KNOTS ( 'NONE', 3,
 ( #4689, #35124, #41576, #15453, #11792, #21730, #1465, #21086, #34488, #4910, #18058, #28440, #15023, #24995, #5548, #24780, #18489, #31253, #2111, #37925, #21521, #18700, #31896, #1680, #2324, #28651, #41782, #14808 ),
 .UNSPECIFIED., .F., .F.,
 ( 4, 2, 2, 2, 2, 2, 2, 2, 2, 2, 2, 2, 2, 4 ),
 ( 0.000000000000000000, 0.001286352574009830274, 0.002572705148019660548, 0.005145410296039321096, 0.006431762870049149636, 0.007718115444058978175, 0.009004468018068808449, 0.01029082059207863699, 0.01286352574009829233, 0.01543623088811794768, 0.01672258346212777622, 0.01800893603613760649, 0.01929528861014742983, 0.02058164118415726010 ),
 .UNSPECIFIED. ) ;
#22604 = CARTESIAN_POINT ( 'NONE',  ( -5.405949406250003975, -9.363379034771801557, -37.84375000204837391 ) ) ;
#22605 = CARTESIAN_POINT ( 'NONE',  ( -10.81189881249999729, 6.242252689847871849, -30.90625000204834905 ) ) ;
#22606 = COORDINATED_UNIVERSAL_TIME_OFFSET ( 6, 0, .AHEAD. ) ;
#22607 = CARTESIAN_POINT ( 'NONE',  ( 7.644554776091147741E-16, 12.48450537969573659, -81.96875000204839523 ) ) ;
#22608 = DIRECTION ( 'NONE',  ( 0.000000000000000000, -1.000000000000000000, 0.000000000000000000 ) ) ;
#22609 = VECTOR ( 'NONE', #38116, 1000.000000000000114 ) ;
#22610 = VECTOR ( 'NONE', #39738, 1000.000000000000000 ) ;
#22611 = CARTESIAN_POINT ( 'NONE',  ( 10.81189881249999729, 0.000000000000000000, -197.8437500020484094 ) ) ;
#22612 =( BOUNDED_CURVE ( )  B_SPLINE_CURVE ( 2, ( #34508, #15679, #35142, #8805, #18508, #2341, #6209 ),
 .UNSPECIFIED., .F., .F. ) 
 B_SPLINE_CURVE_WITH_KNOTS ( ( 3, 2, 2, 3 ),
 ( 0.1417910447761193959, 0.1430348258706467535, 0.1442786069651741387, 0.1455223880597014963 ),
 .UNSPECIFIED. ) 
 CURVE ( )  GEOMETRIC_REPRESENTATION_ITEM ( )  RATIONAL_B_SPLINE_CURVE ( ( 1.000000000000000000, 0.8660254037844387076, 1.000000000000000000, 0.8660254037844387076, 1.000000000000000000, 0.8660254037844387076, 1.000000000000000000 ) ) 
 REPRESENTATION_ITEM ( '' )  );
#22613 = CARTESIAN_POINT ( 'NONE',  ( -11.54700538379250396, -20.00000000000000355, 0.000000000000000000 ) ) ;
#22614 = CARTESIAN_POINT ( 'NONE',  ( 7.070501591499376803E-16, 11.54700538379251284, -49.62499999999997868 ) ) ;
#22615 = CARTESIAN_POINT ( 'NONE',  ( -2.293366432827344421E-15, -12.48450537969573659, -157.9062500020483810 ) ) ;
#22616 = CARTESIAN_POINT ( 'NONE',  ( -10.00000000000000000, -5.773502691896251982, -9.000000004096754935 ) ) ;
#22617 = CARTESIAN_POINT ( 'NONE',  ( 9.999999999999998224, 0.000000000000000000, -99.87500000409679046 ) ) ;
#22618 = CARTESIAN_POINT ( 'NONE',  ( 5.405949406249999534, 9.363379034771803333, -125.5937500020483668 ) ) ;
#22619 = CARTESIAN_POINT ( 'NONE',  ( 10.81189881249999729, 0.000000000000000000, -94.53125000204838102 ) ) ;
#22620 = CARTESIAN_POINT ( 'NONE',  ( 7.644554776091147741E-16, 12.48450537969573659, -108.9687500020483668 ) ) ;
#22621 = CARTESIAN_POINT ( 'NONE',  ( 5.405949406249999534, 9.363379034771803333, -79.09375000204838102 ) ) ;
#22622 = CARTESIAN_POINT ( 'NONE',  ( -5.405949406250003975, -9.363379034771801557, -87.53125000204838102 ) ) ;
#22623 = CARTESIAN_POINT ( 'NONE',  ( 7.070501591499377789E-16, 11.54700538379251284, -167.0000000040967905 ) ) ;
#22624 =( BOUNDED_CURVE ( )  B_SPLINE_CURVE ( 2, ( #29915, #13477, #26668, #26878, #40033, #7238, #12167 ),
 .UNSPECIFIED., .F., .F. ) 
 B_SPLINE_CURVE_WITH_KNOTS ( ( 3, 2, 2, 3 ),
 ( 0.1156716417910447492, 0.1169154228855721483, 0.1181592039800995753, 0.1194029850746269744 ),
 .UNSPECIFIED. ) 
 CURVE ( )  GEOMETRIC_REPRESENTATION_ITEM ( )  RATIONAL_B_SPLINE_CURVE ( ( 1.000000000000003109, 0.8660254037844358210, 1.000000000000000000, 0.8660254037844387076, 1.000000000000000000, 0.8660254037844267172, 1.000000000000011990 ) ) 
 REPRESENTATION_ITEM ( '' )  );
#22625 = CARTESIAN_POINT ( 'NONE',  ( 9.999999999999998224, 0.000000000000000000, -66.49999999999997158 ) ) ;
#22626 = CARTESIAN_POINT ( 'NONE',  ( -10.81189881249999729, 1.324075727343319199E-15, -165.7812500020484094 ) ) ;
#22627 = CARTESIAN_POINT ( 'NONE',  ( 10.81189881249999551, -6.242252689847874514, -180.1562500020484379 ) ) ;
#22628 = EDGE_CURVE ( 'NONE', #20876, #342, #27558, .T. ) ;
#22629 = CARTESIAN_POINT ( 'NONE',  ( 10.00000000000000000, 5.773502691896255534, -159.7500000040967905 ) ) ;
#22630 = DIRECTION ( 'NONE',  ( -0.7559289460184526188, -8.392497208503125347E-17, 0.6546536707079791961 ) ) ;
#22631 = CARTESIAN_POINT ( 'NONE',  ( 5.405949406249992428, -9.363379034771808662, -9.093750002048345493 ) ) ;
#22632 = CARTESIAN_POINT ( 'NONE',  ( -2.121150477449813534E-15, -11.54700538379251284, -59.75000000409676915 ) ) ;
#22633 = CARTESIAN_POINT ( 'NONE',  ( 10.81189881249999907, 6.242252689847868297, -115.2187500020483810 ) ) ;
#22634 = CARTESIAN_POINT ( 'NONE',  ( -2.121150477449813534E-15, -11.54700538379251284, -87.87499999999997158 ) ) ;
#22635 = CARTESIAN_POINT ( 'NONE',  ( 5.405949406249999534, 9.363379034771803333, -14.78125000204835793 ) ) ;
#22636 = CARTESIAN_POINT ( 'NONE',  ( 5.000000000000000000, 8.660254037844385522, -95.12500000409677625 ) ) ;
#22637 = DIRECTION ( 'NONE',  ( -0.000000000000000000, -0.000000000000000000, -1.000000000000000000 ) ) ;
#22638 = CARTESIAN_POINT ( 'NONE',  ( -10.81189881249999907, -6.242252689847864744, -111.6562500020483952 ) ) ;
#22639 = CARTESIAN_POINT ( 'NONE',  ( -2.293366432827344421E-15, -12.48450537969573659, -90.40625000204838102 ) ) ;
#22640 = ORIENTED_EDGE ( 'NONE', *, *, #22059, .F. ) ;
#22641 =( BOUNDED_SURFACE ( )  B_SPLINE_SURFACE ( 1, 2, ( 
 ( #32590, #19607, #15312, #25480, #18982, #5619, #22017, #16138, #29338, #12906, #18770, #36027, #22231, #15515, #38414, #28720, #35403, #26102, #38626, #5828, #39256, #32169, #22434, #42063, #9689, #22865, #6465, #42269, #32787, #28508, #41639, #2804, #12074, #12493, #25269, #8858, #25685, #38838, #35613, #6041, #19191, #32380, #15936, #16781, #39466, #40097, #424, #10318, #36865, #10108, #29982, #13117, #17208, #13546, #26730, #33226, #9900, #36234, #10529, #39736, #20670, #26940, #23504, #7307, #13749, #23712, #20457, #16349, #39883, #23284, #13333, #16999, #26316, #33645, #29770, #23932, #36654, #23076, #7519, #30198, #6666, #36446, #26523, #33437, #19817, #214, #16570, #3655, #20248, #634, #4068, #30410, #33005, #842, #7096, #3226, #27157, #6880, #3863, #29549, #10741, #13962, #20032, #3434, #40298, #37076, #39672, #30828, #34717, #31269, #4280, #8167, #34504, #11378, #40508, #37941, #14390, #24576, #40935, #11168, #18074, #1696, #4924, #27587, #37724, #37507, #14822, #17634, #28020, #28236, #14615, #18289, #21315, #1048, #17851, #27804, #31048, #15039, #21537, #37290, #40726, #21100, #31476, #4701, #34070, #1909, #41150, #11588, #4491, #24795, #8386, #5141, #14172, #24150, #41371, #1266, #10953, #11807, #25010, #27373, #1479, #24365, #38152, #7736, #8595, #20883, #33856, #17422, #30619, #7950, #34287, #38995, #12859, #18933, #35564, #22179, #32328, #5564, #29285, #15880, #2337, #12648, #31910, #26053, #21958, #19349, #25839, #39204, #19142, #32536, #25219, #9431, #42430, #12024, #35350, #28876, #42009, #35138, #15466, #21750, #38363, #29082, #18716, #5779, #2754, #5992, #28667, #9217, #12233, #12438, #28458, #22386, #25425, #2964, #16091, #38568, #8801, #42219, #41796, #9011, #2548, #15258, #25633, #32117, #34928, #15675, #31693, #5349, #22596, #2126, #38791, #35773, #6203, #18504, #41591, #42640, #6616, #26469, #23234, #39618, #36394, #16302, #6825, #3381, #13492, #19981, #29716, #33170, #6413, #3176, #3602, #39414, #29929, #16517, #16731, #370, #29498, #26680, #19553, #160, #23450, #13067, #10055, #32738, #26263, #39832, #9640, #10265, #9848, #22813, #23025, #35976, #36177, #19768, #32951, #13282, #4753, #4975, #11859, #7568, #17682, #11218, #40560, #14224, #18121, #31316, #1748, #27425, #28285, #14445, #11004, #30669, #24198, #1312, #14875, #34119, #37347, #41199, #4540, #1531, #7794, #21587, #28072, #8434, #34549, #11639, #37990, #25057, #37773, #1959, #34335, #33912, #24843, #20936, #30878, #34766, #5187, #4332, #31531, #27637, #21149, #1097, #18341, #17900, #14664, #15088, #40777, #31098, #17471, #41422, #27853, #40987, #37558, #24418, #7997, #20721, #11429, #24626, #8217, #21366, #42266, #6038, #32377, #12692, #8644, #22227, #2385, #5613, #9264, #18556, #25888, #22432, #19187, #12072, #2801, #35401, #19395, #29131, #2595, #15930, #31746, #41636, #39042, #31956, #22647, #32165, #9479, #35820, #25266, #6252, #2174, #5825, #12904, #38412, #35611, #15309, #18767, #32587, #38200, #3012, #28506, #16136, #22013, #29335, #18980, #8853, #15512, #42476, #15724, #21799, #34979, #5405, #28717, #41843, #35186, #12281, #25477, #38623, #9059, #28923, #42059, #12488, #25682, #38835, #29546, #19814, #23501, #9897, #41804, #16996, #23072, #20029, #16347, #40093, #3860, #26936, #10315, #30193, #13746, #837, #13541, #20453, #10104, #9687, #629, #13114, #26313, #36650, #7094, #22861, #7303, #32785, #39668, #19604, #20244, #23281, #33220, #10525, #33001, #36441, #36024, #23709, #6877, #3651, #13330, #3223, #39463, #33433, #6462, #26100, #36860, #16778, #33641, #4062, #17204, #30405, #39251, #29978, #3430, #36229, #39879, #6663, #16567, #29764, #210, #421, #26520, #26726, #6123, #25976, #12988, #22735, #41931, #19481, #36106, #42144, #16017, #2674, #9352, #39127, #38492, #5707, #12784, #38711, #29424, #38921, #32667, #35901, #32038, #9561, #8936, #12575, #19693, #2468, #29213, #22100, #12362, #6338, #2266, #3096, #25346, #16224, #28799, #42565, #25768, #15597, #22313, #9772, #22521, #42352, #6540, #15387, #25560, #5913, #35274, #18858, #26185, #39333, #22952, #9145, #28586, #35486, #19066, #32247, #15808, #29004, #41714, #35694, #19268, #12153, #32462, #2887, #23156, #4153, #10610, #33730, #17083, #23797, #20541, #7605, #20328, #27239, #16866, #16437, #36952, #6750, #33089, #721, #30282, #29635, #14044, #39546, #3736, #26395, #27034, #30069, #39971, #7394, #39756, #511, #79, #17296, #13626, #26819, #20123, #9977, #36319, #40179, #13202, #32877, #13840, #10401, #30501, #927, #40382, #10824, #3308, #23592, #10191, #292, #3945, #19904, #24017, #16653, #37158, #36738, #3516, #29854, #13413, #33311, #26606, #7176, #23376, #36526, #6967, #33522, #8041, #37812, #18159, #34588, #1784, #37385, #14914, #17939, #2000, #11680, #4581, #31354, #15126, #1571, #5223, #8256, #30705, #4791, #14701, #31138, #28322, #8472, #24234, #1351, #21186, #18379, #34375, #20975, #31568, #5018, #27890, #34160, #21402, #41023, #38029, #1136, #11040, #21624, #17721, #40597, #41462, #34803, #14259, #11467, #30916, #41241, #7828, #24668, #27462, #28114, #24879, #11897, #25092, #14481, #38237, #20759, #33948, #4370, #17509, #27676, #40814, #11254, #24451, #37597, #42307, #18807, #12940, #8891, #6289, #12729, #26136, #6078, #19433, #12109, #25927, #16177, #41674, #9099, #15762, #28960, #22054, #31994, #8682, #25304, #15971, #35227, #22267, #19225, #35648, #5658, #38872, #41881, #42096, #15344, #9302, #12317, #32624, #3049, #25515, #38448, #29167, #2420, #15552, #32203, #2214, #12530, #21836, #29372, #28754, #22471, #35016, #42514, #39078, #38663, #31783, #25723, #2837, #5445, #35437, #9517, #32415, #18596, #22687, #35855, #28542, #5864, #19018, #2630, #30015, #3688, #16603, #23540, #36689, #10351, #19855, #16816, #246, #7129, #20283, #30232, #26973, #13994, #26768, #33678, #23324, #22905, #672, #13153, #39500, #33472, #3898, #36061, #20493, #3259, #10144, #32828, #17033, #36479, #461, #13790, #36272, #4105, #40132, #30, #33040, #26560, #36900, #6914, #9931, #7344, #10561, #33262, #23110, #39921, #13577, #23747, #19644, #29587, #17246, #6703, #16387, #30446, #877, #26347, #20067, #3468, #39288, #29806, #9722, #13368, #6495, #39707, #37975, #4959, #24182, #1733, #18325, #24401, #40970, #27621, #37756, #10987, #34751, #21349, #7776, #18106, #37329, #31514, #27407, #24829, #31301, #1944, #24607, #8419, #30652, #14859, #5171, #17455, #40761, #34321, #4738, #40543, #20919, #27190, #1082, #34535, #34101, #11203, #8200, #11413, #4524, #14649, #17667, #17884, #33894, #27838, #30861, #21570, #40334, #1297, #14208, #28056, #14428, #37542, #7982, #20706, #31082, #10776, #23965, #21133, #41182, #37109, #7553, #11622, #1515, #4316, #22211, #9250, #6239, #12056, #15917, #12472, #28271, #32151, #15710, #35387, #2370, #2581, #25667, #28909, #38821, #31729, #22419, #12266, #39030, #6025, #5811, #35597, #8628, #18538, #19175, #8839, #42254, #9046, #2788, #32364, #2159, #29118, #21784, #25462, #32573, #15293, #42046, #34964, #25252, #12679, #15069, #25876, #38184, #9465, #41622, #22634, #38607, #28490, #35173, #35807, #18964, #19383, #41407, #11841, #38397, #18752, #5387, #21995, #25042, #5598, #31942, #15496, #28702, #41829, #6448, #26087, #19590, #39450, #406, #29534, #32773, #36635, #42676, #39654, #36011, #16981, #23487, #3846, #29966, #7081, #33420, #20442, #33208, #40080, #29752, #29321, #20231, #3209, #16336, #13527, #26714, #42465, #26922, #9676, #16554, #39238, #39866, #197, #10091, #19801, #13102, #23269, #13318, #30179, #26507, #36428, #32989, #22849, #26301, #10300, #12893, #2999, #617, #6864, #13733, #10511, #23698, #36847, #16124, #20015, #9885, #23059, #16766, #36215, #7290, #6651, #3417, #3639, #825, #37922, #4686, #20868, #11362, #14374, #24557, #30392, #17405, #4264, #27785, #37707, #4049, #17616, #40490, #1032, #17835, #13946, #21297, #30603, #11571, #30811, #27139, #8368, #31030, #34052, #8149, #27571, #34485, #40282, #14155, #27355, #4474, #7933, #1462, #14595, #40919, #7499, #4907, #1250, #14805, #18054, #40706, #31249, #10723, #37060, #1677, #10936, #28001, #11149, #41131, #24777, #20651, #33627, #23916, #24348, #17193, #33838, #24129, #37271, #7720, #37489, #21083, #34271, #1891, #38773, #5331, #32098, #31893, #34909, #41573, #29065, #18697, #18915, #25823, #21518, #31674, #25201, #11789, #28219, #2531, #15656, #28856, #41352, #42203, #28437, #24991, #15020, #38133, #15239, #41992, #18486, #8576, #12421, #2108, #15450, #21726, #35545, #25615, #22368, #5762, #9199, #5975, #38978, #8992, #15864, #5545, #5119, #19126, #12006, #38342, #32311, #2734, #18268, #12629, #8784, #35121, #21941, #34699, #2321, #28648, #41778, #12212, #25405, #38551, #31457, #22160, #35335, #39395, #2948, #42413, #16716, #6185, #26874, #33152, #29697, #13472, #19966, #26036, #9622, #3582, #6811, #35757, #33371, #16076, #23009, #29269, #29911, #6596, #16499, #26246, #12844, #143, #19752, #23434, #36163, #32934, #9827, #39188, #22794, #350, #19324, #9414, #26664, #13264, #39814, #10246, #36582, #7029, #22579, #3366, #16284, #19538, #23218, #32519, #20181, #35956, #30126, #26450, #6397, #13683, #36376, #39602, #3791, #10036, #16925, #32722, #3155, #29482, #563, #42622, #13052, #11092, #21030, #13897, #34220, #37215, #21846, #30979, #4422, #4636, #33575, #771, #7882, #33786, #24502, #34001, #27732, #17782, #27090, #1408, #3998, #7662, #15354, #40233, #24295, #17141, #7446, #14538, #40029, #40868, #20384, #11309, #23862, #38248, #20815, #10668, #17352, #5455, #17562, #37439, #2227, #10459, #20599, #983, #30342, #37010, #8693, #35025, #18605, #4209, #31793, #30556, #14100, #27302, #40438, #10882, #23650, #24074, #30762, #36796, #1195, #14319, #27518, #7234, #40650, #29384, #12740, #19443, #16187, #3270, #15981, #22916, #12541, #12122, #32635, #2848, #29178, #6089, #35237, #3062, #9109, #19236, #35658, #5875, #25940, #39089, #42317, #22277, #32424, #32213, #9528, #12327, #22698, #36071, #9314, #12952, #35867, #38459, #22482, #19029, #25525, #6507, #42527, #32004, #35449, #15772, #26147, #42106, #28765, #39298, #6300, #9735, #41893, #19657, #32842, #28552, #8900, #18820, #41684, #38674, #5667, #25314, #22065, #2429, #25733, #2641, #15564, #28969, #38883, #23121, #20294, #40145, #27202, #36912, #13380, #33692, #7566, #13589, #30245, #16829, #26986, #259, #23978, #10573, #39721, #7358, #26572, #20718, #16615, #14007, #20505, #33909, #13802, #40346, #19868, #4118, #37122, #6716, #30028, #23553, #36701, #29818, #10157, #16400, #33054, #23759, #23338, #474, #17258, #685, #36490, #3911, #6927, #7141, #36286, #17045, #20080, #10789, #29600, #33274, #3480, #30461, #3700, #26782, #39934, #9942, #33485, #43, #13166, #10361, #888, #26360, #39513, #37988, #11215, #27422, #11427, #41195, #38198, #1310, #5185, #1746, #17468, #14873, #14662, #17680, #24416, #11856, #1529, #28069, #8642, #4330, #14443, #7994, #37344, #11002, #11636, #24841, #8432, #24196, #25055, #37556, #7791, #40558, #20934, #40774, #21585, #30875, #34116, #34763, #27635, #40985, #4538, #18339, #31529, #1957, #31314, #15083, #28283, #21797, #34547, #41420, #31096, #30667, #1095, #21147, #34333, #14222, #4751, #17897, #27851, #24622, #37770, #8215, #21364, #4973, #18119, #9057, #38409, #42057, #2593, #6251, #5823, #18978, #22224, #28504, #25264, #42265, #31743, #9686, #15929, #12486, #39041, #2799, #29130, #9478, #5402, #32163, #41841, #2383, #6036, #15307, #22646, #18765, #12903, #15722, #2172, #39249, #19186, #35399, #12690, #28920, #25887, #41634, #31954, #5610, #25680, #9262, #32375, #35818, #19394, #8851, #32586, #38832, #16135, #3011, #22430, #29333, #12070, #22010, #42475, #28715, #26099, #35609, #34977, #18553, #35184, #15510, #12279, #25475, #38621, #23071, #7092, #42688, #33000, #26933, #40292, #3858, #3221, #40091, #6662, #10522, #36023, #6875, #29763, #3428, #36647, #16346, #23707, #19812, #834, #20027, #32784, #27149, #20242, #10103, #627, #3650, #13743, #19603, #16566, #36227, #23280, #39878, #33431, #16993, #30191, #39462, #36858, #33219, #4060, #7301, #29977, #20451, #29545, #26312, #33638, #209, #17202, #16777, #30403, #13956, #9896, #22860, #13113, #420, #6461, #13329, #26519, #39667, #36439, #13540, #26725, #10311, #23499, #28013, #37282, #21307, #21093, #24141, #30822, #18278, #7942, #8159, #15030, #10734, #20877, #14384, #1041, #17415, #34495, #4917, #18065, #30613, #31468, #17627, #14166, #33850, #27365, #4485, #31261, #7729, #40501, #1687, #34063, #4696, #10946, #24788, #14816, #11580, #37717, #41141, #37932, #28229, #40928, #5131, #37500, #37070, #8378, #1260 ),
 ( #11371, #31041, #27581, #21528, #40718, #1473, #17845, #11159, #34710, #1901, #24568, #24358, #14607, #34281, #23926, #27797, #7512, #20662, #4274, #25833, #15668, #8588, #22171, #31903, #38355, #35767, #29075, #2119, #21952, #28660, #38988, #12225, #41584, #9424, #12431, #35345, #12016, #42003, #5773, #15873, #21740, #31685, #42213, #25212, #18497, #22590, #12640, #34920, #38562, #8794, #19136, #15249, #18926, #5342, #2542, #22380, #6195, #32321, #35133, #19339, #32529, #9003, #25627, #41790, #9209, #5556, #2958, #35557, #18709, #2747, #2332, #16085, #15461, #41363, #11800, #25003, #38784, #38145, #28449, #25417, #32110, #28869, #5985, #36388, #6821, #29493, #9841, #4008, #3168, #36592, #13062, #153, #26674, #13485, #42632, #16726, #19762, #19975, #35969, #29921, #32945, #26884, #40039, #3375, #16295, #7039, #26256, #23019, #10048, #22804, #33162, #33587, #10469, #23659, #32732, #33381, #36807, #19548, #29708, #3594, #363, #39405, #36172, #29280, #6608, #20192, #16510, #13273, #39825, #10258, #26463, #23444, #39612, #3800, #6407, #16939, #23228, #7245, #20395, #30136, #574, #13692, #42424, #12854, #26046, #39198, #9633, #21469, #41087, #37225, #4646, #17151, #24733, #8104, #24086, #40242, #24305, #11319, #8324, #14111, #18004, #14551, #30352, #34230, #17794, #37449, #23872, #21255, #40449, #7893, #21040, #7673, #1419, #27742, #30991, #10893, #40878, #20825, #24512, #993, #37665, #11530, #40662, #1634, #34443, #27100, #11102, #34012, #27314, #37880, #4862, #20610, #4433, #17572, #14762, #30773, #17363, #27958, #31206, #34651, #30564, #782, #13907, #10679, #37020, #7460, #33796, #1206, #4221, #14331, #27527, #41309, #2283, #2065, #25574, #38090, #41732, #11747, #8953, #28817, #15823, #38729, #15194, #22328, #38936, #15404, #18874, #5503, #15612, #31632, #12590, #41947, #28391, #9159, #41531, #9367, #5289, #2690, #35504, #22536, #2484, #5929, #25783, #8530, #18652, #12171, #25361, #18441, #11961, #5079, #21685, #12379, #25151, #31848, #19081, #32054, #38299, #35290, #8744, #38509, #24947, #5722, #21897, #29020, #42158, #35077, #34866, #32261, #28602, #22116, #18225, #31414, #1851, #14977, #28175, #13004, #23170, #35709, #524, #26623, #42581, #16032, #94, #29866, #26831, #32682, #36541, #33109, #6139, #9991, #36333, #13217, #42367, #39771, #16239, #26411, #39560, #26199, #19919, #3532, #6764, #29440, #16669, #39346, #307, #19497, #13426, #30085, #16454, #20137, #10205, #2903, #29652, #9788, #3112, #13640, #23391, #39144, #22967, #36123, #33324, #6554, #35916, #3748, #6982, #16882, #6352, #39984, #10415, #19283, #29228, #25994, #32477, #19710, #12799, #9575, #22750, #32891, #3321, #20555, #1364, #13854, #17522, #30296, #27474, #4596, #34388, #14496, #33745, #40826, #14714, #20773, #37399, #24033, #34177, #7408, #31153, #17735, #4166, #27688, #17311, #27903, #23812, #21202, #11268, #41037, #20990, #4805, #27051, #30723, #30929, #23608, #30515, #24464, #37611, #36753, #40609, #24249, #1150, #734, #8055, #941, #14273, #11052, #14060, #7842, #17954, #1585, #27253, #7189, #40393, #20344, #10838, #33536, #3958, #4383, #17097, #40195, #10625, #36965, #37171, #7620, #33962, #41900, #14929, #34817, #41479, #9115, #25106, #11698, #22285, #25319, #5460, #24894, #12128, #18609, #28771, #34602, #1801, #12333, #38043, #31367, #38681, #25532, #5033, #8699, #8485, #32010, #28127, #31802, #18174, #15359, #35245, #35457, #2435, #21638, #5882, #2646, #21852, #38465, #11912, #22070, #5241, #19036, #5676, #18394, #15570, #31582, #15778, #2014, #32220, #28975, #11480, #8907, #24681, #41257, #37828, #8270, #15143, #38253, #2234, #28557, #28341, #35031, #21417, #41689, #18826, #25947, #12959, #39520, #26367, #42325, #29605, #32642, #19663, #6096, #49, #3069, #40296, #10739, #16195, #29186, #7306, #12750, #22705, #22923, #35665, #6514, #4279, #23931, #19451, #13173, #42114, #7518, #33644, #6306, #22490, #35874, #32851, #3278, #29394, #9948, #23128, #36292, #42535, #16406, #26155, #20456, #39096, #4066, #37075, #36077, #27154, #17207, #9321, #30409, #39305, #9534, #20668, #840, #2857, #9742, #13961, #33855, #17421, #12548, #25740, #38892, #19243, #32432, #15989, #1478, #28019, #40506, #7734, #41149, #17632, #37288, #24793, #37940, #10952, #4700, #30827, #31268, #20882, #14613, #24148, #11376, #4923, #8385, #1694, #1265, #11587, #18287, #17850, #8165, #21098, #34502, #14389, #5140, #18071, #27586, #14821, #40725, #31474, #4490, #21535, #34716, #1908, #21314, #30618, #34069, #1046, #14171, #11165, #31047, #24575, #37723, #24364, #37505, #27371, #40934, #7948, #34285, #27802, #23849, #10656, #26652, #13883, #16912, #3986, #33140, #27079, #30114, #24060, #37203, #551, #13458, #33774, #39802, #7016, #7222, #19952, #33562, #30750, #7650, #3778, #40222, #26438, #33989, #17340, #33358, #6796, #17127, #20585, #17549, #23421, #27289, #36998, #39589, #760, #7433, #30330, #3568, #30543, #1183, #4196, #971, #14088, #40426, #10869, #20801, #10024, #10447, #13670, #36570, #4410, #16702, #23204, #10234, #36363, #23639, #29899, #337, #20168, #26863, #40017, #20373, #36785, #11080, #40856, #27720, #1613, #31394, #11727, #28154, #38070, #30965, #8510, #11509, #38279, #5268, #21447, #21664, #7870, #17770, #24925, #8082, #41509, #8301, #2042, #34845, #1396, #18420, #21018, #24711, #31830, #14526, #41288, #34208, #24490, #31610, #14305, #15173, #37427, #28370, #11296, #11942, #37857, #37643, #34419, #21880, #34630, #25133, #18636, #27504, #21233, #17983, #4624, #4838, #8726, #35058, #5486, #31183, #40639, #14742, #27935, #41064, #5056, #18204, #24282, #1828, #14956, #14685, #20741, #30482, #36934, #40796, #24436, #1334, #911, #27873, #4352, #14465, #30899, #1118, #8024, #21168, #37579, #17493, #27655, #27445, #34358, #7588, #4774, #18141, #4562, #8238, #11237, #33711, #17704, #14242, #33929, #31337, #11450, #27222, #30686, #11022, #21386, #37367, #24000, #34569, #17922, #5000, #40581, #10807, #31119, #37140, #24216, #1552, #17277, #41006, #28096, #1768, #7810, #24650, #23780, #14897, #37793, #20958, #4136, #41224, #7377, #34144, #20523, #14026, #40366, #24862, #29306, #12879, #32557, #18361, #16322, #35582, #2986, #19370, #32350, #39225, #9663, #26074, #6011, #16110, #15900, #22836, #38220, #35998, #6638, #35794, #39437, #42452, #21606, #6225, #2774, #9236, #19788, #42663, #15109, #19160, #42241, #9870, #25861, #11879, #23043, #6432, #19576, #25075, #32759, #3196, #29521, #34785, #1983, #13087, #22405, #31550, #36201, #26287, #5206, #9453, #29105, #32975, #28304, #3404, #41443, #16539, #29738, #11661, #38010, #12666, #8455, #39016, #22619, #13934, #606, #10708, #26702, #7706, #37050, #23475, #33827, #10288, #4460, #394, #40476, #4251, #17603, #40271, #10924, #3626, #17393, #20856, #33195, #13721, #7277, #20431, #13513, #36623, #185, #16753, #7487, #39854, #26911, #23905, #27128, #7070, #30380, #33409, #33616, #6850, #812, #3834, #24118, #40068, #20638, #20219, #34040, #30590, #16970, #1021, #30165, #13305, #10499, #37254, #14141, #26494, #27342, #39639, #29954, #10080, #23256, #23687, #36834, #4035, #17182, #36416, #20003, #5533, #4673, #38120, #14583, #1661, #28206, #15008, #31018, #18254, #21285, #8354, #37477, #31445, #34471, #28424, #41560, #4893, #17823, #8565, #1448, #11350, #11557, #24336, #37910, #35108, #11993, #8136, #1880, #30799, #38329, #21715, #37694, #11134, #21505, #24979, #24543, #34896, #27770, #7921, #1236, #5107, #41340, #34687, #21068, #5320, #18041, #11777, #18474, #31237, #31661, #2095, #15225, #14793, #25188, #27988, #8771, #40908, #21928, #14361, #24766, #27559, #40693, #34259, #41118, #9186, #15643, #13036, #6381, #22147, #41977, #5961, #16268, #32295, #18903, #29467, #32503, #12616, #32084, #19311, #25809, #35940, #41766, #8980, #19524, #2518, #38539, #3141, #32708, #12200, #15850, #28843, #39172, #35321, #38965, #25391, #22564, #42398, #42609, #9606, #12409, #26230, #9814, #29050, #2933, #26020, #25602, #2719, #16062, #29254, #38760, #6170, #22357, #9400, #5750, #12829, #35533, #39378, #22992, #19112, #42189, #22779, #35742, #36149, #18682, #31880, #2310, #15437, #28635, #26649, #36782, #6582, #14085, #40219, #13454, #29683, #13667, #758, #29895, #10653, #3565, #13248, #19738, #23636, #7218, #26860, #26435, #23845, #334, #40014, #10444, #39799, #33559, #3982, #20370, #10231, #17124, #23419, #30327, #33137, #13880, #968, #30110, #33771, #27076, #16484, #548, #36567, #16699, #27286, #36995, #10022, #7013, #20165, #4193, #33355, #6793, #17338, #7430, #20581, #19949, #30541, #40422, #10866, #127, #39586, #24057, #3775, #23201, #32918, #3351, #36360, #16909, #34205, #14953, #27501, #31180, #1180, #41061, #18200, #5265, #28151, #4621, #11724, #28367, #34416, #8299, #37640, #5053, #21015, #2039, #31391, #17767, #41285, #30961, #41506, #37424, #34841, #24922, #11938, #34627, #18417, #40636, #38066, #15170, #11076, #8079, #1609, #14739, #7867, #1393, #37199, #24279, #14523, #27932, #14301, #11506, #1825, #31607, #8507, #27716, #21661, #7647, #4834, #21443, #21230, #20798, #40854, #33986, #4407, #11293, #17546, #24487, #30748, #17980, #24708, #37854, #29420, #22517, #22731, #28582, #29209, #32663, #15384, #25556, #32243, #2670, #25342, #5704, #42560, #41711, #32457, #8933, #38707, #35690, #9348, #38489, #12571, #15593, #15803, #31827, #25764, #28795, #35897, #6334, #41926, #12150, #2883, #22097, #18855, #5909, #18633, #28999, #25130, #19477, #2463, #38917, #38276, #3093, #16013, #32035, #5483, #42140, #19264, #12358, #42348, #35271, #2263, #8722, #6119, #12780, #25972, #9141, #39123, #22309, #9557, #16220, #35482, #21877, #35055, #19062, #36315, #20119, #16649, #23587, #39542, #36734, #7390, #36522, #40174, #30065, #22948, #6962, #3512, #9973, #20537, #717, #16432, #6747, #288, #10606, #26602, #13198, #23793, #26815, #33307, #26391, #13623, #3732, #30278, #36102, #3304, #13836, #23153, #32873, #36948, #27030, #6536, #10187, #19900, #33518, #33084, #29850, #13409, #507, #10397, #39967, #7172, #29631, #20324, #23372, #33726, #3941, #16862, #17079, #19689, #74, #4149, #39752, #17293, #30497, #12984, #26181, #39328, #9768, #7601, #11250, #18375, #1132, #27886, #20755, #11036, #5014, #923, #24664, #24013, #18155, #27458, #11463, #24448, #14255, #20971, #8469, #40810, #41019, #5219, #14039, #24230, #4575, #33944, #4366, #37806, #8252, #21399, #17505, #31134, #27235, #21620, #34584, #7824, #37154, #8037, #31350, #37381, #1780, #40594, #30700, #40378, #17935, #1567, #21181, #34157, #14910, #17717, #34371, #4787, #30912, #28109, #41237, #14697, #1348, #11675, #14477, #24875, #27672, #38025, #34799, #37593, #10820, #5860, #41458, #12313, #22050, #28538, #25922, #19221, #35011, #12105, #18802, #29163, #2416, #31779, #42303, #2626, #25511, #2209, #32199, #38659, #6073, #11893, #21832, #32411, #15341, #8678, #15967, #2833, #25088, #28750, #41670, #9297, #5441, #9096, #38233, #35432, #12526, #12725, #22467, #25300, #18593, #39074, #38443, #42093, #41876, #8887, #35223, #9512, #22263, #28956, #35851, #31564, #5654, #31990, #15548, #19014, #25719, #22683, #15758, #35644, #38868, #6285, #1997, #15122, #28317, #13149, #16812, #3255, #22901, #33035, #36057, #26344, #6492, #33468, #39917, #20280, #3684, #10347, #7125, #36896, #6909, #13786, #3464, #3045, #23535, #19640, #32824, #30011, #457, #16173, #668, #26132, #16599, #12935, #13573, #29802, #26556, #36268, #16381, #39704, #242, #3894, #13364, #10140, #6699, #39285, #9718, #26764, #29368, #19430, #36685, #23320, #17029, #30228, #26969, #40127, #32620, #36475, #39496, #29583, #33258, #42509, #10557, #26, #23743, #20063, #9927, #23106, #19850, #37325, #27834, #30857, #40966, #4101, #33890, #20702, #7772, #24397, #4734, #21128, #31078, #23961, #1511, #4519, #31297, #11409, #14424, #14645, #873, #10772, #17881, #1078, #34531, #1294, #37752, #24603, #37105, #8196, #13989, #17663, #24825, #7549, #34317, #27186, #17451, #21345, #7340, #4955, #18102, #17242, #4312, #30647, #20915, #37538, #1729, #14855, #28052, #14204, #41178, #27617, #11617, #20489, #40757, #33675, #40330, #27403, #30442, #40539, #10983, #11199, #24178, #34098, #7978, #18960, #1940, #5594, #12675, #38180, #22207, #15066, #5383, #42042, #37971, #32147, #18321, #12469, #21780, #5807, #18747, #8624, #15289, #2784, #35169, #35382, #42250, #8415, #18534, #41618, #28266, #41403, #2577, #35593, #12262, #28905, #31725, #2154, #11837, #31510, #25038, #28486, #15706, #34960, #12052, #8835, #25248, #38393, #21991, #9245, #25663, #38818, #22415, #6021, #19171, #21566, #25458, #32360, #31939, #34747, #15913 ) ),
 .UNSPECIFIED., .F., .F., .F. ) 
 B_SPLINE_SURFACE_WITH_KNOTS ( ( 2, 2 ),
 ( 3, 2, 2, 2, 2, 2, 2, 2, 2, 2, 2, 2, 2, 2, 2, 2, 2, 2, 2, 2, 2, 2, 2, 2, 2, 2, 2, 2, 2, 2, 2, 2, 2, 2, 2, 2, 2, 2, 2, 2, 2, 2, 2, 2, 2, 2, 2, 2, 2, 2, 2, 2, 2, 2, 2, 2, 2, 2, 2, 2, 2, 2, 2, 2, 2, 2, 2, 2, 2, 2, 2, 2, 2, 2, 2, 2, 2, 2, 2, 2, 2, 2, 2, 2, 2, 2, 2, 2, 2, 2, 2, 2, 2, 2, 2, 2, 2, 2, 2, 2, 2, 2, 2, 2, 2, 2, 2, 2, 2, 2, 2, 2, 2, 2, 2, 2, 2, 2, 2, 2, 2, 2, 2, 2, 2, 2, 2, 2, 2, 2, 2, 2, 2, 2, 2, 2, 2, 2, 2, 2, 2, 2, 2, 2, 2, 2, 2, 2, 2, 2, 2, 2, 2, 2, 2, 2, 2, 2, 2, 2, 2, 2, 2, 2, 2, 2, 2, 2, 2, 2, 2, 2, 2, 2, 2, 2, 2, 2, 2, 2, 2, 2, 2, 2, 2, 2, 2, 2, 2, 2, 2, 2, 2, 2, 2, 2, 2, 2, 2, 2, 2, 2, 2, 2, 2, 2, 2, 2, 2, 2, 2, 2, 2, 2, 2, 2, 2, 2, 2, 2, 2, 2, 2, 2, 2, 2, 2, 2, 2, 2, 2, 2, 2, 2, 2, 2, 2, 2, 2, 2, 2, 2, 2, 2, 2, 2, 2, 2, 2, 2, 2, 2, 2, 2, 2, 2, 2, 2, 2, 2, 2, 2, 2, 2, 2, 2, 2, 2, 2, 2, 2, 2, 2, 2, 2, 2, 2, 2, 2, 2, 2, 2, 2, 2, 2, 2, 2, 2, 2, 2, 2, 2, 2, 2, 2, 2, 2, 2, 2, 2, 2, 2, 2, 2, 2, 2, 2, 2, 2, 2, 2, 2, 2, 2, 2, 2, 2, 2, 2, 2, 2, 2, 2, 2, 2, 2, 2, 2, 2, 2, 2, 2, 2, 2, 2, 2, 2, 2, 2, 2, 2, 2, 2, 2, 2, 2, 2, 2, 2, 2, 2, 2, 2, 2, 2, 2, 2, 2, 2, 2, 2, 2, 2, 2, 2, 2, 2, 2, 2, 2, 2, 2, 2, 2, 2, 2, 2, 2, 2, 2, 2, 2, 2, 2, 2, 2, 2, 2, 2, 2, 2, 2, 2, 2, 2, 2, 2, 2, 2, 2, 2, 2, 2, 2, 2, 2, 2, 2, 2, 2, 2, 2, 2, 2, 2, 2, 2, 2, 2, 2, 2, 2, 2, 2, 2, 2, 2, 2, 2, 2, 2, 2, 2, 2, 2, 2, 2, 2, 2, 2, 2, 2, 2, 2, 2, 2, 2, 2, 2, 2, 2, 2, 2, 2, 2, 2, 2, 2, 2, 2, 2, 2, 2, 2, 2, 2, 2, 2, 2, 2, 2, 2, 2, 2, 2, 2, 2, 2, 2, 2, 2, 2, 2, 2, 2, 2, 2, 2, 2, 2, 2, 2, 2, 2, 2, 2, 2, 2, 2, 2, 2, 2, 2, 2, 2, 2, 2, 2, 2, 2, 2, 2, 2, 2, 2, 2, 2, 2, 2, 2, 2, 2, 2, 2, 2, 2, 2, 2, 2, 2, 2, 2, 2, 2, 2, 2, 2, 2, 2, 2, 2, 2, 2, 2, 2, 2, 2, 2, 2, 2, 2, 2, 2, 2, 2, 2, 2, 2, 2, 2, 2, 2, 2, 2, 2, 2, 2, 2, 2, 2, 2, 2, 2, 2, 2, 2, 2, 2, 2, 2, 2, 2, 2, 2, 2, 2, 2, 2, 2, 2, 2, 2, 2, 2, 2, 2, 2, 2, 2, 2, 2, 2, 2, 2, 2, 2, 2, 2, 2, 2, 2, 2, 2, 2, 2, 2, 2, 2, 2, 2, 2, 2, 2, 2, 2, 2, 2, 2, 2, 2, 2, 2, 2, 2, 2, 2, 2, 2, 2, 2, 2, 2, 2, 2, 2, 2, 2, 2, 2, 2, 2, 2, 2, 2, 2, 2, 2, 2, 2, 2, 2, 2, 2, 2, 2, 2, 2, 2, 2, 2, 2, 2, 2, 2, 2, 2, 2, 2, 2, 2, 2, 2, 2, 2, 2, 2, 2, 2, 2, 2, 2, 2, 2, 2, 2, 2, 2, 2, 2, 2, 2, 2, 2, 2, 2, 2, 2, 2, 2, 2, 2, 2, 2, 2, 2, 2, 2, 2, 2, 2, 2, 2, 2, 2, 2, 2, 2, 2, 2, 2, 2, 2, 2, 2, 2, 2, 2, 2, 2, 2, 2, 2, 2, 2, 2, 2, 2, 2, 2, 2, 2, 2, 2, 2, 2, 2, 2, 2, 2, 2, 2, 2, 2, 2, 2, 2, 2, 2, 2, 2, 2, 2, 2, 2, 2, 2, 2, 2, 2, 2, 2, 2, 2, 2, 2, 2, 2, 2, 2, 2, 2, 2, 2, 2, 2, 2, 2, 2, 2, 2, 3 ),
 ( 0.000000000000000000, 1.000000000000000000 ),
 ( 0.000000000000000000, 0.001243781094527363160, 0.002487562189054726321, 0.003731343283582089481, 0.004975124378109452641, 0.006218905472636816235, 0.007462686567164178962, 0.008706467661691542556, 0.009950248756218905283, 0.01119402985074626801, 0.01243781094527363247, 0.01368159203980099520, 0.01492537313432835792, 0.01616915422885572065, 0.01741293532338308511, 0.01865671641791044610, 0.01990049751243781057, 0.02114427860696517503, 0.02238805970149253602, 0.02363184079601990048, 0.02487562189054726494, 0.02611940298507462593, 0.02736318407960199039, 0.02860696517412935486, 0.02985074626865671585, 0.03109452736318408031, 0.03233830845771144130, 0.03358208955223880576, 0.03482587064676617022, 0.03606965174129353469, 0.03731343283582089221, 0.03855721393034825667, 0.03980099502487562113, 0.04104477611940298559, 0.04228855721393035005, 0.04353233830845771452, 0.04477611940298507204, 0.04601990049751243650, 0.04726368159203980096, 0.04850746268656716542, 0.04975124378109452988, 0.05099502487562188741, 0.05223880597014925187, 0.05348258706467661633, 0.05472636815920398079, 0.05597014925373134525, 0.05721393034825870971, 0.05845771144278606724, 0.05970149253731343170, 0.06094527363184079616, 0.06218905472636816062, 0.06343283582089552508, 0.06467661691542288260, 0.06592039800995025400, 0.06716417910447761153, 0.06840796019900496905, 0.06965174129353234045, 0.07089552238805969797, 0.07213930348258706937, 0.07338308457711442689, 0.07462686567164178442, 0.07587064676616915582, 0.07711442786069651334, 0.07835820895522388474, 0.07960199004975124226, 0.08084577114427861366, 0.08208955223880597118, 0.08333333333333332871, 0.08457711442786070011, 0.08582089552238805763, 0.08706467661691542903, 0.08830845771144278655, 0.08955223880597014408, 0.09079601990049751548, 0.09203980099502487300, 0.09328358208955224440, 0.09452736318407960192, 0.09577114427860695944, 0.09701492537313433084, 0.09825870646766168837, 0.09950248756218905977, 0.1007462686567164173, 0.1019900497512437748, 0.1032338308457711462, 0.1044776119402985037, 0.1057213930348258751, 0.1069651741293532327, 0.1082089552238805902, 0.1094527363184079616, 0.1106965174129353191, 0.1119402985074626905, 0.1131840796019900480, 0.1144278606965174194, 0.1156716417910447769, 0.1169154228855721345, 0.1181592039800995059, 0.1194029850746268634, 0.1206467661691542348, 0.1218905472636815923, 0.1231343283582089498, 0.1243781094527363212, 0.1256218905472636926, 0.1268656716417910502, 0.1281094527363184077, 0.1293532338308457652, 0.1305970149253731227, 0.1318407960199005080, 0.1330845771144278655, 0.1343283582089552231, 0.1355721393034825806, 0.1368159203980099381, 0.1380597014925373234, 0.1393034825870646809, 0.1405472636815920384, 0.1417910447761193959, 0.1430348258706467535, 0.1442786069651741387, 0.1455223880597014963, 0.1467661691542288538, 0.1480099502487562113, 0.1492537313432835688, 0.1504975124378109541, 0.1517412935323383116, 0.1529850746268656692, 0.1542288557213930267, 0.1554726368159203842, 0.1567164179104477695, 0.1579601990049751270, 0.1592039800995024845, 0.1604477611940298420, 0.1616915422885572273, 0.1629353233830845848, 0.1641791044776119424, 0.1654228855721392999, 0.1666666666666666574, 0.1679104477611940427, 0.1691542288557214002, 0.1703980099502487577, 0.1716417910447761153, 0.1728855721393034728, 0.1741293532338308581, 0.1753731343283582156, 0.1766169154228855731, 0.1778606965174129306, 0.1791044776119402882, 0.1803482587064676734, 0.1815920398009950310, 0.1828358208955223885, 0.1840796019900497460, 0.1853233830845771035, 0.1865671641791044888, 0.1878109452736318463, 0.1890547263681592038, 0.1902985074626865614, 0.1915422885572139189, 0.1927860696517413042, 0.1940298507462686617, 0.1952736318407960192, 0.1965174129353233767, 0.1977611940298507343, 0.1990049751243781195, 0.2002487562189054771, 0.2014925373134328346, 0.2027363184079601921, 0.2039800995024875496, 0.2052238805970149349, 0.2064676616915422924, 0.2077114427860696499, 0.2089552238805970075, 0.2101990049751243650, 0.2114427860696517503, 0.2126865671641791078, 0.2139303482587064653, 0.2151741293532338228, 0.2164179104477611804, 0.2176616915422885656, 0.2189054726368159232, 0.2201492537313432807, 0.2213930348258706382, 0.2226368159203980235, 0.2238805970149253810, 0.2251243781094527385, 0.2263681592039800961, 0.2276119402985074536, 0.2288557213930348389, 0.2300995024875621964, 0.2313432835820895539, 0.2325870646766169114, 0.2338308457711442689, 0.2350746268656716542, 0.2363184079601990117, 0.2375621890547263693, 0.2388059701492537268, 0.2400497512437810843, 0.2412935323383084696, 0.2425373134328358271, 0.2437810945273631846, 0.2450248756218905422, 0.2462686567164178997, 0.2475124378109452850, 0.2487562189054726425, 0.2500000000000000000, 0.2512437810945273853, 0.2524875621890547150, 0.2537313432835821003, 0.2549751243781094301, 0.2562189054726368154, 0.2574626865671642006, 0.2587064676616915304, 0.2599502487562189157, 0.2611940298507462455, 0.2624378109452736307, 0.2636815920398010160, 0.2649253731343283458, 0.2661691542288557311, 0.2674129353233830608, 0.2686567164179104461, 0.2699004975124378314, 0.2711442786069651611, 0.2723880597014925464, 0.2736318407960198762, 0.2748756218905472615, 0.2761194029850746468, 0.2773631840796019765, 0.2786069651741293618, 0.2798507462686566916, 0.2810945273631840768, 0.2823383084577114621, 0.2835820895522387919, 0.2848258706467661772, 0.2860696517412935069, 0.2873134328358208922, 0.2885572139303482775, 0.2898009950248756073, 0.2910447761194029925, 0.2922885572139303223, 0.2935323383084577076, 0.2947761194029850929, 0.2960199004975124226, 0.2972636815920398079, 0.2985074626865671377, 0.2997512437810945229, 0.3009950248756219082, 0.3022388059701492380, 0.3034825870646766233, 0.3047263681592039530, 0.3059701492537313383, 0.3072139303482587236, 0.3084577114427860534, 0.3097014925373134386, 0.3109452736318407684, 0.3121890547263681537, 0.3134328358208955390, 0.3146766169154228687, 0.3159203980099502540, 0.3171641791044776393, 0.3184079601990049690, 0.3196517412935323543, 0.3208955223880596841, 0.3221393034825870694, 0.3233830845771144546, 0.3246268656716417844, 0.3258706467661691697, 0.3271144278606964995, 0.3283582089552238847, 0.3296019900497512700, 0.3308457711442785998, 0.3320895522388059851, 0.3333333333333333148, 0.3345771144278607001, 0.3358208955223880854, 0.3370646766169154152, 0.3383084577114428004, 0.3395522388059701302, 0.3407960199004975155, 0.3420398009950249008, 0.3432835820895522305, 0.3445273631840796158, 0.3457711442786069456, 0.3470149253731343308, 0.3482587064676617161, 0.3495024875621890459, 0.3507462686567164312, 0.3519900497512437609, 0.3532338308457711462, 0.3544776119402985315, 0.3557213930348258613, 0.3569651741293532465, 0.3582089552238805763, 0.3594527363184079616, 0.3606965174129353469, 0.3619402985074626766, 0.3631840796019900619, 0.3644278606965173917, 0.3656716417910447769, 0.3669154228855721622, 0.3681592039800994920, 0.3694029850746268773, 0.3706467661691542070, 0.3718905472636815923, 0.3731343283582089776, 0.3743781094527363074, 0.3756218905472636926, 0.3768656716417910224, 0.3781094527363184077, 0.3793532338308457930, 0.3805970149253731227, 0.3818407960199005080, 0.3830845771144278378, 0.3843283582089552231, 0.3855721393034826083, 0.3868159203980099381, 0.3880597014925373234, 0.3893034825870646531, 0.3905472636815920384, 0.3917910447761194237, 0.3930348258706467535, 0.3942786069651741387, 0.3955223880597014685, 0.3967661691542288538, 0.3980099502487562391, 0.3992537313432835688, 0.4004975124378109541, 0.4017412935323382839, 0.4029850746268656692, 0.4042288557213930544, 0.4054726368159203842, 0.4067164179104477695, 0.4079601990049750992, 0.4092039800995024845, 0.4104477611940298698, 0.4116915422885571996, 0.4129353233830845848, 0.4141791044776119146, 0.4154228855721392999, 0.4166666666666666852, 0.4179104477611940149, 0.4191542288557214002, 0.4203980099502487300, 0.4216417910447761153, 0.4228855721393035005, 0.4241293532338308303, 0.4253731343283582156, 0.4266169154228855454, 0.4278606965174129306, 0.4291044776119403159, 0.4303482587064676457, 0.4315920398009950310, 0.4328358208955223607, 0.4340796019900497460, 0.4353233830845771313, 0.4365671641791044610, 0.4378109452736318463, 0.4390547263681592316, 0.4402985074626865614, 0.4415422885572139466, 0.4427860696517412764, 0.4440298507462686617, 0.4452736318407960470, 0.4465174129353233767, 0.4477611940298507620, 0.4490049751243780918, 0.4502487562189054771, 0.4514925373134328623, 0.4527363184079601921, 0.4539800995024875774, 0.4552238805970149071, 0.4564676616915422924, 0.4577114427860696777, 0.4589552238805970075, 0.4601990049751243927, 0.4614427860696517225, 0.4626865671641791078, 0.4639303482587064931, 0.4651741293532338228, 0.4664179104477612081, 0.4676616915422885379, 0.4689054726368159232, 0.4701492537313433084, 0.4713930348258706382, 0.4726368159203980235, 0.4738805970149253532, 0.4751243781094527385, 0.4763681592039801238, 0.4776119402985074536, 0.4788557213930348389, 0.4800995024875621686, 0.4813432835820895539, 0.4825870646766169392, 0.4838308457711442689, 0.4850746268656716542, 0.4863184079601989840, 0.4875621890547263693, 0.4888059701492537545, 0.4900497512437810843, 0.4912935323383084696, 0.4925373134328357994, 0.4937810945273631846, 0.4950248756218905699, 0.4962686567164178997, 0.4975124378109452850, 0.4987562189054726147, 0.5000000000000000000, 0.5012437810945273853, 0.5024875621890547706, 0.5037313432835820448, 0.5049751243781094301, 0.5062189054726368154, 0.5074626865671642006, 0.5087064676616915859, 0.5099502487562188602, 0.5111940298507462455, 0.5124378109452736307, 0.5136815920398010160, 0.5149253731343284013, 0.5161691542288556755, 0.5174129353233830608, 0.5186567164179104461, 0.5199004975124378314, 0.5211442786069652167, 0.5223880597014924909, 0.5236318407960198762, 0.5248756218905472615, 0.5261194029850746468, 0.5273631840796020320, 0.5286069651741293063, 0.5298507462686566916, 0.5310945273631840768, 0.5323383084577114621, 0.5335820895522388474, 0.5348258706467661217, 0.5360696517412935069, 0.5373134328358208922, 0.5385572139303482775, 0.5398009950248756628, 0.5410447761194029370, 0.5422885572139303223, 0.5435323383084577076, 0.5447761194029850929, 0.5460199004975124781, 0.5472636815920397524, 0.5485074626865671377, 0.5497512437810945229, 0.5509950248756219082, 0.5522388059701492935, 0.5534825870646765678, 0.5547263681592039530, 0.5559701492537313383, 0.5572139303482587236, 0.5584577114427861089, 0.5597014925373133831, 0.5609452736318407684, 0.5621890547263681537, 0.5634328358208955390, 0.5646766169154229242, 0.5659203980099501985, 0.5671641791044775838, 0.5684079601990049690, 0.5696517412935323543, 0.5708955223880597396, 0.5721393034825870139, 0.5733830845771143991, 0.5746268656716417844, 0.5758706467661691697, 0.5771144278606965550, 0.5783582089552238292, 0.5796019900497512145, 0.5808457711442785998, 0.5820895522388059851, 0.5833333333333333703, 0.5845771144278606446, 0.5858208955223880299, 0.5870646766169154152, 0.5883084577114428004, 0.5895522388059701857, 0.5907960199004974600, 0.5920398009950248452, 0.5932835820895522305, 0.5945273631840796158, 0.5957711442786070011, 0.5970149253731342753, 0.5982587064676616606, 0.5995024875621890459, 0.6007462686567164312, 0.6019900497512438164, 0.6032338308457710907, 0.6044776119402984760, 0.6057213930348258613, 0.6069651741293532465, 0.6082089552238806318, 0.6094527363184079061, 0.6106965174129352913, 0.6119402985074626766, 0.6131840796019900619, 0.6144278606965174472, 0.6156716417910447214, 0.6169154228855721067, 0.6181592039800994920, 0.6194029850746268773, 0.6206467661691542625, 0.6218905472636815368, 0.6231343283582089221, 0.6243781094527363074, 0.6256218905472636926, 0.6268656716417910779, 0.6281094527363184632, 0.6293532338308457375, 0.6305970149253731227, 0.6318407960199005080, 0.6330845771144278933, 0.6343283582089552786, 0.6355721393034825528, 0.6368159203980099381, 0.6380597014925373234, 0.6393034825870647087, 0.6405472636815920939, 0.6417910447761193682, 0.6430348258706467535, 0.6442786069651741387, 0.6455223880597015240, 0.6467661691542289093, 0.6480099502487561836, 0.6492537313432835688, 0.6504975124378109541, 0.6517412935323383394, 0.6529850746268657247, 0.6542288557213929989, 0.6554726368159203842, 0.6567164179104477695, 0.6579601990049751548, 0.6592039800995025400, 0.6604477611940298143, 0.6616915422885571996, 0.6629353233830845848, 0.6641791044776119701, 0.6654228855721393554, 0.6666666666666666297, 0.6679104477611940149, 0.6691542288557214002, 0.6703980099502487855, 0.6716417910447761708, 0.6728855721393034450, 0.6741293532338308303, 0.6753731343283582156, 0.6766169154228856009, 0.6778606965174129861, 0.6791044776119402604, 0.6803482587064676457, 0.6815920398009950310, 0.6828358208955224162, 0.6840796019900498015, 0.6853233830845770758, 0.6865671641791044610, 0.6878109452736318463, 0.6890547263681592316, 0.6902985074626866169, 0.6915422885572138911, 0.6927860696517412764, 0.6940298507462686617, 0.6952736318407960470, 0.6965174129353234322, 0.6977611940298507065, 0.6990049751243780918, 0.7002487562189054771, 0.7014925373134328623, 0.7027363184079602476, 0.7039800995024875219, 0.7052238805970149071, 0.7064676616915422924, 0.7077114427860696777, 0.7089552238805970630, 0.7101990049751243372, 0.7114427860696517225, 0.7126865671641791078, 0.7139303482587064931, 0.7151741293532338783, 0.7164179104477611526, 0.7176616915422885379, 0.7189054726368159232, 0.7201492537313433084, 0.7213930348258706937, 0.7226368159203979680, 0.7238805970149253532, 0.7251243781094527385, 0.7263681592039801238, 0.7276119402985075091, 0.7288557213930347833, 0.7300995024875621686, 0.7313432835820895539, 0.7325870646766169392, 0.7338308457711443245, 0.7350746268656715987, 0.7363184079601989840, 0.7375621890547263693, 0.7388059701492537545, 0.7400497512437811398, 0.7412935323383084141, 0.7425373134328357994, 0.7437810945273631846, 0.7450248756218905699, 0.7462686567164179552, 0.7475124378109452294, 0.7487562189054726147, 0.7500000000000000000, 0.7512437810945273853, 0.7524875621890547706, 0.7537313432835820448, 0.7549751243781094301, 0.7562189054726368154, 0.7574626865671642006, 0.7587064676616915859, 0.7599502487562188602, 0.7611940298507462455, 0.7624378109452736307, 0.7636815920398010160, 0.7649253731343284013, 0.7661691542288556755, 0.7674129353233830608, 0.7686567164179104461, 0.7699004975124378314, 0.7711442786069652167, 0.7723880597014924909, 0.7736318407960198762, 0.7748756218905472615, 0.7761194029850746468, 0.7773631840796020320, 0.7786069651741293063, 0.7798507462686566916, 0.7810945273631840768, 0.7823383084577114621, 0.7835820895522388474, 0.7848258706467661217, 0.7860696517412935069, 0.7873134328358208922, 0.7885572139303482775, 0.7898009950248756628, 0.7910447761194029370, 0.7922885572139303223, 0.7935323383084577076, 0.7947761194029850929, 0.7960199004975124781, 0.7972636815920397524, 0.7985074626865671377, 0.7997512437810945229, 0.8009950248756219082, 0.8022388059701492935, 0.8034825870646765678, 0.8047263681592039530, 0.8059701492537313383, 0.8072139303482587236, 0.8084577114427861089, 0.8097014925373133831, 0.8109452736318407684, 0.8121890547263681537, 0.8134328358208955390, 0.8146766169154229242, 0.8159203980099501985, 0.8171641791044775838, 0.8184079601990049690, 0.8196517412935323543, 0.8208955223880597396, 0.8221393034825870139, 0.8233830845771143991, 0.8246268656716417844, 0.8258706467661691697, 0.8271144278606965550, 0.8283582089552238292, 0.8296019900497512145, 0.8308457711442785998, 0.8320895522388059851, 0.8333333333333333703, 0.8345771144278606446, 0.8358208955223880299, 0.8370646766169154152, 0.8383084577114428004, 0.8395522388059701857, 0.8407960199004974600, 0.8420398009950248452, 0.8432835820895522305, 0.8445273631840796158, 0.8457711442786070011, 0.8470149253731342753, 0.8482587064676616606, 0.8495024875621890459, 0.8507462686567164312, 0.8519900497512438164, 0.8532338308457710907, 0.8544776119402984760, 0.8557213930348258613, 0.8569651741293532465, 0.8582089552238806318, 0.8594527363184079061, 0.8606965174129352913, 0.8619402985074626766, 0.8631840796019900619, 0.8644278606965174472, 0.8656716417910447214, 0.8669154228855721067, 0.8681592039800994920, 0.8694029850746268773, 0.8706467661691542625, 0.8718905472636815368, 0.8731343283582089221, 0.8743781094527363074, 0.8756218905472636926, 0.8768656716417910779, 0.8781094527363184632, 0.8793532338308457375, 0.8805970149253731227, 0.8818407960199005080, 0.8830845771144278933, 0.8843283582089552786, 0.8855721393034825528, 0.8868159203980099381, 0.8880597014925373234, 0.8893034825870647087, 0.8905472636815920939, 0.8917910447761193682, 0.8930348258706467535, 0.8942786069651741387, 0.8955223880597015240, 0.8967661691542289093, 0.8980099502487561836, 0.8992537313432835688, 0.9004975124378109541, 0.9017412935323383394, 0.9029850746268657247, 0.9042288557213929989, 0.9054726368159203842, 0.9067164179104477695, 0.9079601990049751548, 0.9092039800995025400, 0.9104477611940298143, 0.9116915422885571996, 0.9129353233830845848, 0.9141791044776119701, 0.9154228855721393554, 0.9166666666666666297, 0.9179104477611940149, 0.9191542288557214002, 0.9203980099502487855, 0.9216417910447761708, 0.9228855721393034450, 0.9241293532338308303, 0.9253731343283582156, 0.9266169154228856009, 0.9278606965174129861, 0.9291044776119402604, 0.9303482587064676457, 0.9315920398009950310, 0.9328358208955224162, 0.9340796019900498015, 0.9353233830845770758, 0.9365671641791044610, 0.9378109452736318463, 0.9390547263681592316, 0.9402985074626866169, 0.9415422885572138911, 0.9427860696517412764, 0.9440298507462686617, 0.9452736318407960470, 0.9465174129353234322, 0.9477611940298507065, 0.9490049751243780918, 0.9502487562189054771, 0.9514925373134328623, 0.9527363184079602476, 0.9539800995024875219, 0.9552238805970149071, 0.9564676616915422924, 0.9577114427860696777, 0.9589552238805970630, 0.9601990049751243372, 0.9614427860696517225, 0.9626865671641791078, 0.9639303482587064931, 0.9651741293532338783, 0.9664179104477611526, 0.9676616915422885379, 0.9689054726368159232, 0.9701492537313433084, 0.9713930348258706937, 0.9726368159203979680, 0.9738805970149253532, 0.9751243781094527385, 0.9763681592039801238, 0.9776119402985075091, 0.9788557213930347833, 0.9800995024875621686, 0.9813432835820895539, 0.9825870646766169392, 0.9838308457711443245, 0.9850746268656715987, 0.9863184079601989840, 0.9875621890547263693, 0.9888059701492537545, 0.9900497512437811398, 0.9912935323383084141, 0.9925373134328357994, 0.9937810945273631846, 0.9950248756218905699 ),
 .UNSPECIFIED. ) 
 GEOMETRIC_REPRESENTATION_ITEM ( )  RATIONAL_B_SPLINE_SURFACE ( (
 ( 1.000000000000000000, 0.8660254037844387076, 1.000000000000000000, 0.8660254037844387076, 1.000000000000000000, 0.8660254037844387076, 1.000000000000000000, 0.8660254037844387076, 1.000000000000000000, 0.8660254037844387076, 1.000000000000000000, 0.8660254037844387076, 1.000000000000000000, 0.8660254037844387076, 1.000000000000000000, 0.8660254037844387076, 1.000000000000000000, 0.8660254037844387076, 1.000000000000000000, 0.8660254037844387076, 1.000000000000000000, 0.8660254037844387076, 1.000000000000000000, 0.8660254037844387076, 1.000000000000000000, 0.8660254037844387076, 1.000000000000000000, 0.8660254037844387076, 1.000000000000000000, 0.8660254037844387076, 1.000000000000000000, 0.8660254037844387076, 1.000000000000000000, 0.8660254037844387076, 1.000000000000000000, 0.8660254037844387076, 1.000000000000000000, 0.8660254037844387076, 1.000000000000000000, 0.8660254037844387076, 1.000000000000000000, 0.8660254037844387076, 1.000000000000000000, 0.8660254037844387076, 1.000000000000000000, 0.8660254037844387076, 1.000000000000000000, 0.8660254037844387076, 1.000000000000000000, 0.8660254037844387076, 1.000000000000000000, 0.8660254037844387076, 1.000000000000000000, 0.8660254037844387076, 1.000000000000000000, 0.8660254037844387076, 1.000000000000000000, 0.8660254037844387076, 1.000000000000000000, 0.8660254037844387076, 1.000000000000000000, 0.8660254037844387076, 1.000000000000000000, 0.8660254037844387076, 1.000000000000000000, 0.8660254037844387076, 1.000000000000000000, 0.8660254037844387076, 1.000000000000000000, 0.8660254037844387076, 1.000000000000000000, 0.8660254037844387076, 1.000000000000000000, 0.8660254037844387076, 1.000000000000000000, 0.8660254037844387076, 1.000000000000000000, 0.8660254037844387076, 1.000000000000000000, 0.8660254037844387076, 1.000000000000000000, 0.8660254037844387076, 1.000000000000000000, 0.8660254037844387076, 1.000000000000000000, 0.8660254037844387076, 1.000000000000000000, 0.8660254037844387076, 1.000000000000000000, 0.8660254037844387076, 1.000000000000000000, 0.8660254037844387076, 1.000000000000000000, 0.8660254037844387076, 1.000000000000000000, 0.8660254037844387076, 1.000000000000000000, 0.8660254037844387076, 1.000000000000000000, 0.8660254037844387076, 1.000000000000000000, 0.8660254037844387076, 1.000000000000000000, 0.8660254037844387076, 1.000000000000000000, 0.8660254037844387076, 1.000000000000000000, 0.8660254037844387076, 1.000000000000000000, 0.8660254037844387076, 1.000000000000000000, 0.8660254037844387076, 1.000000000000000000, 0.8660254037844387076, 1.000000000000000000, 0.8660254037844387076, 1.000000000000000000, 0.8660254037844387076, 1.000000000000000000, 0.8660254037844387076, 1.000000000000000000, 0.8660254037844387076, 1.000000000000000000, 0.8660254037844387076, 1.000000000000000000, 0.8660254037844387076, 1.000000000000000000, 0.8660254037844387076, 1.000000000000000000, 0.8660254037844387076, 1.000000000000000000, 0.8660254037844387076, 1.000000000000000000, 0.8660254037844387076, 1.000000000000000000, 0.8660254037844387076, 1.000000000000000000, 0.8660254037844387076, 1.000000000000000000, 0.8660254037844387076, 1.000000000000000000, 0.8660254037844387076, 1.000000000000000000, 0.8660254037844387076, 1.000000000000000000, 0.8660254037844387076, 1.000000000000000000, 0.8660254037844387076, 1.000000000000000000, 0.8660254037844387076, 1.000000000000000000, 0.8660254037844387076, 1.000000000000000000, 0.8660254037844387076, 1.000000000000000000, 0.8660254037844387076, 1.000000000000000000, 0.8660254037844387076, 1.000000000000000000, 0.8660254037844387076, 1.000000000000000000, 0.8660254037844387076, 1.000000000000000000, 0.8660254037844387076, 1.000000000000000000, 0.8660254037844387076, 1.000000000000000000, 0.8660254037844387076, 1.000000000000000000, 0.8660254037844387076, 1.000000000000000000, 0.8660254037844387076, 1.000000000000000000, 0.8660254037844387076, 1.000000000000000000, 0.8660254037844387076, 1.000000000000000000, 0.8660254037844387076, 1.000000000000000000, 0.8660254037844387076, 1.000000000000000000, 0.8660254037844387076, 1.000000000000000000, 0.8660254037844387076, 1.000000000000000000, 0.8660254037844387076, 1.000000000000000000, 0.8660254037844387076, 1.000000000000000000, 0.8660254037844387076, 1.000000000000000000, 0.8660254037844387076, 1.000000000000000000, 0.8660254037844387076, 1.000000000000000000, 0.8660254037844387076, 1.000000000000000000, 0.8660254037844387076, 1.000000000000000000, 0.8660254037844387076, 1.000000000000000000, 0.8660254037844387076, 1.000000000000000000, 0.8660254037844387076, 1.000000000000000000, 0.8660254037844387076, 1.000000000000000000, 0.8660254037844387076, 1.000000000000000000, 0.8660254037844387076, 1.000000000000000000, 0.8660254037844387076, 1.000000000000000000, 0.8660254037844387076, 1.000000000000000000, 0.8660254037844387076, 1.000000000000000000, 0.8660254037844387076, 1.000000000000000000, 0.8660254037844387076, 1.000000000000000000, 0.8660254037844387076, 1.000000000000000000, 0.8660254037844387076, 1.000000000000000000, 0.8660254037844387076, 1.000000000000000000, 0.8660254037844387076, 1.000000000000000000, 0.8660254037844387076, 1.000000000000000000, 0.8660254037844387076, 1.000000000000000000, 0.8660254037844387076, 1.000000000000000000, 0.8660254037844387076, 1.000000000000000000, 0.8660254037844387076, 1.000000000000000000, 0.8660254037844387076, 1.000000000000000000, 0.8660254037844387076, 1.000000000000000000, 0.8660254037844387076, 1.000000000000000000, 0.8660254037844387076, 1.000000000000000000, 0.8660254037844387076, 1.000000000000000000, 0.8660254037844387076, 1.000000000000000000, 0.8660254037844387076, 1.000000000000000000, 0.8660254037844387076, 1.000000000000000000, 0.8660254037844387076, 1.000000000000000000, 0.8660254037844387076, 1.000000000000000000, 0.8660254037844387076, 1.000000000000000000, 0.8660254037844387076, 1.000000000000000000, 0.8660254037844387076, 1.000000000000000000, 0.8660254037844387076, 1.000000000000000000, 0.8660254037844387076, 1.000000000000000000, 0.8660254037844387076, 1.000000000000000000, 0.8660254037844387076, 1.000000000000000000, 0.8660254037844387076, 1.000000000000000000, 0.8660254037844387076, 1.000000000000000000, 0.8660254037844387076, 1.000000000000000000, 0.8660254037844387076, 1.000000000000000000, 0.8660254037844387076, 1.000000000000000000, 0.8660254037844387076, 1.000000000000000000, 0.8660254037844387076, 1.000000000000000000, 0.8660254037844387076, 1.000000000000000000, 0.8660254037844387076, 1.000000000000000000, 0.8660254037844387076, 1.000000000000000000, 0.8660254037844387076, 1.000000000000000000, 0.8660254037844387076, 1.000000000000000000, 0.8660254037844387076, 1.000000000000000000, 0.8660254037844387076, 1.000000000000000000, 0.8660254037844387076, 1.000000000000000000, 0.8660254037844387076, 1.000000000000000000, 0.8660254037844387076, 1.000000000000000000, 0.8660254037844387076, 1.000000000000000000, 0.8660254037844387076, 1.000000000000000000, 0.8660254037844387076, 1.000000000000000000, 0.8660254037844387076, 1.000000000000000000, 0.8660254037844387076, 1.000000000000000000, 0.8660254037844387076, 1.000000000000000000, 0.8660254037844387076, 1.000000000000000000, 0.8660254037844387076, 1.000000000000000000, 0.8660254037844387076, 1.000000000000000000, 0.8660254037844387076, 1.000000000000000000, 0.8660254037844387076, 1.000000000000000000, 0.8660254037844387076, 1.000000000000000000, 0.8660254037844387076, 1.000000000000000000, 0.8660254037844387076, 1.000000000000000000, 0.8660254037844387076, 1.000000000000000000, 0.8660254037844387076, 1.000000000000000000, 0.8660254037844387076, 1.000000000000000000, 0.8660254037844387076, 1.000000000000000000, 0.8660254037844387076, 1.000000000000000000, 0.8660254037844387076, 1.000000000000000000, 0.8660254037844387076, 1.000000000000000000, 0.8660254037844387076, 1.000000000000000000, 0.8660254037844387076, 1.000000000000000000, 0.8660254037844387076, 1.000000000000000000, 0.8660254037844387076, 1.000000000000000000, 0.8660254037844387076, 1.000000000000000000, 0.8660254037844387076, 1.000000000000000000, 0.8660254037844387076, 1.000000000000000000, 0.8660254037844387076, 1.000000000000000000, 0.8660254037844387076, 1.000000000000000000, 0.8660254037844387076, 1.000000000000000000, 0.8660254037844387076, 1.000000000000000000, 0.8660254037844387076, 1.000000000000000000, 0.8660254037844387076, 1.000000000000000000, 0.8660254037844387076, 1.000000000000000000, 0.8660254037844387076, 1.000000000000000000, 0.8660254037844387076, 1.000000000000000000, 0.8660254037844387076, 1.000000000000000000, 0.8660254037844387076, 1.000000000000000000, 0.8660254037844387076, 1.000000000000000000, 0.8660254037844387076, 1.000000000000000000, 0.8660254037844387076, 1.000000000000000000, 0.8660254037844387076, 1.000000000000000000, 0.8660254037844387076, 1.000000000000000000, 0.8660254037844387076, 1.000000000000000000, 0.8660254037844387076, 1.000000000000000000, 0.8660254037844387076, 1.000000000000000000, 0.8660254037844387076, 1.000000000000000000, 0.8660254037844387076, 1.000000000000000000, 0.8660254037844387076, 1.000000000000000000, 0.8660254037844387076, 1.000000000000000000, 0.8660254037844387076, 1.000000000000000000, 0.8660254037844387076, 1.000000000000000000, 0.8660254037844387076, 1.000000000000000000, 0.8660254037844387076, 1.000000000000000000, 0.8660254037844387076, 1.000000000000000000, 0.8660254037844387076, 1.000000000000000000, 0.8660254037844387076, 1.000000000000000000, 0.8660254037844387076, 1.000000000000000000, 0.8660254037844387076, 1.000000000000000000, 0.8660254037844387076, 1.000000000000000000, 0.8660254037844387076, 1.000000000000000000, 0.8660254037844387076, 1.000000000000000000, 0.8660254037844387076, 1.000000000000000000, 0.8660254037844387076, 1.000000000000000000, 0.8660254037844387076, 1.000000000000000000, 0.8660254037844387076, 1.000000000000000000, 0.8660254037844387076, 1.000000000000000000, 0.8660254037844387076, 1.000000000000000000, 0.8660254037844387076, 1.000000000000000000, 0.8660254037844387076, 1.000000000000000000, 0.8660254037844387076, 1.000000000000000000, 0.8660254037844387076, 1.000000000000000000, 0.8660254037844387076, 1.000000000000000000, 0.8660254037844387076, 1.000000000000000000, 0.8660254037844387076, 1.000000000000000000, 0.8660254037844387076, 1.000000000000000000, 0.8660254037844387076, 1.000000000000000000, 0.8660254037844387076, 1.000000000000000000, 0.8660254037844387076, 1.000000000000000000, 0.8660254037844387076, 1.000000000000000000, 0.8660254037844387076, 1.000000000000000000, 0.8660254037844387076, 1.000000000000000000, 0.8660254037844387076, 1.000000000000000000, 0.8660254037844387076, 1.000000000000000000, 0.8660254037844387076, 1.000000000000000000, 0.8660254037844387076, 1.000000000000000000, 0.8660254037844387076, 1.000000000000000000, 0.8660254037844387076, 1.000000000000000000, 0.8660254037844387076, 1.000000000000000000, 0.8660254037844387076, 1.000000000000000000, 0.8660254037844387076, 1.000000000000000000, 0.8660254037844387076, 1.000000000000000000, 0.8660254037844387076, 1.000000000000000000, 0.8660254037844387076, 1.000000000000000000, 0.8660254037844387076, 1.000000000000000000, 0.8660254037844387076, 1.000000000000000000, 0.8660254037844387076, 1.000000000000000000, 0.8660254037844387076, 1.000000000000000000, 0.8660254037844387076, 1.000000000000000000, 0.8660254037844387076, 1.000000000000000000, 0.8660254037844387076, 1.000000000000000000, 0.8660254037844387076, 1.000000000000000000, 0.8660254037844387076, 1.000000000000000000, 0.8660254037844387076, 1.000000000000000000, 0.8660254037844387076, 1.000000000000000000, 0.8660254037844387076, 1.000000000000000000, 0.8660254037844387076, 1.000000000000000000, 0.8660254037844387076, 1.000000000000000000, 0.8660254037844387076, 1.000000000000000000, 0.8660254037844387076, 1.000000000000000000, 0.8660254037844387076, 1.000000000000000000, 0.8660254037844387076, 1.000000000000000000, 0.8660254037844387076, 1.000000000000000000, 0.8660254037844387076, 1.000000000000000000, 0.8660254037844387076, 1.000000000000000000, 0.8660254037844387076, 1.000000000000000000, 0.8660254037844387076, 1.000000000000000000, 0.8660254037844387076, 1.000000000000000000, 0.8660254037844387076, 1.000000000000000000, 0.8660254037844387076, 1.000000000000000000, 0.8660254037844387076, 1.000000000000000000, 0.8660254037844387076, 1.000000000000000000, 0.8660254037844387076, 1.000000000000000000, 0.8660254037844387076, 1.000000000000000000, 0.8660254037844387076, 1.000000000000000000, 0.8660254037844387076, 1.000000000000000000, 0.8660254037844387076, 1.000000000000000000, 0.8660254037844387076, 1.000000000000000000, 0.8660254037844387076, 1.000000000000000000, 0.8660254037844387076, 1.000000000000000000, 0.8660254037844387076, 1.000000000000000000, 0.8660254037844387076, 1.000000000000000000, 0.8660254037844387076, 1.000000000000000000, 0.8660254037844387076, 1.000000000000000000, 0.8660254037844387076, 1.000000000000000000, 0.8660254037844387076, 1.000000000000000000, 0.8660254037844387076, 1.000000000000000000, 0.8660254037844387076, 1.000000000000000000, 0.8660254037844387076, 1.000000000000000000, 0.8660254037844387076, 1.000000000000000000, 0.8660254037844387076, 1.000000000000000000, 0.8660254037844387076, 1.000000000000000000, 0.8660254037844387076, 1.000000000000000000, 0.8660254037844387076, 1.000000000000000000, 0.8660254037844387076, 1.000000000000000000, 0.8660254037844387076, 1.000000000000000000, 0.8660254037844387076, 1.000000000000000000, 0.8660254037844387076, 1.000000000000000000, 0.8660254037844387076, 1.000000000000000000, 0.8660254037844387076, 1.000000000000000000, 0.8660254037844387076, 1.000000000000000000, 0.8660254037844387076, 1.000000000000000000, 0.8660254037844387076, 1.000000000000000000, 0.8660254037844387076, 1.000000000000000000, 0.8660254037844387076, 1.000000000000000000, 0.8660254037844387076, 1.000000000000000000, 0.8660254037844387076, 1.000000000000000000, 0.8660254037844387076, 1.000000000000000000, 0.8660254037844387076, 1.000000000000000000, 0.8660254037844387076, 1.000000000000000000, 0.8660254037844387076, 1.000000000000000000, 0.8660254037844387076, 1.000000000000000000, 0.8660254037844387076, 1.000000000000000000, 0.8660254037844387076, 1.000000000000000000, 0.8660254037844387076, 1.000000000000000000, 0.8660254037844387076, 1.000000000000000000, 0.8660254037844387076, 1.000000000000000000, 0.8660254037844387076, 1.000000000000000000, 0.8660254037844387076, 1.000000000000000000, 0.8660254037844387076, 1.000000000000000000, 0.8660254037844387076, 1.000000000000000000, 0.8660254037844387076, 1.000000000000000000, 0.8660254037844387076, 1.000000000000000000, 0.8660254037844387076, 1.000000000000000000, 0.8660254037844387076, 1.000000000000000000, 0.8660254037844387076, 1.000000000000000000, 0.8660254037844387076, 1.000000000000000000, 0.8660254037844387076, 1.000000000000000000, 0.8660254037844387076, 1.000000000000000000, 0.8660254037844387076, 1.000000000000000000, 0.8660254037844387076, 1.000000000000000000, 0.8660254037844387076, 1.000000000000000000, 0.8660254037844387076, 1.000000000000000000, 0.8660254037844387076, 1.000000000000000000, 0.8660254037844387076, 1.000000000000000000, 0.8660254037844387076, 1.000000000000000000, 0.8660254037844387076, 1.000000000000000000, 0.8660254037844387076, 1.000000000000000000, 0.8660254037844387076, 1.000000000000000000, 0.8660254037844387076, 1.000000000000000000, 0.8660254037844387076, 1.000000000000000000, 0.8660254037844387076, 1.000000000000000000, 0.8660254037844387076, 1.000000000000000000, 0.8660254037844387076, 1.000000000000000000, 0.8660254037844387076, 1.000000000000000000, 0.8660254037844387076, 1.000000000000000000, 0.8660254037844387076, 1.000000000000000000, 0.8660254037844387076, 1.000000000000000000, 0.8660254037844387076, 1.000000000000000000, 0.8660254037844387076, 1.000000000000000000, 0.8660254037844387076, 1.000000000000000000, 0.8660254037844387076, 1.000000000000000000, 0.8660254037844387076, 1.000000000000000000, 0.8660254037844387076, 1.000000000000000000, 0.8660254037844387076, 1.000000000000000000, 0.8660254037844387076, 1.000000000000000000, 0.8660254037844387076, 1.000000000000000000, 0.8660254037844387076, 1.000000000000000000, 0.8660254037844387076, 1.000000000000000000, 0.8660254037844387076, 1.000000000000000000, 0.8660254037844387076, 1.000000000000000000, 0.8660254037844387076, 1.000000000000000000, 0.8660254037844387076, 1.000000000000000000, 0.8660254037844387076, 1.000000000000000000, 0.8660254037844387076, 1.000000000000000000, 0.8660254037844387076, 1.000000000000000000, 0.8660254037844387076, 1.000000000000000000, 0.8660254037844387076, 1.000000000000000000, 0.8660254037844387076, 1.000000000000000000, 0.8660254037844387076, 1.000000000000000000, 0.8660254037844387076, 1.000000000000000000, 0.8660254037844387076, 1.000000000000000000, 0.8660254037844387076, 1.000000000000000000, 0.8660254037844387076, 1.000000000000000000, 0.8660254037844387076, 1.000000000000000000, 0.8660254037844387076, 1.000000000000000000, 0.8660254037844387076, 1.000000000000000000, 0.8660254037844387076, 1.000000000000000000, 0.8660254037844387076, 1.000000000000000000, 0.8660254037844387076, 1.000000000000000000, 0.8660254037844387076, 1.000000000000000000, 0.8660254037844387076, 1.000000000000000000, 0.8660254037844387076, 1.000000000000000000, 0.8660254037844387076, 1.000000000000000000, 0.8660254037844387076, 1.000000000000000000, 0.8660254037844387076, 1.000000000000000000, 0.8660254037844387076, 1.000000000000000000, 0.8660254037844387076, 1.000000000000000000, 0.8660254037844387076, 1.000000000000000000, 0.8660254037844387076, 1.000000000000000000, 0.8660254037844387076, 1.000000000000000000, 0.8660254037844387076, 1.000000000000000000, 0.8660254037844387076, 1.000000000000000000, 0.8660254037844387076, 1.000000000000000000, 0.8660254037844387076, 1.000000000000000000, 0.8660254037844387076, 1.000000000000000000, 0.8660254037844387076, 1.000000000000000000, 0.8660254037844387076, 1.000000000000000000, 0.8660254037844387076, 1.000000000000000000, 0.8660254037844387076, 1.000000000000000000, 0.8660254037844387076, 1.000000000000000000, 0.8660254037844387076, 1.000000000000000000, 0.8660254037844387076, 1.000000000000000000, 0.8660254037844387076, 1.000000000000000000, 0.8660254037844387076, 1.000000000000000000, 0.8660254037844387076, 1.000000000000000000, 0.8660254037844387076, 1.000000000000000000, 0.8660254037844387076, 1.000000000000000000, 0.8660254037844387076, 1.000000000000000000, 0.8660254037844387076, 1.000000000000000000, 0.8660254037844387076, 1.000000000000000000, 0.8660254037844387076, 1.000000000000000000, 0.8660254037844387076, 1.000000000000000000, 0.8660254037844387076, 1.000000000000000000, 0.8660254037844387076, 1.000000000000000000, 0.8660254037844387076, 1.000000000000000000, 0.8660254037844387076, 1.000000000000000000, 0.8660254037844387076, 1.000000000000000000, 0.8660254037844387076, 1.000000000000000000, 0.8660254037844387076, 1.000000000000000000, 0.8660254037844387076, 1.000000000000000000, 0.8660254037844387076, 1.000000000000000000, 0.8660254037844387076, 1.000000000000000000, 0.8660254037844387076, 1.000000000000000000, 0.8660254037844387076, 1.000000000000000000, 0.8660254037844387076, 1.000000000000000000, 0.8660254037844387076, 1.000000000000000000, 0.8660254037844387076, 1.000000000000000000, 0.8660254037844387076, 1.000000000000000000, 0.8660254037844387076, 1.000000000000000000, 0.8660254037844387076, 1.000000000000000000, 0.8660254037844387076, 1.000000000000000000, 0.8660254037844387076, 1.000000000000000000, 0.8660254037844387076, 1.000000000000000000, 0.8660254037844387076, 1.000000000000000000, 0.8660254037844387076, 1.000000000000000000, 0.8660254037844387076, 1.000000000000000000, 0.8660254037844387076, 1.000000000000000000, 0.8660254037844387076, 1.000000000000000000, 0.8660254037844387076, 1.000000000000000000, 0.8660254037844387076, 1.000000000000000000, 0.8660254037844387076, 1.000000000000000000, 0.8660254037844387076, 1.000000000000000000, 0.8660254037844387076, 1.000000000000000000, 0.8660254037844387076, 1.000000000000000000, 0.8660254037844387076, 1.000000000000000000, 0.8660254037844387076, 1.000000000000000000, 0.8660254037844387076, 1.000000000000000000, 0.8660254037844387076, 1.000000000000000000, 0.8660254037844387076, 1.000000000000000000, 0.8660254037844387076, 1.000000000000000000, 0.8660254037844387076, 1.000000000000000000, 0.8660254037844387076, 1.000000000000000000, 0.8660254037844387076, 1.000000000000000000, 0.8660254037844387076, 1.000000000000000000, 0.8660254037844387076, 1.000000000000000000, 0.8660254037844387076, 1.000000000000000000, 0.8660254037844387076, 1.000000000000000000, 0.8660254037844387076, 1.000000000000000000, 0.8660254037844387076, 1.000000000000000000, 0.8660254037844387076, 1.000000000000000000, 0.8660254037844387076, 1.000000000000000000, 0.8660254037844387076, 1.000000000000000000, 0.8660254037844387076, 1.000000000000000000, 0.8660254037844387076, 1.000000000000000000, 0.8660254037844387076, 1.000000000000000000, 0.8660254037844387076, 1.000000000000000000, 0.8660254037844387076, 1.000000000000000000, 0.8660254037844387076, 1.000000000000000000, 0.8660254037844387076, 1.000000000000000000, 0.8660254037844387076, 1.000000000000000000, 0.8660254037844387076, 1.000000000000000000, 0.8660254037844387076, 1.000000000000000000, 0.8660254037844387076, 1.000000000000000000, 0.8660254037844387076, 1.000000000000000000, 0.8660254037844387076, 1.000000000000000000, 0.8660254037844387076, 1.000000000000000000, 0.8660254037844387076, 1.000000000000000000, 0.8660254037844387076, 1.000000000000000000, 0.8660254037844387076, 1.000000000000000000, 0.8660254037844387076, 1.000000000000000000, 0.8660254037844387076, 1.000000000000000000, 0.8660254037844387076, 1.000000000000000000, 0.8660254037844387076, 1.000000000000000000, 0.8660254037844387076, 1.000000000000000000, 0.8660254037844387076, 1.000000000000000000, 0.8660254037844387076, 1.000000000000000000, 0.8660254037844387076, 1.000000000000000000, 0.8660254037844387076, 1.000000000000000000, 0.8660254037844387076, 1.000000000000000000, 0.8660254037844387076, 1.000000000000000000, 0.8660254037844387076, 1.000000000000000000, 0.8660254037844387076, 1.000000000000000000, 0.8660254037844387076, 1.000000000000000000, 0.8660254037844387076, 1.000000000000000000, 0.8660254037844387076, 1.000000000000000000, 0.8660254037844387076, 1.000000000000000000, 0.8660254037844387076, 1.000000000000000000, 0.8660254037844387076, 1.000000000000000000, 0.8660254037844387076, 1.000000000000000000, 0.8660254037844387076, 1.000000000000000000, 0.8660254037844387076, 1.000000000000000000, 0.8660254037844387076, 1.000000000000000000, 0.8660254037844387076, 1.000000000000000000, 0.8660254037844387076, 1.000000000000000000, 0.8660254037844387076, 1.000000000000000000, 0.8660254037844387076, 1.000000000000000000, 0.8660254037844387076, 1.000000000000000000, 0.8660254037844387076, 1.000000000000000000, 0.8660254037844387076, 1.000000000000000000, 0.8660254037844387076, 1.000000000000000000, 0.8660254037844387076, 1.000000000000000000, 0.8660254037844387076, 1.000000000000000000, 0.8660254037844387076, 1.000000000000000000, 0.8660254037844387076, 1.000000000000000000, 0.8660254037844387076, 1.000000000000000000, 0.8660254037844387076, 1.000000000000000000, 0.8660254037844387076, 1.000000000000000000, 0.8660254037844387076, 1.000000000000000000, 0.8660254037844387076, 1.000000000000000000, 0.8660254037844387076, 1.000000000000000000, 0.8660254037844387076, 1.000000000000000000, 0.8660254037844387076, 1.000000000000000000, 0.8660254037844387076, 1.000000000000000000, 0.8660254037844387076, 1.000000000000000000, 0.8660254037844387076, 1.000000000000000000, 0.8660254037844387076, 1.000000000000000000, 0.8660254037844387076, 1.000000000000000000, 0.8660254037844387076, 1.000000000000000000, 0.8660254037844387076, 1.000000000000000000, 0.8660254037844387076, 1.000000000000000000, 0.8660254037844387076, 1.000000000000000000, 0.8660254037844387076, 1.000000000000000000, 0.8660254037844387076, 1.000000000000000000, 0.8660254037844387076, 1.000000000000000000, 0.8660254037844387076, 1.000000000000000000, 0.8660254037844387076, 1.000000000000000000, 0.8660254037844387076, 1.000000000000000000, 0.8660254037844387076, 1.000000000000000000, 0.8660254037844387076, 1.000000000000000000, 0.8660254037844387076, 1.000000000000000000, 0.8660254037844387076, 1.000000000000000000, 0.8660254037844387076, 1.000000000000000000, 0.8660254037844387076, 1.000000000000000000, 0.8660254037844387076, 1.000000000000000000, 0.8660254037844387076, 1.000000000000000000, 0.8660254037844387076, 1.000000000000000000, 0.8660254037844387076, 1.000000000000000000, 0.8660254037844387076, 1.000000000000000000, 0.8660254037844387076, 1.000000000000000000, 0.8660254037844387076, 1.000000000000000000, 0.8660254037844387076, 1.000000000000000000, 0.8660254037844387076, 1.000000000000000000, 0.8660254037844387076, 1.000000000000000000, 0.8660254037844387076, 1.000000000000000000, 0.8660254037844387076, 1.000000000000000000, 0.8660254037844387076, 1.000000000000000000, 0.8660254037844387076, 1.000000000000000000, 0.8660254037844387076, 1.000000000000000000, 0.8660254037844387076, 1.000000000000000000, 0.8660254037844387076, 1.000000000000000000, 0.8660254037844387076, 1.000000000000000000, 0.8660254037844387076, 1.000000000000000000, 0.8660254037844387076, 1.000000000000000000, 0.8660254037844387076, 1.000000000000000000, 0.8660254037844387076, 1.000000000000000000, 0.8660254037844387076, 1.000000000000000000, 0.8660254037844387076, 1.000000000000000000, 0.8660254037844387076, 1.000000000000000000, 0.8660254037844387076, 1.000000000000000000, 0.8660254037844387076, 1.000000000000000000, 0.8660254037844387076, 1.000000000000000000, 0.8660254037844387076, 1.000000000000000000, 0.8660254037844387076, 1.000000000000000000, 0.8660254037844387076, 1.000000000000000000, 0.8660254037844387076, 1.000000000000000000, 0.8660254037844387076, 1.000000000000000000, 0.8660254037844387076, 1.000000000000000000, 0.8660254037844387076, 1.000000000000000000, 0.8660254037844387076, 1.000000000000000000, 0.8660254037844387076, 1.000000000000000000, 0.8660254037844387076, 1.000000000000000000, 0.8660254037844387076, 1.000000000000000000, 0.8660254037844387076, 1.000000000000000000, 0.8660254037844387076, 1.000000000000000000, 0.8660254037844387076, 1.000000000000000000, 0.8660254037844387076, 1.000000000000000000, 0.8660254037844387076, 1.000000000000000000, 0.8660254037844387076, 1.000000000000000000, 0.8660254037844387076, 1.000000000000000000, 0.8660254037844387076, 1.000000000000000000, 0.8660254037844387076, 1.000000000000000000, 0.8660254037844387076, 1.000000000000000000, 0.8660254037844387076, 1.000000000000000000, 0.8660254037844387076, 1.000000000000000000, 0.8660254037844387076, 1.000000000000000000, 0.8660254037844387076, 1.000000000000000000, 0.8660254037844387076, 1.000000000000000000, 0.8660254037844387076, 1.000000000000000000, 0.8660254037844387076, 1.000000000000000000, 0.8660254037844387076, 1.000000000000000000, 0.8660254037844387076, 1.000000000000000000, 0.8660254037844387076, 1.000000000000000000, 0.8660254037844387076, 1.000000000000000000, 0.8660254037844387076, 1.000000000000000000, 0.8660254037844387076, 1.000000000000000000, 0.8660254037844387076, 1.000000000000000000, 0.8660254037844387076, 1.000000000000000000, 0.8660254037844387076, 1.000000000000000000, 0.8660254037844387076, 1.000000000000000000, 0.8660254037844387076, 1.000000000000000000, 0.8660254037844387076, 1.000000000000000000, 0.8660254037844387076, 1.000000000000000000, 0.8660254037844387076, 1.000000000000000000, 0.8660254037844387076, 1.000000000000000000, 0.8660254037844387076, 1.000000000000000000, 0.8660254037844387076, 1.000000000000000000, 0.8660254037844387076, 1.000000000000000000, 0.8660254037844387076, 1.000000000000000000, 0.8660254037844387076, 1.000000000000000000, 0.8660254037844387076, 1.000000000000000000, 0.8660254037844387076, 1.000000000000000000, 0.8660254037844387076, 1.000000000000000000, 0.8660254037844387076, 1.000000000000000000, 0.8660254037844387076, 1.000000000000000000, 0.8660254037844387076, 1.000000000000000000, 0.8660254037844387076, 1.000000000000000000, 0.8660254037844387076, 1.000000000000000000, 0.8660254037844387076, 1.000000000000000000, 0.8660254037844387076, 1.000000000000000000, 0.8660254037844387076, 1.000000000000000000, 0.8660254037844387076, 1.000000000000000000, 0.8660254037844387076, 1.000000000000000000, 0.8660254037844387076, 1.000000000000000000, 0.8660254037844387076, 1.000000000000000000, 0.8660254037844387076, 1.000000000000000000, 0.8660254037844387076, 1.000000000000000000, 0.8660254037844387076, 1.000000000000000000, 0.8660254037844387076, 1.000000000000000000, 0.8660254037844387076, 1.000000000000000000, 0.8660254037844387076, 1.000000000000000000, 0.8660254037844387076, 1.000000000000000000, 0.8660254037844387076, 1.000000000000000000, 0.8660254037844387076, 1.000000000000000000, 0.8660254037844387076, 1.000000000000000000, 0.8660254037844387076, 1.000000000000000000, 0.8660254037844387076, 1.000000000000000000, 0.8660254037844387076, 1.000000000000000000, 0.8660254037844387076, 1.000000000000000000, 0.8660254037844387076, 1.000000000000000000, 0.8660254037844387076, 1.000000000000000000, 0.8660254037844387076, 1.000000000000000000, 0.8660254037844387076, 1.000000000000000000, 0.8660254037844387076, 1.000000000000000000, 0.8660254037844387076, 1.000000000000000000, 0.8660254037844387076, 1.000000000000000000, 0.8660254037844387076, 1.000000000000000000, 0.8660254037844387076, 1.000000000000000000, 0.8660254037844387076, 1.000000000000000000, 0.8660254037844387076, 1.000000000000000000, 0.8660254037844387076, 1.000000000000000000, 0.8660254037844387076, 1.000000000000000000, 0.8660254037844387076, 1.000000000000000000, 0.8660254037844387076, 1.000000000000000000, 0.8660254037844387076, 1.000000000000000000, 0.8660254037844387076, 1.000000000000000000, 0.8660254037844387076, 1.000000000000000000, 0.8660254037844387076, 1.000000000000000000, 0.8660254037844387076, 1.000000000000000000, 0.8660254037844387076, 1.000000000000000000, 0.8660254037844387076, 1.000000000000000000, 0.8660254037844387076, 1.000000000000000000, 0.8660254037844387076, 1.000000000000000000, 0.8660254037844387076, 1.000000000000000000, 0.8660254037844387076, 1.000000000000000000, 0.8660254037844387076, 1.000000000000000000, 0.8660254037844387076, 1.000000000000000000, 0.8660254037844387076, 1.000000000000000000, 0.8660254037844387076, 1.000000000000000000, 0.8660254037844387076, 1.000000000000000000, 0.8660254037844387076, 1.000000000000000000, 0.8660254037844387076, 1.000000000000000000, 0.8660254037844387076, 1.000000000000000000, 0.8660254037844387076, 1.000000000000000000, 0.8660254037844387076, 1.000000000000000000, 0.8660254037844387076, 1.000000000000000000, 0.8660254037844387076, 1.000000000000000000, 0.8660254037844387076, 1.000000000000000000, 0.8660254037844387076, 1.000000000000000000, 0.8660254037844387076, 1.000000000000000000, 0.8660254037844387076, 1.000000000000000000, 0.8660254037844387076, 1.000000000000000000, 0.8660254037844387076, 1.000000000000000000, 0.8660254037844387076, 1.000000000000000000, 0.8660254037844387076, 1.000000000000000000, 0.8660254037844387076, 1.000000000000000000, 0.8660254037844387076, 1.000000000000000000, 0.8660254037844387076, 1.000000000000000000, 0.8660254037844387076, 1.000000000000000000, 0.8660254037844387076, 1.000000000000000000, 0.8660254037844387076, 1.000000000000000000, 0.8660254037844387076, 1.000000000000000000, 0.8660254037844387076, 1.000000000000000000, 0.8660254037844387076, 1.000000000000000000, 0.8660254037844387076, 1.000000000000000000, 0.8660254037844387076, 1.000000000000000000, 0.8660254037844387076, 1.000000000000000000, 0.8660254037844387076, 1.000000000000000000, 0.8660254037844387076, 1.000000000000000000, 0.8660254037844387076, 1.000000000000000000, 0.8660254037844387076, 1.000000000000000000, 0.8660254037844387076, 1.000000000000000000, 0.8660254037844387076, 1.000000000000000000, 0.8660254037844387076, 1.000000000000000000, 0.8660254037844387076, 1.000000000000000000, 0.8660254037844387076, 1.000000000000000000, 0.8660254037844387076, 1.000000000000000000, 0.8660254037844387076, 1.000000000000000000, 0.8660254037844387076, 1.000000000000000000, 0.8660254037844387076, 1.000000000000000000, 0.8660254037844387076, 1.000000000000000000, 0.8660254037844387076, 1.000000000000000000, 0.8660254037844387076, 1.000000000000000000, 0.8660254037844387076, 1.000000000000000000, 0.8660254037844387076, 1.000000000000000000, 0.8660254037844387076, 1.000000000000000000, 0.8660254037844387076, 1.000000000000000000, 0.8660254037844387076, 1.000000000000000000, 0.8660254037844387076, 1.000000000000000000, 0.8660254037844387076, 1.000000000000000000, 0.8660254037844387076, 1.000000000000000000, 0.8660254037844387076, 1.000000000000000000, 0.8660254037844387076, 1.000000000000000000, 0.8660254037844387076, 1.000000000000000000, 0.8660254037844387076, 1.000000000000000000, 0.8660254037844387076, 1.000000000000000000, 0.8660254037844387076, 1.000000000000000000, 0.8660254037844387076, 1.000000000000000000, 0.8660254037844387076, 1.000000000000000000, 0.8660254037844387076, 1.000000000000000000, 0.8660254037844387076, 1.000000000000000000, 0.8660254037844387076, 1.000000000000000000, 0.8660254037844387076, 1.000000000000000000, 0.8660254037844387076, 1.000000000000000000, 0.8660254037844387076, 1.000000000000000000, 0.8660254037844387076, 1.000000000000000000, 0.8660254037844387076, 1.000000000000000000, 0.8660254037844387076, 1.000000000000000000, 0.8660254037844387076, 1.000000000000000000, 0.8660254037844387076, 1.000000000000000000, 0.8660254037844387076, 1.000000000000000000, 0.8660254037844387076, 1.000000000000000000, 0.8660254037844387076, 1.000000000000000000, 0.8660254037844387076, 1.000000000000000000, 0.8660254037844387076, 1.000000000000000000, 0.8660254037844387076, 1.000000000000000000, 0.8660254037844387076, 1.000000000000000000, 0.8660254037844387076, 1.000000000000000000, 0.8660254037844387076, 1.000000000000000000, 0.8660254037844387076, 1.000000000000000000, 0.8660254037844387076, 1.000000000000000000, 0.8660254037844387076, 1.000000000000000000, 0.8660254037844387076, 1.000000000000000000, 0.8660254037844387076, 1.000000000000000000, 0.8660254037844387076, 1.000000000000000000, 0.8660254037844387076, 1.000000000000000000, 0.8660254037844387076, 1.000000000000000000, 0.8660254037844387076, 1.000000000000000000, 0.8660254037844387076, 1.000000000000000000, 0.8660254037844387076, 1.000000000000000000, 0.8660254037844387076, 1.000000000000000000, 0.8660254037844387076, 1.000000000000000000, 0.8660254037844387076, 1.000000000000000000, 0.8660254037844387076, 1.000000000000000000, 0.8660254037844387076, 1.000000000000000000, 0.8660254037844387076, 1.000000000000000000, 0.8660254037844387076, 1.000000000000000000, 0.8660254037844387076, 1.000000000000000000, 0.8660254037844387076, 1.000000000000000000, 0.8660254037844387076, 1.000000000000000000, 0.8660254037844387076, 1.000000000000000000, 0.8660254037844387076, 1.000000000000000000, 0.8660254037844387076, 1.000000000000000000, 0.8660254037844387076, 1.000000000000000000, 0.8660254037844387076, 1.000000000000000000, 0.8660254037844387076, 1.000000000000000000, 0.8660254037844387076, 1.000000000000000000, 0.8660254037844387076, 1.000000000000000000, 0.8660254037844387076, 1.000000000000000000, 0.8660254037844387076, 1.000000000000000000, 0.8660254037844387076, 1.000000000000000000, 0.8660254037844387076, 1.000000000000000000, 0.8660254037844387076, 1.000000000000000000, 0.8660254037844387076, 1.000000000000000000, 0.8660254037844387076, 1.000000000000000000, 0.8660254037844387076, 1.000000000000000000),
 ( 1.000000000000000000, 0.8660254037844387076, 1.000000000000000000, 0.8660254037844387076, 1.000000000000000000, 0.8660254037844387076, 1.000000000000000000, 0.8660254037844387076, 1.000000000000000000, 0.8660254037844387076, 1.000000000000000000, 0.8660254037844387076, 1.000000000000000000, 0.8660254037844387076, 1.000000000000000000, 0.8660254037844387076, 1.000000000000000000, 0.8660254037844387076, 1.000000000000000000, 0.8660254037844387076, 1.000000000000000000, 0.8660254037844387076, 1.000000000000000000, 0.8660254037844387076, 1.000000000000000000, 0.8660254037844387076, 1.000000000000000000, 0.8660254037844387076, 1.000000000000000000, 0.8660254037844387076, 1.000000000000000000, 0.8660254037844387076, 1.000000000000000000, 0.8660254037844387076, 1.000000000000000000, 0.8660254037844387076, 1.000000000000000000, 0.8660254037844387076, 1.000000000000000000, 0.8660254037844387076, 1.000000000000000000, 0.8660254037844387076, 1.000000000000000000, 0.8660254037844387076, 1.000000000000000000, 0.8660254037844387076, 1.000000000000000000, 0.8660254037844387076, 1.000000000000000000, 0.8660254037844387076, 1.000000000000000000, 0.8660254037844387076, 1.000000000000000000, 0.8660254037844387076, 1.000000000000000000, 0.8660254037844387076, 1.000000000000000000, 0.8660254037844387076, 1.000000000000000000, 0.8660254037844387076, 1.000000000000000000, 0.8660254037844387076, 1.000000000000000000, 0.8660254037844387076, 1.000000000000000000, 0.8660254037844387076, 1.000000000000000000, 0.8660254037844387076, 1.000000000000000000, 0.8660254037844387076, 1.000000000000000000, 0.8660254037844387076, 1.000000000000000000, 0.8660254037844387076, 1.000000000000000000, 0.8660254037844387076, 1.000000000000000000, 0.8660254037844387076, 1.000000000000000000, 0.8660254037844387076, 1.000000000000000000, 0.8660254037844387076, 1.000000000000000000, 0.8660254037844387076, 1.000000000000000000, 0.8660254037844387076, 1.000000000000000000, 0.8660254037844387076, 1.000000000000000000, 0.8660254037844387076, 1.000000000000000000, 0.8660254037844387076, 1.000000000000000000, 0.8660254037844387076, 1.000000000000000000, 0.8660254037844387076, 1.000000000000000000, 0.8660254037844387076, 1.000000000000000000, 0.8660254037844387076, 1.000000000000000000, 0.8660254037844387076, 1.000000000000000000, 0.8660254037844387076, 1.000000000000000000, 0.8660254037844387076, 1.000000000000000000, 0.8660254037844387076, 1.000000000000000000, 0.8660254037844387076, 1.000000000000000000, 0.8660254037844387076, 1.000000000000000000, 0.8660254037844387076, 1.000000000000000000, 0.8660254037844387076, 1.000000000000000000, 0.8660254037844387076, 1.000000000000000000, 0.8660254037844387076, 1.000000000000000000, 0.8660254037844387076, 1.000000000000000000, 0.8660254037844387076, 1.000000000000000000, 0.8660254037844387076, 1.000000000000000000, 0.8660254037844387076, 1.000000000000000000, 0.8660254037844387076, 1.000000000000000000, 0.8660254037844387076, 1.000000000000000000, 0.8660254037844387076, 1.000000000000000000, 0.8660254037844387076, 1.000000000000000000, 0.8660254037844387076, 1.000000000000000000, 0.8660254037844387076, 1.000000000000000000, 0.8660254037844387076, 1.000000000000000000, 0.8660254037844387076, 1.000000000000000000, 0.8660254037844387076, 1.000000000000000000, 0.8660254037844387076, 1.000000000000000000, 0.8660254037844387076, 1.000000000000000000, 0.8660254037844387076, 1.000000000000000000, 0.8660254037844387076, 1.000000000000000000, 0.8660254037844387076, 1.000000000000000000, 0.8660254037844387076, 1.000000000000000000, 0.8660254037844387076, 1.000000000000000000, 0.8660254037844387076, 1.000000000000000000, 0.8660254037844387076, 1.000000000000000000, 0.8660254037844387076, 1.000000000000000000, 0.8660254037844387076, 1.000000000000000000, 0.8660254037844387076, 1.000000000000000000, 0.8660254037844387076, 1.000000000000000000, 0.8660254037844387076, 1.000000000000000000, 0.8660254037844387076, 1.000000000000000000, 0.8660254037844387076, 1.000000000000000000, 0.8660254037844387076, 1.000000000000000000, 0.8660254037844387076, 1.000000000000000000, 0.8660254037844387076, 1.000000000000000000, 0.8660254037844387076, 1.000000000000000000, 0.8660254037844387076, 1.000000000000000000, 0.8660254037844387076, 1.000000000000000000, 0.8660254037844387076, 1.000000000000000000, 0.8660254037844387076, 1.000000000000000000, 0.8660254037844387076, 1.000000000000000000, 0.8660254037844387076, 1.000000000000000000, 0.8660254037844387076, 1.000000000000000000, 0.8660254037844387076, 1.000000000000000000, 0.8660254037844387076, 1.000000000000000000, 0.8660254037844387076, 1.000000000000000000, 0.8660254037844387076, 1.000000000000000000, 0.8660254037844387076, 1.000000000000000000, 0.8660254037844387076, 1.000000000000000000, 0.8660254037844387076, 1.000000000000000000, 0.8660254037844387076, 1.000000000000000000, 0.8660254037844387076, 1.000000000000000000, 0.8660254037844387076, 1.000000000000000000, 0.8660254037844387076, 1.000000000000000000, 0.8660254037844387076, 1.000000000000000000, 0.8660254037844387076, 1.000000000000000000, 0.8660254037844387076, 1.000000000000000000, 0.8660254037844387076, 1.000000000000000000, 0.8660254037844387076, 1.000000000000000000, 0.8660254037844387076, 1.000000000000000000, 0.8660254037844387076, 1.000000000000000000, 0.8660254037844387076, 1.000000000000000000, 0.8660254037844387076, 1.000000000000000000, 0.8660254037844387076, 1.000000000000000000, 0.8660254037844387076, 1.000000000000000000, 0.8660254037844387076, 1.000000000000000000, 0.8660254037844387076, 1.000000000000000000, 0.8660254037844387076, 1.000000000000000000, 0.8660254037844387076, 1.000000000000000000, 0.8660254037844387076, 1.000000000000000000, 0.8660254037844387076, 1.000000000000000000, 0.8660254037844387076, 1.000000000000000000, 0.8660254037844387076, 1.000000000000000000, 0.8660254037844387076, 1.000000000000000000, 0.8660254037844387076, 1.000000000000000000, 0.8660254037844387076, 1.000000000000000000, 0.8660254037844387076, 1.000000000000000000, 0.8660254037844387076, 1.000000000000000000, 0.8660254037844387076, 1.000000000000000000, 0.8660254037844387076, 1.000000000000000000, 0.8660254037844387076, 1.000000000000000000, 0.8660254037844387076, 1.000000000000000000, 0.8660254037844387076, 1.000000000000000000, 0.8660254037844387076, 1.000000000000000000, 0.8660254037844387076, 1.000000000000000000, 0.8660254037844387076, 1.000000000000000000, 0.8660254037844387076, 1.000000000000000000, 0.8660254037844387076, 1.000000000000000000, 0.8660254037844387076, 1.000000000000000000, 0.8660254037844387076, 1.000000000000000000, 0.8660254037844387076, 1.000000000000000000, 0.8660254037844387076, 1.000000000000000000, 0.8660254037844387076, 1.000000000000000000, 0.8660254037844387076, 1.000000000000000000, 0.8660254037844387076, 1.000000000000000000, 0.8660254037844387076, 1.000000000000000000, 0.8660254037844387076, 1.000000000000000000, 0.8660254037844387076, 1.000000000000000000, 0.8660254037844387076, 1.000000000000000000, 0.8660254037844387076, 1.000000000000000000, 0.8660254037844387076, 1.000000000000000000, 0.8660254037844387076, 1.000000000000000000, 0.8660254037844387076, 1.000000000000000000, 0.8660254037844387076, 1.000000000000000000, 0.8660254037844387076, 1.000000000000000000, 0.8660254037844387076, 1.000000000000000000, 0.8660254037844387076, 1.000000000000000000, 0.8660254037844387076, 1.000000000000000000, 0.8660254037844387076, 1.000000000000000000, 0.8660254037844387076, 1.000000000000000000, 0.8660254037844387076, 1.000000000000000000, 0.8660254037844387076, 1.000000000000000000, 0.8660254037844387076, 1.000000000000000000, 0.8660254037844387076, 1.000000000000000000, 0.8660254037844387076, 1.000000000000000000, 0.8660254037844387076, 1.000000000000000000, 0.8660254037844387076, 1.000000000000000000, 0.8660254037844387076, 1.000000000000000000, 0.8660254037844387076, 1.000000000000000000, 0.8660254037844387076, 1.000000000000000000, 0.8660254037844387076, 1.000000000000000000, 0.8660254037844387076, 1.000000000000000000, 0.8660254037844387076, 1.000000000000000000, 0.8660254037844387076, 1.000000000000000000, 0.8660254037844387076, 1.000000000000000000, 0.8660254037844387076, 1.000000000000000000, 0.8660254037844387076, 1.000000000000000000, 0.8660254037844387076, 1.000000000000000000, 0.8660254037844387076, 1.000000000000000000, 0.8660254037844387076, 1.000000000000000000, 0.8660254037844387076, 1.000000000000000000, 0.8660254037844387076, 1.000000000000000000, 0.8660254037844387076, 1.000000000000000000, 0.8660254037844387076, 1.000000000000000000, 0.8660254037844387076, 1.000000000000000000, 0.8660254037844387076, 1.000000000000000000, 0.8660254037844387076, 1.000000000000000000, 0.8660254037844387076, 1.000000000000000000, 0.8660254037844387076, 1.000000000000000000, 0.8660254037844387076, 1.000000000000000000, 0.8660254037844387076, 1.000000000000000000, 0.8660254037844387076, 1.000000000000000000, 0.8660254037844387076, 1.000000000000000000, 0.8660254037844387076, 1.000000000000000000, 0.8660254037844387076, 1.000000000000000000, 0.8660254037844387076, 1.000000000000000000, 0.8660254037844387076, 1.000000000000000000, 0.8660254037844387076, 1.000000000000000000, 0.8660254037844387076, 1.000000000000000000, 0.8660254037844387076, 1.000000000000000000, 0.8660254037844387076, 1.000000000000000000, 0.8660254037844387076, 1.000000000000000000, 0.8660254037844387076, 1.000000000000000000, 0.8660254037844387076, 1.000000000000000000, 0.8660254037844387076, 1.000000000000000000, 0.8660254037844387076, 1.000000000000000000, 0.8660254037844387076, 1.000000000000000000, 0.8660254037844387076, 1.000000000000000000, 0.8660254037844387076, 1.000000000000000000, 0.8660254037844387076, 1.000000000000000000, 0.8660254037844387076, 1.000000000000000000, 0.8660254037844387076, 1.000000000000000000, 0.8660254037844387076, 1.000000000000000000, 0.8660254037844387076, 1.000000000000000000, 0.8660254037844387076, 1.000000000000000000, 0.8660254037844387076, 1.000000000000000000, 0.8660254037844387076, 1.000000000000000000, 0.8660254037844387076, 1.000000000000000000, 0.8660254037844387076, 1.000000000000000000, 0.8660254037844387076, 1.000000000000000000, 0.8660254037844387076, 1.000000000000000000, 0.8660254037844387076, 1.000000000000000000, 0.8660254037844387076, 1.000000000000000000, 0.8660254037844387076, 1.000000000000000000, 0.8660254037844387076, 1.000000000000000000, 0.8660254037844387076, 1.000000000000000000, 0.8660254037844387076, 1.000000000000000000, 0.8660254037844387076, 1.000000000000000000, 0.8660254037844387076, 1.000000000000000000, 0.8660254037844387076, 1.000000000000000000, 0.8660254037844387076, 1.000000000000000000, 0.8660254037844387076, 1.000000000000000000, 0.8660254037844387076, 1.000000000000000000, 0.8660254037844387076, 1.000000000000000000, 0.8660254037844387076, 1.000000000000000000, 0.8660254037844387076, 1.000000000000000000, 0.8660254037844387076, 1.000000000000000000, 0.8660254037844387076, 1.000000000000000000, 0.8660254037844387076, 1.000000000000000000, 0.8660254037844387076, 1.000000000000000000, 0.8660254037844387076, 1.000000000000000000, 0.8660254037844387076, 1.000000000000000000, 0.8660254037844387076, 1.000000000000000000, 0.8660254037844387076, 1.000000000000000000, 0.8660254037844387076, 1.000000000000000000, 0.8660254037844387076, 1.000000000000000000, 0.8660254037844387076, 1.000000000000000000, 0.8660254037844387076, 1.000000000000000000, 0.8660254037844387076, 1.000000000000000000, 0.8660254037844387076, 1.000000000000000000, 0.8660254037844387076, 1.000000000000000000, 0.8660254037844387076, 1.000000000000000000, 0.8660254037844387076, 1.000000000000000000, 0.8660254037844387076, 1.000000000000000000, 0.8660254037844387076, 1.000000000000000000, 0.8660254037844387076, 1.000000000000000000, 0.8660254037844387076, 1.000000000000000000, 0.8660254037844387076, 1.000000000000000000, 0.8660254037844387076, 1.000000000000000000, 0.8660254037844387076, 1.000000000000000000, 0.8660254037844387076, 1.000000000000000000, 0.8660254037844387076, 1.000000000000000000, 0.8660254037844387076, 1.000000000000000000, 0.8660254037844387076, 1.000000000000000000, 0.8660254037844387076, 1.000000000000000000, 0.8660254037844387076, 1.000000000000000000, 0.8660254037844387076, 1.000000000000000000, 0.8660254037844387076, 1.000000000000000000, 0.8660254037844387076, 1.000000000000000000, 0.8660254037844387076, 1.000000000000000000, 0.8660254037844387076, 1.000000000000000000, 0.8660254037844387076, 1.000000000000000000, 0.8660254037844387076, 1.000000000000000000, 0.8660254037844387076, 1.000000000000000000, 0.8660254037844387076, 1.000000000000000000, 0.8660254037844387076, 1.000000000000000000, 0.8660254037844387076, 1.000000000000000000, 0.8660254037844387076, 1.000000000000000000, 0.8660254037844387076, 1.000000000000000000, 0.8660254037844387076, 1.000000000000000000, 0.8660254037844387076, 1.000000000000000000, 0.8660254037844387076, 1.000000000000000000, 0.8660254037844387076, 1.000000000000000000, 0.8660254037844387076, 1.000000000000000000, 0.8660254037844387076, 1.000000000000000000, 0.8660254037844387076, 1.000000000000000000, 0.8660254037844387076, 1.000000000000000000, 0.8660254037844387076, 1.000000000000000000, 0.8660254037844387076, 1.000000000000000000, 0.8660254037844387076, 1.000000000000000000, 0.8660254037844387076, 1.000000000000000000, 0.8660254037844387076, 1.000000000000000000, 0.8660254037844387076, 1.000000000000000000, 0.8660254037844387076, 1.000000000000000000, 0.8660254037844387076, 1.000000000000000000, 0.8660254037844387076, 1.000000000000000000, 0.8660254037844387076, 1.000000000000000000, 0.8660254037844387076, 1.000000000000000000, 0.8660254037844387076, 1.000000000000000000, 0.8660254037844387076, 1.000000000000000000, 0.8660254037844387076, 1.000000000000000000, 0.8660254037844387076, 1.000000000000000000, 0.8660254037844387076, 1.000000000000000000, 0.8660254037844387076, 1.000000000000000000, 0.8660254037844387076, 1.000000000000000000, 0.8660254037844387076, 1.000000000000000000, 0.8660254037844387076, 1.000000000000000000, 0.8660254037844387076, 1.000000000000000000, 0.8660254037844387076, 1.000000000000000000, 0.8660254037844387076, 1.000000000000000000, 0.8660254037844387076, 1.000000000000000000, 0.8660254037844387076, 1.000000000000000000, 0.8660254037844387076, 1.000000000000000000, 0.8660254037844387076, 1.000000000000000000, 0.8660254037844387076, 1.000000000000000000, 0.8660254037844387076, 1.000000000000000000, 0.8660254037844387076, 1.000000000000000000, 0.8660254037844387076, 1.000000000000000000, 0.8660254037844387076, 1.000000000000000000, 0.8660254037844387076, 1.000000000000000000, 0.8660254037844387076, 1.000000000000000000, 0.8660254037844387076, 1.000000000000000000, 0.8660254037844387076, 1.000000000000000000, 0.8660254037844387076, 1.000000000000000000, 0.8660254037844387076, 1.000000000000000000, 0.8660254037844387076, 1.000000000000000000, 0.8660254037844387076, 1.000000000000000000, 0.8660254037844387076, 1.000000000000000000, 0.8660254037844387076, 1.000000000000000000, 0.8660254037844387076, 1.000000000000000000, 0.8660254037844387076, 1.000000000000000000, 0.8660254037844387076, 1.000000000000000000, 0.8660254037844387076, 1.000000000000000000, 0.8660254037844387076, 1.000000000000000000, 0.8660254037844387076, 1.000000000000000000, 0.8660254037844387076, 1.000000000000000000, 0.8660254037844387076, 1.000000000000000000, 0.8660254037844387076, 1.000000000000000000, 0.8660254037844387076, 1.000000000000000000, 0.8660254037844387076, 1.000000000000000000, 0.8660254037844387076, 1.000000000000000000, 0.8660254037844387076, 1.000000000000000000, 0.8660254037844387076, 1.000000000000000000, 0.8660254037844387076, 1.000000000000000000, 0.8660254037844387076, 1.000000000000000000, 0.8660254037844387076, 1.000000000000000000, 0.8660254037844387076, 1.000000000000000000, 0.8660254037844387076, 1.000000000000000000, 0.8660254037844387076, 1.000000000000000000, 0.8660254037844387076, 1.000000000000000000, 0.8660254037844387076, 1.000000000000000000, 0.8660254037844387076, 1.000000000000000000, 0.8660254037844387076, 1.000000000000000000, 0.8660254037844387076, 1.000000000000000000, 0.8660254037844387076, 1.000000000000000000, 0.8660254037844387076, 1.000000000000000000, 0.8660254037844387076, 1.000000000000000000, 0.8660254037844387076, 1.000000000000000000, 0.8660254037844387076, 1.000000000000000000, 0.8660254037844387076, 1.000000000000000000, 0.8660254037844387076, 1.000000000000000000, 0.8660254037844387076, 1.000000000000000000, 0.8660254037844387076, 1.000000000000000000, 0.8660254037844387076, 1.000000000000000000, 0.8660254037844387076, 1.000000000000000000, 0.8660254037844387076, 1.000000000000000000, 0.8660254037844387076, 1.000000000000000000, 0.8660254037844387076, 1.000000000000000000, 0.8660254037844387076, 1.000000000000000000, 0.8660254037844387076, 1.000000000000000000, 0.8660254037844387076, 1.000000000000000000, 0.8660254037844387076, 1.000000000000000000, 0.8660254037844387076, 1.000000000000000000, 0.8660254037844387076, 1.000000000000000000, 0.8660254037844387076, 1.000000000000000000, 0.8660254037844387076, 1.000000000000000000, 0.8660254037844387076, 1.000000000000000000, 0.8660254037844387076, 1.000000000000000000, 0.8660254037844387076, 1.000000000000000000, 0.8660254037844387076, 1.000000000000000000, 0.8660254037844387076, 1.000000000000000000, 0.8660254037844387076, 1.000000000000000000, 0.8660254037844387076, 1.000000000000000000, 0.8660254037844387076, 1.000000000000000000, 0.8660254037844387076, 1.000000000000000000, 0.8660254037844387076, 1.000000000000000000, 0.8660254037844387076, 1.000000000000000000, 0.8660254037844387076, 1.000000000000000000, 0.8660254037844387076, 1.000000000000000000, 0.8660254037844387076, 1.000000000000000000, 0.8660254037844387076, 1.000000000000000000, 0.8660254037844387076, 1.000000000000000000, 0.8660254037844387076, 1.000000000000000000, 0.8660254037844387076, 1.000000000000000000, 0.8660254037844387076, 1.000000000000000000, 0.8660254037844387076, 1.000000000000000000, 0.8660254037844387076, 1.000000000000000000, 0.8660254037844387076, 1.000000000000000000, 0.8660254037844387076, 1.000000000000000000, 0.8660254037844387076, 1.000000000000000000, 0.8660254037844387076, 1.000000000000000000, 0.8660254037844387076, 1.000000000000000000, 0.8660254037844387076, 1.000000000000000000, 0.8660254037844387076, 1.000000000000000000, 0.8660254037844387076, 1.000000000000000000, 0.8660254037844387076, 1.000000000000000000, 0.8660254037844387076, 1.000000000000000000, 0.8660254037844387076, 1.000000000000000000, 0.8660254037844387076, 1.000000000000000000, 0.8660254037844387076, 1.000000000000000000, 0.8660254037844387076, 1.000000000000000000, 0.8660254037844387076, 1.000000000000000000, 0.8660254037844387076, 1.000000000000000000, 0.8660254037844387076, 1.000000000000000000, 0.8660254037844387076, 1.000000000000000000, 0.8660254037844387076, 1.000000000000000000, 0.8660254037844387076, 1.000000000000000000, 0.8660254037844387076, 1.000000000000000000, 0.8660254037844387076, 1.000000000000000000, 0.8660254037844387076, 1.000000000000000000, 0.8660254037844387076, 1.000000000000000000, 0.8660254037844387076, 1.000000000000000000, 0.8660254037844387076, 1.000000000000000000, 0.8660254037844387076, 1.000000000000000000, 0.8660254037844387076, 1.000000000000000000, 0.8660254037844387076, 1.000000000000000000, 0.8660254037844387076, 1.000000000000000000, 0.8660254037844387076, 1.000000000000000000, 0.8660254037844387076, 1.000000000000000000, 0.8660254037844387076, 1.000000000000000000, 0.8660254037844387076, 1.000000000000000000, 0.8660254037844387076, 1.000000000000000000, 0.8660254037844387076, 1.000000000000000000, 0.8660254037844387076, 1.000000000000000000, 0.8660254037844387076, 1.000000000000000000, 0.8660254037844387076, 1.000000000000000000, 0.8660254037844387076, 1.000000000000000000, 0.8660254037844387076, 1.000000000000000000, 0.8660254037844387076, 1.000000000000000000, 0.8660254037844387076, 1.000000000000000000, 0.8660254037844387076, 1.000000000000000000, 0.8660254037844387076, 1.000000000000000000, 0.8660254037844387076, 1.000000000000000000, 0.8660254037844387076, 1.000000000000000000, 0.8660254037844387076, 1.000000000000000000, 0.8660254037844387076, 1.000000000000000000, 0.8660254037844387076, 1.000000000000000000, 0.8660254037844387076, 1.000000000000000000, 0.8660254037844387076, 1.000000000000000000, 0.8660254037844387076, 1.000000000000000000, 0.8660254037844387076, 1.000000000000000000, 0.8660254037844387076, 1.000000000000000000, 0.8660254037844387076, 1.000000000000000000, 0.8660254037844387076, 1.000000000000000000, 0.8660254037844387076, 1.000000000000000000, 0.8660254037844387076, 1.000000000000000000, 0.8660254037844387076, 1.000000000000000000, 0.8660254037844387076, 1.000000000000000000, 0.8660254037844387076, 1.000000000000000000, 0.8660254037844387076, 1.000000000000000000, 0.8660254037844387076, 1.000000000000000000, 0.8660254037844387076, 1.000000000000000000, 0.8660254037844387076, 1.000000000000000000, 0.8660254037844387076, 1.000000000000000000, 0.8660254037844387076, 1.000000000000000000, 0.8660254037844387076, 1.000000000000000000, 0.8660254037844387076, 1.000000000000000000, 0.8660254037844387076, 1.000000000000000000, 0.8660254037844387076, 1.000000000000000000, 0.8660254037844387076, 1.000000000000000000, 0.8660254037844387076, 1.000000000000000000, 0.8660254037844387076, 1.000000000000000000, 0.8660254037844387076, 1.000000000000000000, 0.8660254037844387076, 1.000000000000000000, 0.8660254037844387076, 1.000000000000000000, 0.8660254037844387076, 1.000000000000000000, 0.8660254037844387076, 1.000000000000000000, 0.8660254037844387076, 1.000000000000000000, 0.8660254037844387076, 1.000000000000000000, 0.8660254037844387076, 1.000000000000000000, 0.8660254037844387076, 1.000000000000000000, 0.8660254037844387076, 1.000000000000000000, 0.8660254037844387076, 1.000000000000000000, 0.8660254037844387076, 1.000000000000000000, 0.8660254037844387076, 1.000000000000000000, 0.8660254037844387076, 1.000000000000000000, 0.8660254037844387076, 1.000000000000000000, 0.8660254037844387076, 1.000000000000000000, 0.8660254037844387076, 1.000000000000000000, 0.8660254037844387076, 1.000000000000000000, 0.8660254037844387076, 1.000000000000000000, 0.8660254037844387076, 1.000000000000000000, 0.8660254037844387076, 1.000000000000000000, 0.8660254037844387076, 1.000000000000000000, 0.8660254037844387076, 1.000000000000000000, 0.8660254037844387076, 1.000000000000000000, 0.8660254037844387076, 1.000000000000000000, 0.8660254037844387076, 1.000000000000000000, 0.8660254037844387076, 1.000000000000000000, 0.8660254037844387076, 1.000000000000000000, 0.8660254037844387076, 1.000000000000000000, 0.8660254037844387076, 1.000000000000000000, 0.8660254037844387076, 1.000000000000000000, 0.8660254037844387076, 1.000000000000000000, 0.8660254037844387076, 1.000000000000000000, 0.8660254037844387076, 1.000000000000000000, 0.8660254037844387076, 1.000000000000000000, 0.8660254037844387076, 1.000000000000000000, 0.8660254037844387076, 1.000000000000000000, 0.8660254037844387076, 1.000000000000000000, 0.8660254037844387076, 1.000000000000000000, 0.8660254037844387076, 1.000000000000000000, 0.8660254037844387076, 1.000000000000000000, 0.8660254037844387076, 1.000000000000000000, 0.8660254037844387076, 1.000000000000000000, 0.8660254037844387076, 1.000000000000000000, 0.8660254037844387076, 1.000000000000000000, 0.8660254037844387076, 1.000000000000000000, 0.8660254037844387076, 1.000000000000000000, 0.8660254037844387076, 1.000000000000000000, 0.8660254037844387076, 1.000000000000000000, 0.8660254037844387076, 1.000000000000000000, 0.8660254037844387076, 1.000000000000000000, 0.8660254037844387076, 1.000000000000000000, 0.8660254037844387076, 1.000000000000000000, 0.8660254037844387076, 1.000000000000000000, 0.8660254037844387076, 1.000000000000000000, 0.8660254037844387076, 1.000000000000000000, 0.8660254037844387076, 1.000000000000000000, 0.8660254037844387076, 1.000000000000000000, 0.8660254037844387076, 1.000000000000000000, 0.8660254037844387076, 1.000000000000000000, 0.8660254037844387076, 1.000000000000000000, 0.8660254037844387076, 1.000000000000000000, 0.8660254037844387076, 1.000000000000000000, 0.8660254037844387076, 1.000000000000000000, 0.8660254037844387076, 1.000000000000000000, 0.8660254037844387076, 1.000000000000000000, 0.8660254037844387076, 1.000000000000000000, 0.8660254037844387076, 1.000000000000000000, 0.8660254037844387076, 1.000000000000000000, 0.8660254037844387076, 1.000000000000000000, 0.8660254037844387076, 1.000000000000000000, 0.8660254037844387076, 1.000000000000000000, 0.8660254037844387076, 1.000000000000000000, 0.8660254037844387076, 1.000000000000000000, 0.8660254037844387076, 1.000000000000000000, 0.8660254037844387076, 1.000000000000000000, 0.8660254037844387076, 1.000000000000000000, 0.8660254037844387076, 1.000000000000000000, 0.8660254037844387076, 1.000000000000000000, 0.8660254037844387076, 1.000000000000000000, 0.8660254037844387076, 1.000000000000000000, 0.8660254037844387076, 1.000000000000000000, 0.8660254037844387076, 1.000000000000000000, 0.8660254037844387076, 1.000000000000000000, 0.8660254037844387076, 1.000000000000000000, 0.8660254037844387076, 1.000000000000000000, 0.8660254037844387076, 1.000000000000000000, 0.8660254037844387076, 1.000000000000000000, 0.8660254037844387076, 1.000000000000000000, 0.8660254037844387076, 1.000000000000000000, 0.8660254037844387076, 1.000000000000000000, 0.8660254037844387076, 1.000000000000000000, 0.8660254037844387076, 1.000000000000000000, 0.8660254037844387076, 1.000000000000000000, 0.8660254037844387076, 1.000000000000000000, 0.8660254037844387076, 1.000000000000000000, 0.8660254037844387076, 1.000000000000000000, 0.8660254037844387076, 1.000000000000000000, 0.8660254037844387076, 1.000000000000000000, 0.8660254037844387076, 1.000000000000000000, 0.8660254037844387076, 1.000000000000000000, 0.8660254037844387076, 1.000000000000000000, 0.8660254037844387076, 1.000000000000000000, 0.8660254037844387076, 1.000000000000000000, 0.8660254037844387076, 1.000000000000000000, 0.8660254037844387076, 1.000000000000000000, 0.8660254037844387076, 1.000000000000000000, 0.8660254037844387076, 1.000000000000000000, 0.8660254037844387076, 1.000000000000000000, 0.8660254037844387076, 1.000000000000000000, 0.8660254037844387076, 1.000000000000000000, 0.8660254037844387076, 1.000000000000000000, 0.8660254037844387076, 1.000000000000000000, 0.8660254037844387076, 1.000000000000000000, 0.8660254037844387076, 1.000000000000000000, 0.8660254037844387076, 1.000000000000000000, 0.8660254037844387076, 1.000000000000000000, 0.8660254037844387076, 1.000000000000000000, 0.8660254037844387076, 1.000000000000000000, 0.8660254037844387076, 1.000000000000000000, 0.8660254037844387076, 1.000000000000000000, 0.8660254037844387076, 1.000000000000000000, 0.8660254037844387076, 1.000000000000000000, 0.8660254037844387076, 1.000000000000000000, 0.8660254037844387076, 1.000000000000000000, 0.8660254037844387076, 1.000000000000000000, 0.8660254037844387076, 1.000000000000000000, 0.8660254037844387076, 1.000000000000000000, 0.8660254037844387076, 1.000000000000000000, 0.8660254037844387076, 1.000000000000000000, 0.8660254037844387076, 1.000000000000000000, 0.8660254037844387076, 1.000000000000000000, 0.8660254037844387076, 1.000000000000000000, 0.8660254037844387076, 1.000000000000000000, 0.8660254037844387076, 1.000000000000000000, 0.8660254037844387076, 1.000000000000000000, 0.8660254037844387076, 1.000000000000000000, 0.8660254037844387076, 1.000000000000000000, 0.8660254037844387076, 1.000000000000000000, 0.8660254037844387076, 1.000000000000000000, 0.8660254037844387076, 1.000000000000000000, 0.8660254037844387076, 1.000000000000000000, 0.8660254037844387076, 1.000000000000000000, 0.8660254037844387076, 1.000000000000000000, 0.8660254037844387076, 1.000000000000000000, 0.8660254037844387076, 1.000000000000000000, 0.8660254037844387076, 1.000000000000000000, 0.8660254037844387076, 1.000000000000000000, 0.8660254037844387076, 1.000000000000000000, 0.8660254037844387076, 1.000000000000000000, 0.8660254037844387076, 1.000000000000000000, 0.8660254037844387076, 1.000000000000000000, 0.8660254037844387076, 1.000000000000000000, 0.8660254037844387076, 1.000000000000000000, 0.8660254037844387076, 1.000000000000000000, 0.8660254037844387076, 1.000000000000000000, 0.8660254037844387076, 1.000000000000000000, 0.8660254037844387076, 1.000000000000000000, 0.8660254037844387076, 1.000000000000000000, 0.8660254037844387076, 1.000000000000000000, 0.8660254037844387076, 1.000000000000000000, 0.8660254037844387076, 1.000000000000000000, 0.8660254037844387076, 1.000000000000000000, 0.8660254037844387076, 1.000000000000000000, 0.8660254037844387076, 1.000000000000000000, 0.8660254037844387076, 1.000000000000000000, 0.8660254037844387076, 1.000000000000000000, 0.8660254037844387076, 1.000000000000000000, 0.8660254037844387076, 1.000000000000000000, 0.8660254037844387076, 1.000000000000000000, 0.8660254037844387076, 1.000000000000000000, 0.8660254037844387076, 1.000000000000000000, 0.8660254037844387076, 1.000000000000000000, 0.8660254037844387076, 1.000000000000000000, 0.8660254037844387076, 1.000000000000000000, 0.8660254037844387076, 1.000000000000000000, 0.8660254037844387076, 1.000000000000000000, 0.8660254037844387076, 1.000000000000000000, 0.8660254037844387076, 1.000000000000000000, 0.8660254037844387076, 1.000000000000000000, 0.8660254037844387076, 1.000000000000000000, 0.8660254037844387076, 1.000000000000000000, 0.8660254037844387076, 1.000000000000000000, 0.8660254037844387076, 1.000000000000000000, 0.8660254037844387076, 1.000000000000000000, 0.8660254037844387076, 1.000000000000000000, 0.8660254037844387076, 1.000000000000000000, 0.8660254037844387076, 1.000000000000000000, 0.8660254037844387076, 1.000000000000000000, 0.8660254037844387076, 1.000000000000000000, 0.8660254037844387076, 1.000000000000000000, 0.8660254037844387076, 1.000000000000000000, 0.8660254037844387076, 1.000000000000000000, 0.8660254037844387076, 1.000000000000000000, 0.8660254037844387076, 1.000000000000000000, 0.8660254037844387076, 1.000000000000000000, 0.8660254037844387076, 1.000000000000000000, 0.8660254037844387076, 1.000000000000000000, 0.8660254037844387076, 1.000000000000000000, 0.8660254037844387076, 1.000000000000000000, 0.8660254037844387076, 1.000000000000000000, 0.8660254037844387076, 1.000000000000000000, 0.8660254037844387076, 1.000000000000000000, 0.8660254037844387076, 1.000000000000000000, 0.8660254037844387076, 1.000000000000000000, 0.8660254037844387076, 1.000000000000000000, 0.8660254037844387076, 1.000000000000000000, 0.8660254037844387076, 1.000000000000000000, 0.8660254037844387076, 1.000000000000000000, 0.8660254037844387076, 1.000000000000000000, 0.8660254037844387076, 1.000000000000000000, 0.8660254037844387076, 1.000000000000000000, 0.8660254037844387076, 1.000000000000000000, 0.8660254037844387076, 1.000000000000000000, 0.8660254037844387076, 1.000000000000000000, 0.8660254037844387076, 1.000000000000000000, 0.8660254037844387076, 1.000000000000000000, 0.8660254037844387076, 1.000000000000000000, 0.8660254037844387076, 1.000000000000000000, 0.8660254037844387076, 1.000000000000000000, 0.8660254037844387076, 1.000000000000000000, 0.8660254037844387076, 1.000000000000000000, 0.8660254037844387076, 1.000000000000000000, 0.8660254037844387076, 1.000000000000000000, 0.8660254037844387076, 1.000000000000000000, 0.8660254037844387076, 1.000000000000000000, 0.8660254037844387076, 1.000000000000000000, 0.8660254037844387076, 1.000000000000000000, 0.8660254037844387076, 1.000000000000000000, 0.8660254037844387076, 1.000000000000000000, 0.8660254037844387076, 1.000000000000000000, 0.8660254037844387076, 1.000000000000000000, 0.8660254037844387076, 1.000000000000000000, 0.8660254037844387076, 1.000000000000000000, 0.8660254037844387076, 1.000000000000000000, 0.8660254037844387076, 1.000000000000000000, 0.8660254037844387076, 1.000000000000000000, 0.8660254037844387076, 1.000000000000000000, 0.8660254037844387076, 1.000000000000000000, 0.8660254037844387076, 1.000000000000000000, 0.8660254037844387076, 1.000000000000000000, 0.8660254037844387076, 1.000000000000000000, 0.8660254037844387076, 1.000000000000000000, 0.8660254037844387076, 1.000000000000000000, 0.8660254037844387076, 1.000000000000000000, 0.8660254037844387076, 1.000000000000000000, 0.8660254037844387076, 1.000000000000000000, 0.8660254037844387076, 1.000000000000000000, 0.8660254037844387076, 1.000000000000000000, 0.8660254037844387076, 1.000000000000000000, 0.8660254037844387076, 1.000000000000000000, 0.8660254037844387076, 1.000000000000000000, 0.8660254037844387076, 1.000000000000000000, 0.8660254037844387076, 1.000000000000000000, 0.8660254037844387076, 1.000000000000000000, 0.8660254037844387076, 1.000000000000000000, 0.8660254037844387076, 1.000000000000000000, 0.8660254037844387076, 1.000000000000000000, 0.8660254037844387076, 1.000000000000000000, 0.8660254037844387076, 1.000000000000000000, 0.8660254037844387076, 1.000000000000000000, 0.8660254037844387076, 1.000000000000000000, 0.8660254037844387076, 1.000000000000000000, 0.8660254037844387076, 1.000000000000000000, 0.8660254037844387076, 1.000000000000000000, 0.8660254037844387076, 1.000000000000000000, 0.8660254037844387076, 1.000000000000000000, 0.8660254037844387076, 1.000000000000000000, 0.8660254037844387076, 1.000000000000000000, 0.8660254037844387076, 1.000000000000000000, 0.8660254037844387076, 1.000000000000000000, 0.8660254037844387076, 1.000000000000000000, 0.8660254037844387076, 1.000000000000000000, 0.8660254037844387076, 1.000000000000000000, 0.8660254037844387076, 1.000000000000000000, 0.8660254037844387076, 1.000000000000000000, 0.8660254037844387076, 1.000000000000000000, 0.8660254037844387076, 1.000000000000000000, 0.8660254037844387076, 1.000000000000000000, 0.8660254037844387076, 1.000000000000000000, 0.8660254037844387076, 1.000000000000000000, 0.8660254037844387076, 1.000000000000000000, 0.8660254037844387076, 1.000000000000000000, 0.8660254037844387076, 1.000000000000000000, 0.8660254037844387076, 1.000000000000000000, 0.8660254037844387076, 1.000000000000000000, 0.8660254037844387076, 1.000000000000000000, 0.8660254037844387076, 1.000000000000000000, 0.8660254037844387076, 1.000000000000000000, 0.8660254037844387076, 1.000000000000000000, 0.8660254037844387076, 1.000000000000000000, 0.8660254037844387076, 1.000000000000000000, 0.8660254037844387076, 1.000000000000000000, 0.8660254037844387076, 1.000000000000000000, 0.8660254037844387076, 1.000000000000000000, 0.8660254037844387076, 1.000000000000000000, 0.8660254037844387076, 1.000000000000000000, 0.8660254037844387076, 1.000000000000000000, 0.8660254037844387076, 1.000000000000000000, 0.8660254037844387076, 1.000000000000000000, 0.8660254037844387076, 1.000000000000000000, 0.8660254037844387076, 1.000000000000000000, 0.8660254037844387076, 1.000000000000000000, 0.8660254037844387076, 1.000000000000000000, 0.8660254037844387076, 1.000000000000000000, 0.8660254037844387076, 1.000000000000000000, 0.8660254037844387076, 1.000000000000000000, 0.8660254037844387076, 1.000000000000000000, 0.8660254037844387076, 1.000000000000000000, 0.8660254037844387076, 1.000000000000000000, 0.8660254037844387076, 1.000000000000000000, 0.8660254037844387076, 1.000000000000000000, 0.8660254037844387076, 1.000000000000000000, 0.8660254037844387076, 1.000000000000000000, 0.8660254037844387076, 1.000000000000000000, 0.8660254037844387076, 1.000000000000000000, 0.8660254037844387076, 1.000000000000000000, 0.8660254037844387076, 1.000000000000000000, 0.8660254037844387076, 1.000000000000000000, 0.8660254037844387076, 1.000000000000000000, 0.8660254037844387076, 1.000000000000000000) ) ) 
 REPRESENTATION_ITEM ( '' )  SURFACE ( )  );
#22642 = CARTESIAN_POINT ( 'NONE',  ( 9.999999999999996447, -5.773502691896262640, -82.00000000409676204 ) ) ;
#22643 = DIRECTION ( 'NONE',  ( -0.000000000000000000, -0.000000000000000000, -1.000000000000000000 ) ) ;
#22644 = CARTESIAN_POINT ( 'NONE',  ( 5.405949406249992428, -9.363379034771808662, -43.59375000204837391 ) ) ;
#22645 = ORIENTED_EDGE ( 'NONE', *, *, #15617, .F. ) ;
#22646 = CARTESIAN_POINT ( 'NONE',  ( 10.00000000000000000, 5.773502691896255534, -18.37499999999997513 ) ) ;
#22647 = CARTESIAN_POINT ( 'NONE',  ( -4.999999999999996447, 8.660254037844387298, -154.5000000000000000 ) ) ;
#22648 = CARTESIAN_POINT ( 'NONE',  ( -10.00000000000000000, -5.773502691896251982, -12.00000000409676204 ) ) ;
#22649 = EDGE_CURVE ( 'NONE', #13797, #14989, #11133, .T. ) ;
#22650 = DIRECTION ( 'NONE',  ( -1.000000000000000000, 0.000000000000000000, 0.000000000000000000 ) ) ;
#22652 = ORIENTED_EDGE ( 'NONE', *, *, #28347, .T. ) ;
#22651 = CARTESIAN_POINT ( 'NONE',  ( -10.81189881249999729, 1.324075727343319199E-15, -125.2812500020483668 ) ) ;
#22653 = CARTESIAN_POINT ( 'NONE',  ( 9.999999999999998224, 0.000000000000000000, -21.49999999999996447 ) ) ;
#22654 = EDGE_LOOP ( 'NONE', ( #7140, #8746 ) ) ;
#22655 = CARTESIAN_POINT ( 'NONE',  ( -5.405949406249996869, 9.363379034771805109, -56.53125000204836681 ) ) ;
#22656 = SECURITY_CLASSIFICATION_LEVEL ( 'unclassified' ) ;
#22657 = CARTESIAN_POINT ( 'NONE',  ( 5.405949406249992428, -9.363379034771808662, -102.0937500020483810 ) ) ;
#22659 = VERTEX_POINT ( 'NONE', #28423 ) ;
#22658 = ORIENTED_EDGE ( 'NONE', *, *, #33578, .F. ) ;
#22660 = DIRECTION ( 'NONE',  ( 1.000000000000000000, 0.000000000000000000, 0.000000000000000000 ) ) ;
#22661 = CARTESIAN_POINT ( 'NONE',  ( -5.000000000000003553, -8.660254037844383745, -116.4999999999999858 ) ) ;
#22662 = CARTESIAN_POINT ( 'NONE',  ( 7.644554776091147741E-16, 12.48450537969573659, -178.1562500020484094 ) ) ;
#22663 = FACE_OUTER_BOUND ( 'NONE', #4444, .T. ) ;
#22664 = CARTESIAN_POINT ( 'NONE',  ( 9.999999999999998224, 0.000000000000000000, -50.37500000409675494 ) ) ;
#22665 = EDGE_CURVE ( 'NONE', #42101, #39394, #13767, .T. ) ;
#22666 = CARTESIAN_POINT ( 'NONE',  ( 10.81189881249999551, -6.242252689847874514, -128.9687500020483810 ) ) ;
#22667 = VECTOR ( 'NONE', #33520, 1000.000000000000000 ) ;
#22668 = CARTESIAN_POINT ( 'NONE',  ( 7.644554776091147741E-16, 12.48450537969573659, -102.9687500020483952 ) ) ;
#22669 = CARTESIAN_POINT ( 'NONE',  ( 9.999999999999998224, 0.000000000000000000, -138.8750000040968189 ) ) ;
#22670 = CARTESIAN_POINT ( 'NONE',  ( 5.405949406249999534, 9.363379034771803333, -112.2812500020483952 ) ) ;
#22671 = CARTESIAN_POINT ( 'NONE',  ( -5.000000000000003553, -8.660254037844383745, -191.8750000040967905 ) ) ;
#22672 = CARTESIAN_POINT ( 'NONE',  ( 10.81189881249999551, -6.242252689847874514, -115.4687500020483810 ) ) ;
#22673 = CARTESIAN_POINT ( 'NONE',  ( 7.644554776091147741E-16, 12.48450537969573659, -184.1562500020484094 ) ) ;
#22674 = EDGE_CURVE ( 'NONE', #14006, #36710, #9639, .T. ) ;
#22675 = CARTESIAN_POINT ( 'NONE',  ( -5.000000000000003553, -8.660254037844383745, -47.49999999999998579 ) ) ;
#22676 = CARTESIAN_POINT ( 'NONE',  ( -9.999999999999998224, 5.773502691896259087, -136.3750000000000000 ) ) ;
#22677 = CARTESIAN_POINT ( 'NONE',  ( -9.999999999999998224, 5.773502691896259087, -7.374999999999964473 ) ) ;
#22678 = CARTESIAN_POINT ( 'NONE',  ( 10.81189881249999729, 0.000000000000000000, -71.84375000204836681 ) ) ;
#22679 = VECTOR ( 'NONE', #13261, 1000.000000000000000 ) ;
#22680 = CARTESIAN_POINT ( 'NONE',  ( 5.405949406249999534, 9.363379034771803333, -50.59375000204835260 ) ) ;
#22681 = DESIGN_CONTEXT ( 'detailed design', #9654, 'design' ) ;
#22682 = CARTESIAN_POINT ( 'NONE',  ( 9.999999999999996447, -5.773502691896262640, -176.5000000040968189 ) ) ;
#22683 = CARTESIAN_POINT ( 'NONE',  ( -10.81189881249999729, 6.242252689847871849, -23.40625000204837747 ) ) ;
#22684 = CARTESIAN_POINT ( 'NONE',  ( -10.81189881249999729, 1.324075727343319199E-15, -30.59375000204836326 ) ) ;
#22685 = CARTESIAN_POINT ( 'NONE',  ( -9.999999999999998224, 1.224646799147353059E-15, -106.2499999999999858 ) ) ;
#22686 = CARTESIAN_POINT ( 'NONE',  ( 10.81189881249999907, 6.242252689847868297, -136.2187500020483810 ) ) ;
#22687 = CARTESIAN_POINT ( 'NONE',  ( 4.999999999999992006, -8.660254037844389075, -110.2499999999999858 ) ) ;
#22688 = CARTESIAN_POINT ( 'NONE',  ( -10.00000000000076916, 5.773502691895813221, -110.8749999999999574 ) ) ;
#22689 = CARTESIAN_POINT ( 'NONE',  ( -9.999999999999998224, 5.773502691896259087, -67.37499999999998579 ) ) ;
#22690 = CARTESIAN_POINT ( 'NONE',  ( -5.405949406249996869, 9.363379034771805109, -128.5312500020484094 ) ) ;
#22691 = CARTESIAN_POINT ( 'NONE',  ( 5.405949406249992428, -9.363379034771808662, -115.7812500020483952 ) ) ;
#22692 = ORIENTED_EDGE ( 'NONE', *, *, #12535, .F. ) ;
#22693 = CARTESIAN_POINT ( 'NONE',  ( 9.999999999999998224, 0.000000000000000000, -114.8750000040967905 ) ) ;
#22694 = CARTESIAN_POINT ( 'NONE',  ( 9.999999999999996447, -5.773502691896262640, -106.0000000040967763 ) ) ;
#22695 = CARTESIAN_POINT ( 'NONE',  ( -9.999999999999998224, 1.224646799147353059E-15, -102.1250000040967905 ) ) ;
#22696 = CARTESIAN_POINT ( 'NONE',  ( -5.405949406249996869, 9.363379034771805109, -68.34375000204836681 ) ) ;
#22697 = ORIENTED_EDGE ( 'NONE', *, *, #1146, .F. ) ;
#22698 = CARTESIAN_POINT ( 'NONE',  ( 7.070501591499377789E-16, 11.54700538379251284, -42.12499999999997868 ) ) ;
#22699 = CARTESIAN_POINT ( 'NONE',  ( -9.999999999999998224, 1.224646799147353059E-15, -21.12500000409675494 ) ) ;
#22700 = CARTESIAN_POINT ( 'NONE',  ( -5.405949406249996869, 9.363379034771805109, -47.53125000204838813 ) ) ;
#22701 = CARTESIAN_POINT ( 'NONE',  ( 9.999999999999998224, 0.000000000000000000, -24.87500000409675849 ) ) ;
#22702 = CARTESIAN_POINT ( 'NONE',  ( 5.000000000000000000, 8.660254037844385522, -44.12500000409677625 ) ) ;
#22703 = CARTESIAN_POINT ( 'NONE',  ( 7.644554776091147741E-16, 12.48450537969573659, -37.15625000204836681 ) ) ;
#22704 = CARTESIAN_POINT ( 'NONE',  ( -9.999999999999998224, 1.224646799147353059E-15, -117.1250000040967905 ) ) ;
#22705 = CARTESIAN_POINT ( 'NONE',  ( -5.405949406249996869, 9.363379034771805109, -139.0312500020484094 ) ) ;
#22706 = CARTESIAN_POINT ( 'NONE',  ( -2.293366432827344421E-15, -12.48450537969573659, -147.4062500020483810 ) ) ;
#22707 = EDGE_CURVE ( 'NONE', #12159, #2188, #40496, .T. ) ;
#22708 =( BOUNDED_CURVE ( )  B_SPLINE_CURVE ( 2, ( #8031, #27023, #33513, #7384, #37374, #24007, #27665 ),
 .UNSPECIFIED., .F., .F. ) 
 B_SPLINE_CURVE_WITH_KNOTS ( ( 3, 2, 2, 3 ),
 ( 0.4402985074626867279, 0.4415422885572141132, 0.4427860696517414429, 0.4440298507462688282 ),
 .UNSPECIFIED. ) 
 CURVE ( )  GEOMETRIC_REPRESENTATION_ITEM ( )  RATIONAL_B_SPLINE_CURVE ( ( 0.9999999999999820144, 0.8660254037844566932, 1.000000000000000000, 0.8660254037844387076, 1.000000000000000000, 0.8660254037844207220, 1.000000000000017986 ) ) 
 REPRESENTATION_ITEM ( '' )  );
#22709 = CARTESIAN_POINT ( 'NONE',  ( 9.999999999999479527, 5.773502691896553074, -150.7500000040967336 ) ) ;
#22710 = ORIENTED_EDGE ( 'NONE', *, *, #24156, .T. ) ;
#22711 = AXIS2_PLACEMENT_3D ( 'NONE', #39149, #25364, #28604 ) ;
#22712 = ORIENTED_EDGE ( 'NONE', *, *, #27036, .F. ) ;
#22713 = ORIENTED_EDGE ( 'NONE', *, *, #27856, .F. ) ;
#22714 = DIRECTION ( 'NONE',  ( -0.000000000000000000, -0.000000000000000000, 1.000000000000000000 ) ) ;
#22715 = CARTESIAN_POINT ( 'NONE',  ( 5.405949406249999534, 9.363379034771803333, -170.5937500020484094 ) ) ;
#22716 = CONICAL_SURFACE ( 'NONE', #40617, 45.00000000000000711, 0.7853981633974459475 ) ;
#22717 = CARTESIAN_POINT ( 'NONE',  ( -2.293366432827344421E-15, -12.48450537969573659, -21.21875000204837036 ) ) ;
#22718 = LINE ( 'NONE', #12970, #37080 ) ;
#22719 = CARTESIAN_POINT ( 'NONE',  ( 7.644554776091147741E-16, 12.48450537969573659, -161.4687500020484094 ) ) ;
#22720 = CARTESIAN_POINT ( 'NONE',  ( 5.405949406249992428, -9.363379034771808662, -142.5937500020483810 ) ) ;
#22721 = DIRECTION ( 'NONE',  ( -0.000000000000000000, -0.000000000000000000, -1.000000000000000000 ) ) ;
#22722 = CARTESIAN_POINT ( 'NONE',  ( -5.405949406249996869, 9.363379034771805109, -123.8437500020483952 ) ) ;
#22723 = CARTESIAN_POINT ( 'NONE',  ( 10.81189881249999551, -6.242252689847874514, -129.1562500020483810 ) ) ;
#22724 = CARTESIAN_POINT ( 'NONE',  ( 5.405949406249992428, -9.363379034771808662, -21.09375000204835615 ) ) ;
#22725 = CARTESIAN_POINT ( 'NONE',  ( 10.81189881249999729, 6.242252689847867408, -145.2187500020484094 ) ) ;
#22726 = CARTESIAN_POINT ( 'NONE',  ( 9.999999999999998224, 0.000000000000000000, -179.0000000000000000 ) ) ;
#22727 = CARTESIAN_POINT ( 'NONE',  ( 0.000000000000000000, 0.000000000000000000, -200.0000000000000000 ) ) ;
#22728 = CARTESIAN_POINT ( 'NONE',  ( -9.999999999999998224, 5.773502691896259087, -161.8750000000000000 ) ) ;
#22729 = CARTESIAN_POINT ( 'NONE',  ( -9.999999999999998224, 1.224646799147353059E-15, -168.1250000040967905 ) ) ;
#22730 = CARTESIAN_POINT ( 'NONE',  ( -2.293366432827344421E-15, -12.48450537969573659, -76.71875000204838102 ) ) ;
#22731 = CARTESIAN_POINT ( 'NONE',  ( 10.81189881249999551, -6.242252689847874514, -54.15625000204837391 ) ) ;
#22732 = CARTESIAN_POINT ( 'NONE',  ( -5.405949406249996869, 9.363379034771805109, -50.34375000204835260 ) ) ;
#22733 = CARTESIAN_POINT ( 'NONE',  ( 9.999999999999998224, 0.000000000000000000, -15.87500000409675138 ) ) ;
#22734 = CARTESIAN_POINT ( 'NONE',  ( -10.81189881249999907, -6.242252689847864744, -159.4687500020484094 ) ) ;
#22735 = CARTESIAN_POINT ( 'NONE',  ( 7.070501591499377789E-16, 11.54700538379251284, -141.1250000000000000 ) ) ;
#22736 = CARTESIAN_POINT ( 'NONE',  ( 10.81189881249999729, 6.242252689847867408, -140.9062500020484094 ) ) ;
#22737 = CARTESIAN_POINT ( 'NONE',  ( -5.000000000000003553, -8.660254037844383745, -151.0000000000000000 ) ) ;
#22738 = CARTESIAN_POINT ( 'NONE',  ( -4.999999999999996447, 8.660254037844387298, -117.3750000040967905 ) ) ;
#22739 = CARTESIAN_POINT ( 'NONE',  ( -9.999999999999998224, 5.773502691896259087, -89.87499999999998579 ) ) ;
#22740 = ORIENTED_EDGE ( 'NONE', *, *, #7944, .F. ) ;
#22741 = CARTESIAN_POINT ( 'NONE',  ( -10.81189881249999729, -6.242252689847864744, -119.1562500020484237 ) ) ;
#22742 = CARTESIAN_POINT ( 'NONE',  ( 5.000000000000000000, 8.660254037844385522, -137.1250000040967620 ) ) ;
#22743 = DIRECTION ( 'NONE',  ( -0.000000000000000000, -0.000000000000000000, -1.000000000000000000 ) ) ;
#22744 = CARTESIAN_POINT ( 'NONE',  ( -5.405949406250003975, -9.363379034771801557, -176.0312500020483810 ) ) ;
#22745 = CARTESIAN_POINT ( 'NONE',  ( 9.999999999999996447, -5.773502691896262640, -53.50000000409677625 ) ) ;
#22746 = CARTESIAN_POINT ( 'NONE',  ( 0.000000000000000000, 0.000000000000000000, -99.99999999999998579 ) ) ;
#22747 = CARTESIAN_POINT ( 'NONE',  ( 10.81189881249999551, -6.242252689847874514, -63.15625000204838813 ) ) ;
#22748 =( BOUNDED_CURVE ( )  B_SPLINE_CURVE ( 2, ( #37268, #15017, #41349, #18265, #38130, #34696, #7930 ),
 .UNSPECIFIED., .F., .F. ) 
 B_SPLINE_CURVE_WITH_KNOTS ( ( 3, 2, 2, 3 ),
 ( 0.08582089552238814090, 0.08706467661691551230, 0.08830845771144288370, 0.08955223880597024122 ),
 .UNSPECIFIED. ) 
 CURVE ( )  GEOMETRIC_REPRESENTATION_ITEM ( )  RATIONAL_B_SPLINE_CURVE ( ( 0.9999999999999910072, 0.8660254037844477004, 1.000000000000000000, 0.8660254037844387076, 1.000000000000000000, 0.8660254037844282715, 1.000000000000010436 ) ) 
 REPRESENTATION_ITEM ( '' )  );
#22749 = CARTESIAN_POINT ( 'NONE',  ( 10.00000000000154010, -5.773502691895370020, -63.62499999999992895 ) ) ;
#22750 = CARTESIAN_POINT ( 'NONE',  ( 10.81189881249999729, 0.000000000000000000, -157.5312500020484094 ) ) ;
#22751 = CARTESIAN_POINT ( 'NONE',  ( 7.644554776091147741E-16, 12.48450537969573659, -140.4687500020483810 ) ) ;
#22752 = CARTESIAN_POINT ( 'NONE',  ( -4.999999999999996447, 8.660254037844387298, -100.4999999999999858 ) ) ;
#22754 = EDGE_CURVE ( 'NONE', #15095, #16464, #25657, .T. ) ;
#22753 = FACE_OUTER_BOUND ( 'NONE', #21540, .T. ) ;
#22755 = ORIENTED_EDGE ( 'NONE', *, *, #40781, .T. ) ;
#22756 = EDGE_CURVE ( 'NONE', #38155, #38638, #31482, .T. ) ;
#22757 = CARTESIAN_POINT ( 'NONE',  ( 9.999999999999998224, 0.000000000000000000, -114.8750000040967905 ) ) ;
#22759 = VERTEX_POINT ( 'NONE', #2718 ) ;
#22758 = CARTESIAN_POINT ( 'NONE',  ( 10.81189881249999729, 0.000000000000000000, -70.53125000204838102 ) ) ;
#22760 = APPROVAL_DATE_TIME ( #3332, #10370 ) ;
#22762 = ORIENTED_EDGE ( 'NONE', *, *, #28566, .F. ) ;
#22761 = CARTESIAN_POINT ( 'NONE',  ( -5.405949406250003975, -9.363379034771801557, -118.8437500020483810 ) ) ;
#22763 = ORIENTED_EDGE ( 'NONE', *, *, #22014, .F. ) ;
#22764 = CARTESIAN_POINT ( 'NONE',  ( 5.405949406249992428, -9.363379034771808662, -27.09375000204835970 ) ) ;
#22765 = CARTESIAN_POINT ( 'NONE',  ( -10.81189881249999907, -6.242252689847864744, -193.9687500020484094 ) ) ;
#22766 = CARTESIAN_POINT ( 'NONE',  ( -10.81189881249999729, 6.242252689847871849, -59.21875000204837391 ) ) ;
#22767 = CARTESIAN_POINT ( 'NONE',  ( -9.999999999999998224, 1.224646799147353059E-15, -127.2499999999999716 ) ) ;
#22768 = CARTESIAN_POINT ( 'NONE',  ( -2.121150477449813534E-15, -11.54700538379251284, -32.37499999999996447 ) ) ;
#22769 = EDGE_CURVE ( 'NONE', #22182, #27209, #16544, .T. ) ;
#22770 = CARTESIAN_POINT ( 'NONE',  ( -5.405949406250003975, -9.363379034771801557, -190.8437500020484094 ) ) ;
#22771 = CARTESIAN_POINT ( 'NONE',  ( 10.81189881249999551, -6.242252689847874514, -166.4687500020484094 ) ) ;
#22772 = CARTESIAN_POINT ( 'NONE',  ( 5.405949406249992428, -9.363379034771808662, -151.5937500020483810 ) ) ;
#22773 = CARTESIAN_POINT ( 'NONE',  ( -10.81189881249999729, -6.242252689847864744, -168.4687500020483526 ) ) ;
#22774 = LINE ( 'NONE', #3560, #8854 ) ;
#22775 = CARTESIAN_POINT ( 'NONE',  ( -4.999999999999996447, 8.660254037844387298, -193.8750000040967905 ) ) ;
#22776 = CARTESIAN_POINT ( 'NONE',  ( 10.00000000000000000, 5.773502691896255534, -186.3750000000000284 ) ) ;
#22777 = CARTESIAN_POINT ( 'NONE',  ( 10.81189881249999907, 6.242252689847868297, -100.2187500020483810 ) ) ;
#22778 = CARTESIAN_POINT ( 'NONE',  ( -4.999999999999996447, 8.660254037844387298, -108.3750000040967763 ) ) ;
#22779 = CARTESIAN_POINT ( 'NONE',  ( -10.81189881249999729, 6.242252689847871849, -71.40625000204838102 ) ) ;
#22780 = LINE ( 'NONE', #32709, #16416 ) ;
#22781 = CARTESIAN_POINT ( 'NONE',  ( 7.644554776091147741E-16, 12.48450537969573659, -188.4687500020484094 ) ) ;
#22782 = CARTESIAN_POINT ( 'NONE',  ( -5.405949406250003975, -9.363379034771801557, -82.84375000204836681 ) ) ;
#22783 = ADVANCED_FACE ( 'NONE', ( #35320 ), #5749, .T. ) ;
#22784 = CARTESIAN_POINT ( 'NONE',  ( -5.405949406250003975, -9.363379034771801557, -62.03125000204837391 ) ) ;
#22785 = CARTESIAN_POINT ( 'NONE',  ( -10.00000000000000000, -5.773502691896251982, -135.0000000040967905 ) ) ;
#22786 = CARTESIAN_POINT ( 'NONE',  ( 10.00000000000000000, 5.773502691896255534, -118.8749999999999858 ) ) ;
#22787 = EDGE_LOOP ( 'NONE', ( #25745, #6150, #33967, #5230 ) ) ;
#22788 = CARTESIAN_POINT ( 'NONE',  ( -10.81189881249999729, 6.242252689847871849, -144.9062500020484094 ) ) ;
#22789 = CARTESIAN_POINT ( 'NONE',  ( 5.405949406249999534, 9.363379034771803333, -158.7812500020484094 ) ) ;
#22790 = CARTESIAN_POINT ( 'NONE',  ( 5.405949406249992428, -9.363379034771808662, -198.2812500020484094 ) ) ;
#22791 = CARTESIAN_POINT ( 'NONE',  ( 9.999999999999998224, 0.000000000000000000, -200.0000000000000000 ) ) ;
#22792 = CARTESIAN_POINT ( 'NONE',  ( -5.405949406250003975, -9.363379034771801557, -90.34375000204838102 ) ) ;
#22793 = ORIENTED_EDGE ( 'NONE', *, *, #36252, .T. ) ;
#22794 = CARTESIAN_POINT ( 'NONE',  ( 9.999999999999996447, -5.773502691896262640, -57.62499999999998579 ) ) ;
#22795 = CARTESIAN_POINT ( 'NONE',  ( -2.293366432827344421E-15, -12.48450537969573659, -190.7187500020484094 ) ) ;
#22796 = CARTESIAN_POINT ( 'NONE',  ( -2.121150477449813534E-15, -11.54700538379251284, -70.25000000409679046 ) ) ;
#22797 = CARTESIAN_POINT ( 'NONE',  ( 4.999999999999992006, -8.660254037844389075, -169.1250000040967905 ) ) ;
#22798 = CARTESIAN_POINT ( 'NONE',  ( 4.999999999999992006, -8.660254037844389075, -123.7500000000000000 ) ) ;
#22799 = CARTESIAN_POINT ( 'NONE',  ( -10.81189881249999729, 1.324075727343319199E-15, -83.28125000204838102 ) ) ;
#22800 = CARTESIAN_POINT ( 'NONE',  ( -10.81189881249999729, 1.324075727343319199E-15, -71.28125000204838102 ) ) ;
#22801 = CARTESIAN_POINT ( 'NONE',  ( 10.00000000000000000, 5.773502691896255534, -62.25000000409676915 ) ) ;
#22802 = CARTESIAN_POINT ( 'NONE',  ( -10.81189881249999907, -6.242252689847864744, -21.46875000204836681 ) ) ;
#22803 = CARTESIAN_POINT ( 'NONE',  ( 9.999999999999998224, 0.000000000000000000, -200.0000000000000000 ) ) ;
#22804 = CARTESIAN_POINT ( 'NONE',  ( 10.81189881249999907, 6.242252689847868297, -185.9062500020484094 ) ) ;
#22805 = VECTOR ( 'NONE', #36658, 1000.000000000000000 ) ;
#22806 = CARTESIAN_POINT ( 'NONE',  ( 10.81189881249999729, 0.000000000000000000, -13.53125000204835615 ) ) ;
#22807 = CARTESIAN_POINT ( 'NONE',  ( 5.000000000000000000, 8.660254037844385522, -79.74999999999998579 ) ) ;
#22808 = FACE_OUTER_BOUND ( 'NONE', #1271, .T. ) ;
#22809 = VECTOR ( 'NONE', #13906, 1000.000000000000000 ) ;
#22810 = CARTESIAN_POINT ( 'NONE',  ( -10.00000000000000000, -0.8677423694974171209, 0.000000000000000000 ) ) ;
#22811 = CARTESIAN_POINT ( 'NONE',  ( -1.040834085586084257E-14, -20.00000000000000355, 22.49999999999999289 ) ) ;
#22812 = ADVANCED_FACE ( 'NONE', ( #29253 ), #19111, .T. ) ;
#22813 = CARTESIAN_POINT ( 'NONE',  ( -9.999999999999998224, 5.773502691896259087, -166.3749999999999716 ) ) ;
#22814 = CYLINDRICAL_SURFACE ( 'NONE', #40633, 9.999999999999998224 ) ;
#22815 = EDGE_CURVE ( 'NONE', #42101, #12898, #39377, .T. ) ;
#22817 = ORIENTED_EDGE ( 'NONE', *, *, #28094, .F. ) ;
#22816 = CARTESIAN_POINT ( 'NONE',  ( -5.405949406249996869, 9.363379034771805109, -97.03125000204839523 ) ) ;
#22818 = CARTESIAN_POINT ( 'NONE',  ( 9.999999999999998224, 0.000000000000000000, -24.87500000409675849 ) ) ;
#22820 = ORIENTED_EDGE ( 'NONE', *, *, #23564, .F. ) ;
#22819 = LINE ( 'NONE', #33598, #665 ) ;
#22821 = VERTEX_POINT ( 'NONE', #9185 ) ;
#22822 = CARTESIAN_POINT ( 'NONE',  ( -10.81189881249999729, 6.242252689847871849, -38.21875000204836681 ) ) ;
#22823 = CARTESIAN_POINT ( 'NONE',  ( 7.644554776091147741E-16, 12.48450537969573659, -20.65625000204838102 ) ) ;
#22824 = APPROVAL_DATE_TIME ( #2347, #23837 ) ;
#22825 = CARTESIAN_POINT ( 'NONE',  ( -5.405949406249996869, 9.363379034771805109, -75.84375000204838102 ) ) ;
#22826 = DIRECTION ( 'NONE',  ( -0.000000000000000000, -0.000000000000000000, 1.000000000000000000 ) ) ;
#22827 = CARTESIAN_POINT ( 'NONE',  ( -5.405949406250003975, -9.363379034771801557, -196.8437500020484094 ) ) ;
#22828 = EDGE_CURVE ( 'NONE', #24456, #14015, #42188, .T. ) ;
#22829 = CARTESIAN_POINT ( 'NONE',  ( 5.000000000000000000, 8.660254037844385522, -124.7500000000000000 ) ) ;
#22830 = CARTESIAN_POINT ( 'NONE',  ( 10.00000000000012790, 5.773502691896179151, -172.8750000000000000 ) ) ;
#22831 = CARTESIAN_POINT ( 'NONE',  ( -10.81189881249999729, 6.242252689847871849, -155.4062500020483810 ) ) ;
#22832 = CARTESIAN_POINT ( 'NONE',  ( -5.000000000000003553, -8.660254037844383745, 0.1249999959032355168 ) ) ;
#22833 = CARTESIAN_POINT ( 'NONE',  ( 9.999999999999742428, 5.773502691896404748, -121.8750000000000142 ) ) ;
#22834 = APPROVAL_PERSON_ORGANIZATION ( #28031, #9846, #5149 ) ;
#22835 = CARTESIAN_POINT ( 'NONE',  ( -10.81189881249999907, -6.242252689847864744, -118.9687500020483810 ) ) ;
#22836 = CARTESIAN_POINT ( 'NONE',  ( 10.81189881249999907, 6.242252689847868297, -100.4062500020483952 ) ) ;
#22837 = CARTESIAN_POINT ( 'NONE',  ( 10.81189881249999729, 0.000000000000000000, -109.3437500020483810 ) ) ;
#22838 = CARTESIAN_POINT ( 'NONE',  ( -10.81189881249999729, 1.324075727343319199E-15, -81.59375000204838102 ) ) ;
#22839 = CARTESIAN_POINT ( 'NONE',  ( -5.405949406250003975, -9.363379034771801557, -86.03125000204838102 ) ) ;
#22840 = CARTESIAN_POINT ( 'NONE',  ( -2.121150477449813534E-15, -11.54700538379251284, -170.7500000040967620 ) ) ;
#22841 = DIRECTION ( 'NONE',  ( 1.000000000000000000, 0.000000000000000000, 0.000000000000000000 ) ) ;
#22842 = CARTESIAN_POINT ( 'NONE',  ( 10.81189881249999729, 6.242252689847867408, -169.4062500020484094 ) ) ;
#22843 = CARTESIAN_POINT ( 'NONE',  ( 5.405949406249992428, -9.363379034771808662, -177.2812500020484094 ) ) ;
#22844 = CARTESIAN_POINT ( 'NONE',  ( 9.999999999999996447, -5.773502691896262640, -154.0000000040968189 ) ) ;
#22845 = CARTESIAN_POINT ( 'NONE',  ( -9.999999999999998224, 1.224646799147353059E-15, -197.7500000000000000 ) ) ;
#22846 = CARTESIAN_POINT ( 'NONE',  ( -10.81189881249999907, -6.242252689847864744, -4.968750002048355263 ) ) ;
#22847 = CARTESIAN_POINT ( 'NONE',  ( -2.121150477449813534E-15, -11.54700538379251284, -156.8750000000000000 ) ) ;
#22848 = CARTESIAN_POINT ( 'NONE',  ( 10.81189881249999729, 0.000000000000000000, -113.8437500020483810 ) ) ;
#22849 = CARTESIAN_POINT ( 'NONE',  ( 9.999999999999996447, -5.773502691896262640, -80.12500000000000000 ) ) ;
#22850 = CARTESIAN_POINT ( 'NONE',  ( 5.405949406249999534, 9.363379034771803333, -16.28125000204835970 ) ) ;
#22851 = CARTESIAN_POINT ( 'NONE',  ( 9.999999999999998224, 0.000000000000000000, -96.87500000409677625 ) ) ;
#22852 = CYLINDRICAL_SURFACE ( 'NONE', #40978, 9.999999999999998224 ) ;
#22853 = CARTESIAN_POINT ( 'NONE',  ( -10.81189881249999729, 6.242252689847871849, -104.4062500020483810 ) ) ;
#22854 = CARTESIAN_POINT ( 'NONE',  ( -5.405949406249996869, 9.363379034771805109, -95.53125000204838102 ) ) ;
#22855 = ORIENTED_EDGE ( 'NONE', *, *, #34657, .T. ) ;
#22856 = CARTESIAN_POINT ( 'NONE',  ( -2.121150477449813534E-15, -11.54700538379251284, -82.25000000409676204 ) ) ;
#22857 = FACE_OUTER_BOUND ( 'NONE', #2807, .T. ) ;
#22858 = CARTESIAN_POINT ( 'NONE',  ( -10.81189881249999729, 6.242252689847871849, -38.21875000204835970 ) ) ;
#22859 = ORIENTED_EDGE ( 'NONE', *, *, #8003, .T. ) ;
#22860 = CARTESIAN_POINT ( 'NONE',  ( -5.000000000000003553, -8.660254037844383745, -6.999999999999978684 ) ) ;
#22861 = CARTESIAN_POINT ( 'NONE',  ( -2.121150477449813534E-15, -11.54700538379251284, -146.3750000000000000 ) ) ;
#22862 = CARTESIAN_POINT ( 'NONE',  ( -5.000000000000003553, -8.660254037844383745, -8.875000004096744277 ) ) ;
#22863 = AXIS2_PLACEMENT_3D ( 'NONE', #11005, #21150, #37348 ) ;
#22864 = PRODUCT_DEFINITION_FORMATION_WITH_SPECIFIED_SOURCE ( 'ANY', '', #21848, .NOT_KNOWN. ) ;
#22865 = CARTESIAN_POINT ( 'NONE',  ( 10.00000000000000000, 5.773502691896255534, -196.8750000000000284 ) ) ;
#22867 = ORIENTED_EDGE ( 'NONE', *, *, #30548, .T. ) ;
#22866 = CARTESIAN_POINT ( 'NONE',  ( 10.81189881249999551, -6.242252689847874514, -117.1562500020483810 ) ) ;
#22868 = CARTESIAN_POINT ( 'NONE',  ( -9.999999999999998224, 1.224646799147353059E-15, -142.2500000000000000 ) ) ;
#22869 = ORIENTED_EDGE ( 'NONE', *, *, #34654, .T. ) ;
#22870 =( BOUNDED_CURVE ( )  B_SPLINE_CURVE ( 2, ( #36230, #33221, #10737, #6664, #39669, #10316, #13331 ),
 .UNSPECIFIED., .F., .F. ) 
 B_SPLINE_CURVE_WITH_KNOTS ( ( 3, 2, 2, 3 ),
 ( 0.8320895522388060961, 0.8333333333333334814, 0.8345771144278608666, 0.8358208955223882519 ),
 .UNSPECIFIED. ) 
 CURVE ( )  GEOMETRIC_REPRESENTATION_ITEM ( )  RATIONAL_B_SPLINE_CURVE ( ( 0.9999999999999880096, 0.8660254037844506980, 1.000000000000000000, 0.8660254037844387076, 1.000000000000000000, 0.8660254037844148378, 1.000000000000023981 ) ) 
 REPRESENTATION_ITEM ( '' )  );
#22871 = CARTESIAN_POINT ( 'NONE',  ( -5.405949406249996869, 9.363379034771805109, -52.03125000204835970 ) ) ;
#22872 = COORDINATED_UNIVERSAL_TIME_OFFSET ( 6, 0, .AHEAD. ) ;
#22873 = VECTOR ( 'NONE', #8450, 1000.000000000000000 ) ;
#22874 = EDGE_CURVE ( 'NONE', #40403, #30149, #28693, .T. ) ;
#22875 = CARTESIAN_POINT ( 'NONE',  ( 10.81189881249999729, 0.000000000000000000, -104.8437500020483810 ) ) ;
#22876 = CARTESIAN_POINT ( 'NONE',  ( -10.81189881249999729, 1.324075727343319199E-15, -122.2812500020483952 ) ) ;
#22877 = EDGE_LOOP ( 'NONE', ( #37356, #13965, #23433, #27753 ) ) ;
#22878 = CARTESIAN_POINT ( 'NONE',  ( 4.999999999999992006, -8.660254037844389075, -132.7499999999999716 ) ) ;
#22879 = DIRECTION ( 'NONE',  ( 0.000000000000000000, 0.000000000000000000, -1.000000000000000000 ) ) ;
#22880 =( BOUNDED_CURVE ( )  B_SPLINE_CURVE ( 2, ( #26142, #22478, #19232, #42102, #5664, #12323, #2223 ),
 .UNSPECIFIED., .F., .F. ) 
 B_SPLINE_CURVE_WITH_KNOTS ( ( 3, 2, 2, 3 ),
 ( 0.1156716417910447492, 0.1169154228855721483, 0.1181592039800995753, 0.1194029850746269744 ),
 .UNSPECIFIED. ) 
 CURVE ( )  GEOMETRIC_REPRESENTATION_ITEM ( )  RATIONAL_B_SPLINE_CURVE ( ( 1.000000000000003109, 0.8660254037844358210, 1.000000000000000000, 0.8660254037844387076, 1.000000000000000000, 0.8660254037844267172, 1.000000000000011990 ) ) 
 REPRESENTATION_ITEM ( '' )  );
#22881 = CARTESIAN_POINT ( 'NONE',  ( 5.405949406249992428, -9.363379034771808662, -181.7812500020483810 ) ) ;
#22882 = CARTESIAN_POINT ( 'NONE',  ( 7.644554776091147741E-16, 12.48450537969573659, 0.5312499979516547288 ) ) ;
#22883 = CARTESIAN_POINT ( 'NONE',  ( 9.999999999999998224, 0.000000000000000000, -8.375000004096744277 ) ) ;
#22884 = CARTESIAN_POINT ( 'NONE',  ( -10.81189881249999729, 6.242252689847871849, -132.7187500020483810 ) ) ;
#22885 = CARTESIAN_POINT ( 'NONE',  ( 10.81189881249999907, 6.242252689847868297, -101.7187500020483810 ) ) ;
#22886 = CARTESIAN_POINT ( 'NONE',  ( -9.999999999999998224, 1.224646799147353059E-15, -158.7500000000000000 ) ) ;
#22887 = CARTESIAN_POINT ( 'NONE',  ( 10.81189881249999729, 0.000000000000000000, -112.5312500020483952 ) ) ;
#22888 = CARTESIAN_POINT ( 'NONE',  ( -2.121150477449813534E-15, -11.54700538379251284, -197.7500000040967905 ) ) ;
#22890 = EDGE_CURVE ( 'NONE', #30244, #3006, #25904, .T. ) ;
#22889 = CARTESIAN_POINT ( 'NONE',  ( -5.405949406249996869, 9.363379034771805109, -117.8437500020483810 ) ) ;
#22891 = AXIS2_PLACEMENT_3D ( 'NONE', #12175, #15409, #25366 ) ;
#22892 = CARTESIAN_POINT ( 'NONE',  ( -10.81189881249999729, -6.242252689847864744, -185.1562500020484094 ) ) ;
#22893 =( BOUNDED_CURVE ( )  B_SPLINE_CURVE ( 2, ( #6346, #9780, #19489, #3105, #22960, #36115, #22109 ),
 .UNSPECIFIED., .F., .F. ) 
 B_SPLINE_CURVE_WITH_KNOTS ( ( 3, 2, 2, 3 ),
 ( 0.2873134328358210032, 0.2885572139303483885, 0.2898009950248757183, 0.2910447761194031036 ),
 .UNSPECIFIED. ) 
 CURVE ( )  GEOMETRIC_REPRESENTATION_ITEM ( )  RATIONAL_B_SPLINE_CURVE ( ( 0.9999999999999880096, 0.8660254037844506980, 1.000000000000000000, 0.8660254037844387076, 1.000000000000000000, 0.8660254037844267172, 1.000000000000011990 ) ) 
 REPRESENTATION_ITEM ( '' )  );
#22894 = CYLINDRICAL_SURFACE ( 'NONE', #2726, 20.00000000000000355 ) ;
#22895 = CARTESIAN_POINT ( 'NONE',  ( -9.999999999999998224, 1.224646799147353059E-15, -142.2500000000000000 ) ) ;
#22896 = CARTESIAN_POINT ( 'NONE',  ( 7.070501591499377789E-16, 11.54700538379251284, -3.124999999999961364 ) ) ;
#22897 = CARTESIAN_POINT ( 'NONE',  ( -5.405949406250003975, -9.363379034771801557, -63.34375000204836681 ) ) ;
#22898 = CARTESIAN_POINT ( 'NONE',  ( -5.405949406250003975, -9.363379034771801557, -51.34375000204835260 ) ) ;
#22899 =( REPRESENTATION_RELATIONSHIP ('NONE','NONE', #21658, #36293 ) REPRESENTATION_RELATIONSHIP_WITH_TRANSFORMATION ( #29508 )SHAPE_REPRESENTATION_RELATIONSHIP( ) );
#22900 = CARTESIAN_POINT ( 'NONE',  ( -5.000000000000003553, -8.660254037844383745, -179.8750000040967905 ) ) ;
#22901 = CARTESIAN_POINT ( 'NONE',  ( -5.405949406249996869, 9.363379034771805109, -22.03125000204836326 ) ) ;
#22902 = CARTESIAN_POINT ( 'NONE',  ( 7.644554776091147741E-16, 12.48450537969573659, -30.96875000204835260 ) ) ;
#22903 = CARTESIAN_POINT ( 'NONE',  ( 9.999999999999998224, 0.000000000000000000, -176.0000000000000000 ) ) ;
#22904 = CARTESIAN_POINT ( 'NONE',  ( -10.81189881249999729, 1.324075727343319199E-15, -137.0937500020483810 ) ) ;
#22905 = CARTESIAN_POINT ( 'NONE',  ( -2.121150477449813534E-15, -11.54700538379251284, -107.3749999999999716 ) ) ;
#22906 = CARTESIAN_POINT ( 'NONE',  ( -9.999999999999998224, 1.224646799147353059E-15, -115.2499999999999858 ) ) ;
#22907 = CARTESIAN_POINT ( 'NONE',  ( -9.999999999999998224, 1.224646799147353059E-15, -68.74999999999997158 ) ) ;
#22908 = CARTESIAN_POINT ( 'NONE',  ( -10.81189881249999907, -6.242252689847864744, -134.1562500020483810 ) ) ;
#22909 = CARTESIAN_POINT ( 'NONE',  ( 10.81189881249999551, -6.242252689847874514, -115.6562500020483810 ) ) ;
#22910 = ORIENTED_EDGE ( 'NONE', *, *, #17051, .F. ) ;
#22911 = FACE_BOUND ( 'NONE', #28242, .T. ) ;
#22912 = CARTESIAN_POINT ( 'NONE',  ( -5.000000000000003553, -8.660254037844383745, -110.8750000040967763 ) ) ;
#22913 = CARTESIAN_POINT ( 'NONE',  ( 5.000000000000000000, 8.660254037844385522, -101.1250000040967905 ) ) ;
#22914 = CARTESIAN_POINT ( 'NONE',  ( 10.81189881249999729, 0.000000000000000000, -64.34375000204836681 ) ) ;
#22915 = ORIENTED_EDGE ( 'NONE', *, *, #6671, .T. ) ;
#22916 = CARTESIAN_POINT ( 'NONE',  ( -9.999999999999998224, 1.224646799147353059E-15, -44.74999999999998579 ) ) ;
#22917 = VECTOR ( 'NONE', #18559, 1000.000000000000000 ) ;
#22918 = CARTESIAN_POINT ( 'NONE',  ( 9.999999999999998224, 0.000000000000000000, -15.87500000409675138 ) ) ;
#22919 = CARTESIAN_POINT ( 'NONE',  ( 7.644554776091147741E-16, 12.48450537969573659, -41.65625000204836681 ) ) ;
#22920 = LINE ( 'NONE', #38887, #19397 ) ;
#22921 = CARTESIAN_POINT ( 'NONE',  ( -9.999999999999998224, 5.773502691896259087, -33.25000000409675494 ) ) ;
#22922 = CARTESIAN_POINT ( 'NONE',  ( 9.999999999999998224, 0.000000000000000000, -200.0000000000000000 ) ) ;
#22923 = CARTESIAN_POINT ( 'NONE',  ( -10.81189881249999729, 6.242252689847871849, -138.9062500020484094 ) ) ;
#22924 = CARTESIAN_POINT ( 'NONE',  ( 5.405949406249992428, -9.363379034771808662, -153.2812500020484094 ) ) ;
#22925 = DIRECTION ( 'NONE',  ( -0.000000000000000000, -1.000000000000000000, -0.000000000000000000 ) ) ;
#22926 = ORIENTED_EDGE ( 'NONE', *, *, #31024, .T. ) ;
#22927 = VECTOR ( 'NONE', #40655, 1000.000000000000000 ) ;
#22928 = EDGE_CURVE ( 'NONE', #36134, #6564, #29824, .T. ) ;
#22929 = ORIENTED_EDGE ( 'NONE', *, *, #14598, .F. ) ;
#22930 = ORIENTED_EDGE ( 'NONE', *, *, #13755, .T. ) ;
#22931 = LINE ( 'NONE', #16842, #2881 ) ;
#22932 = CARTESIAN_POINT ( 'NONE',  ( -10.81189881249999729, 1.324075727343319199E-15, -174.5937500020484094 ) ) ;
#22933 = AXIS2_PLACEMENT_3D ( 'NONE', #471, #26983, #3477 ) ;
#22934 = CARTESIAN_POINT ( 'NONE',  ( -10.81189881249999907, -6.242252689847864744, -24.46875000204836681 ) ) ;
#22935 = CARTESIAN_POINT ( 'NONE',  ( 9.999999999999998224, 0.000000000000000000, -128.3750000040967905 ) ) ;
#22936 = CARTESIAN_POINT ( 'NONE',  ( 5.405949406249999534, 9.363379034771803333, -154.0937500020483810 ) ) ;
#22937 = CARTESIAN_POINT ( 'NONE',  ( -10.81189881249999729, 6.242252689847871849, -143.2187500020484094 ) ) ;
#22938 = ADVANCED_FACE ( 'NONE', ( #29682 ), #17337, .F. ) ;
#22939 = CARTESIAN_POINT ( 'NONE',  ( -5.405949406250003975, -9.363379034771801557, -123.3437500020483952 ) ) ;
#22940 = CARTESIAN_POINT ( 'NONE',  ( -10.81189881249999729, 6.242252689847871849, -132.9062500020483810 ) ) ;
#22941 = CARTESIAN_POINT ( 'NONE',  ( -5.405949406249996869, 9.363379034771805109, -21.84375000204835615 ) ) ;
#22942 = CARTESIAN_POINT ( 'NONE',  ( 5.405949406249999534, 9.363379034771803333, -134.5937500020483810 ) ) ;
#22943 = CARTESIAN_POINT ( 'NONE',  ( -9.999999999999227285, -5.773502691896698735, -126.0000000040967478 ) ) ;
#22944 = CARTESIAN_POINT ( 'NONE',  ( 9.999999999999998224, 0.000000000000000000, -25.99999999999996803 ) ) ;
#22945 = CARTESIAN_POINT ( 'NONE',  ( -2.121150477449813534E-15, -11.54700538379251284, -167.3750000000000000 ) ) ;
#22946 = CARTESIAN_POINT ( 'NONE',  ( 9.999999999999998224, 0.000000000000000000, -86.37500000409677625 ) ) ;
#22947 = CARTESIAN_POINT ( 'NONE',  ( -2.293366432827344421E-15, -12.48450537969573659, -69.21875000204839523 ) ) ;
#22948 = CARTESIAN_POINT ( 'NONE',  ( 10.81189881249999551, -6.242252689847874514, -45.15625000204836681 ) ) ;
#22949 = CARTESIAN_POINT ( 'NONE',  ( 5.405949406249999534, 9.363379034771803333, -53.59375000204835970 ) ) ;
#22950 = DIRECTION ( 'NONE',  ( -0.000000000000000000, -0.000000000000000000, -1.000000000000000000 ) ) ;
#22951 = CARTESIAN_POINT ( 'NONE',  ( -10.81189881249999729, 6.242252689847871849, -158.2187500020483810 ) ) ;
#22952 = CARTESIAN_POINT ( 'NONE',  ( 5.000000000000000000, 8.660254037844385522, -135.2499999999999716 ) ) ;
#22953 = CARTESIAN_POINT ( 'NONE',  ( -10.81189881249999729, -6.242252689847864744, -140.1562500020484094 ) ) ;
#22954 = CARTESIAN_POINT ( 'NONE',  ( -9.999999999999998224, 1.224646799147353059E-15, -99.12500000409677625 ) ) ;
#22955 = CARTESIAN_POINT ( 'NONE',  ( -2.121150477449813534E-15, -11.54700538379251284, -112.2500000040967763 ) ) ;
#22956 = CARTESIAN_POINT ( 'NONE',  ( -9.999999999999998224, 5.773502691896259087, -94.37499999999998579 ) ) ;
#22957 = ORIENTED_EDGE ( 'NONE', *, *, #42564, .F. ) ;
#22958 = CARTESIAN_POINT ( 'NONE',  ( -2.293366432827344421E-15, -12.48450537969573659, -117.4062500020483952 ) ) ;
#22959 = CARTESIAN_POINT ( 'NONE',  ( 7.070501591499377789E-16, 11.54700538379251284, -132.5000000040967620 ) ) ;
#22960 = CARTESIAN_POINT ( 'NONE',  ( 4.999999999999992006, -8.660254037844389075, -140.6250000040967905 ) ) ;
#22961 = CARTESIAN_POINT ( 'NONE',  ( 10.81189881249999729, 0.000000000000000000, -174.0312500020484094 ) ) ;
#22962 = CARTESIAN_POINT ( 'NONE',  ( -10.00000000000000000, -5.773502691896251982, -40.50000000409675494 ) ) ;
#22963 =( BOUNDED_CURVE ( )  B_SPLINE_CURVE ( 2, ( #9345, #16009, #9763, #39748, #23368, #29204, #12776 ),
 .UNSPECIFIED., .F., .F. ) 
 B_SPLINE_CURVE_WITH_KNOTS ( ( 3, 2, 2, 3 ),
 ( 0.7686567164179105571, 0.7699004975124379424, 0.7711442786069654387, 0.7723880597014927130 ),
 .UNSPECIFIED. ) 
 CURVE ( )  GEOMETRIC_REPRESENTATION_ITEM ( )  RATIONAL_B_SPLINE_CURVE ( ( 0.9999999999999880096, 0.8660254037844506980, 1.000000000000000000, 0.8660254037844387076, 1.000000000000000000, 0.8660254037844148378, 1.000000000000023981 ) ) 
 REPRESENTATION_ITEM ( '' )  );
#22964 = CYLINDRICAL_SURFACE ( 'NONE', #33186, 9.999999999999998224 ) ;
#22965 = CARTESIAN_POINT ( 'NONE',  ( -5.405949406250003975, -9.363379034771801557, -63.53125000204837391 ) ) ;
#22966 = CARTESIAN_POINT ( 'NONE',  ( 5.000000000000000000, 8.660254037844385522, -156.2500000000000000 ) ) ;
#22967 = CARTESIAN_POINT ( 'NONE',  ( -10.81189881249999729, 1.324075727343319199E-15, -159.7812500020484094 ) ) ;
#22968 = CARTESIAN_POINT ( 'NONE',  ( -10.81189881249999907, -6.242252689847864744, -139.9687500020483810 ) ) ;
#22969 = CARTESIAN_POINT ( 'NONE',  ( 0.000000000000000000, 0.000000000000000000, -200.0000000000000000 ) ) ;
#22970 = CARTESIAN_POINT ( 'NONE',  ( -4.999999999999996447, 8.660254037844387298, -174.0000000000000284 ) ) ;
#22971 = EDGE_LOOP ( 'NONE', ( #9746, #20732, #38847, #18564 ) ) ;
#22972 = CARTESIAN_POINT ( 'NONE',  ( -7.959047257566134870E-15, -125.0000000000000000, 2.499999999999992006 ) ) ;
#22974 = ORIENTED_EDGE ( 'NONE', *, *, #6438, .T. ) ;
#22973 = CARTESIAN_POINT ( 'NONE',  ( -10.81189881249999729, 6.242252689847871849, -68.40625000204840944 ) ) ;
#22975 = DATE_AND_TIME ( #33332, #19368 ) ;
#22977 = VERTEX_POINT ( 'NONE', #6581 ) ;
#22976 = CARTESIAN_POINT ( 'NONE',  ( 5.405949406249992428, -9.363379034771808662, -117.0937500020483810 ) ) ;
#22978 = VERTEX_POINT ( 'NONE', #3564 ) ;
#22979 = CARTESIAN_POINT ( 'NONE',  ( -2.293366432827344421E-15, -12.48450537969573659, -21.21875000204837036 ) ) ;
#22980 = CARTESIAN_POINT ( 'NONE',  ( -5.405949406249996869, 9.363379034771805109, -198.8437500020484094 ) ) ;
#22981 = CARTESIAN_POINT ( 'NONE',  ( -10.81189881249999907, -6.242252689847864744, -49.96875000204835970 ) ) ;
#22982 = CARTESIAN_POINT ( 'NONE',  ( 10.00000000000076916, -5.773502691895816774, -112.0000000040967620 ) ) ;
#22983 = CARTESIAN_POINT ( 'NONE',  ( 5.000000000000000000, 8.660254037844385522, -31.74999999999997158 ) ) ;
#22984 = CARTESIAN_POINT ( 'NONE',  ( -5.405949406249996869, 9.363379034771805109, -177.8437500020483810 ) ) ;
#22985 = CARTESIAN_POINT ( 'NONE',  ( -10.81189881249999729, 6.242252689847871849, -168.7187500020483810 ) ) ;
#22986 = CARTESIAN_POINT ( 'NONE',  ( 10.81189881249999551, -6.242252689847874514, -148.4687500020484094 ) ) ;
#22987 = CARTESIAN_POINT ( 'NONE',  ( 5.405949406249999534, 9.363379034771803333, -164.5937500020484094 ) ) ;
#22988 = CARTESIAN_POINT ( 'NONE',  ( -4.999999999999996447, 8.660254037844387298, -187.8750000040967905 ) ) ;
#22989 = CARTESIAN_POINT ( 'NONE',  ( 4.999999999999992006, -8.660254037844389075, -191.2500000000000000 ) ) ;
#22990 = CARTESIAN_POINT ( 'NONE',  ( -10.81189881249999729, 6.242252689847871849, -95.21875000204838102 ) ) ;
#22991 = DIRECTION ( 'NONE',  ( -0.000000000000000000, -0.000000000000000000, 1.000000000000000000 ) ) ;
#22992 = CARTESIAN_POINT ( 'NONE',  ( 5.405949406249999534, 9.363379034771803333, -71.78125000204838102 ) ) ;
#22993 = CARTESIAN_POINT ( 'NONE',  ( 5.000000000000000000, 8.660254037844385522, -89.12500000409677625 ) ) ;
#22994 = ADVANCED_FACE ( 'NONE', ( #126 ), #33770, .T. ) ;
#22995 = CARTESIAN_POINT ( 'NONE',  ( -5.405949406249996869, 9.363379034771805109, -189.8437500020483810 ) ) ;
#22996 = CARTESIAN_POINT ( 'NONE',  ( -2.293366432827344421E-15, -12.48450537969573659, -162.4062500020483810 ) ) ;
#22997 = EDGE_CURVE ( 'NONE', #33637, #17527, #16698, .T. ) ;
#22998 = CARTESIAN_POINT ( 'NONE',  ( -5.405949406250003975, -9.363379034771801557, -59.03125000204836681 ) ) ;
#22999 = CARTESIAN_POINT ( 'NONE',  ( 7.070501591499377789E-16, 11.54700538379251284, -141.5000000040967905 ) ) ;
#23000 = CARTESIAN_POINT ( 'NONE',  ( 4.999999999999992006, -8.660254037844389075, -117.7500000000000000 ) ) ;
#23001 =( BOUNDED_CURVE ( )  B_SPLINE_CURVE ( 2, ( #14081, #7425, #14734, #1604, #23840, #27496, #27280 ),
 .UNSPECIFIED., .F., .F. ) 
 B_SPLINE_CURVE_WITH_KNOTS ( ( 3, 2, 2, 3 ),
 ( 0.3582089552238806873, 0.3594527363184080726, 0.3606965174129355134, 0.3619402985074628432 ),
 .UNSPECIFIED. ) 
 CURVE ( )  GEOMETRIC_REPRESENTATION_ITEM ( )  RATIONAL_B_SPLINE_CURVE ( ( 0.9999999999999880096, 0.8660254037844506980, 1.000000000000000000, 0.8660254037844387076, 1.000000000000000000, 0.8660254037844207220, 1.000000000000017986 ) ) 
 REPRESENTATION_ITEM ( '' )  );
#23002 = ORIENTED_EDGE ( 'NONE', *, *, #38238, .F. ) ;
#23003 = CARTESIAN_POINT ( 'NONE',  ( -2.293366432827344421E-15, -12.48450537969573659, -142.9062500020484094 ) ) ;
#23004 = CARTESIAN_POINT ( 'NONE',  ( 10.81189881249999729, 0.000000000000000000, -154.5312500020484094 ) ) ;
#23005 = CARTESIAN_POINT ( 'NONE',  ( 7.644554776091147741E-16, 12.48450537969573659, -197.6562500020484379 ) ) ;
#23006 = CARTESIAN_POINT ( 'NONE',  ( -2.121150477449813534E-15, -11.54700538379251284, -43.25000000409675494 ) ) ;
#23007 = CARTESIAN_POINT ( 'NONE',  ( -10.81189881249999729, 6.242252689847871849, -92.21875000204838102 ) ) ;
#23008 = EDGE_LOOP ( 'NONE', ( #40568, #24581, #16399, #29141 ) ) ;
#23009 = CARTESIAN_POINT ( 'NONE',  ( -2.121150477449813534E-15, -11.54700538379251284, -59.37500000000000000 ) ) ;
#23010 = CARTESIAN_POINT ( 'NONE',  ( -5.405949406250003975, -9.363379034771801557, -192.3437500020484094 ) ) ;
#23011 = CARTESIAN_POINT ( 'NONE',  ( -9.999999999999998224, 5.773502691896259087, -69.25000000409677625 ) ) ;
#23012 = CARTESIAN_POINT ( 'NONE',  ( -9.999999999999998224, 1.224646799147353059E-15, -169.6250000040967905 ) ) ;
#23013 = CARTESIAN_POINT ( 'NONE',  ( -9.999999999999998224, 1.224646799147353059E-15, -145.2500000000000000 ) ) ;
#23014 = CARTESIAN_POINT ( 'NONE',  ( 7.644554776091147741E-16, 12.48450537969573659, -88.15625000204838102 ) ) ;
#23015 = CARTESIAN_POINT ( 'NONE',  ( -10.81189881249999729, 6.242252689847871849, -69.90625000204839523 ) ) ;
#23016 = CARTESIAN_POINT ( 'NONE',  ( -4.999999999999996447, 8.660254037844387298, -63.37500000409676204 ) ) ;
#23017 = CARTESIAN_POINT ( 'NONE',  ( 5.405949406249999534, 9.363379034771803333, -16.09375000204835260 ) ) ;
#23018 = DIRECTION ( 'NONE',  ( 1.000000000000000000, 0.000000000000000000, 0.000000000000000000 ) ) ;
#23019 = CARTESIAN_POINT ( 'NONE',  ( 10.81189881249999551, -6.242252689847874514, -186.1562500020484379 ) ) ;
#23020 = CARTESIAN_POINT ( 'NONE',  ( 7.644554776091147741E-16, 12.48450537969573659, -8.656250002048365033 ) ) ;
#23021 = CARTESIAN_POINT ( 'NONE',  ( 0.000000000000000000, 0.000000000000000000, -99.99999999999998579 ) ) ;
#23022 = CARTESIAN_POINT ( 'NONE',  ( -5.000000000000003553, -8.660254037844383745, -118.0000000000000000 ) ) ;
#23023 = CARTESIAN_POINT ( 'NONE',  ( -8.675003188131697129, -4.974413003141672895, -0.0003472602639886801512 ) ) ;
#23024 = CARTESIAN_POINT ( 'NONE',  ( 0.000000000000000000, 0.000000000000000000, -220.0000000000000000 ) ) ;
#23025 = CARTESIAN_POINT ( 'NONE',  ( -9.999999999999998224, 1.224646799147353059E-15, -166.2500000000000000 ) ) ;
#23026 = CARTESIAN_POINT ( 'NONE',  ( 9.999999999999998224, 0.000000000000000000, -97.99999999999998579 ) ) ;
#23028 = VERTEX_POINT ( 'NONE', #26859 ) ;
#23027 = CARTESIAN_POINT ( 'NONE',  ( -5.405949406249996869, 9.363379034771805109, -92.53125000204838102 ) ) ;
#23029 = CARTESIAN_POINT ( 'NONE',  ( -2.121150477449813534E-15, -11.54700538379251284, -160.2500000040967620 ) ) ;
#23031 = ORIENTED_EDGE ( 'NONE', *, *, #22141, .F. ) ;
#23030 = CARTESIAN_POINT ( 'NONE',  ( 10.00000000000038369, -5.773502691896038819, -153.6250000000000284 ) ) ;
#23032 = VERTEX_POINT ( 'NONE', #27285 ) ;
#23033 = CARTESIAN_POINT ( 'NONE',  ( 7.644554776091147741E-16, 12.48450537969573659, -30.96875000204835260 ) ) ;
#23034 = CARTESIAN_POINT ( 'NONE',  ( 7.644554776091147741E-16, 12.48450537969573659, -23.65625000204838102 ) ) ;
#23035 = CARTESIAN_POINT ( 'NONE',  ( 7.644554776091147741E-16, 12.48450537969573659, -74.46875000204838102 ) ) ;
#23036 = FACE_OUTER_BOUND ( 'NONE', #18891, .T. ) ;
#23037 = CARTESIAN_POINT ( 'NONE',  ( 7.644554776091147741E-16, 12.48450537969573659, -191.4687500020484094 ) ) ;
#23038 = CARTESIAN_POINT ( 'NONE',  ( 0.000000000000000000, 0.000000000000000000, -200.0000000000000000 ) ) ;
#23039 = CARTESIAN_POINT ( 'NONE',  ( -5.405949406250003975, -9.363379034771801557, -153.5312500020484094 ) ) ;
#23040 = CARTESIAN_POINT ( 'NONE',  ( -9.999999999999998224, 5.773502691896259087, -1.750000004096752049 ) ) ;
#23041 = CARTESIAN_POINT ( 'NONE',  ( 5.000000000000000000, 8.660254037844385522, -50.12500000409675494 ) ) ;
#23042 = CARTESIAN_POINT ( 'NONE',  ( 10.81189881249999729, 0.000000000000000000, -122.8437500020483952 ) ) ;
#23043 = CARTESIAN_POINT ( 'NONE',  ( -5.405949406250003975, -9.363379034771801557, -98.03125000204839523 ) ) ;
#23044 = EDGE_CURVE ( 'NONE', #29057, #5036, #34741, .T. ) ;
#23045 = CARTESIAN_POINT ( 'NONE',  ( -5.405949406249996869, 9.363379034771805109, -108.8437500020483810 ) ) ;
#23046 = CARTESIAN_POINT ( 'NONE',  ( 10.81189881249999907, 6.242252689847868297, -80.71875000204838102 ) ) ;
#23047 = CARTESIAN_POINT ( 'NONE',  ( -10.81189881249999907, -6.242252689847864744, -86.15625000204836681 ) ) ;
#23048 = CARTESIAN_POINT ( 'NONE',  ( -2.121150477449813534E-15, -11.54700538379251284, -163.2500000040967620 ) ) ;
#23049 = EDGE_CURVE ( 'NONE', #17267, #34592, #10753, .T. ) ;
#23050 = CARTESIAN_POINT ( 'NONE',  ( -5.000000000000003553, -8.660254037844383745, -66.99999999999997158 ) ) ;
#23051 = CARTESIAN_POINT ( 'NONE',  ( 5.405949406249999534, 9.363379034771803333, -164.7812500020484094 ) ) ;
#23052 = CARTESIAN_POINT ( 'NONE',  ( -10.81189881249999729, 1.324075727343319199E-15, -180.7812500020484094 ) ) ;
#23053 = ADVANCED_FACE ( 'NONE', ( #40421 ), #30109, .T. ) ;
#23054 = CARTESIAN_POINT ( 'NONE',  ( 4.999999999999992006, -8.660254037844389075, -155.6250000040967905 ) ) ;
#23055 = CYLINDRICAL_SURFACE ( 'NONE', #19444, 9.999999999999998224 ) ;
#23056 = CARTESIAN_POINT ( 'NONE',  ( -5.405949406249996869, 9.363379034771805109, -3.843750002048368586 ) ) ;
#23057 = CARTESIAN_POINT ( 'NONE',  ( -5.000000000000003553, -8.660254037844383745, -149.5000000000000000 ) ) ;
#23058 = CARTESIAN_POINT ( 'NONE',  ( -10.81189881249999729, 6.242252689847871849, -114.7187500020483810 ) ) ;
#23059 = CARTESIAN_POINT ( 'NONE',  ( 10.00000000000000000, 5.773502691896255534, -78.37499999999998579 ) ) ;
#23060 = CARTESIAN_POINT ( 'NONE',  ( 10.81189881249999907, 6.242252689847868297, -14.90625000204837036 ) ) ;
#23061 = CARTESIAN_POINT ( 'NONE',  ( -2.121150477449813534E-15, -11.54700538379251284, -89.75000000409677625 ) ) ;
#23062 = CARTESIAN_POINT ( 'NONE',  ( 0.000000000000000000, 0.000000000000000000, -160.0000000000000000 ) ) ;
#23063 = CC_DESIGN_PERSON_AND_ORGANIZATION_ASSIGNMENT ( #33234, #23722, ( #10757 ) ) ;
#23064 = CARTESIAN_POINT ( 'NONE',  ( -10.81189881249999729, 6.242252689847871849, -111.9062500020483810 ) ) ;
#23065 = CARTESIAN_POINT ( 'NONE',  ( -5.405949406250003975, -9.363379034771801557, -95.03125000204838102 ) ) ;
#23066 = VERTEX_POINT ( 'NONE', #10443 ) ;
#23067 = CARTESIAN_POINT ( 'NONE',  ( -5.000000000000003553, -8.660254037844383745, -80.87500000409677625 ) ) ;
#23068 = CARTESIAN_POINT ( 'NONE',  ( -9.999999999999998224, 1.224646799147353059E-15, -200.0000000000000000 ) ) ;
#23069 = CARTESIAN_POINT ( 'NONE',  ( -5.405949406249996869, 9.363379034771805109, -45.84375000204838102 ) ) ;
#23070 = EDGE_LOOP ( 'NONE', ( #18547, #40557, #31648, #22640 ) ) ;
#23071 = CARTESIAN_POINT ( 'NONE',  ( -4.999999999999996447, 8.660254037844387298, -13.49999999999995737 ) ) ;
#23072 = CARTESIAN_POINT ( 'NONE',  ( 5.000000000000000000, 8.660254037844385522, -148.7500000000000000 ) ) ;
#23073 = CARTESIAN_POINT ( 'NONE',  ( 7.070501591499376803E-16, 11.54700538379251284, -139.6250000000000000 ) ) ;
#23074 = CARTESIAN_POINT ( 'NONE',  ( -9.999999999999998224, 5.773502691896259087, -12.25000000409676204 ) ) ;
#23075 = EDGE_CURVE ( 'NONE', #19091, #11871, #6366, .T. ) ;
#23076 = CARTESIAN_POINT ( 'NONE',  ( -9.999999999999998224, 5.773502691896259087, -190.3750000000000000 ) ) ;
#23078 = EDGE_LOOP ( 'NONE', ( #22869, #3148 ) ) ;
#23077 = CARTESIAN_POINT ( 'NONE',  ( -10.81189881249999729, 1.324075727343319199E-15, -120.7812500020483952 ) ) ;
#23079 = CARTESIAN_POINT ( 'NONE',  ( 9.999999999999998224, 0.000000000000000000, -23.37500000409675849 ) ) ;
#23080 = VERTEX_POINT ( 'NONE', #8078 ) ;
#23081 = CARTESIAN_POINT ( 'NONE',  ( 7.644554776091147741E-16, 12.48450537969573659, -47.65625000204836681 ) ) ;
#23082 = CALENDAR_DATE ( 2026, 28, 9 ) ;
#23083 = CARTESIAN_POINT ( 'NONE',  ( 5.405949406249992428, -9.363379034771808662, -94.59375000204838102 ) ) ;
#23084 = CARTESIAN_POINT ( 'NONE',  ( 5.405949406249999534, 9.363379034771803333, -121.2812500020483952 ) ) ;
#23085 = ORIENTED_EDGE ( 'NONE', *, *, #24107, .F. ) ;
#23086 = CARTESIAN_POINT ( 'NONE',  ( -9.999999999999998224, 1.224646799147353059E-15, -51.12500000409675494 ) ) ;
#23087 = CARTESIAN_POINT ( 'NONE',  ( 0.000000000000000000, 0.000000000000000000, -169.9999999999999716 ) ) ;
#23088 = CARTESIAN_POINT ( 'NONE',  ( -2.293366432827344421E-15, -12.48450537969573659, -178.9062500020484379 ) ) ;
#23089 = CARTESIAN_POINT ( 'NONE',  ( 4.999999999999992006, -8.660254037844389075, -26.24999999999996803 ) ) ;
#23090 = CARTESIAN_POINT ( 'NONE',  ( -9.999999999999998224, 1.224646799147353059E-15, -13.62500000409674961 ) ) ;
#23091 = CARTESIAN_POINT ( 'NONE',  ( 5.405949406249992428, -9.363379034771808662, -129.0937500020483810 ) ) ;
#23092 = CARTESIAN_POINT ( 'NONE',  ( -5.405949406250003975, -9.363379034771801557, -99.34375000204838102 ) ) ;
#23093 = DIRECTION ( 'NONE',  ( -0.000000000000000000, -0.000000000000000000, 1.000000000000000000 ) ) ;
#23094 = CARTESIAN_POINT ( 'NONE',  ( -2.293366432827344421E-15, -12.48450537969573659, -108.4062500020483810 ) ) ;
#23095 = CARTESIAN_POINT ( 'NONE',  ( -2.121150477449813534E-15, -11.54700538379251284, -188.7500000040967905 ) ) ;
#23096 = CARTESIAN_POINT ( 'NONE',  ( 10.81189881249999729, 0.000000000000000000, -115.3437500020483810 ) ) ;
#23097 = CARTESIAN_POINT ( 'NONE',  ( 5.405949406249999534, 9.363379034771803333, -190.2812500020484094 ) ) ;
#23098 = AXIS2_PLACEMENT_3D ( 'NONE', #25255, #38400, #38611 ) ;
#23099 = CARTESIAN_POINT ( 'NONE',  ( 0.000000000000000000, 0.000000000000000000, -200.0000000000000000 ) ) ;
#23100 = DIRECTION ( 'NONE',  ( -0.000000000000000000, -0.000000000000000000, 1.000000000000000000 ) ) ;
#23101 = CARTESIAN_POINT ( 'NONE',  ( 10.00000000000000000, 5.773502691896255534, -142.8750000000000000 ) ) ;
#23102 = CARTESIAN_POINT ( 'NONE',  ( 7.070501591499377789E-16, 11.54700538379251284, -6.124999999999964473 ) ) ;
#23103 = CARTESIAN_POINT ( 'NONE',  ( -10.81189881249999729, 6.242252689847871849, -57.71875000204836681 ) ) ;
#23104 = CARTESIAN_POINT ( 'NONE',  ( -2.293366432827344421E-15, -12.48450537969573659, -46.71875000204835970 ) ) ;
#23105 = CARTESIAN_POINT ( 'NONE',  ( -10.00000000000000000, -5.773502691896251982, -178.5000000040967905 ) ) ;
#23106 = CARTESIAN_POINT ( 'NONE',  ( 7.644554776091147741E-16, 12.48450537969573659, -14.65625000204836859 ) ) ;
#23107 = CARTESIAN_POINT ( 'NONE',  ( -10.81189881249999729, 1.324075727343319199E-15, -33.59375000204836681 ) ) ;
#23108 = CARTESIAN_POINT ( 'NONE',  ( 10.00000000000051159, -5.773502691895965988, -105.6249999999999858 ) ) ;
#23109 = CARTESIAN_POINT ( 'NONE',  ( 10.81189881249999907, 6.242252689847868297, -137.7187500020484094 ) ) ;
#23110 = CARTESIAN_POINT ( 'NONE',  ( 9.999999999999998224, 0.000000000000000000, -103.9999999999999858 ) ) ;
#23111 = CARTESIAN_POINT ( 'NONE',  ( -10.81189881249999729, 6.242252689847871849, -39.90625000204836681 ) ) ;
#23112 = DIRECTION ( 'NONE',  ( -0.000000000000000000, -0.000000000000000000, 1.000000000000000000 ) ) ;
#23113 = CARTESIAN_POINT ( 'NONE',  ( 10.00000000000000000, 5.773502691896255534, -69.37499999999998579 ) ) ;
#23114 = CARTESIAN_POINT ( 'NONE',  ( -5.405949406249996869, 9.363379034771805109, -130.0312500020484094 ) ) ;
#23115 = CARTESIAN_POINT ( 'NONE',  ( 10.81189881249999729, 0.000000000000000000, -117.0312500020483952 ) ) ;
#23116 = VERTEX_POINT ( 'NONE', #11937 ) ;
#23117 = CARTESIAN_POINT ( 'NONE',  ( 10.00000000000000000, 5.773502691896255534, -108.7500000040967905 ) ) ;
#23118 = CARTESIAN_POINT ( 'NONE',  ( 9.999999999999998224, 0.000000000000000000, -194.3750000040967905 ) ) ;
#23119 = CARTESIAN_POINT ( 'NONE',  ( 10.81189881249999551, -6.242252689847874514, -68.96875000204839523 ) ) ;
#23120 = VERTEX_POINT ( 'NONE', #37423 ) ;
#23121 = CARTESIAN_POINT ( 'NONE',  ( -4.999999999999996447, 8.660254037844387298, -37.49999999999997868 ) ) ;
#23122 = ADVANCED_FACE ( 'NONE', ( #17545 ), #34204, .F. ) ;
#23123 = CARTESIAN_POINT ( 'NONE',  ( 4.999999999999992006, -8.660254037844389075, -17.62500000409675138 ) ) ;
#23124 = CARTESIAN_POINT ( 'NONE',  ( 7.644554776091147741E-16, 12.48450537969573659, -43.15625000204837391 ) ) ;
#23125 = LINE ( 'NONE', #13804, #24943 ) ;
#23126 = CARTESIAN_POINT ( 'NONE',  ( -5.000000000000003553, -8.660254037844383745, -37.37500000409676915 ) ) ;
#23127 = CARTESIAN_POINT ( 'NONE',  ( 5.000000000000000000, 8.660254037844385522, -156.6250000040967905 ) ) ;
#23128 = CARTESIAN_POINT ( 'NONE',  ( 5.405949406249992428, -9.363379034771808662, -136.7812500020483810 ) ) ;
#23129 = CARTESIAN_POINT ( 'NONE',  ( 10.81189881249999729, 0.000000000000000000, -139.5312500020484094 ) ) ;
#23130 = AXIS2_PLACEMENT_3D ( 'NONE', #1423, #14556, #30778 ) ;
#23131 = CARTESIAN_POINT ( 'NONE',  ( 9.999999999999998224, 0.000000000000000000, -78.49999999999998579 ) ) ;
#23132 = ORIENTED_EDGE ( 'NONE', *, *, #41755, .T. ) ;
#23133 = EDGE_LOOP ( 'NONE', ( #25263, #31143, #18908, #22235 ) ) ;
#23134 = ORIENTED_EDGE ( 'NONE', *, *, #19567, .F. ) ;
#23135 = CARTESIAN_POINT ( 'NONE',  ( 9.999999999999998224, 0.000000000000000000, -200.0000000000000000 ) ) ;
#23136 = CARTESIAN_POINT ( 'NONE',  ( 5.405949406249992428, -9.363379034771808662, -172.5937500020484094 ) ) ;
#23137 = CARTESIAN_POINT ( 'NONE',  ( 7.644554776091147741E-16, 12.48450537969573659, -21.96875000204837391 ) ) ;
#23138 = DIRECTION ( 'NONE',  ( 1.000000000000000000, 0.000000000000000000, 0.000000000000000000 ) ) ;
#23139 = CARTESIAN_POINT ( 'NONE',  ( 5.405949406249999534, 9.363379034771803333, -158.5937500020483810 ) ) ;
#23140 = CARTESIAN_POINT ( 'NONE',  ( -5.405949406249996869, 9.363379034771805109, -147.8437500020483810 ) ) ;
#23141 = CARTESIAN_POINT ( 'NONE',  ( 4.999999999999992006, -8.660254037844389075, -9.749999999999953815 ) ) ;
#23142 = CARTESIAN_POINT ( 'NONE',  ( 10.81189881249999907, 6.242252689847868297, -122.7187500020483810 ) ) ;
#23143 = AXIS2_PLACEMENT_3D ( 'NONE', #20733, #14456, #34779 ) ;
#23144 = CARTESIAN_POINT ( 'NONE',  ( 10.81189881249999907, 6.242252689847868297, -128.9062500020483810 ) ) ;
#23145 = CARTESIAN_POINT ( 'NONE',  ( -10.81189881249999729, 6.242252689847871849, -15.71875000204835793 ) ) ;
#23146 = CARTESIAN_POINT ( 'NONE',  ( 10.81189881249999729, 0.000000000000000000, -140.8437500020483810 ) ) ;
#23147 = CARTESIAN_POINT ( 'NONE',  ( 0.000000000000000000, 0.000000000000000000, -99.99999999999998579 ) ) ;
#23148 = AXIS2_PLACEMENT_3D ( 'NONE', #48, #35873, #32641 ) ;
#23149 = DIRECTION ( 'NONE',  ( 1.000000000000000000, -3.469446951953614805E-17, 0.000000000000000000 ) ) ;
#23150 = CARTESIAN_POINT ( 'NONE',  ( 9.999999999999998224, 0.000000000000000000, -162.5000000000000000 ) ) ;
#23151 = CARTESIAN_POINT ( 'NONE',  ( 9.999999999999994671, -5.773502691896262640, -167.5000000040967905 ) ) ;
#23152 = CARTESIAN_POINT ( 'NONE',  ( 5.405949406249992428, -9.363379034771808662, -72.09375000204836681 ) ) ;
#23153 = CARTESIAN_POINT ( 'NONE',  ( -2.293366432827344421E-15, -12.48450537969573659, -42.40625000204837391 ) ) ;
#23154 = CARTESIAN_POINT ( 'NONE',  ( 10.81189881249999551, -6.242252689847874514, -52.46875000204837391 ) ) ;
#23155 = CARTESIAN_POINT ( 'NONE',  ( -5.405949406250003975, -9.363379034771801557, -159.3437500020484094 ) ) ;
#23156 = CARTESIAN_POINT ( 'NONE',  ( -4.999999999999996447, 8.660254037844387298, -133.5000000000000000 ) ) ;
#23157 = CARTESIAN_POINT ( 'NONE',  ( -10.81189881249999729, -6.242252689847864744, -135.6562500020484094 ) ) ;
#23158 = CARTESIAN_POINT ( 'NONE',  ( 0.000000000000000000, 0.000000000000000000, -99.99999999999998579 ) ) ;
#23159 = CARTESIAN_POINT ( 'NONE',  ( 4.999999999999992006, -8.660254037844389075, -112.1250000040967763 ) ) ;
#23160 = CARTESIAN_POINT ( 'NONE',  ( 9.999999999999996447, -5.773502691896262640, -92.12499999999998579 ) ) ;
#23161 = ORIENTED_EDGE ( 'NONE', *, *, #13888, .T. ) ;
#23162 = CARTESIAN_POINT ( 'NONE',  ( -10.81189881249999729, 6.242252689847871849, -113.4062500020483952 ) ) ;
#23163 = CARTESIAN_POINT ( 'NONE',  ( 4.999999999999992006, -8.660254037844389075, -128.6250000040967620 ) ) ;
#23164 = CARTESIAN_POINT ( 'NONE',  ( 9.999999999999998224, 0.000000000000000000, -39.49999999999997868 ) ) ;
#23165 = CARTESIAN_POINT ( 'NONE',  ( 7.644554776091147741E-16, 12.48450537969573659, -164.6562500020484094 ) ) ;
#23166 = CARTESIAN_POINT ( 'NONE',  ( 10.00000000000000000, 5.773502691896255534, -45.75000000409676915 ) ) ;
#23167 = CARTESIAN_POINT ( 'NONE',  ( 9.999999999999998224, 0.000000000000000000, -149.3750000040967905 ) ) ;
#23168 = CARTESIAN_POINT ( 'NONE',  ( -2.293366432827344421E-15, -12.48450537969573659, -54.40625000204838102 ) ) ;
#23169 = CARTESIAN_POINT ( 'NONE',  ( -4.999999999999996447, 8.660254037844387298, -100.8750000040967905 ) ) ;
#23170 = CARTESIAN_POINT ( 'NONE',  ( 10.81189881249999729, 0.000000000000000000, -165.0312500020484094 ) ) ;
#23171 = CARTESIAN_POINT ( 'NONE',  ( 5.405949406249999534, 9.363379034771803333, -139.0937500020483810 ) ) ;
#23172 = CARTESIAN_POINT ( 'NONE',  ( -2.121150477449813534E-15, -11.54700538379251284, -50.75000000409676204 ) ) ;
#23173 = CARTESIAN_POINT ( 'NONE',  ( -9.999999999999996447, 5.773502691896259975, -171.2500000040967905 ) ) ;
#23174 = ORIENTED_EDGE ( 'NONE', *, *, #4812, .F. ) ;
#23175 = CARTESIAN_POINT ( 'NONE',  ( -5.000000000000003553, -8.660254037844383745, -78.99999999999998579 ) ) ;
#23176 = VECTOR ( 'NONE', #42282, 1000.000000000000000 ) ;
#23177 = EDGE_CURVE ( 'NONE', #28563, #4341, #1969, .T. ) ;
#23178 = B_SPLINE_CURVE_WITH_KNOTS ( 'NONE', 3,
 ( #32447, #8923, #38696, #5897, #5256, #25962 ),
 .UNSPECIFIED., .F., .F.,
 ( 4, 2, 4 ),
 ( 0.000000000000000000, 0.004265001810245392516, 0.008530003620490783298 ),
 .UNSPECIFIED. ) ;
#23180 = VERTEX_POINT ( 'NONE', #14300 ) ;
#23179 = CARTESIAN_POINT ( 'NONE',  ( -2.293366432827344421E-15, -12.48450537969573659, -73.90625000204836681 ) ) ;
#23181 = APPLICATION_PROTOCOL_DEFINITION ( 'international standard', 'config_control_design', 1994, #9654 ) ;
#23183 = ORIENTED_EDGE ( 'NONE', *, *, #30657, .F. ) ;
#23182 = CARTESIAN_POINT ( 'NONE',  ( -2.293366432827344421E-15, -12.48450537969573659, -120.2187500020483952 ) ) ;
#23184 = ORIENTED_EDGE ( 'NONE', *, *, #36231, .F. ) ;
#23185 = CARTESIAN_POINT ( 'NONE',  ( 10.81189881249999729, 6.242252689847867408, -22.21875000204837747 ) ) ;
#23186 = CARTESIAN_POINT ( 'NONE',  ( 10.81189881249999551, -6.242252689847874514, -196.4687500020484094 ) ) ;
#23187 = CARTESIAN_POINT ( 'NONE',  ( -10.81189881249999729, 6.242252689847871849, -44.21875000204836681 ) ) ;
#23188 = CARTESIAN_POINT ( 'NONE',  ( 9.999999999999994671, -5.773502691896262640, -134.1250000000000000 ) ) ;
#23189 = CARTESIAN_POINT ( 'NONE',  ( -4.999999999999996447, 8.660254037844387298, -25.49999999999996803 ) ) ;
#23190 = CARTESIAN_POINT ( 'NONE',  ( -5.405949406250003975, -9.363379034771801557, -178.8437500020483810 ) ) ;
#23191 = CARTESIAN_POINT ( 'NONE',  ( -10.81189881249999907, -6.242252689847864744, -165.4687500020484094 ) ) ;
#23192 = CARTESIAN_POINT ( 'NONE',  ( -10.81189881249999729, 6.242252689847871849, -149.2187500020484379 ) ) ;
#23193 = EDGE_CURVE ( 'NONE', #10633, #36222, #3337, .T. ) ;
#23194 = CARTESIAN_POINT ( 'NONE',  ( -10.81189881249999729, 1.324075727343319199E-15, -161.0937500020484094 ) ) ;
#23195 = CARTESIAN_POINT ( 'NONE',  ( -9.999999999999998224, 0.000000000000000000, -99.99999999999998579 ) ) ;
#23196 = CARTESIAN_POINT ( 'NONE',  ( 9.999999999998969713, 5.773502691896851502, -102.7500000040967620 ) ) ;
#23197 = CARTESIAN_POINT ( 'NONE',  ( 4.999999999999992006, -8.660254037844389075, -186.7500000000000000 ) ) ;
#23198 = CARTESIAN_POINT ( 'NONE',  ( 7.644554776091147741E-16, 12.48450537969573659, -99.96875000204839523 ) ) ;
#23199 = EDGE_CURVE ( 'NONE', #26946, #21791, #2232, .T. ) ;
#23200 = CARTESIAN_POINT ( 'NONE',  ( -2.121150477449813534E-15, -11.54700538379251284, -101.3750000000000000 ) ) ;
#23201 = CARTESIAN_POINT ( 'NONE',  ( 10.81189881249999729, 0.000000000000000000, -63.03125000204837391 ) ) ;
#23202 = CARTESIAN_POINT ( 'NONE',  ( 0.000000000000000000, 0.000000000000000000, -99.99999999999998579 ) ) ;
#23203 = CARTESIAN_POINT ( 'NONE',  ( -2.293366432827344421E-15, -12.48450537969573659, -187.7187500020484094 ) ) ;
#23204 = CARTESIAN_POINT ( 'NONE',  ( 5.405949406249999534, 9.363379034771803333, -119.7812500020483952 ) ) ;
#23205 = CARTESIAN_POINT ( 'NONE',  ( 10.81189881249999551, -6.242252689847874514, -163.6562500020484094 ) ) ;
#23206 =( BOUNDED_CURVE ( )  B_SPLINE_CURVE ( 2, ( #27643, #40151, #33492, #21155, #898, #27860, #34128 ),
 .UNSPECIFIED., .F., .F. ) 
 B_SPLINE_CURVE_WITH_KNOTS ( ( 3, 2, 2, 3 ),
 ( 0.1194029850746269744, 0.1206467661691543042, 0.1218905472636816062, 0.1231343283582089221 ),
 .UNSPECIFIED. ) 
 CURVE ( )  GEOMETRIC_REPRESENTATION_ITEM ( )  RATIONAL_B_SPLINE_CURVE ( ( 0.9999999999999880096, 0.8660254037844506980, 1.000000000000000000, 0.8660254037844387076, 1.000000000000000000, 0.8660254037844417052, 0.9999999999999970024 ) ) 
 REPRESENTATION_ITEM ( '' )  );
#23207 = CARTESIAN_POINT ( 'NONE',  ( -10.81189881249999729, 1.324075727343319199E-15, -50.28125000204835970 ) ) ;
#23208 = CARTESIAN_POINT ( 'NONE',  ( -5.000000000000003553, -8.660254037844383745, -140.8750000040967905 ) ) ;
#23209 = CARTESIAN_POINT ( 'NONE',  ( -9.999999999999998224, 1.224646799147353059E-15, -116.7499999999999858 ) ) ;
#23210 = VERTEX_POINT ( 'NONE', #18199 ) ;
#23211 = CARTESIAN_POINT ( 'NONE',  ( -10.81189881249999729, 6.242252689847871849, -131.4062500020483810 ) ) ;
#23212 = CC_DESIGN_SECURITY_CLASSIFICATION ( #16278, ( #42695 ) ) ;
#23213 = CARTESIAN_POINT ( 'NONE',  ( 10.81189881249999907, 6.242252689847868297, -145.4062500020484094 ) ) ;
#23214 = CARTESIAN_POINT ( 'NONE',  ( 5.405949406249999534, 9.363379034771803333, -199.2812500020484094 ) ) ;
#23215 = CARTESIAN_POINT ( 'NONE',  ( 10.00000000000051159, -5.773502691895965988, -43.00000000409674072 ) ) ;
#23216 = CARTESIAN_POINT ( 'NONE',  ( 7.644554776091147741E-16, 12.48450537969573659, -81.96875000204839523 ) ) ;
#23217 = ORIENTED_EDGE ( 'NONE', *, *, #40022, .T. ) ;
#23218 = CARTESIAN_POINT ( 'NONE',  ( 10.00000000000000000, 5.773502691896255534, -55.87499999999997158 ) ) ;
#23219 = CARTESIAN_POINT ( 'NONE',  ( 10.81189881249999551, -6.242252689847874514, -187.4687500020484094 ) ) ;
#23220 = CARTESIAN_POINT ( 'NONE',  ( -4.999999999999996447, 8.660254037844387298, -66.37500000409676204 ) ) ;
#23221 = FACE_OUTER_BOUND ( 'NONE', #8173, .T. ) ;
#23222 = CARTESIAN_POINT ( 'NONE',  ( -10.00000000000051337, 5.773502691895962435, -139.7500000040967905 ) ) ;
#23223 = CARTESIAN_POINT ( 'NONE',  ( 10.81189881249999729, 0.000000000000000000, -84.03125000204838102 ) ) ;
#23224 = CARTESIAN_POINT ( 'NONE',  ( -10.81189881249999729, -6.242252689847864744, -59.15625000204838813 ) ) ;
#23225 = CARTESIAN_POINT ( 'NONE',  ( -5.000000000000003553, -8.660254037844383745, -61.37500000409676204 ) ) ;
#23226 = CARTESIAN_POINT ( 'NONE',  ( -5.405949406250003975, -9.363379034771801557, -21.34375000204835615 ) ) ;
#23227 = CARTESIAN_POINT ( 'NONE',  ( 0.000000000000000000, 0.000000000000000000, -200.0000000000000000 ) ) ;
#23228 = CARTESIAN_POINT ( 'NONE',  ( -5.405949406249996869, 9.363379034771805109, -182.5312500020484094 ) ) ;
#23229 = CARTESIAN_POINT ( 'NONE',  ( 10.81189881249999729, 0.000000000000000000, -10.53125000204835260 ) ) ;
#23230 = CARTESIAN_POINT ( 'NONE',  ( 6.964452268037472749, 6.964452268037473637, -201.2186212422413689 ) ) ;
#23231 = CARTESIAN_POINT ( 'NONE',  ( -9.999999999999998224, 1.224646799147353059E-15, -175.6250000040968189 ) ) ;
#23232 = DIRECTION ( 'NONE',  ( -1.734723475976806848E-16, 1.000000000000000000, 0.000000000000000000 ) ) ;
#23233 = CARTESIAN_POINT ( 'NONE',  ( -6.454000741078234960, 7.688134883229009731, -0.000000000000000000 ) ) ;
#23234 = CARTESIAN_POINT ( 'NONE',  ( 4.999999999999992006, -8.660254037844389075, -170.2500000000000000 ) ) ;
#23235 = CARTESIAN_POINT ( 'NONE',  ( -5.000000000000003553, -8.660254037844383745, -137.8750000040967905 ) ) ;
#23237 = ORIENTED_EDGE ( 'NONE', *, *, #3528, .T. ) ;
#23236 = CARTESIAN_POINT ( 'NONE',  ( -10.81189881249999907, -6.242252689847864744, -95.15625000204839523 ) ) ;
#23238 = ADVANCED_FACE ( 'NONE', ( #21442 ), #1608, .T. ) ;
#23240 = ORIENTED_EDGE ( 'NONE', *, *, #32291, .F. ) ;
#23239 = CARTESIAN_POINT ( 'NONE',  ( 10.81189881249999729, 0.000000000000000000, -101.8437500020483810 ) ) ;
#23241 = EDGE_LOOP ( 'NONE', ( #39180, #41850, #28026, #34454 ) ) ;
#23242 = CARTESIAN_POINT ( 'NONE',  ( 7.644554776091147741E-16, 12.48450537969573659, -36.96875000204835970 ) ) ;
#23243 = CARTESIAN_POINT ( 'NONE',  ( 10.81189881249999729, 0.000000000000000000, -25.53125000204836681 ) ) ;
#23244 = APPROVAL_STATUS ( 'not_yet_approved' ) ;
#23245 = CARTESIAN_POINT ( 'NONE',  ( 7.644554776091147741E-16, 12.48450537969573659, -69.96875000204838102 ) ) ;
#23246 = CARTESIAN_POINT ( 'NONE',  ( 10.00000000000051159, -5.773502691895965988, -115.0000000040967905 ) ) ;
#23247 = CARTESIAN_POINT ( 'NONE',  ( -5.405949406249996869, 9.363379034771805109, -194.3437500020484094 ) ) ;
#23248 = CARTESIAN_POINT ( 'NONE',  ( 10.81189881249999729, 0.000000000000000000, -152.8437500020483810 ) ) ;
#23249 =( BOUNDED_CURVE ( )  B_SPLINE_CURVE ( 2, ( #4142, #33717, #1340, #8030, #27663, #34364, #21174 ),
 .UNSPECIFIED., .F., .F. ) 
 B_SPLINE_CURVE_WITH_KNOTS ( ( 3, 2, 2, 3 ),
 ( 0.1604477611940298698, 0.1616915422885572551, 0.1629353233830845848, 0.1641791044776119424 ),
 .UNSPECIFIED. ) 
 CURVE ( )  GEOMETRIC_REPRESENTATION_ITEM ( )  RATIONAL_B_SPLINE_CURVE ( ( 0.9999999999999970024, 0.8660254037844417052, 1.000000000000000000, 0.8660254037844387076, 1.000000000000000000, 0.8660254037844387076, 1.000000000000000000 ) ) 
 REPRESENTATION_ITEM ( '' )  );
#23250 = CARTESIAN_POINT ( 'NONE',  ( -24.99999999999999645, 0.000000000000000000, -103.0000000000000000 ) ) ;
#23251 = CARTESIAN_POINT ( 'NONE',  ( 9.999999999999998224, 1.224646799147353059E-15, -99.99999999999998579 ) ) ;
#23252 = CARTESIAN_POINT ( 'NONE',  ( -10.81189881249999729, 1.324075727343319199E-15, -149.2812500020483810 ) ) ;
#23253 = CARTESIAN_POINT ( 'NONE',  ( -9.999999999999998224, 1.224646799147353059E-15, -6.125000004096770034 ) ) ;
#23254 = CARTESIAN_POINT ( 'NONE',  ( 0.000000000000000000, 0.000000000000000000, -200.0000000000000000 ) ) ;
#23255 = CARTESIAN_POINT ( 'NONE',  ( -10.81189881249999729, 1.324075727343319199E-15, -117.5937500020483810 ) ) ;
#23256 = CARTESIAN_POINT ( 'NONE',  ( 5.405949406249992428, -9.363379034771808662, -87.28125000204838102 ) ) ;
#23257 = CARTESIAN_POINT ( 'NONE',  ( 10.81189881249999729, 6.242252689847867408, -110.7187500020483810 ) ) ;
#23258 = CARTESIAN_POINT ( 'NONE',  ( -5.405949406250003975, -9.363379034771801557, -67.84375000204836681 ) ) ;
#23259 = CARTESIAN_POINT ( 'NONE',  ( -10.81189881249999907, -6.242252689847864744, -81.65625000204839523 ) ) ;
#23260 = CARTESIAN_POINT ( 'NONE',  ( 5.000000000000000000, 8.660254037844385522, -161.1250000040967905 ) ) ;
#23261 =( BOUNDED_CURVE ( )  B_SPLINE_CURVE ( 2, ( #30740, #30951, #8498, #14513, #21651, #14078, #27276 ),
 .UNSPECIFIED., .F., .F. ) 
 B_SPLINE_CURVE_WITH_KNOTS ( ( 3, 2, 2, 3 ),
 ( 0.1044776119402986148, 0.1057213930348259306, 0.1069651741293532465, 0.1082089552238805485 ),
 .UNSPECIFIED. ) 
 CURVE ( )  GEOMETRIC_REPRESENTATION_ITEM ( )  RATIONAL_B_SPLINE_CURVE ( ( 0.9999999999999880096, 0.8660254037844506980, 1.000000000000000000, 0.8660254037844387076, 1.000000000000000000, 0.8660254037844431485, 0.9999999999999955591 ) ) 
 REPRESENTATION_ITEM ( '' )  );
#23262 = DIRECTION ( 'NONE',  ( -0.000000000000000000, -0.000000000000000000, -1.000000000000000000 ) ) ;
#23263 = CARTESIAN_POINT ( 'NONE',  ( 5.405949406249992428, -9.363379034771808662, -166.7812500020484094 ) ) ;
#23264 = CARTESIAN_POINT ( 'NONE',  ( 5.405949406249992428, -9.363379034771808662, -181.7812500020483810 ) ) ;
#23265 = CARTESIAN_POINT ( 'NONE',  ( -9.999999999999998224, 1.224646799147353059E-15, -190.2500000000000000 ) ) ;
#23266 = CARTESIAN_POINT ( 'NONE',  ( -5.405949406250003975, -9.363379034771801557, -3.343750002048367698 ) ) ;
#23267 = CARTESIAN_POINT ( 'NONE',  ( 4.999999999999992006, -8.660254037844389075, -149.2500000000000000 ) ) ;
#23268 = CARTESIAN_POINT ( 'NONE',  ( -10.81189881249999907, -6.242252689847864744, -114.4687500020483810 ) ) ;
#23269 = CARTESIAN_POINT ( 'NONE',  ( -9.999999999999998224, 5.773502691896259087, -80.87499999999998579 ) ) ;
#23270 = CARTESIAN_POINT ( 'NONE',  ( 7.644554776091147741E-16, 12.48450537969573659, -11.65625000204836859 ) ) ;
#23271 = CARTESIAN_POINT ( 'NONE',  ( 7.070501591499377789E-16, 11.54700538379251284, -92.00000000409677625 ) ) ;
#23272 = DIRECTION ( 'NONE',  ( -0.000000000000000000, -0.000000000000000000, 1.000000000000000000 ) ) ;
#23273 = CARTESIAN_POINT ( 'NONE',  ( -10.81189881249999729, 1.324075727343319199E-15, -108.7812500020483810 ) ) ;
#23274 = CARTESIAN_POINT ( 'NONE',  ( 10.81189881249999729, 0.000000000000000000, -84.03125000204838102 ) ) ;
#23275 = ORIENTED_EDGE ( 'NONE', *, *, #1854, .F. ) ;
#23276 = CARTESIAN_POINT ( 'NONE',  ( 7.070501591499377789E-16, 11.54700538379251284, -86.00000000409676204 ) ) ;
#23277 = CARTESIAN_POINT ( 'NONE',  ( -2.121150477449813534E-15, -11.54700538379251284, -140.7500000040967905 ) ) ;
#23278 = CARTESIAN_POINT ( 'NONE',  ( -10.81189881249999729, 6.242252689847871849, -45.71875000204836681 ) ) ;
#23279 = ORIENTED_EDGE ( 'NONE', *, *, #19372, .T. ) ;
#23280 = CARTESIAN_POINT ( 'NONE',  ( 9.999999999999996447, -5.773502691896262640, -9.624999999999982236 ) ) ;
#23281 = CARTESIAN_POINT ( 'NONE',  ( 7.070501591499377789E-16, 11.54700538379251284, -145.6250000000000284 ) ) ;
#23282 = CARTESIAN_POINT ( 'NONE',  ( 9.999999999999998224, 0.000000000000000000, -96.87500000409677625 ) ) ;
#23283 = CARTESIAN_POINT ( 'NONE',  ( -2.121150477449813534E-15, -11.54700538379251284, -14.75000000409676382 ) ) ;
#23284 = CARTESIAN_POINT ( 'NONE',  ( -2.121150477449813534E-15, -11.54700538379251284, -191.3750000000000284 ) ) ;
#23285 = DIRECTION ( 'NONE',  ( 1.000000000000000000, 0.000000000000000000, 0.000000000000000000 ) ) ;
#23287 = ORIENTED_EDGE ( 'NONE', *, *, #26750, .T. ) ;
#23286 = CARTESIAN_POINT ( 'NONE',  ( 5.405949406249999534, 9.363379034771803333, -115.2812500020483952 ) ) ;
#23288 = CARTESIAN_POINT ( 'NONE',  ( 9.999999999999998224, 1.224646799147353059E-15, -99.99999999999998579 ) ) ;
#23289 = EDGE_CURVE ( 'NONE', #36923, #12994, #7866, .T. ) ;
#23290 = AXIS2_PLACEMENT_3D ( 'NONE', #16687, #13236, #26637 ) ;
#23291 = EDGE_CURVE ( 'NONE', #23881, #33268, #32849, .T. ) ;
#23292 = ORIENTED_EDGE ( 'NONE', *, *, #19687, .T. ) ;
#23293 = EDGE_CURVE ( 'NONE', #13652, #4202, #14522, .T. ) ;
#23294 = CARTESIAN_POINT ( 'NONE',  ( 10.81189881249999551, -6.242252689847874514, -49.65625000204837391 ) ) ;
#23295 = APPROVAL_STATUS ( 'not_yet_approved' ) ;
#23296 = CARTESIAN_POINT ( 'NONE',  ( -10.81189881249999907, -6.242252689847864744, -93.46875000204836681 ) ) ;
#23297 = CARTESIAN_POINT ( 'NONE',  ( 7.644554776091147741E-16, 12.48450537969573659, -122.6562500020483952 ) ) ;
#23298 = ORIENTED_EDGE ( 'NONE', *, *, #42648, .F. ) ;
#23299 = CARTESIAN_POINT ( 'NONE',  ( -5.000000000000003553, -8.660254037844383745, -111.9999999999999858 ) ) ;
#23300 = APPROVAL ( #34077, 'UNSPECIFIED' ) ;
#23301 = CARTESIAN_POINT ( 'NONE',  ( 25.00000000000000000, 3.061616997868383043E-15, -170.0000000000000000 ) ) ;
#23302 = CARTESIAN_POINT ( 'NONE',  ( 7.644554776091147741E-16, 12.48450537969573659, -170.6562500020484094 ) ) ;
#23303 = CARTESIAN_POINT ( 'NONE',  ( -1.040834085586084257E-14, -125.0000000000000000, 22.49999999999999289 ) ) ;
#23304 = EDGE_CURVE ( 'NONE', #2497, #5570, #21259, .T. ) ;
#23305 = CARTESIAN_POINT ( 'NONE',  ( 7.644554776091147741E-16, 12.48450537969573659, -132.9687500020483810 ) ) ;
#23306 = CARTESIAN_POINT ( 'NONE',  ( 7.644554776091147741E-16, 12.48450537969573659, -98.46875000204839523 ) ) ;
#23307 = CARTESIAN_POINT ( 'NONE',  ( 7.070501591499376803E-16, 11.54700538379251284, -116.0000000040967905 ) ) ;
#23308 = CARTESIAN_POINT ( 'NONE',  ( -10.81189881249999729, 1.324075727343319199E-15, -107.2812500020483810 ) ) ;
#23309 = CARTESIAN_POINT ( 'NONE',  ( 4.999999999999992006, -8.660254037844389075, -185.6250000040967905 ) ) ;
#23310 = CARTESIAN_POINT ( 'NONE',  ( 7.644554776091147741E-16, 12.48450537969573659, -113.4687500020483668 ) ) ;
#23311 = CARTESIAN_POINT ( 'NONE',  ( -10.81189881249999729, 1.324075727343319199E-15, -189.7812500020484094 ) ) ;
#23312 = CARTESIAN_POINT ( 'NONE',  ( -9.999999999999998224, 1.224646799147353059E-15, -200.0000000000000000 ) ) ;
#23313 = DIRECTION ( 'NONE',  ( -1.000000000000000000, 0.000000000000000000, 0.000000000000000000 ) ) ;
#23314 = CARTESIAN_POINT ( 'NONE',  ( -10.00000000000000000, -5.773502691896251982, -130.1250000000000000 ) ) ;
#23315 = CARTESIAN_POINT ( 'NONE',  ( 5.000000000000000000, 8.660254037844385522, -3.249999999999975131 ) ) ;
#23316 = ADVANCED_FACE ( 'NONE', ( #26338 ), #20, .T. ) ;
#23317 = CARTESIAN_POINT ( 'NONE',  ( -10.81189881249999729, 6.242252689847871849, -60.71875000204837391 ) ) ;
#23318 = CARTESIAN_POINT ( 'NONE',  ( 7.644554776091147741E-16, 12.48450537969573659, -51.96875000204836681 ) ) ;
#23319 = CARTESIAN_POINT ( 'NONE',  ( 9.999999999999998224, 0.000000000000000000, -177.8750000040967905 ) ) ;
#23320 = CARTESIAN_POINT ( 'NONE',  ( 10.81189881249999551, -6.242252689847874514, -16.65625000204837747 ) ) ;
#23321 = CARTESIAN_POINT ( 'NONE',  ( -10.81189881249999729, 6.242252689847871849, -33.71875000204835260 ) ) ;
#23322 = FACE_OUTER_BOUND ( 'NONE', #15945, .T. ) ;
#23323 = CARTESIAN_POINT ( 'NONE',  ( -5.405949406250003975, -9.363379034771801557, -136.8437500020484094 ) ) ;
#23324 = CARTESIAN_POINT ( 'NONE',  ( -5.000000000000003553, -8.660254037844383745, -107.4999999999999858 ) ) ;
#23325 = CARTESIAN_POINT ( 'NONE',  ( 7.644554776091147741E-16, 12.48450537969573659, -32.65625000204835970 ) ) ;
#23326 = EDGE_CURVE ( 'NONE', #21643, #32599, #29309, .T. ) ;
#23327 = AXIS2_PLACEMENT_3D ( 'NONE', #17333, #4188, #20576 ) ;
#23328 = DIRECTION ( 'NONE',  ( 1.000000000000000000, 0.000000000000000000, 0.000000000000000000 ) ) ;
#23329 = CARTESIAN_POINT ( 'NONE',  ( -9.999999999999998224, 5.773502691896259087, -59.87499999999998579 ) ) ;
#23330 = CARTESIAN_POINT ( 'NONE',  ( 5.405949406249999534, 9.363379034771803333, -131.7812500020483810 ) ) ;
#23331 = CARTESIAN_POINT ( 'NONE',  ( 7.644554776091147741E-16, 12.48450537969573659, -113.6562500020483952 ) ) ;
#23332 = ORIENTED_EDGE ( 'NONE', *, *, #13919, .F. ) ;
#23333 = FACE_BOUND ( 'NONE', #2651, .T. ) ;
#23334 = CARTESIAN_POINT ( 'NONE',  ( -2.121150477449813534E-15, -11.54700538379251284, -109.2500000040967763 ) ) ;
#23335 = CARTESIAN_POINT ( 'NONE',  ( -9.999999999999998224, 1.224646799147353059E-15, -200.0000000000000000 ) ) ;
#23336 = CARTESIAN_POINT ( 'NONE',  ( 10.81189881249999907, 6.242252689847868297, -65.71875000204838102 ) ) ;
#23337 = ORIENTED_EDGE ( 'NONE', *, *, #26094, .F. ) ;
#23338 = CARTESIAN_POINT ( 'NONE',  ( -9.999999999999998224, 5.773502691896259087, -32.87499999999997158 ) ) ;
#23339 = B_SPLINE_CURVE_WITH_KNOTS ( 'NONE', 3,
 ( #41062, #35056, #21231, #18418, #11507, #34842, #11939, #24709, #22098, #5054, #41928, #5266, #38067, #25131, #37855, #28152, #35272, #8508, #21444, #31608, #31392, #28368, #34628, #4835, #32036, #1826, #5484, #15385, #25343 ),
 .UNSPECIFIED., .F., .F.,
 ( 4, 2, 2, 2, 2, 2, 2, 2, 2, 2, 2, 2, 1, 2, 4 ),
 ( 0.000000000000000000, 0.001276655870610509703, 0.002553311741221020708, 0.005106623482442043151, 0.006383279353052552854, 0.007659935223663064292, 0.008936591094273573996, 0.01021324696488408630, 0.01148990283549459861, 0.01276655870610510918, 0.01531987044732613552, 0.01659652631793664609, 0.01787318218854715840, 0.01914983805915767071, 0.02042649392976818301 ),
 .UNSPECIFIED. ) ;
#23340 = CARTESIAN_POINT ( 'NONE',  ( -2.121150477449813534E-15, -11.54700538379251284, -17.75000000409676559 ) ) ;
#23341 = CARTESIAN_POINT ( 'NONE',  ( -2.293366432827344421E-15, -12.48450537969573659, -45.40625000204837391 ) ) ;
#23342 = EDGE_CURVE ( 'NONE', #3545, #4655, #30075, .T. ) ;
#23343 = CARTESIAN_POINT ( 'NONE',  ( -9.999999999999998224, 1.224646799147353059E-15, -2.749999999999974687 ) ) ;
#23344 = CARTESIAN_POINT ( 'NONE',  ( -9.999999999999998224, 5.773502691896259087, -36.25000000409675494 ) ) ;
#23345 = DIRECTION ( 'NONE',  ( -1.000000000000000000, 0.000000000000000000, 0.000000000000000000 ) ) ;
#23346 = CARTESIAN_POINT ( 'NONE',  ( -10.81189881249999729, 6.242252689847871849, -141.9062500020484094 ) ) ;
#23347 = CARTESIAN_POINT ( 'NONE',  ( -9.999999999999227285, -5.773502691896698735, -110.6249999999999574 ) ) ;
#23348 = EDGE_LOOP ( 'NONE', ( #28936, #31914, #3154, #22546 ) ) ;
#23349 = EDGE_CURVE ( 'NONE', #28187, #39897, #18456, .T. ) ;
#23350 = ORIENTED_EDGE ( 'NONE', *, *, #13460, .T. ) ;
#23351 = ORIENTED_EDGE ( 'NONE', *, *, #38580, .T. ) ;
#23352 = VECTOR ( 'NONE', #29633, 1000.000000000000000 ) ;
#23353 = DIRECTION ( 'NONE',  ( -0.000000000000000000, -0.000000000000000000, 1.000000000000000000 ) ) ;
#23354 = CARTESIAN_POINT ( 'NONE',  ( -9.999999999999998224, 1.224646799147353059E-15, -163.2500000000000000 ) ) ;
#23355 = CARTESIAN_POINT ( 'NONE',  ( 10.81189881249999551, -6.242252689847874514, -172.4687500020484094 ) ) ;
#23356 = CARTESIAN_POINT ( 'NONE',  ( 10.81189881249999551, -6.242252689847874514, -20.96875000204836681 ) ) ;
#23357 = CARTESIAN_POINT ( 'NONE',  ( 9.999999999999998224, 0.000000000000000000, -111.8750000040967763 ) ) ;
#23358 = FACE_OUTER_BOUND ( 'NONE', #17692, .T. ) ;
#23359 = CARTESIAN_POINT ( 'NONE',  ( -10.81189881249999729, -6.242252689847864744, -154.9687500020484094 ) ) ;
#23360 = CARTESIAN_POINT ( 'NONE',  ( -10.81189881249999729, 6.242252689847871849, -144.7187500020483810 ) ) ;
#23361 = CARTESIAN_POINT ( 'NONE',  ( 4.999999999999992006, -8.660254037844389075, -116.2499999999999858 ) ) ;
#23362 = CARTESIAN_POINT ( 'NONE',  ( -5.405949406250003975, -9.363379034771801557, -126.3437500020483952 ) ) ;
#23363 = CARTESIAN_POINT ( 'NONE',  ( 7.644554776091147741E-16, 12.48450537969573659, -134.6562500020483810 ) ) ;
#23364 = CARTESIAN_POINT ( 'NONE',  ( -10.81189881249999729, 6.242252689847871849, -11.21875000204836859 ) ) ;
#23366 = EDGE_CURVE ( 'NONE', #2600, #41098, #29575, .T. ) ;
#23365 = CARTESIAN_POINT ( 'NONE',  ( 10.81189881249999551, -6.242252689847874514, -137.9687500020483810 ) ) ;
#23367 = CARTESIAN_POINT ( 'NONE',  ( 10.00000000000025402, -5.773502691896113426, -129.6250000000000000 ) ) ;
#23368 = CARTESIAN_POINT ( 'NONE',  ( -4.999999999999996447, 8.660254037844387298, -43.87500000409677625 ) ) ;
#23369 = CARTESIAN_POINT ( 'NONE',  ( 4.999999999999992006, -8.660254037844389075, -156.7500000000000000 ) ) ;
#23370 = CARTESIAN_POINT ( 'NONE',  ( 7.070501591499376803E-16, 11.54700538379251284, -99.50000000409679046 ) ) ;
#23371 = CARTESIAN_POINT ( 'NONE',  ( 5.405949406249992428, -9.363379034771808662, -75.09375000204838102 ) ) ;
#23372 = CARTESIAN_POINT ( 'NONE',  ( 5.405949406249999534, 9.363379034771803333, -40.28125000204838102 ) ) ;
#23373 = CARTESIAN_POINT ( 'NONE',  ( 5.405949406249992428, -9.363379034771808662, -55.59375000204835970 ) ) ;
#23374 = CARTESIAN_POINT ( 'NONE',  ( 4.999999999999992006, -8.660254037844389075, -141.7500000000000000 ) ) ;
#23375 = CARTESIAN_POINT ( 'NONE',  ( 5.405949406249992428, -9.363379034771808662, -162.0937500020484094 ) ) ;
#23376 = CARTESIAN_POINT ( 'NONE',  ( -4.999999999999996447, 8.660254037844387298, -126.0000000000000000 ) ) ;
#23377 = CARTESIAN_POINT ( 'NONE',  ( -2.293366432827344421E-15, -12.48450537969573659, -136.9062500020484094 ) ) ;
#23378 = CARTESIAN_POINT ( 'NONE',  ( 9.999999999999998224, 0.000000000000000000, -200.0000000000000000 ) ) ;
#23379 = CARTESIAN_POINT ( 'NONE',  ( 9.999999999999996447, -5.773502691896262640, -116.5000000040967763 ) ) ;
#23380 = CARTESIAN_POINT ( 'NONE',  ( 9.999999999999998224, 0.000000000000000000, -90.49999999999998579 ) ) ;
#23381 =( BOUNDED_CURVE ( )  B_SPLINE_CURVE ( 2, ( #37236, #33808, #10689, #11113, #24523, #14122, #10905 ),
 .UNSPECIFIED., .F., .F. ) 
 B_SPLINE_CURVE_WITH_KNOTS ( ( 3, 2, 2, 3 ),
 ( 0.3768656716417911334, 0.3781094527363185187, 0.3793532338308459040, 0.3805970149253732338 ),
 .UNSPECIFIED. ) 
 CURVE ( )  GEOMETRIC_REPRESENTATION_ITEM ( )  RATIONAL_B_SPLINE_CURVE ( ( 0.9999999999999880096, 0.8660254037844506980, 1.000000000000000000, 0.8660254037844387076, 1.000000000000000000, 0.8660254037844267172, 1.000000000000011990 ) ) 
 REPRESENTATION_ITEM ( '' )  );
#23382 = VERTEX_POINT ( 'NONE', #236 ) ;
#23383 = CARTESIAN_POINT ( 'NONE',  ( -10.81189881249999729, -6.242252689847864744, -108.6562500020483952 ) ) ;
#23384 = CARTESIAN_POINT ( 'NONE',  ( -5.000000000000003553, -8.660254037844383745, -131.8750000040967905 ) ) ;
#23385 = FACE_OUTER_BOUND ( 'NONE', #34242, .T. ) ;
#23386 = CARTESIAN_POINT ( 'NONE',  ( -5.405949406249996869, 9.363379034771805109, -167.5312500020484094 ) ) ;
#23387 = CARTESIAN_POINT ( 'NONE',  ( 5.000000000000000000, 8.660254037844385522, -39.62500000409676915 ) ) ;
#23388 = CARTESIAN_POINT ( 'NONE',  ( -10.00000000000038547, 5.773502691896036154, -154.7500000040967905 ) ) ;
#23389 = CARTESIAN_POINT ( 'NONE',  ( 5.405949406249992428, -9.363379034771808662, -49.78125000204838813 ) ) ;
#23390 = CARTESIAN_POINT ( 'NONE',  ( 9.999999999999998224, 0.000000000000000000, -73.99999999999998579 ) ) ;
#23391 = CARTESIAN_POINT ( 'NONE',  ( -5.405949406249996869, 9.363379034771805109, -160.0312500020484094 ) ) ;
#23392 = CARTESIAN_POINT ( 'NONE',  ( -10.81189881249999729, 6.242252689847871849, -134.2187500020483810 ) ) ;
#23393 = CARTESIAN_POINT ( 'NONE',  ( 4.999999999999992006, -8.660254037844389075, -50.62500000409675494 ) ) ;
#23394 = VERTEX_POINT ( 'NONE', #36262 ) ;
#23395 = CARTESIAN_POINT ( 'NONE',  ( 9.999999999999998224, 0.000000000000000000, -189.5000000000000000 ) ) ;
#23396 = AXIS2_PLACEMENT_3D ( 'NONE', #18586, #28532, #12520 ) ;
#23398 = ORIENTED_EDGE ( 'NONE', *, *, #33406, .F. ) ;
#23397 = CARTESIAN_POINT ( 'NONE',  ( 10.81189881249999729, 0.000000000000000000, -72.03125000204838102 ) ) ;
#23399 = APPROVAL_DATE_TIME ( #36763, #11985 ) ;
#23401 = ORIENTED_EDGE ( 'NONE', *, *, #37566, .F. ) ;
#23400 = CARTESIAN_POINT ( 'NONE',  ( 5.405949406249992428, -9.363379034771808662, -121.5937500020483952 ) ) ;
#23402 = CARTESIAN_POINT ( 'NONE',  ( 5.405949406249999534, 9.363379034771803333, -17.59375000204835260 ) ) ;
#23403 = UNCERTAINTY_MEASURE_WITH_UNIT (LENGTH_MEASURE( 1.000000000000000082E-05 ), #11537, 'distance_accuracy_value', 'NONE');
#23404 = CARTESIAN_POINT ( 'NONE',  ( -10.81189881249999907, -6.242252689847864744, -198.4687500020484379 ) ) ;
#23406 = EDGE_CURVE ( 'NONE', #39897, #23938, #19844, .T. ) ;
#23405 = CARTESIAN_POINT ( 'NONE',  ( 10.81189881249999551, -6.242252689847874514, -43.46875000204836681 ) ) ;
#23407 = CARTESIAN_POINT ( 'NONE',  ( 0.000000000000000000, 0.000000000000000000, -200.0000000000000000 ) ) ;
#23408 = CARTESIAN_POINT ( 'NONE',  ( 10.00000000000102318, -5.773502691895667560, -10.00000000409673184 ) ) ;
#23409 = CARTESIAN_POINT ( 'NONE',  ( 10.81189881249999729, 0.000000000000000000, -176.8437500020483810 ) ) ;
#23410 = CARTESIAN_POINT ( 'NONE',  ( 5.405949406249999534, 9.363379034771803333, -172.0937500020484094 ) ) ;
#23411 = CARTESIAN_POINT ( 'NONE',  ( 10.81189881249999907, 6.242252689847868297, -148.2187500020484094 ) ) ;
#23412 = CARTESIAN_POINT ( 'NONE',  ( 10.81189881249999729, 0.000000000000000000, -161.8437500020484094 ) ) ;
#23413 = DIRECTION ( 'NONE',  ( 1.000000000000000000, 0.000000000000000000, 0.000000000000000000 ) ) ;
#23414 = CARTESIAN_POINT ( 'NONE',  ( 7.070501591499376803E-16, 11.54700538379251284, -194.0000000040968189 ) ) ;
#23415 = CARTESIAN_POINT ( 'NONE',  ( 9.999999999999998224, 0.000000000000000000, -185.0000000000000000 ) ) ;
#23416 = VECTOR ( 'NONE', #25576, 1000.000000000000000 ) ;
#23417 = CARTESIAN_POINT ( 'NONE',  ( -2.293366432827344421E-15, -12.48450537969573659, -100.7187500020483952 ) ) ;
#23418 = CARTESIAN_POINT ( 'NONE',  ( 9.999999999999998224, 0.000000000000000000, -138.5000000000000000 ) ) ;
#23419 = CARTESIAN_POINT ( 'NONE',  ( -10.81189881249999729, 6.242252689847871849, -66.90625000204839523 ) ) ;
#23420 = CARTESIAN_POINT ( 'NONE',  ( 5.405949406249992428, -9.363379034771808662, -186.0937500020483810 ) ) ;
#23421 = CARTESIAN_POINT ( 'NONE',  ( -5.405949406249996869, 9.363379034771805109, -122.5312500020483952 ) ) ;
#23422 = CARTESIAN_POINT ( 'NONE',  ( 5.405949406249999534, 9.363379034771803333, -160.2812500020484094 ) ) ;
#23423 = CARTESIAN_POINT ( 'NONE',  ( -5.405949406249996869, 9.363379034771805109, -55.03125000204836681 ) ) ;
#23424 = CARTESIAN_POINT ( 'NONE',  ( 10.00000000000000000, 5.773502691896255534, -141.7500000040967905 ) ) ;
#23425 = CARTESIAN_POINT ( 'NONE',  ( -4.999999999999996447, 8.660254037844387298, -115.4999999999999858 ) ) ;
#23426 = ADVANCED_FACE ( 'NONE', ( #33252 ), #8721, .T. ) ;
#23427 = ORIENTED_EDGE ( 'NONE', *, *, #929, .T. ) ;
#23428 = CARTESIAN_POINT ( 'NONE',  ( -2.293366432827344421E-15, -12.48450537969573659, -130.9062500020483810 ) ) ;
#23429 = CARTESIAN_POINT ( 'NONE',  ( 10.81189881249999729, 0.000000000000000000, -150.0312500020483810 ) ) ;
#23430 = CARTESIAN_POINT ( 'NONE',  ( 5.405949406249992428, -9.363379034771808662, -187.7812500020484094 ) ) ;
#23431 = CARTESIAN_POINT ( 'NONE',  ( 17.32050807568890960, 1.173974112367310985E-14, 49.99999999999998579 ) ) ;
#23432 = CARTESIAN_POINT ( 'NONE',  ( -5.405949406250003975, -9.363379034771801557, -84.34375000204836681 ) ) ;
#23433 = ORIENTED_EDGE ( 'NONE', *, *, #38294, .F. ) ;
#23434 = CARTESIAN_POINT ( 'NONE',  ( -9.999999999999998224, 1.224646799147353059E-15, -58.24999999999997158 ) ) ;
#23435 = CARTESIAN_POINT ( 'NONE',  ( 10.81189881249999551, -6.242252689847874514, -176.9687500020483810 ) ) ;
#23436 = CARTESIAN_POINT ( 'NONE',  ( 4.999999999999992006, -8.660254037844389075, -64.12500000409676204 ) ) ;
#23437 = CARTESIAN_POINT ( 'NONE',  ( -9.999999999999227285, -5.773502691896698735, -109.5000000040967478 ) ) ;
#23438 = CARTESIAN_POINT ( 'NONE',  ( 11.54700538379250396, 20.00000000000000711, 49.99999999999998579 ) ) ;
#23439 = CARTESIAN_POINT ( 'NONE',  ( -10.81189881249999729, 1.324075727343319199E-15, -78.78125000204838102 ) ) ;
#23440 = CARTESIAN_POINT ( 'NONE',  ( 5.405949406249992428, -9.363379034771808662, -60.28125000204836681 ) ) ;
#23441 = CARTESIAN_POINT ( 'NONE',  ( -9.999999999999998224, 5.773502691896259087, -52.75000000409676915 ) ) ;
#23442 = CARTESIAN_POINT ( 'NONE',  ( -10.81189881249999729, 1.324075727343319199E-15, -9.593750002048345493 ) ) ;
#23443 = CARTESIAN_POINT ( 'NONE',  ( -31.99999999999997158, 4.102566777143632196E-15, -180.0000000000000000 ) ) ;
#23444 = CARTESIAN_POINT ( 'NONE',  ( 10.81189881249999551, -6.242252689847874514, -183.1562500020484094 ) ) ;
#23445 = CARTESIAN_POINT ( 'NONE',  ( 5.405949406249999534, 9.363379034771803333, -13.28125000204835615 ) ) ;
#23446 = CARTESIAN_POINT ( 'NONE',  ( -10.00000000000102496, 5.773502691895664007, -85.37499999999994316 ) ) ;
#23447 = CARTESIAN_POINT ( 'NONE',  ( -9.999999999999998224, 1.224646799147353059E-15, -200.0000000000000000 ) ) ;
#23448 = CARTESIAN_POINT ( 'NONE',  ( 0.000000000000000000, 0.000000000000000000, -200.0000000000000000 ) ) ;
#23449 = CARTESIAN_POINT ( 'NONE',  ( -2.121150477449813534E-15, -11.54700538379251284, -134.7500000040967905 ) ) ;
#23450 = CARTESIAN_POINT ( 'NONE',  ( -5.000000000000003553, -8.660254037844383745, -167.5000000000000000 ) ) ;
#23451 = CARTESIAN_POINT ( 'NONE',  ( -2.121150477449813534E-15, -11.54700538379251284, -62.37499999999997158 ) ) ;
#23452 = AXIS2_PLACEMENT_3D ( 'NONE', #8162, #4920, #41145 ) ;
#23454 = ORIENTED_EDGE ( 'NONE', *, *, #16169, .F. ) ;
#23453 = CARTESIAN_POINT ( 'NONE',  ( -10.81189881249999729, 1.324075727343319199E-15, -95.28125000204838102 ) ) ;
#23455 = CARTESIAN_POINT ( 'NONE',  ( -10.00000000000154188, 5.773502691895366468, -82.75000000409673362 ) ) ;
#23457 = VERTEX_POINT ( 'NONE', #13358 ) ;
#23456 = CARTESIAN_POINT ( 'NONE',  ( -5.405949406250003975, -9.363379034771801557, -102.3437500020483810 ) ) ;
#23458 = ORIENTED_EDGE ( 'NONE', *, *, #4281, .T. ) ;
#23459 = EDGE_CURVE ( 'NONE', #1402, #7087, #35054, .T. ) ;
#23460 = CARTESIAN_POINT ( 'NONE',  ( 10.81189881249999729, 0.000000000000000000, -37.34375000204836681 ) ) ;
#23461 = CARTESIAN_POINT ( 'NONE',  ( -5.405949406250003975, -9.363379034771801557, -24.53125000204836681 ) ) ;
#23462 = CARTESIAN_POINT ( 'NONE',  ( 5.405949406249999534, 9.363379034771803333, -68.59375000204836681 ) ) ;
#23463 = CARTESIAN_POINT ( 'NONE',  ( 9.999999999999998224, 0.000000000000000000, -73.99999999999998579 ) ) ;
#23464 = CARTESIAN_POINT ( 'NONE',  ( -4.999999999999996447, 8.660254037844387298, -46.49999999999998579 ) ) ;
#23465 = CARTESIAN_POINT ( 'NONE',  ( -2.293366432827344421E-15, -12.48450537969573659, -195.2187500020484094 ) ) ;
#23466 = CARTESIAN_POINT ( 'NONE',  ( 10.81189881249999907, 6.242252689847868297, -151.2187500020483810 ) ) ;
#23467 =( BOUNDED_CURVE ( )  B_SPLINE_CURVE ( 2, ( #23766, #17053, #34342, #14014, #36708, #17689, #1104 ),
 .UNSPECIFIED., .F., .F. ) 
 B_SPLINE_CURVE_WITH_KNOTS ( ( 3, 2, 2, 3 ),
 ( 0.3432835820895522860, 0.3445273631840797268, 0.3457711442786070566, 0.3470149253731344974 ),
 .UNSPECIFIED. ) 
 CURVE ( )  GEOMETRIC_REPRESENTATION_ITEM ( )  RATIONAL_B_SPLINE_CURVE ( ( 0.9999999999999940048, 0.8660254037844447028, 1.000000000000000000, 0.8660254037844387076, 1.000000000000000000, 0.8660254037844207220, 1.000000000000017986 ) ) 
 REPRESENTATION_ITEM ( '' )  );
#23468 = CARTESIAN_POINT ( 'NONE',  ( 10.00000000000000000, 5.773502691896255534, -132.7500000040967905 ) ) ;
#23469 = DIRECTION ( 'NONE',  ( 3.469446951953614805E-17, 1.000000000000000000, -0.000000000000000000 ) ) ;
#23470 = CARTESIAN_POINT ( 'NONE',  ( 5.405949406249999534, 9.363379034771803333, -146.7812500020483810 ) ) ;
#23471 = CARTESIAN_POINT ( 'NONE',  ( -9.999999999999998224, 5.773502691896259087, -3.250000004096759376 ) ) ;
#23472 = CARTESIAN_POINT ( 'NONE',  ( -4.999999999999996447, 8.660254037844387298, -49.87500000409675494 ) ) ;
#23473 = CARTESIAN_POINT ( 'NONE',  ( 7.644554776091147741E-16, 12.48450537969573659, -122.4687500020483952 ) ) ;
#23474 = CARTESIAN_POINT ( 'NONE',  ( -4.999999999999996447, 8.660254037844387298, -160.8750000040967905 ) ) ;
#23475 = CARTESIAN_POINT ( 'NONE',  ( -10.81189881249999907, -6.242252689847864744, -93.65625000204840944 ) ) ;
#23476 = CARTESIAN_POINT ( 'NONE',  ( 7.644554776091147741E-16, 12.48450537969573659, -105.9687500020483668 ) ) ;
#23477 = CARTESIAN_POINT ( 'NONE',  ( 7.644554776091147741E-16, 12.48450537969573659, -68.46875000204838102 ) ) ;
#23478 = CARTESIAN_POINT ( 'NONE',  ( 10.81189881249999551, -6.242252689847874514, -73.65625000204836681 ) ) ;
#23479 = CARTESIAN_POINT ( 'NONE',  ( -2.121150477449813534E-15, -11.54700538379251284, -158.7500000040968189 ) ) ;
#23480 = CARTESIAN_POINT ( 'NONE',  ( 10.81189881249999729, 0.000000000000000000, -157.5312500020484094 ) ) ;
#23481 = CARTESIAN_POINT ( 'NONE',  ( -10.81189881249999907, -6.242252689847864744, -173.1562500020484094 ) ) ;
#23482 = AXIS2_PLACEMENT_3D ( 'NONE', #21481, #17802, #11328 ) ;
#23483 = CARTESIAN_POINT ( 'NONE',  ( -9.999999999999998224, 1.224646799147353059E-15, -114.1250000040967763 ) ) ;
#23484 = CARTESIAN_POINT ( 'NONE',  ( 5.405949406249999534, 9.363379034771803333, 0.4062499979516354109 ) ) ;
#23485 = CARTESIAN_POINT ( 'NONE',  ( -10.81189881249999729, 1.324075727343319199E-15, -107.0937500020483810 ) ) ;
#23486 = EDGE_CURVE ( 'NONE', #16772, #27040, #5239, .T. ) ;
#23487 = CARTESIAN_POINT ( 'NONE',  ( -4.999999999999996447, 8.660254037844387298, -83.99999999999997158 ) ) ;
#23488 = CARTESIAN_POINT ( 'NONE',  ( -5.405949406250003975, -9.363379034771801557, -5.031250002048376579 ) ) ;
#23489 = CARTESIAN_POINT ( 'NONE',  ( 10.00000000000000000, 5.773502691896255534, -86.25000000409677625 ) ) ;
#23490 = VECTOR ( 'NONE', #35968, 1000.000000000000000 ) ;
#23491 = CARTESIAN_POINT ( 'NONE',  ( 4.999999999999992006, -8.660254037844389075, -95.62500000409677625 ) ) ;
#23492 = CARTESIAN_POINT ( 'NONE',  ( -10.81189881249999729, 1.324075727343319199E-15, -99.78125000204839523 ) ) ;
#23493 = CARTESIAN_POINT ( 'NONE',  ( -10.81189881249999729, 1.324075727343319199E-15, -86.28125000204838102 ) ) ;
#23494 = VERTEX_POINT ( 'NONE', #22308 ) ;
#23495 = CARTESIAN_POINT ( 'NONE',  ( -5.000000000000003553, -8.660254037844383745, -82.37500000409676204 ) ) ;
#23496 = CARTESIAN_POINT ( 'NONE',  ( -4.999999999999996447, 8.660254037844387298, -133.8750000040967905 ) ) ;
#23497 = CARTESIAN_POINT ( 'NONE',  ( 5.405949406249992428, -9.363379034771808662, -34.59375000204836681 ) ) ;
#23498 = ORIENTED_EDGE ( 'NONE', *, *, #1806, .F. ) ;
#23499 = CARTESIAN_POINT ( 'NONE',  ( -10.00000000000000000, -5.773502691896251982, -5.624999999999962697 ) ) ;
#23500 = CARTESIAN_POINT ( 'NONE',  ( 5.405949406249999534, 9.363379034771803333, -40.28125000204838102 ) ) ;
#23501 = CARTESIAN_POINT ( 'NONE',  ( 4.999999999999992006, -8.660254037844389075, -149.2500000000000000 ) ) ;
#23502 = CARTESIAN_POINT ( 'NONE',  ( -2.121150477449813534E-15, -11.54700538379251284, -14.75000000409676737 ) ) ;
#23503 = CARTESIAN_POINT ( 'NONE',  ( 5.000000000000000000, 8.660254037844385522, -12.62500000409674783 ) ) ;
#23504 = CARTESIAN_POINT ( 'NONE',  ( 5.000000000000000000, 8.660254037844385522, -192.2500000000000000 ) ) ;
#23505 = DIRECTION ( 'NONE',  ( 1.000000000000000000, -0.000000000000000000, -0.000000000000000000 ) ) ;
#23507 = ORIENTED_EDGE ( 'NONE', *, *, #3499, .T. ) ;
#23506 = CARTESIAN_POINT ( 'NONE',  ( -10.81189881249999907, -6.242252689847864744, -117.6562500020483952 ) ) ;
#23508 = CARTESIAN_POINT ( 'NONE',  ( -9.999999999998969713, -5.773502691896847949, -75.00000000409674783 ) ) ;
#23509 = ORIENTED_EDGE ( 'NONE', *, *, #22094, .F. ) ;
#23510 =( BOUNDED_CURVE ( )  B_SPLINE_CURVE ( 2, ( #4121, #17260, #30464, #891, #26364, #41201, #11640 ),
 .UNSPECIFIED., .F., .F. ) 
 B_SPLINE_CURVE_WITH_KNOTS ( ( 3, 2, 2, 3 ),
 ( 0.5410447761194030480, 0.5422885572139304333, 0.5435323383084578186, 0.5447761194029852039 ),
 .UNSPECIFIED. ) 
 CURVE ( )  GEOMETRIC_REPRESENTATION_ITEM ( )  RATIONAL_B_SPLINE_CURVE ( ( 0.9999999999999880096, 0.8660254037844506980, 1.000000000000000000, 0.8660254037844387076, 1.000000000000000000, 0.8660254037844267172, 1.000000000000011990 ) ) 
 REPRESENTATION_ITEM ( '' )  );
#23511 = CARTESIAN_POINT ( 'NONE',  ( 10.81189881249999551, -6.242252689847874514, -48.15625000204836681 ) ) ;
#23512 = COORDINATED_UNIVERSAL_TIME_OFFSET ( 6, 0, .AHEAD. ) ;
#23513 = APPROVAL_PERSON_ORGANIZATION ( #41432, #28088, #4175 ) ;
#23514 = CARTESIAN_POINT ( 'NONE',  ( 10.81189881249999729, 0.000000000000000000, -95.84375000204838102 ) ) ;
#23515 = CARTESIAN_POINT ( 'NONE',  ( 7.644554776091147741E-16, 12.48450537969573659, -121.1562500020483952 ) ) ;
#23516 = ORIENTED_EDGE ( 'NONE', *, *, #1421, .F. ) ;
#23517 = DIRECTION ( 'NONE',  ( -0.000000000000000000, -0.000000000000000000, -1.000000000000000000 ) ) ;
#23518 = DIRECTION ( 'NONE',  ( -1.000000000000000000, 0.000000000000000000, 0.000000000000000000 ) ) ;
#23519 =( BOUNDED_CURVE ( )  B_SPLINE_CURVE ( 2, ( #36068, #27847, #4747, #33905, #31310, #7786, #17893 ),
 .UNSPECIFIED., .F., .F. ) 
 B_SPLINE_CURVE_WITH_KNOTS ( ( 3, 2, 2, 3 ),
 ( 0.4291044776119404269, 0.4303482587064677567, 0.4315920398009951975, 0.4328358208955225273 ),
 .UNSPECIFIED. ) 
 CURVE ( )  GEOMETRIC_REPRESENTATION_ITEM ( )  RATIONAL_B_SPLINE_CURVE ( ( 0.9999999999999880096, 0.8660254037844506980, 1.000000000000000000, 0.8660254037844387076, 1.000000000000000000, 0.8660254037844207220, 1.000000000000017986 ) ) 
 REPRESENTATION_ITEM ( '' )  );
#23520 = CARTESIAN_POINT ( 'NONE',  ( -5.405949406250003975, -9.363379034771801557, -170.0312500020484094 ) ) ;
#23521 = CARTESIAN_POINT ( 'NONE',  ( -9.999999999999998224, 1.224646799147353059E-15, -200.0000000000000000 ) ) ;
#23522 = CARTESIAN_POINT ( 'NONE',  ( 5.405949406249999534, 9.363379034771803333, -131.5937500020483810 ) ) ;
#23523 = CARTESIAN_POINT ( 'NONE',  ( -10.81189881249999907, -6.242252689847864744, -91.96875000204838102 ) ) ;
#23524 = CARTESIAN_POINT ( 'NONE',  ( 0.000000000000000000, 0.000000000000000000, -103.0000000000000000 ) ) ;
#23525 = CARTESIAN_POINT ( 'NONE',  ( -2.293366432827344421E-15, -12.48450537969573659, -97.90625000204839523 ) ) ;
#23526 = CARTESIAN_POINT ( 'NONE',  ( 9.999999999999996447, -5.773502691896262640, -182.5000000040968189 ) ) ;
#23527 = CARTESIAN_POINT ( 'NONE',  ( -10.81189881249999729, -6.242252689847864744, -111.4687500020483810 ) ) ;
#23528 = CARTESIAN_POINT ( 'NONE',  ( -10.81189881249999729, 6.242252689847871849, -179.4062500020484094 ) ) ;
#23529 = CARTESIAN_POINT ( 'NONE',  ( 9.999999999999998224, 0.000000000000000000, -126.8750000040967905 ) ) ;
#23530 = CARTESIAN_POINT ( 'NONE',  ( -10.81189881249999729, 6.242252689847871849, -179.4062500020484094 ) ) ;
#23531 = CARTESIAN_POINT ( 'NONE',  ( -10.81189881249999729, 6.242252689847871849, -195.9062500020484094 ) ) ;
#23532 = CARTESIAN_POINT ( 'NONE',  ( -10.81189881249999729, 6.242252689847871849, -62.21875000204838813 ) ) ;
#23533 = CARTESIAN_POINT ( 'NONE',  ( 10.81189881249999907, 6.242252689847868297, -44.71875000204837391 ) ) ;
#23534 = CARTESIAN_POINT ( 'NONE',  ( 4.999999999999992006, -8.660254037844389075, -182.6250000040967905 ) ) ;
#23535 = CARTESIAN_POINT ( 'NONE',  ( -5.405949406250003975, -9.363379034771801557, -20.03125000204836326 ) ) ;
#23536 = CARTESIAN_POINT ( 'NONE',  ( -5.405949406249996869, 9.363379034771805109, -26.34375000204835970 ) ) ;
#23537 = CYLINDRICAL_SURFACE ( 'NONE', #37131, 9.999999999999998224 ) ;
#23538 = CARTESIAN_POINT ( 'NONE',  ( 10.81189881249999729, 0.000000000000000000, -131.8437500020484094 ) ) ;
#23539 = EDGE_CURVE ( 'NONE', #6043, #22060, #35270, .T. ) ;
#23540 = CARTESIAN_POINT ( 'NONE',  ( -10.00000000000000000, -5.773502691896251982, -109.1249999999999858 ) ) ;
#23541 = CARTESIAN_POINT ( 'NONE',  ( -10.81189881249999907, -6.242252689847864744, -39.65625000204836681 ) ) ;
#23542 = CARTESIAN_POINT ( 'NONE',  ( -9.999999999999998224, 1.224646799147353059E-15, -169.2500000000000000 ) ) ;
#23543 = ADVANCED_FACE ( 'NONE', ( #18632 ), #18854, .T. ) ;
#23544 = CARTESIAN_POINT ( 'NONE',  ( -10.00000000000000000, -5.773502691896251982, -61.12499999999998579 ) ) ;
#23545 = CARTESIAN_POINT ( 'NONE',  ( 7.644554776091147741E-16, 12.48450537969573659, -134.6562500020483810 ) ) ;
#23546 = CARTESIAN_POINT ( 'NONE',  ( 5.405949406249992428, -9.363379034771808662, -111.2812500020483810 ) ) ;
#23547 = ORIENTED_EDGE ( 'NONE', *, *, #39722, .F. ) ;
#23548 = CARTESIAN_POINT ( 'NONE',  ( 9.999999999999872102, 5.773502691896329253, -160.8750000000000000 ) ) ;
#23549 = CARTESIAN_POINT ( 'NONE',  ( 5.000000000000000000, 8.660254037844385522, -110.1250000040967763 ) ) ;
#23550 = CARTESIAN_POINT ( 'NONE',  ( -9.999999999999227285, -5.773502691896698735, -136.5000000040967620 ) ) ;
#23551 = CARTESIAN_POINT ( 'NONE',  ( -10.81189881249999907, -6.242252689847864744, -64.96875000204838102 ) ) ;
#23552 = VERTEX_POINT ( 'NONE', #2462 ) ;
#23553 = CARTESIAN_POINT ( 'NONE',  ( 4.999999999999992006, -8.660254037844389075, -33.74999999999997158 ) ) ;
#23554 = APPROVAL_PERSON_ORGANIZATION ( #4932, #23300, #31277 ) ;
#23555 = CARTESIAN_POINT ( 'NONE',  ( -5.405949406249996869, 9.363379034771805109, -38.53125000204838102 ) ) ;
#23556 = CARTESIAN_POINT ( 'NONE',  ( 9.999999999999998224, 0.000000000000000000, -111.8750000040967763 ) ) ;
#23557 = CARTESIAN_POINT ( 'NONE',  ( 7.070501591499377789E-16, 11.54700538379251284, -36.50000000409675494 ) ) ;
#23558 = CARTESIAN_POINT ( 'NONE',  ( -5.500000000000005329, -20.00000000000000000, -220.0000000000000000 ) ) ;
#23559 = VECTOR ( 'NONE', #34444, 1000.000000000000000 ) ;
#23560 = CARTESIAN_POINT ( 'NONE',  ( 7.644554776091147741E-16, 12.48450537969573659, -145.1562500020484094 ) ) ;
#23561 = CARTESIAN_POINT ( 'NONE',  ( -9.999999999999742428, -5.773502691896402084, -120.0000000040967905 ) ) ;
#23562 = EDGE_LOOP ( 'NONE', ( #41695, #3918, #35353, #26098 ) ) ;
#23563 = ORIENTED_EDGE ( 'NONE', *, *, #15645, .T. ) ;
#23564 = EDGE_CURVE ( 'NONE', #2600, #18939, #6615, .T. ) ;
#23565 = DIRECTION ( 'NONE',  ( 1.000000000000000000, 0.000000000000000000, 0.000000000000000000 ) ) ;
#23566 = LINE ( 'NONE', #3492, #8402 ) ;
#23567 = CARTESIAN_POINT ( 'NONE',  ( -2.293366432827344421E-15, -12.48450537969573659, -162.2187500020483810 ) ) ;
#23568 = DIRECTION ( 'NONE',  ( -1.000000000000000000, 0.000000000000000000, 0.000000000000000000 ) ) ;
#23569 = CARTESIAN_POINT ( 'NONE',  ( -10.81189881249999729, 1.324075727343319199E-15, -20.09375000204835615 ) ) ;
#23570 = CARTESIAN_POINT ( 'NONE',  ( -9.999999999999998224, 1.224646799147353059E-15, -200.0000000000000000 ) ) ;
#23571 = CARTESIAN_POINT ( 'NONE',  ( 9.999999999999998224, 0.000000000000000000, -156.8750000040967905 ) ) ;
#23572 = CARTESIAN_POINT ( 'NONE',  ( -10.81189881249999729, -6.242252689847864744, -159.4687500020484094 ) ) ;
#23573 = CARTESIAN_POINT ( 'NONE',  ( -10.81189881249999729, 6.242252689847871849, -140.2187500020483810 ) ) ;
#23574 = CARTESIAN_POINT ( 'NONE',  ( 9.999999999998969713, 5.773502691896851502, -67.87499999999998579 ) ) ;
#23575 = CARTESIAN_POINT ( 'NONE',  ( 10.81189881249999907, 6.242252689847868297, -121.2187500020483952 ) ) ;
#23576 = CARTESIAN_POINT ( 'NONE',  ( 10.81189881249999551, -6.242252689847874514, 0.03124999795164895566 ) ) ;
#23577 = CARTESIAN_POINT ( 'NONE',  ( -2.293366432827344421E-15, -12.48450537969573659, -123.4062500020484094 ) ) ;
#23578 = CARTESIAN_POINT ( 'NONE',  ( -5.405949406250003975, -9.363379034771801557, -9.343750002048345493 ) ) ;
#23579 = CARTESIAN_POINT ( 'NONE',  ( 7.644554776091147741E-16, 12.48450537969573659, -140.4687500020483810 ) ) ;
#23580 = CARTESIAN_POINT ( 'NONE',  ( 10.37090729747365714, -3.076925949860441545, -179.9999999999999432 ) ) ;
#23581 = CARTESIAN_POINT ( 'NONE',  ( 9.999999999999998224, 0.000000000000000000, -125.3750000040967905 ) ) ;
#23582 = CARTESIAN_POINT ( 'NONE',  ( -5.000000000000003553, -8.660254037844383745, -152.5000000000000000 ) ) ;
#23583 = CARTESIAN_POINT ( 'NONE',  ( -9.999999999999998224, 1.224646799147353059E-15, -17.74999999999996092 ) ) ;
#23584 = AXIS2_PLACEMENT_3D ( 'NONE', #37451, #21041, #4648 ) ;
#23585 = CARTESIAN_POINT ( 'NONE',  ( 7.644554776091147741E-16, 12.48450537969573659, -86.46875000204838102 ) ) ;
#23586 = CARTESIAN_POINT ( 'NONE',  ( 5.405949406249999534, 9.363379034771803333, -62.59375000204836681 ) ) ;
#23587 = CARTESIAN_POINT ( 'NONE',  ( -5.405949406249996869, 9.363379034771805109, -46.03125000204838813 ) ) ;
#23588 = CARTESIAN_POINT ( 'NONE',  ( -2.293366432827344421E-15, -12.48450537969573659, -51.21875000204836681 ) ) ;
#23589 = CARTESIAN_POINT ( 'NONE',  ( 9.999999999999998224, 0.000000000000000000, -113.3750000040967763 ) ) ;
#23590 = CARTESIAN_POINT ( 'NONE',  ( -5.405949406249996869, 9.363379034771805109, -159.8437500020484094 ) ) ;
#23591 = ADVANCED_FACE ( 'NONE', ( #7543 ), #4514, .F. ) ;
#23592 = CARTESIAN_POINT ( 'NONE',  ( 10.00000000000000000, 5.773502691896255534, -127.8749999999999858 ) ) ;
#23593 = CARTESIAN_POINT ( 'NONE',  ( -5.405949406249996869, 9.363379034771805109, -142.0312500020483810 ) ) ;
#23594 =( BOUNDED_CURVE ( )  B_SPLINE_CURVE ( 2, ( #42097, #8257, #34589, #28115, #11682, #28323, #41463 ),
 .UNSPECIFIED., .F., .F. ) 
 B_SPLINE_CURVE_WITH_KNOTS ( ( 3, 2, 2, 3 ),
 ( 0.7835820895522389584, 0.7848258706467662327, 0.7860696517412937290, 0.7873134328358211143 ),
 .UNSPECIFIED. ) 
 CURVE ( )  GEOMETRIC_REPRESENTATION_ITEM ( )  RATIONAL_B_SPLINE_CURVE ( ( 0.9999999999999880096, 0.8660254037844506980, 1.000000000000000000, 0.8660254037844387076, 1.000000000000000000, 0.8660254037844148378, 1.000000000000023981 ) ) 
 REPRESENTATION_ITEM ( '' )  );
#23595 = CARTESIAN_POINT ( 'NONE',  ( -9.999999999999998224, 1.224646799147353059E-15, -200.0000000000000000 ) ) ;
#23596 = CARTESIAN_POINT ( 'NONE',  ( -5.000000000000003553, -8.660254037844383745, -81.99999999999998579 ) ) ;
#23597 = CARTESIAN_POINT ( 'NONE',  ( -2.293366432827344421E-15, -12.48450537969573659, -15.40625000204837391 ) ) ;
#23598 = EDGE_CURVE ( 'NONE', #7415, #6469, #31463, .T. ) ;
#23599 = ORIENTED_EDGE ( 'NONE', *, *, #28324, .T. ) ;
#23600 = CARTESIAN_POINT ( 'NONE',  ( 10.81189881249999729, 6.242252689847867408, -110.9062500020483952 ) ) ;
#23601 = CARTESIAN_POINT ( 'NONE',  ( -9.999999999999998224, 1.224646799147353059E-15, -135.1250000040967620 ) ) ;
#23602 = CARTESIAN_POINT ( 'NONE',  ( -9.999999999999998224, 1.224646799147353059E-15, -56.74999999999996447 ) ) ;
#23603 = EDGE_CURVE ( 'NONE', #587, #3228, #3807, .T. ) ;
#23604 = CARTESIAN_POINT ( 'NONE',  ( -9.999999999999998224, 1.224646799147353059E-15, -42.12500000409677625 ) ) ;
#23605 = CARTESIAN_POINT ( 'NONE',  ( 10.00000000000051159, -5.773502691895965988, -91.00000000409676204 ) ) ;
#23606 = CARTESIAN_POINT ( 'NONE',  ( 5.405949406249992428, -9.363379034771808662, -55.78125000204836681 ) ) ;
#23607 = VECTOR ( 'NONE', #22826, 1000.000000000000000 ) ;
#23608 = CARTESIAN_POINT ( 'NONE',  ( 10.81189881249999551, -6.242252689847874514, -153.1562500020484379 ) ) ;
#23609 = CARTESIAN_POINT ( 'NONE',  ( -10.81189881249999729, 6.242252689847871849, -135.7187500020483810 ) ) ;
#23610 = CARTESIAN_POINT ( 'NONE',  ( -5.000000000000003553, -8.660254037844383745, -33.99999999999997158 ) ) ;
#23611 = CARTESIAN_POINT ( 'NONE',  ( 5.000000000000000000, 8.660254037844385522, -171.6250000040968189 ) ) ;
#23612 = ORIENTED_EDGE ( 'NONE', *, *, #4064, .F. ) ;
#23613 = CARTESIAN_POINT ( 'NONE',  ( 9.999999999999998224, 0.000000000000000000, -200.0000000000000000 ) ) ;
#23614 = ADVANCED_FACE ( 'NONE', ( #7974 ), #21733, .T. ) ;
#23615 = VECTOR ( 'NONE', #14868, 1000.000000000000000 ) ;
#23617 = ORIENTED_EDGE ( 'NONE', *, *, #29653, .F. ) ;
#23616 = CARTESIAN_POINT ( 'NONE',  ( -10.81189881249999729, 6.242252689847871849, -63.90625000204836681 ) ) ;
#23618 = PERSON_AND_ORGANIZATION ( #11915, #17965 ) ;
#23620 = VERTEX_POINT ( 'NONE', #40534 ) ;
#23619 = CARTESIAN_POINT ( 'NONE',  ( 10.81189881249999729, 0.000000000000000000, -115.3437500020483810 ) ) ;
#23621 = CARTESIAN_POINT ( 'NONE',  ( -5.405949406249996869, 9.363379034771805109, -24.84375000204835970 ) ) ;
#23622 = CARTESIAN_POINT ( 'NONE',  ( 10.81189881249999907, 6.242252689847868297, -194.7187500020484094 ) ) ;
#23623 = CARTESIAN_POINT ( 'NONE',  ( -10.81189881249999729, 6.242252689847871849, -47.21875000204836681 ) ) ;
#23624 = CARTESIAN_POINT ( 'NONE',  ( -9.999999999999998224, 1.224646799147353059E-15, -156.1250000040967905 ) ) ;
#23625 = CARTESIAN_POINT ( 'NONE',  ( 5.000000000000000000, 8.660254037844385522, -152.1250000040967905 ) ) ;
#23626 = CARTESIAN_POINT ( 'NONE',  ( 10.81189881249999729, 0.000000000000000000, -179.8437500020483810 ) ) ;
#23627 = CARTESIAN_POINT ( 'NONE',  ( 7.644554776091147741E-16, 12.48450537969573659, -158.4687500020483810 ) ) ;
#23628 = CARTESIAN_POINT ( 'NONE',  ( -2.293366432827344421E-15, -12.48450537969573659, -148.7187500020484094 ) ) ;
#23629 =( BOUNDED_CURVE ( )  B_SPLINE_CURVE ( 2, ( #18482, #1887, #38129, #8572, #31670, #2104, #41569 ),
 .UNSPECIFIED., .F., .F. ) 
 B_SPLINE_CURVE_WITH_KNOTS ( ( 3, 2, 2, 3 ),
 ( 0.7947761194029852039, 0.7960199004975125892, 0.7972636815920399744, 0.7985074626865673597 ),
 .UNSPECIFIED. ) 
 CURVE ( )  GEOMETRIC_REPRESENTATION_ITEM ( )  RATIONAL_B_SPLINE_CURVE ( ( 0.9999999999999880096, 0.8660254037844506980, 1.000000000000000000, 0.8660254037844387076, 1.000000000000000000, 0.8660254037844148378, 1.000000000000023981 ) ) 
 REPRESENTATION_ITEM ( '' )  );
#23630 = CARTESIAN_POINT ( 'NONE',  ( 7.644554776091147741E-16, 12.48450537969573659, -159.9687500020484094 ) ) ;
#23631 = CARTESIAN_POINT ( 'NONE',  ( -9.999999999999479527, -5.773502691896549521, -118.5000000040967763 ) ) ;
#23632 = DIRECTION ( 'NONE',  ( -0.000000000000000000, -0.000000000000000000, -1.000000000000000000 ) ) ;
#23633 = CARTESIAN_POINT ( 'NONE',  ( 7.070501591499377789E-16, 11.54700538379251284, -177.1250000000000000 ) ) ;
#23634 = CARTESIAN_POINT ( 'NONE',  ( 10.81189881249999729, 0.000000000000000000, -95.84375000204838102 ) ) ;
#23635 = CARTESIAN_POINT ( 'NONE',  ( 4.999999999999992006, -8.660254037844389075, -72.74999999999998579 ) ) ;
#23636 = CARTESIAN_POINT ( 'NONE',  ( 7.644554776091147741E-16, 12.48450537969573659, -68.65625000204840944 ) ) ;
#23637 = CARTESIAN_POINT ( 'NONE',  ( 10.00000000000051159, -5.773502691895965988, -97.00000000409676204 ) ) ;
#23638 = CARTESIAN_POINT ( 'NONE',  ( 7.644554776091147741E-16, 12.48450537969573659, -182.4687500020484094 ) ) ;
#23639 = CARTESIAN_POINT ( 'NONE',  ( -10.81189881249999729, 6.242252689847871849, -119.4062500020483952 ) ) ;
#23640 = CARTESIAN_POINT ( 'NONE',  ( 5.405949406249999534, 9.363379034771803333, -158.7812500020484094 ) ) ;
#23641 = CARTESIAN_POINT ( 'NONE',  ( -10.81189881249999729, 1.324075727343319199E-15, -54.78125000204836681 ) ) ;
#23642 = CARTESIAN_POINT ( 'NONE',  ( 10.00000000000000000, 5.773502691896255534, -140.2500000040967905 ) ) ;
#23643 = CARTESIAN_POINT ( 'NONE',  ( -10.00000000000000000, -5.773502691896251982, -109.1249999999999858 ) ) ;
#23644 = ORIENTED_EDGE ( 'NONE', *, *, #22453, .F. ) ;
#23645 = CARTESIAN_POINT ( 'NONE',  ( -5.405949406249996869, 9.363379034771805109, -131.5312500020484094 ) ) ;
#23646 = CARTESIAN_POINT ( 'NONE',  ( 5.405949406249992428, -9.363379034771808662, -151.7812500020484094 ) ) ;
#23647 = CARTESIAN_POINT ( 'NONE',  ( 7.644554776091147741E-16, 12.48450537969573659, -187.1562500020484094 ) ) ;
#23648 = CARTESIAN_POINT ( 'NONE',  ( 10.81189881249999907, 6.242252689847868297, -79.21875000204838102 ) ) ;
#23649 = ORIENTED_EDGE ( 'NONE', *, *, #37567, .F. ) ;
#23650 = CARTESIAN_POINT ( 'NONE',  ( 7.070501591499377789E-16, 11.54700538379251284, -46.62499999999996447 ) ) ;
#23651 = CARTESIAN_POINT ( 'NONE',  ( -5.405949406250003975, -9.363379034771801557, -183.3437500020483810 ) ) ;
#23652 = CARTESIAN_POINT ( 'NONE',  ( 4.999999999999992006, -8.660254037844389075, -65.62500000409676204 ) ) ;
#23653 = CARTESIAN_POINT ( 'NONE',  ( -4.999999999999996447, 8.660254037844387298, -153.0000000000000000 ) ) ;
#23654 = CARTESIAN_POINT ( 'NONE',  ( 10.81189881249999729, 0.000000000000000000, -79.53125000204838102 ) ) ;
#23655 = CARTESIAN_POINT ( 'NONE',  ( 7.644554776091147741E-16, 12.48450537969573659, -61.15625000204838102 ) ) ;
#23656 = CARTESIAN_POINT ( 'NONE',  ( -2.121150477449813534E-15, -11.54700538379251284, -50.75000000409676915 ) ) ;
#23657 = CARTESIAN_POINT ( 'NONE',  ( 5.405949406249999534, 9.363379034771803333, -13.09375000204834905 ) ) ;
#23658 = CYLINDRICAL_SURFACE ( 'NONE', #39332, 9.999999999999998224 ) ;
#23659 = CARTESIAN_POINT ( 'NONE',  ( -10.81189881249999729, 6.242252689847871849, -185.4062500020484094 ) ) ;
#23660 = EDGE_CURVE ( 'NONE', #21425, #5246, #33096, .T. ) ;
#23661 = CARTESIAN_POINT ( 'NONE',  ( -10.81189881249999729, 6.242252689847871849, -3.906250002048361480 ) ) ;
#23662 = CARTESIAN_POINT ( 'NONE',  ( 5.000000000000000000, 8.660254037844385522, -40.74999999999997868 ) ) ;
#23663 = CARTESIAN_POINT ( 'NONE',  ( 10.00000000000051159, -5.773502691895965988, -148.0000000040967905 ) ) ;
#23664 = CARTESIAN_POINT ( 'NONE',  ( -9.999999999999998224, 0.000000000000000000, -99.99999999999998579 ) ) ;
#23665 = CARTESIAN_POINT ( 'NONE',  ( 0.000000000000000000, 0.000000000000000000, -99.99999999999998579 ) ) ;
#23666 = DIRECTION ( 'NONE',  ( -0.000000000000000000, -0.000000000000000000, 1.000000000000000000 ) ) ;
#23668 = ORIENTED_EDGE ( 'NONE', *, *, #14285, .T. ) ;
#23667 = CARTESIAN_POINT ( 'NONE',  ( 10.81189881249999551, -6.242252689847874514, -90.15625000204836681 ) ) ;
#23669 = CARTESIAN_POINT ( 'NONE',  ( -9.999999999999998224, 1.224646799147353059E-15, -82.62500000409676204 ) ) ;
#23671 = ORIENTED_EDGE ( 'NONE', *, *, #32387, .T. ) ;
#23670 = CARTESIAN_POINT ( 'NONE',  ( -10.81189881249999729, 1.324075727343319199E-15, -101.0937500020483810 ) ) ;
#23672 = VERTEX_POINT ( 'NONE', #33670 ) ;
#23673 = CARTESIAN_POINT ( 'NONE',  ( 5.405949406249992428, -9.363379034771808662, -25.59375000204835970 ) ) ;
#23674 = CARTESIAN_POINT ( 'NONE',  ( 7.644554776091147741E-16, 12.48450537969573659, -22.15625000204837391 ) ) ;
#23675 = CARTESIAN_POINT ( 'NONE',  ( 5.405949406249992428, -9.363379034771808662, -73.59375000204838102 ) ) ;
#23676 = DIRECTION ( 'NONE',  ( -0.000000000000000000, -0.000000000000000000, 1.000000000000000000 ) ) ;
#23677 = CARTESIAN_POINT ( 'NONE',  ( -4.999999999999996447, 8.660254037844387298, -47.99999999999998579 ) ) ;
#23678 = CARTESIAN_POINT ( 'NONE',  ( 10.81189881249999729, 0.000000000000000000, -191.8437500020484094 ) ) ;
#23679 = CARTESIAN_POINT ( 'NONE',  ( -10.81189881249999729, 1.324075727343319199E-15, -153.5937500020483810 ) ) ;
#23680 = DIRECTION ( 'NONE',  ( -1.000000000000000000, 0.000000000000000000, 0.000000000000000000 ) ) ;
#23681 = DIRECTION ( 'NONE',  ( 1.000000000000000000, 0.000000000000000000, 0.000000000000000000 ) ) ;
#23682 = CARTESIAN_POINT ( 'NONE',  ( -2.293366432827344421E-15, -12.48450537969573659, -147.4062500020483810 ) ) ;
#23683 = CARTESIAN_POINT ( 'NONE',  ( 9.999999999999998224, 0.000000000000000000, -2.375000004096766482 ) ) ;
#23684 = CARTESIAN_POINT ( 'NONE',  ( 9.999999999999998224, 0.000000000000000000, -60.87500000409676204 ) ) ;
#23685 = CARTESIAN_POINT ( 'NONE',  ( -2.293366432827344421E-15, -12.48450537969573659, -118.7187500020483952 ) ) ;
#23686 = CARTESIAN_POINT ( 'NONE',  ( -9.999999999999998224, 1.224646799147353059E-15, -140.7500000000000000 ) ) ;
#23687 = CARTESIAN_POINT ( 'NONE',  ( 10.81189881249999551, -6.242252689847874514, -87.15625000204838102 ) ) ;
#23688 = CARTESIAN_POINT ( 'NONE',  ( 7.644554776091147741E-16, 12.48450537969573659, -99.96875000204836681 ) ) ;
#23689 = CARTESIAN_POINT ( 'NONE',  ( -10.81189881249999729, 6.242252689847871849, -68.21875000204838102 ) ) ;
#23690 = CARTESIAN_POINT ( 'NONE',  ( 5.405949406249992428, -9.363379034771808662, -75.28125000204838102 ) ) ;
#23691 = CARTESIAN_POINT ( 'NONE',  ( 5.000000000000000000, 8.660254037844385522, -162.6250000040967905 ) ) ;
#23692 = CARTESIAN_POINT ( 'NONE',  ( 5.405949406249999534, 9.363379034771803333, -155.7812500020484094 ) ) ;
#23693 = CARTESIAN_POINT ( 'NONE',  ( -10.81189881249999907, -6.242252689847864744, -170.1562500020483810 ) ) ;
#23694 = CARTESIAN_POINT ( 'NONE',  ( -9.999999999999998224, 0.000000000000000000, -99.99999999999998579 ) ) ;
#23695 = LINE ( 'NONE', #7286, #6837 ) ;
#23696 = CARTESIAN_POINT ( 'NONE',  ( 9.999999999999998224, 0.000000000000000000, -200.0000000000000000 ) ) ;
#23697 = CARTESIAN_POINT ( 'NONE',  ( -10.81189881249999729, 1.324075727343319199E-15, -102.5937500020483810 ) ) ;
#23698 = CARTESIAN_POINT ( 'NONE',  ( -5.000000000000003553, -8.660254037844383745, -78.99999999999998579 ) ) ;
#23699 = CARTESIAN_POINT ( 'NONE',  ( -5.405949406249996869, 9.363379034771805109, -2.531250002048373915 ) ) ;
#23700 = CARTESIAN_POINT ( 'NONE',  ( 9.999999999999996447, -5.773502691896262640, -86.50000000409676204 ) ) ;
#23701 = DIRECTION ( 'NONE',  ( 1.000000000000000000, 0.000000000000000000, 0.000000000000000000 ) ) ;
#23702 = CARTESIAN_POINT ( 'NONE',  ( 5.405949406249992428, -9.363379034771808662, -102.2812500020483952 ) ) ;
#23703 = CARTESIAN_POINT ( 'NONE',  ( -10.81189881249999729, 6.242252689847871849, -80.40625000204838102 ) ) ;
#23704 = CARTESIAN_POINT ( 'NONE',  ( 4.999999999999992006, -8.660254037844389075, -74.62500000409677625 ) ) ;
#23705 = CARTESIAN_POINT ( 'NONE',  ( 10.81189881249999729, 0.000000000000000000, -35.84375000204836681 ) ) ;
#23706 = ORIENTED_EDGE ( 'NONE', *, *, #36218, .F. ) ;
#23707 = CARTESIAN_POINT ( 'NONE',  ( -2.121150477449813534E-15, -11.54700538379251284, -11.37499999999995737 ) ) ;
#23708 = CARTESIAN_POINT ( 'NONE',  ( 10.81189881249999551, -6.242252689847874514, -30.15625000204835615 ) ) ;
#23709 = CARTESIAN_POINT ( 'NONE',  ( -2.121150477449813534E-15, -11.54700538379251284, -144.8750000000000000 ) ) ;
#23710 = CARTESIAN_POINT ( 'NONE',  ( 9.999999999998969713, 5.773502691896851502, -45.75000000409674783 ) ) ;
#23711 = CARTESIAN_POINT ( 'NONE',  ( 5.000000000000000000, 8.660254037844385522, -5.125000004096769146 ) ) ;
#23712 = CARTESIAN_POINT ( 'NONE',  ( -9.999999999999998224, 5.773502691896259087, -191.8750000000000000 ) ) ;
#23713 = LINE ( 'NONE', #33438, #14422 ) ;
#23715 = ORIENTED_EDGE ( 'NONE', *, *, #1154, .T. ) ;
#23714 = CARTESIAN_POINT ( 'NONE',  ( 7.644554776091147741E-16, 12.48450537969573659, -115.1562500020483952 ) ) ;
#23716 = CARTESIAN_POINT ( 'NONE',  ( -4.999999999999996447, 8.660254037844387298, -22.87500000409675849 ) ) ;
#23717 = EDGE_LOOP ( 'NONE', ( #15365, #36226, #3870, #4708 ) ) ;
#23718 =( BOUNDED_CURVE ( )  B_SPLINE_CURVE ( 2, ( #21903, #18657, #6147, #35508, #8959, #19289, #12383 ),
 .UNSPECIFIED., .F., .F. ) 
 B_SPLINE_CURVE_WITH_KNOTS ( ( 3, 2, 2, 3 ),
 ( 0.7276119402985077311, 0.7288557213930350054, 0.7300995024875623907, 0.7313432835820897759 ),
 .UNSPECIFIED. ) 
 CURVE ( )  GEOMETRIC_REPRESENTATION_ITEM ( )  RATIONAL_B_SPLINE_CURVE ( ( 0.9999999999999761302, 0.8660254037844625774, 1.000000000000000000, 0.8660254037844387076, 1.000000000000000000, 0.8660254037844148378, 1.000000000000023981 ) ) 
 REPRESENTATION_ITEM ( '' )  );
#23719 = ORIENTED_EDGE ( 'NONE', *, *, #10587, .F. ) ;
#23720 = EDGE_CURVE ( 'NONE', #6, #30360, #20981, .T. ) ;
#23721 = CARTESIAN_POINT ( 'NONE',  ( -10.81189881249999729, 1.324075727343319199E-15, -42.78125000204838102 ) ) ;
#23722 = PERSON_AND_ORGANIZATION_ROLE ( 'design_owner' ) ;
#23723 = CARTESIAN_POINT ( 'NONE',  ( -10.81189881249999729, 6.242252689847871849, -92.21875000204838102 ) ) ;
#23724 = CARTESIAN_POINT ( 'NONE',  ( -5.405949406250003975, -9.363379034771801557, -126.5312500020483952 ) ) ;
#23725 = EDGE_LOOP ( 'NONE', ( #7260, #35817, #42474, #41153 ) ) ;
#23726 = FACE_OUTER_BOUND ( 'NONE', #8062, .T. ) ;
#23727 = CARTESIAN_POINT ( 'NONE',  ( 10.81189881249999729, 6.242252689847867408, -196.2187500020484094 ) ) ;
#23728 = CARTESIAN_POINT ( 'NONE',  ( -10.81189881249999729, 1.324075727343319199E-15, -168.7812500020484094 ) ) ;
#23729 = FACE_OUTER_BOUND ( 'NONE', #36978, .T. ) ;
#23730 = CARTESIAN_POINT ( 'NONE',  ( -10.81189881249999729, 1.324075727343319199E-15, -120.5937500020483952 ) ) ;
#23731 = CARTESIAN_POINT ( 'NONE',  ( -5.405949406250003975, -9.363379034771801557, -93.34375000204838102 ) ) ;
#23732 = CARTESIAN_POINT ( 'NONE',  ( -10.81189881249999729, 1.324075727343319199E-15, -198.5937500020484094 ) ) ;
#23733 = CARTESIAN_POINT ( 'NONE',  ( -10.81189881249999729, 1.324075727343319199E-15, -101.2812500020483952 ) ) ;
#23734 = CARTESIAN_POINT ( 'NONE',  ( 9.999999999999998224, 0.000000000000000000, -188.3750000040967905 ) ) ;
#23735 = CARTESIAN_POINT ( 'NONE',  ( -2.293366432827344421E-15, -12.48450537969573659, -109.7187500020483668 ) ) ;
#23736 = CARTESIAN_POINT ( 'NONE',  ( 10.81189881249999729, 6.242252689847867408, -179.9062500020484094 ) ) ;
#23737 = CARTESIAN_POINT ( 'NONE',  ( 9.999999999999998224, 0.000000000000000000, -104.3750000040967763 ) ) ;
#23738 = CARTESIAN_POINT ( 'NONE',  ( 5.000000000000000000, 8.660254037844385522, -132.6250000040967620 ) ) ;
#23739 = CARTESIAN_POINT ( 'NONE',  ( 10.81189881249999729, 0.000000000000000000, -198.0312500020484094 ) ) ;
#23740 = CARTESIAN_POINT ( 'NONE',  ( 10.81189881249999729, 0.000000000000000000, -58.34375000204835970 ) ) ;
#23741 = CARTESIAN_POINT ( 'NONE',  ( -10.81189881249999907, -6.242252689847864744, -39.46875000204835970 ) ) ;
#23742 = CARTESIAN_POINT ( 'NONE',  ( -9.999999999999998224, 1.224646799147353059E-15, -172.6250000040968189 ) ) ;
#23743 = CARTESIAN_POINT ( 'NONE',  ( 10.81189881249999729, 0.000000000000000000, -15.03125000204835793 ) ) ;
#23744 = CARTESIAN_POINT ( 'NONE',  ( -5.405949406250003975, -9.363379034771801557, -18.34375000204835260 ) ) ;
#23745 = LINE ( 'NONE', #36898, #12301 ) ;
#23746 = CARTESIAN_POINT ( 'NONE',  ( -5.405949406249996869, 9.363379034771805109, -132.8437500020484094 ) ) ;
#23747 = CARTESIAN_POINT ( 'NONE',  ( 7.070501591499377789E-16, 11.54700538379251284, -103.6249999999999858 ) ) ;
#23748 = CARTESIAN_POINT ( 'NONE',  ( 5.405949406249992428, -9.363379034771808662, -31.78125000204837391 ) ) ;
#23749 = CARTESIAN_POINT ( 'NONE',  ( -5.000000000000003553, -8.660254037844383745, -49.37500000409678336 ) ) ;
#23750 = CARTESIAN_POINT ( 'NONE',  ( 10.00000000000000000, 5.773502691896255534, -60.37499999999997868 ) ) ;
#23751 = CARTESIAN_POINT ( 'NONE',  ( 5.405949406249992428, -9.363379034771808662, -123.2812500020483952 ) ) ;
#23752 = CARTESIAN_POINT ( 'NONE',  ( -2.293366432827344421E-15, -12.48450537969573659, -111.4062500020483952 ) ) ;
#23753 = VERTEX_POINT ( 'NONE', #4729 ) ;
#23754 = CARTESIAN_POINT ( 'NONE',  ( 9.999999999999998224, 0.000000000000000000, -176.3750000040967905 ) ) ;
#23755 = CARTESIAN_POINT ( 'NONE',  ( -2.121150477449813534E-15, -11.54700538379251284, -100.2500000040967905 ) ) ;
#23756 = CARTESIAN_POINT ( 'NONE',  ( -9.999999999999998224, 1.224646799147353059E-15, -136.6250000040967620 ) ) ;
#23757 = CARTESIAN_POINT ( 'NONE',  ( 10.81189881249999729, 0.000000000000000000, -61.34375000204836681 ) ) ;
#23758 = ORIENTED_EDGE ( 'NONE', *, *, #4523, .T. ) ;
#23759 = CARTESIAN_POINT ( 'NONE',  ( -4.999999999999996447, 8.660254037844387298, -32.99999999999997158 ) ) ;
#23760 = CARTESIAN_POINT ( 'NONE',  ( -5.405949406250003975, -9.363379034771801557, -38.03125000204838102 ) ) ;
#23761 = CARTESIAN_POINT ( 'NONE',  ( 9.999999999999998224, 0.000000000000000000, -200.0000000000000000 ) ) ;
#23762 = CARTESIAN_POINT ( 'NONE',  ( 9.999999999999998224, 0.000000000000000000, -39.87500000409676915 ) ) ;
#23763 =( BOUNDED_CURVE ( )  B_SPLINE_CURVE ( 2, ( #16451, #9572, #22112, #26408, #26196, #35286, #16236 ),
 .UNSPECIFIED., .F., .F. ) 
 B_SPLINE_CURVE_WITH_KNOTS ( ( 3, 2, 2, 3 ),
 ( 0.7462686567164180662, 0.7475124378109453405, 0.7487562189054727257, 0.7500000000000001110 ),
 .UNSPECIFIED. ) 
 CURVE ( )  GEOMETRIC_REPRESENTATION_ITEM ( )  RATIONAL_B_SPLINE_CURVE ( ( 0.9999999999999880096, 0.8660254037844506980, 1.000000000000000000, 0.8660254037844387076, 1.000000000000000000, 0.8660254037844267172, 1.000000000000011990 ) ) 
 REPRESENTATION_ITEM ( '' )  );
#23764 = DIRECTION ( 'NONE',  ( -1.000000000000000000, 0.000000000000000000, 0.000000000000000000 ) ) ;
#23765 = CARTESIAN_POINT ( 'NONE',  ( 10.81189881249999551, -6.242252689847874514, -145.6562500020484094 ) ) ;
#23766 = CARTESIAN_POINT ( 'NONE',  ( 9.999999999999998224, 0.000000000000000000, -129.8750000040967905 ) ) ;
#23767 = ORIENTED_EDGE ( 'NONE', *, *, #41214, .T. ) ;
#23768 =( BOUNDED_CURVE ( )  B_SPLINE_CURVE ( 2, ( #1709, #27816, #14834, #28034, #18301, #31059, #27384 ),
 .UNSPECIFIED., .F., .F. ) 
 B_SPLINE_CURVE_WITH_KNOTS ( ( 3, 2, 2, 3 ),
 ( 0.4514925373134329734, 0.4527363184079603031, 0.4539800995024877439, 0.4552238805970150737 ),
 .UNSPECIFIED. ) 
 CURVE ( )  GEOMETRIC_REPRESENTATION_ITEM ( )  RATIONAL_B_SPLINE_CURVE ( ( 0.9999999999999880096, 0.8660254037844506980, 1.000000000000000000, 0.8660254037844387076, 1.000000000000000000, 0.8660254037844207220, 1.000000000000017986 ) ) 
 REPRESENTATION_ITEM ( '' )  );
#23769 = EDGE_CURVE ( 'NONE', #15394, #25371, #26759, .T. ) ;
#23770 = EDGE_LOOP ( 'NONE', ( #9952, #20450, #33538, #36602 ) ) ;
#23771 = DIRECTION ( 'NONE',  ( -0.000000000000000000, -0.000000000000000000, -1.000000000000000000 ) ) ;
#23772 = FACE_OUTER_BOUND ( 'NONE', #23972, .T. ) ;
#23773 = CARTESIAN_POINT ( 'NONE',  ( 10.81189881249999729, 0.000000000000000000, -167.8437500020484094 ) ) ;
#23774 = VECTOR ( 'NONE', #20566, 1000.000000000000000 ) ;
#23775 = CARTESIAN_POINT ( 'NONE',  ( -10.81189881249999729, 1.324075727343319199E-15, -197.2812500020484094 ) ) ;
#23776 = CARTESIAN_POINT ( 'NONE',  ( 10.81189881249999907, 6.242252689847868297, -19.21875000204837747 ) ) ;
#23777 = CYLINDRICAL_SURFACE ( 'NONE', #12244, 9.999999999999998224 ) ;
#23778 = CARTESIAN_POINT ( 'NONE',  ( -2.293366432827344421E-15, -12.48450537969573659, -154.7187500020483810 ) ) ;
#23779 = CARTESIAN_POINT ( 'NONE',  ( -2.293366432827344421E-15, -12.48450537969573659, -136.7187500020483810 ) ) ;
#23780 = CARTESIAN_POINT ( 'NONE',  ( 5.405949406249992428, -9.363379034771808662, -103.7812500020483810 ) ) ;
#23781 = CARTESIAN_POINT ( 'NONE',  ( 7.644554776091147741E-16, 12.48450537969573659, -114.9687500020483668 ) ) ;
#23782 = CARTESIAN_POINT ( 'NONE',  ( -2.121150477449813534E-15, -11.54700538379251284, -194.7500000040967905 ) ) ;
#23783 = CARTESIAN_POINT ( 'NONE',  ( 10.81189881249999551, -6.242252689847874514, -124.6562500020483952 ) ) ;
#23784 = CARTESIAN_POINT ( 'NONE',  ( 10.81189881249999551, -6.242252689847874514, -7.468750002048351710 ) ) ;
#23785 = CARTESIAN_POINT ( 'NONE',  ( -5.405949406250003975, -9.363379034771801557, -138.3437500020484094 ) ) ;
#23786 = CARTESIAN_POINT ( 'NONE',  ( -5.405949406249996869, 9.363379034771805109, -199.0312500020484094 ) ) ;
#23787 = CARTESIAN_POINT ( 'NONE',  ( -9.999999999999479527, -5.773502691896549521, -97.12499999999997158 ) ) ;
#23788 = CARTESIAN_POINT ( 'NONE',  ( -10.00000000000000000, -5.773502691896251982, -157.1250000000000284 ) ) ;
#23789 = CARTESIAN_POINT ( 'NONE',  ( -2.121150477449813534E-15, -11.54700538379251284, -18.87499999999997158 ) ) ;
#23790 = CARTESIAN_POINT ( 'NONE',  ( 5.405949406249999534, 9.363379034771803333, -83.59375000204836681 ) ) ;
#23791 = CARTESIAN_POINT ( 'NONE',  ( 10.81189881249999729, 0.000000000000000000, -65.84375000204836681 ) ) ;
#23792 = FACE_BOUND ( 'NONE', #21318, .T. ) ;
#23793 = CARTESIAN_POINT ( 'NONE',  ( 10.81189881249999551, -6.242252689847874514, -43.65625000204838102 ) ) ;
#23794 = CARTESIAN_POINT ( 'NONE',  ( 5.405949406249992428, -9.363379034771808662, -48.09375000204838102 ) ) ;
#23795 = CARTESIAN_POINT ( 'NONE',  ( -2.121150477449813534E-15, -11.54700538379251284, -141.8750000000000000 ) ) ;
#23796 = CARTESIAN_POINT ( 'NONE',  ( 10.81189881249999907, 6.242252689847868297, -157.2187500020483810 ) ) ;
#23797 = CARTESIAN_POINT ( 'NONE',  ( -2.121150477449813534E-15, -11.54700538379251284, -132.8750000000000000 ) ) ;
#23798 = CARTESIAN_POINT ( 'NONE',  ( -2.293366432827344421E-15, -12.48450537969573659, -130.9062500020483810 ) ) ;
#23799 = CARTESIAN_POINT ( 'NONE',  ( -3.491915452972480960, 9.450838780596122035, -179.9999999999999147 ) ) ;
#23800 = VECTOR ( 'NONE', #13453, 1000.000000000000000 ) ;
#23801 = CARTESIAN_POINT ( 'NONE',  ( -4.999999999999996447, 8.660254037844387298, -83.99999999999997158 ) ) ;
#23802 = CARTESIAN_POINT ( 'NONE',  ( 10.81189881249999729, 0.000000000000000000, -18.03125000204835970 ) ) ;
#23803 = ORIENTED_EDGE ( 'NONE', *, *, #36968, .T. ) ;
#23804 = CARTESIAN_POINT ( 'NONE',  ( 10.81189881249999729, 0.000000000000000000, -112.5312500020483952 ) ) ;
#23805 = CARTESIAN_POINT ( 'NONE',  ( -10.00000000000000000, -5.773502691896251982, -129.0000000040967905 ) ) ;
#23806 = CARTESIAN_POINT ( 'NONE',  ( -5.000000000000003553, -8.660254037844383745, -185.5000000000000000 ) ) ;
#23807 = CARTESIAN_POINT ( 'NONE',  ( 4.999999999999992006, -8.660254037844389075, -37.12500000409676915 ) ) ;
#23808 = CARTESIAN_POINT ( 'NONE',  ( 9.999999999999998224, 0.000000000000000000, -102.5000000000000000 ) ) ;
#23809 = CARTESIAN_POINT ( 'NONE',  ( 10.81189881249999551, -6.242252689847874514, -49.65625000204837391 ) ) ;
#23810 = AXIS2_PLACEMENT_3D ( 'NONE', #37546, #40134, #36902 ) ;
#23811 = CARTESIAN_POINT ( 'NONE',  ( 10.00000000000025402, -5.773502691896113426, -135.6250000000000000 ) ) ;
#23812 = CARTESIAN_POINT ( 'NONE',  ( 5.405949406249999534, 9.363379034771803333, -154.2812500020484094 ) ) ;
#23813 = CARTESIAN_POINT ( 'NONE',  ( -2.293366432827344421E-15, -12.48450537969573659, -138.2187500020483810 ) ) ;
#23814 = ORIENTED_EDGE ( 'NONE', *, *, #36492, .F. ) ;
#23815 = CARTESIAN_POINT ( 'NONE',  ( 9.999999999999998224, 0.000000000000000000, -200.0000000000000000 ) ) ;
#23816 = ORIENTED_EDGE ( 'NONE', *, *, #39722, .T. ) ;
#23818 = VERTEX_POINT ( 'NONE', #14419 ) ;
#23817 = CARTESIAN_POINT ( 'NONE',  ( 5.405949406249992428, -9.363379034771808662, -60.28125000204836681 ) ) ;
#23819 = APPROVAL_DATE_TIME ( #36976, #42283 ) ;
#23820 = EDGE_CURVE ( 'NONE', #36083, #2497, #41898, .T. ) ;
#23822 = ORIENTED_EDGE ( 'NONE', *, *, #38083, .T. ) ;
#23821 = CARTESIAN_POINT ( 'NONE',  ( 10.81189881249999907, 6.242252689847868297, -110.7187500020483810 ) ) ;
#23823 = EDGE_CURVE ( 'NONE', #18936, #40403, #4376, .T. ) ;
#23824 = EDGE_CURVE ( 'NONE', #33328, #17480, #15164, .T. ) ;
#23825 = VECTOR ( 'NONE', #37631, 1000.000000000000000 ) ;
#23826 = EDGE_CURVE ( 'NONE', #4273, #29829, #22273, .T. ) ;
#23827 = CARTESIAN_POINT ( 'NONE',  ( -10.81189881249999729, -6.242252689847864744, -18.46875000204837036 ) ) ;
#23828 = CARTESIAN_POINT ( 'NONE',  ( -5.405949406249996869, 9.363379034771805109, -192.8437500020484094 ) ) ;
#23829 = AXIS2_PLACEMENT_3D ( 'NONE', #23024, #29715, #39831 ) ;
#23830 = CARTESIAN_POINT ( 'NONE',  ( 5.405949406249999534, 9.363379034771803333, -40.09375000204837391 ) ) ;
#23831 = CARTESIAN_POINT ( 'NONE',  ( -4.999999999999996447, 8.660254037844387298, -153.3750000040967905 ) ) ;
#23832 = CARTESIAN_POINT ( 'NONE',  ( -9.999999999999806377, 5.773502691895924244, -179.8750000000000000 ) ) ;
#23833 = CARTESIAN_POINT ( 'NONE',  ( -10.81189881249999729, -6.242252689847864744, -178.9687500020484094 ) ) ;
#23834 = AXIS2_PLACEMENT_3D ( 'NONE', #32482, #9372, #5508 ) ;
#23835 = CARTESIAN_POINT ( 'NONE',  ( -5.405949406249996869, 9.363379034771805109, -162.8437500020484094 ) ) ;
#23836 =( BOUNDED_CURVE ( )  B_SPLINE_CURVE ( 2, ( #18219, #1844, #8524, #28169, #41303, #37838, #27913 ),
 .UNSPECIFIED., .F., .F. ) 
 B_SPLINE_CURVE_WITH_KNOTS ( ( 3, 2, 2, 3 ),
 ( 0.1679104477611940427, 0.1691542288557214002, 0.1703980099502487855, 0.1716417910447761430 ),
 .UNSPECIFIED. ) 
 CURVE ( )  GEOMETRIC_REPRESENTATION_ITEM ( )  RATIONAL_B_SPLINE_CURVE ( ( 1.000000000000000000, 0.8660254037844387076, 1.000000000000000000, 0.8660254037844387076, 1.000000000000000000, 0.8660254037844357100, 1.000000000000003109 ) ) 
 REPRESENTATION_ITEM ( '' )  );
#23837 = APPROVAL ( #29294, 'UNKNOWN' ) ;
#23838 = CARTESIAN_POINT ( 'NONE',  ( 7.644554776091147741E-16, 12.48450537969573659, -138.9687500020484094 ) ) ;
#23839 = CARTESIAN_POINT ( 'NONE',  ( 10.81189881249999729, 6.242252689847867408, -161.7187500020483810 ) ) ;
#23840 = CARTESIAN_POINT ( 'NONE',  ( -4.999999999999996447, 8.660254037844387298, -126.3750000040967905 ) ) ;
#23841 = DIRECTION ( 'NONE',  ( 1.000000000000000000, 0.000000000000000000, 0.000000000000000000 ) ) ;
#23842 = CARTESIAN_POINT ( 'NONE',  ( 9.999999999999996447, -5.773502691896262640, -176.1250000000000000 ) ) ;
#23843 = CARTESIAN_POINT ( 'NONE',  ( 5.405949406249992428, -9.363379034771808662, -91.59375000204838102 ) ) ;
#23844 = DIRECTION ( 'NONE',  ( -1.000000000000000000, 0.000000000000000000, 0.000000000000000000 ) ) ;
#23845 = CARTESIAN_POINT ( 'NONE',  ( -10.81189881249999907, -6.242252689847864744, -68.15625000204840944 ) ) ;
#23846 = DIRECTION ( 'NONE',  ( -0.000000000000000000, -0.000000000000000000, 1.000000000000000000 ) ) ;
#23847 = CARTESIAN_POINT ( 'NONE',  ( 7.644554776091147741E-16, 12.48450537969573659, -174.9687500020484094 ) ) ;
#23848 = EDGE_CURVE ( 'NONE', #18780, #28714, #24023, .T. ) ;
#23849 = CARTESIAN_POINT ( 'NONE',  ( -2.293366432827344421E-15, -12.48450537969573659, -126.4062500020483952 ) ) ;
#23850 = CARTESIAN_POINT ( 'NONE',  ( -5.405949406249996869, 9.363379034771805109, -161.5312500020484094 ) ) ;
#23851 = CARTESIAN_POINT ( 'NONE',  ( 5.405949406249992428, -9.363379034771808662, -49.78125000204838813 ) ) ;
#23852 = CARTESIAN_POINT ( 'NONE',  ( -9.999999999999998224, 1.224646799147353059E-15, -127.6250000040967620 ) ) ;
#23853 = CARTESIAN_POINT ( 'NONE',  ( 7.070501591499377789E-16, 11.54700538379251284, -111.1249999999999716 ) ) ;
#23854 = VERTEX_POINT ( 'NONE', #18816 ) ;
#23855 = CARTESIAN_POINT ( 'NONE',  ( -10.81189881249999729, 1.324075727343319199E-15, -137.2812500020483810 ) ) ;
#23856 = CARTESIAN_POINT ( 'NONE',  ( -4.999999999999996447, 8.660254037844387298, -156.3750000040967905 ) ) ;
#23857 = CARTESIAN_POINT ( 'NONE',  ( 10.81189881249999907, 6.242252689847868297, -146.9062500020484094 ) ) ;
#23858 = EDGE_CURVE ( 'NONE', #41098, #26093, #39134, .T. ) ;
#23859 = CARTESIAN_POINT ( 'NONE',  ( 7.644554776091147741E-16, 12.48450537969573659, -185.6562500020484094 ) ) ;
#23860 = CARTESIAN_POINT ( 'NONE',  ( 10.81189881249999551, -6.242252689847874514, -85.46875000204836681 ) ) ;
#23861 = ORIENTED_EDGE ( 'NONE', *, *, #28450, .F. ) ;
#23862 = CARTESIAN_POINT ( 'NONE',  ( 7.070501591499377789E-16, 11.54700538379251284, -49.62499999999997868 ) ) ;
#23863 = CARTESIAN_POINT ( 'NONE',  ( -10.81189881249999907, -6.242252689847864744, -181.9687500020484094 ) ) ;
#23864 = CARTESIAN_POINT ( 'NONE',  ( 10.00000000000000000, 5.773502691896255534, -63.75000000409679046 ) ) ;
#23865 = CARTESIAN_POINT ( 'NONE',  ( 0.000000000000000000, 0.000000000000000000, -200.0000000000000000 ) ) ;
#23866 = DIRECTION ( 'NONE',  ( -0.000000000000000000, -0.000000000000000000, 1.000000000000000000 ) ) ;
#23867 = CARTESIAN_POINT ( 'NONE',  ( 5.405949406249992428, -9.363379034771808662, -79.78125000204838102 ) ) ;
#23868 = CARTESIAN_POINT ( 'NONE',  ( 5.405949406249992428, -9.363379034771808662, -63.28125000204837391 ) ) ;
#23869 = CARTESIAN_POINT ( 'NONE',  ( -2.121150477449813534E-15, -11.54700538379251284, -53.75000000409677625 ) ) ;
#23870 = CARTESIAN_POINT ( 'NONE',  ( 7.644554776091147741E-16, 12.48450537969573659, -12.96875000204836503 ) ) ;
#23871 = CARTESIAN_POINT ( 'NONE',  ( 9.999999999999998224, 0.000000000000000000, -29.37500000409676204 ) ) ;
#23872 = CARTESIAN_POINT ( 'NONE',  ( 5.405949406249992428, -9.363379034771808662, -178.7812500020484094 ) ) ;
#23873 = CARTESIAN_POINT ( 'NONE',  ( 7.644554776091147741E-16, 12.48450537969573659, -5.656250002048362369 ) ) ;
#23874 = CARTESIAN_POINT ( 'NONE',  ( 9.999999999999998224, 0.000000000000000000, -200.0000000000000000 ) ) ;
#23875 = CARTESIAN_POINT ( 'NONE',  ( 9.999999999999998224, 0.000000000000000000, -135.8750000040967905 ) ) ;
#23876 = ADVANCED_FACE ( 'NONE', ( #32630 ), #16182, .T. ) ;
#23877 = CARTESIAN_POINT ( 'NONE',  ( -2.121150477449813534E-15, -11.54700538379251284, -103.2500000040967763 ) ) ;
#23878 = CARTESIAN_POINT ( 'NONE',  ( 9.999999999999998224, 0.000000000000000000, -153.5000000000000000 ) ) ;
#23879 = CARTESIAN_POINT ( 'NONE',  ( 4.999999999999992006, -8.660254037844389075, -169.1250000040967905 ) ) ;
#23881 = VERTEX_POINT ( 'NONE', #12947 ) ;
#23880 = CARTESIAN_POINT ( 'NONE',  ( -2.293366432827344421E-15, -12.48450537969573659, -82.90625000204838102 ) ) ;
#23882 =( LENGTH_UNIT ( ) NAMED_UNIT ( * ) SI_UNIT ( .MILLI., .METRE. ) );
#23884 = ORIENTED_EDGE ( 'NONE', *, *, #42274, .T. ) ;
#23883 = LINE ( 'NONE', #14561, #26159 ) ;
#23885 = PRODUCT_DEFINITION_SHAPE ( 'NONE', 'NONE',  #8303 ) ;
#23886 = VERTEX_POINT ( 'NONE', #42313 ) ;
#23887 =( BOUNDED_CURVE ( )  B_SPLINE_CURVE ( 2, ( #549, #4622, #26861, #969, #30328, #14086, #11294 ),
 .UNSPECIFIED., .F., .F. ) 
 B_SPLINE_CURVE_WITH_KNOTS ( ( 3, 2, 2, 3 ),
 ( 0.1492537313432835966, 0.1504975124378109819, 0.1517412935323383116, 0.1529850746268656692 ),
 .UNSPECIFIED. ) 
 CURVE ( )  GEOMETRIC_REPRESENTATION_ITEM ( )  RATIONAL_B_SPLINE_CURVE ( ( 0.9999999999999970024, 0.8660254037844417052, 1.000000000000000000, 0.8660254037844387076, 1.000000000000000000, 0.8660254037844387076, 1.000000000000000000 ) ) 
 REPRESENTATION_ITEM ( '' )  );
#23888 = CARTESIAN_POINT ( 'NONE',  ( 5.405949406249999534, 9.363379034771803333, -25.09375000204835970 ) ) ;
#23889 = CARTESIAN_POINT ( 'NONE',  ( 5.405949406249992428, -9.363379034771808662, -12.28125000204835438 ) ) ;
#23890 = CARTESIAN_POINT ( 'NONE',  ( 10.81189881249999729, 0.000000000000000000, -73.34375000204838102 ) ) ;
#23891 = CARTESIAN_POINT ( 'NONE',  ( 5.000000000000000000, 8.660254037844385522, -164.1250000040967905 ) ) ;
#23892 = CARTESIAN_POINT ( 'NONE',  ( 9.999999999999996447, -5.773502691896262640, -44.12499999999997158 ) ) ;
#23893 = CARTESIAN_POINT ( 'NONE',  ( -2.293366432827344421E-15, -12.48450537969573659, -186.2187500020484094 ) ) ;
#23894 = AXIS2_PLACEMENT_3D ( 'NONE', #5319, #8134, #34686 ) ;
#23895 = CARTESIAN_POINT ( 'NONE',  ( -10.81189881249999907, -6.242252689847864744, -166.9687500020484094 ) ) ;
#23896 = CARTESIAN_POINT ( 'NONE',  ( 5.405949406249999534, 9.363379034771803333, -2.593750002048367254 ) ) ;
#23897 = DIRECTION ( 'NONE',  ( -0.000000000000000000, -0.000000000000000000, 1.000000000000000000 ) ) ;
#23898 = LOCAL_TIME ( 11, 57, 6.000000000000000000, #16954 ) ;
#23899 = CYLINDRICAL_SURFACE ( 'NONE', #38470, 9.999999999999998224 ) ;
#23900 = CARTESIAN_POINT ( 'NONE',  ( -9.999999999999998224, 1.224646799147353059E-15, -143.7500000000000000 ) ) ;
#23901 = CARTESIAN_POINT ( 'NONE',  ( -10.00000000000102496, 5.773502691895664007, -60.25000000409674783 ) ) ;
#23902 = EDGE_CURVE ( 'NONE', #15830, #17639, #3057, .T. ) ;
#23903 = CARTESIAN_POINT ( 'NONE',  ( 10.81189881249999551, -6.242252689847874514, -113.9687500020483810 ) ) ;
#23904 = CARTESIAN_POINT ( 'NONE',  ( -9.999999999999998224, 1.224646799147353059E-15, -200.0000000000000000 ) ) ;
#23905 = CARTESIAN_POINT ( 'NONE',  ( -10.81189881249999907, -6.242252689847864744, -90.65625000204836681 ) ) ;
#23906 = CARTESIAN_POINT ( 'NONE',  ( 10.81189881249999729, 0.000000000000000000, -100.3437500020483810 ) ) ;
#23907 = CARTESIAN_POINT ( 'NONE',  ( 7.644554776091147741E-16, 12.48450537969573659, -69.96875000204838102 ) ) ;
#23908 = CARTESIAN_POINT ( 'NONE',  ( -5.405949406249996869, 9.363379034771805109, -80.53125000204838102 ) ) ;
#23909 = CARTESIAN_POINT ( 'NONE',  ( 9.999999999999996447, -5.773502691896262640, -160.0000000040968189 ) ) ;
#23910 = CARTESIAN_POINT ( 'NONE',  ( 5.405949406249999534, 9.363379034771803333, -158.7812500020484094 ) ) ;
#23911 = CARTESIAN_POINT ( 'NONE',  ( -5.405949406249996869, 9.363379034771805109, -169.0312500020484094 ) ) ;
#23912 = CARTESIAN_POINT ( 'NONE',  ( -2.293366432827344421E-15, -12.48450537969573659, -0.2187500020483512386 ) ) ;
#23913 = CARTESIAN_POINT ( 'NONE',  ( -9.999999999999998224, 1.224646799147353059E-15, -200.0000000000000000 ) ) ;
#23914 = CARTESIAN_POINT ( 'NONE',  ( -10.81189881249999907, -6.242252689847864744, -102.4687500020483810 ) ) ;
#23915 = CARTESIAN_POINT ( 'NONE',  ( -9.999999999999998224, 1.224646799147353059E-15, -76.62500000409677625 ) ) ;
#23916 = CARTESIAN_POINT ( 'NONE',  ( 5.000000000000000000, 8.660254037844385522, -70.74999999999998579 ) ) ;
#23917 = CARTESIAN_POINT ( 'NONE',  ( -10.81189881249999729, 1.324075727343319199E-15, -6.781250002048377468 ) ) ;
#23918 = CARTESIAN_POINT ( 'NONE',  ( 9.999999999999996447, -5.773502691896262640, -92.50000000409677625 ) ) ;
#23919 = CARTESIAN_POINT ( 'NONE',  ( 5.000000000000000000, 8.660254037844385522, -115.7499999999999858 ) ) ;
#23920 = CARTESIAN_POINT ( 'NONE',  ( 5.405949406249999534, 9.363379034771803333, -103.2812500020483952 ) ) ;
#23921 = CARTESIAN_POINT ( 'NONE',  ( 10.81189881249999729, 6.242252689847867408, -82.40625000204836681 ) ) ;
#23922 = CARTESIAN_POINT ( 'NONE',  ( -4.999999999999996447, 8.660254037844387298, -75.37500000409677625 ) ) ;
#23923 = CARTESIAN_POINT ( 'NONE',  ( 9.999999999999998224, 0.000000000000000000, -168.8750000040967905 ) ) ;
#23924 = CARTESIAN_POINT ( 'NONE',  ( 10.81189881249999729, 0.000000000000000000, -32.84375000204836681 ) ) ;
#23925 = ORIENTED_EDGE ( 'NONE', *, *, #19041, .F. ) ;
#23926 = CARTESIAN_POINT ( 'NONE',  ( 5.405949406249999534, 9.363379034771803333, -197.7812500020484094 ) ) ;
#23927 = CARTESIAN_POINT ( 'NONE',  ( 10.81189881249999551, -6.242252689847874514, -27.15625000204838102 ) ) ;
#23928 = CARTESIAN_POINT ( 'NONE',  ( -5.405949406249996869, 9.363379034771805109, -15.84375000204835082 ) ) ;
#23929 = CARTESIAN_POINT ( 'NONE',  ( -5.000000000000003553, -8.660254037844383745, -14.87500000409674961 ) ) ;
#23930 = CARTESIAN_POINT ( 'NONE',  ( -9.999999999999998224, 5.773502691896259087, -7.750000004096757600 ) ) ;
#23931 = CARTESIAN_POINT ( 'NONE',  ( -2.293366432827344421E-15, -12.48450537969573659, -138.4062500020483810 ) ) ;
#23932 = CARTESIAN_POINT ( 'NONE',  ( 7.070501591499377789E-16, 11.54700538379251284, -190.6250000000000000 ) ) ;
#23933 = CARTESIAN_POINT ( 'NONE',  ( -5.000000000000003553, -8.660254037844383745, -155.8750000040967905 ) ) ;
#23935 = VERTEX_POINT ( 'NONE', #38455 ) ;
#23934 = CARTESIAN_POINT ( 'NONE',  ( -10.81189881249999729, 6.242252689847871849, -111.9062500020483810 ) ) ;
#23936 = CARTESIAN_POINT ( 'NONE',  ( 9.999999999999998224, 0.000000000000000000, -115.9999999999999858 ) ) ;
#23937 = VERTEX_POINT ( 'NONE', #41889 ) ;
#23938 = VERTEX_POINT ( 'NONE', #22693 ) ;
#23939 = CARTESIAN_POINT ( 'NONE',  ( -5.405949406250003975, -9.363379034771801557, -44.03125000204838102 ) ) ;
#23940 = COORDINATED_UNIVERSAL_TIME_OFFSET ( 6, 0, .AHEAD. ) ;
#23941 = CARTESIAN_POINT ( 'NONE',  ( -10.81189881249999729, 6.242252689847871849, -98.21875000204838102 ) ) ;
#23942 = CARTESIAN_POINT ( 'NONE',  ( 7.070501591499376803E-16, 11.54700538379251284, -128.0000000040967905 ) ) ;
#23943 = CARTESIAN_POINT ( 'NONE',  ( 7.070501591499376803E-16, 11.54700538379251284, -114.1249999999999858 ) ) ;
#23944 = CARTESIAN_POINT ( 'NONE',  ( -10.81189881249999729, 6.242252689847871849, -192.7187500020483810 ) ) ;
#23945 = CARTESIAN_POINT ( 'NONE',  ( -5.405949406250003975, -9.363379034771801557, -174.5312500020484094 ) ) ;
#23946 = CARTESIAN_POINT ( 'NONE',  ( 10.00000000000000000, 5.773502691896255534, -138.3750000000000000 ) ) ;
#23947 = EDGE_CURVE ( 'NONE', #32856, #4745, #22880, .T. ) ;
#23948 = CARTESIAN_POINT ( 'NONE',  ( -2.293366432827344421E-15, -12.48450537969573659, -126.2187500020483952 ) ) ;
#23949 = CARTESIAN_POINT ( 'NONE',  ( 10.81189881249999551, -6.242252689847874514, -91.46875000204838102 ) ) ;
#23950 = CARTESIAN_POINT ( 'NONE',  ( -9.999999999999998224, 1.224646799147353059E-15, -44.74999999999998579 ) ) ;
#23951 = CARTESIAN_POINT ( 'NONE',  ( -5.405949406249996869, 9.363379034771805109, -100.0312500020483952 ) ) ;
#23952 = CARTESIAN_POINT ( 'NONE',  ( 10.00000000000000000, 5.773502691896255534, -189.7500000040968189 ) ) ;
#23953 = CARTESIAN_POINT ( 'NONE',  ( -10.81189881249999729, 6.242252689847871849, -108.7187500020483810 ) ) ;
#23954 = CARTESIAN_POINT ( 'NONE',  ( -10.81189881249999729, 6.242252689847871849, -182.4062500020484094 ) ) ;
#23955 = CARTESIAN_POINT ( 'NONE',  ( 7.070501591499376803E-16, 11.54700538379251284, -180.1250000000000000 ) ) ;
#23956 = CARTESIAN_POINT ( 'NONE',  ( -9.999999999999998224, 1.224646799147353059E-15, -181.2500000000000284 ) ) ;
#23957 = CARTESIAN_POINT ( 'NONE',  ( 10.81189881249999551, -6.242252689847874514, -196.6562500020484379 ) ) ;
#23958 = CARTESIAN_POINT ( 'NONE',  ( 5.405949406249992428, -9.363379034771808662, -51.09375000204835260 ) ) ;
#23959 = CARTESIAN_POINT ( 'NONE',  ( 10.81189881249999729, 0.000000000000000000, -41.84375000204837391 ) ) ;
#23960 = CARTESIAN_POINT ( 'NONE',  ( 7.070501591499377789E-16, 11.54700538379251284, -168.5000000040967905 ) ) ;
#23961 = CARTESIAN_POINT ( 'NONE',  ( -10.81189881249999729, 6.242252689847871849, -12.90625000204835970 ) ) ;
#23962 = CARTESIAN_POINT ( 'NONE',  ( -10.81189881249999907, -6.242252689847864744, -18.46875000204836681 ) ) ;
#23963 = DIRECTION ( 'NONE',  ( -1.000000000000000000, 0.000000000000000000, 0.000000000000000000 ) ) ;
#23964 = CARTESIAN_POINT ( 'NONE',  ( 10.81189881249999551, -6.242252689847874514, -128.9687500020483810 ) ) ;
#23965 = CARTESIAN_POINT ( 'NONE',  ( -4.999999999999996447, 8.660254037844387298, -94.49999999999998579 ) ) ;
#23966 = CARTESIAN_POINT ( 'NONE',  ( 7.644554776091147741E-16, 12.48450537969573659, -29.65625000204835615 ) ) ;
#23967 = CARTESIAN_POINT ( 'NONE',  ( -9.999999999999998224, 1.224646799147353059E-15, -101.7500000000000000 ) ) ;
#23968 = CARTESIAN_POINT ( 'NONE',  ( 5.000000000000000000, 8.660254037844385522, -63.24999999999997158 ) ) ;
#23969 = CARTESIAN_POINT ( 'NONE',  ( 5.405949406249992428, -9.363379034771808662, -126.2812500020483668 ) ) ;
#23970 = CARTESIAN_POINT ( 'NONE',  ( 7.644554776091147741E-16, 12.48450537969573659, -104.6562500020483810 ) ) ;
#23971 = EDGE_CURVE ( 'NONE', #39100, #41044, #27281, .T. ) ;
#23972 = EDGE_LOOP ( 'NONE', ( #25886, #26840, #24899, #3760 ) ) ;
#23973 = DIRECTION ( 'NONE',  ( 1.000000000000000000, 0.000000000000000000, 0.000000000000000000 ) ) ;
#23974 = CARTESIAN_POINT ( 'NONE',  ( 4.999999999999992006, -8.660254037844389075, -101.6250000040967905 ) ) ;
#23975 = CARTESIAN_POINT ( 'NONE',  ( -9.999999999999998224, 1.224646799147353059E-15, -91.24999999999998579 ) ) ;
#23976 = CARTESIAN_POINT ( 'NONE',  ( -2.293366432827344421E-15, -12.48450537969573659, -57.21875000204836681 ) ) ;
#23977 = ORIENTED_EDGE ( 'NONE', *, *, #39591, .T. ) ;
#23978 = CARTESIAN_POINT ( 'NONE',  ( -9.999999999999998224, 5.773502691896259087, -35.87499999999995737 ) ) ;
#23979 = CIRCLE ( 'NONE', #1235, 35.00000000000000711 ) ;
#23980 = CARTESIAN_POINT ( 'NONE',  ( 10.81189881249999551, -6.242252689847874514, -33.15625000204835970 ) ) ;
#23981 = CARTESIAN_POINT ( 'NONE',  ( 5.000000000000000000, 8.660254037844385522, -35.12500000409676915 ) ) ;
#23982 =( BOUNDED_CURVE ( )  B_SPLINE_CURVE ( 2, ( #9632, #26045, #16938, #39197, #39611, #30135, #26462 ),
 .UNSPECIFIED., .F., .F. ) 
 B_SPLINE_CURVE_WITH_KNOTS ( ( 3, 2, 2, 3 ),
 ( 0.2350746268656717097, 0.2363184079601990950, 0.2375621890547264525, 0.2388059701492538378 ),
 .UNSPECIFIED. ) 
 CURVE ( )  GEOMETRIC_REPRESENTATION_ITEM ( )  RATIONAL_B_SPLINE_CURVE ( ( 0.9999999999999940048, 0.8660254037844447028, 1.000000000000000000, 0.8660254037844387076, 1.000000000000000000, 0.8660254037844267172, 1.000000000000011990 ) ) 
 REPRESENTATION_ITEM ( '' )  );
#23983 = CARTESIAN_POINT ( 'NONE',  ( -10.00000000000000000, -5.773502691896251982, -25.50000000409677270 ) ) ;
#23984 = CARTESIAN_POINT ( 'NONE',  ( -10.81189881249999729, 6.242252689847871849, -132.9062500020483810 ) ) ;
#23985 = CARTESIAN_POINT ( 'NONE',  ( -4.999999999999996447, 8.660254037844387298, -162.3750000040967905 ) ) ;
#23986 = VERTEX_POINT ( 'NONE', #41680 ) ;
#23988 = ORIENTED_EDGE ( 'NONE', *, *, #31063, .F. ) ;
#23987 = EDGE_LOOP ( 'NONE', ( #36870, #10481, #5817, #5194 ) ) ;
#23989 = CARTESIAN_POINT ( 'NONE',  ( -4.999999999999996447, 8.660254037844387298, -107.9999999999999858 ) ) ;
#23990 = CARTESIAN_POINT ( 'NONE',  ( 0.000000000000000000, 0.000000000000000000, -200.0000000000000000 ) ) ;
#23992 = ADVANCED_FACE ( 'NONE', ( #2844 ), #5451, .T. ) ;
#23991 = CARTESIAN_POINT ( 'NONE',  ( -10.81189881249999907, -6.242252689847864744, -166.9687500020484094 ) ) ;
#23993 = CARTESIAN_POINT ( 'NONE',  ( -10.81189881249999729, 6.242252689847871849, -194.4062500020484094 ) ) ;
#23994 = CARTESIAN_POINT ( 'NONE',  ( 5.405949406249999534, 9.363379034771803333, -13.09375000204834905 ) ) ;
#23995 = CARTESIAN_POINT ( 'NONE',  ( 7.070501591499376803E-16, 11.54700538379251284, -171.1250000000000000 ) ) ;
#23996 = VECTOR ( 'NONE', #4189, 1000.000000000000114 ) ;
#23997 = CARTESIAN_POINT ( 'NONE',  ( 5.405949406249999534, 9.363379034771803333, -146.5937500020483810 ) ) ;
#23998 = VECTOR ( 'NONE', #9656, 1000.000000000000000 ) ;
#23999 = CARTESIAN_POINT ( 'NONE',  ( -2.293366432827344421E-15, -12.48450537969573659, -135.2187500020483810 ) ) ;
#24000 = CARTESIAN_POINT ( 'NONE',  ( -10.81189881249999729, 1.324075727343319199E-15, -105.7812500020483810 ) ) ;
#24001 = CARTESIAN_POINT ( 'NONE',  ( -10.81189881249999729, 6.242252689847871849, -119.2187500020483810 ) ) ;
#24002 = CARTESIAN_POINT ( 'NONE',  ( -9.999999999999998224, 5.773502691896259087, -192.2500000040968189 ) ) ;
#24003 = CARTESIAN_POINT ( 'NONE',  ( 7.644554776091147741E-16, 12.48450537969573659, -121.1562500020483952 ) ) ;
#24004 = CARTESIAN_POINT ( 'NONE',  ( -10.81189881249999729, 1.324075727343319199E-15, -11.09375000204834727 ) ) ;
#24005 = CARTESIAN_POINT ( 'NONE',  ( 10.81189881249999551, -6.242252689847874514, -133.4687500020483810 ) ) ;
#24006 = CARTESIAN_POINT ( 'NONE',  ( -24.99999999999999645, 0.000000000000000000, -169.9999999999999716 ) ) ;
#24007 = CARTESIAN_POINT ( 'NONE',  ( -10.00000000000076916, 5.773502691895813221, -109.7500000040967620 ) ) ;
#24008 = CARTESIAN_POINT ( 'NONE',  ( 4.999999999999992006, -8.660254037844389075, -158.2500000000000000 ) ) ;
#24009 = CARTESIAN_POINT ( 'NONE',  ( -5.000000000000003553, -8.660254037844383745, -23.49999999999996447 ) ) ;
#24010 = CARTESIAN_POINT ( 'NONE',  ( -5.405949406249996869, 9.363379034771805109, -74.34375000204838102 ) ) ;
#24011 = CARTESIAN_POINT ( 'NONE',  ( -10.81189881249999729, 1.324075727343319199E-15, -62.09375000204836681 ) ) ;
#24012 = DIRECTION ( 'NONE',  ( -0.000000000000000000, -0.000000000000000000, -1.000000000000000000 ) ) ;
#24013 = CARTESIAN_POINT ( 'NONE',  ( 7.644554776091147741E-16, 12.48450537969573659, -37.15625000204836681 ) ) ;
#24014 = CARTESIAN_POINT ( 'NONE',  ( -10.81189881249999907, -6.242252689847864744, -45.46875000204835970 ) ) ;
#24015 = CARTESIAN_POINT ( 'NONE',  ( -9.999999999999998224, 1.224646799147353059E-15, -139.6250000040967905 ) ) ;
#24016 = CARTESIAN_POINT ( 'NONE',  ( 7.644554776091147741E-16, 12.48450537969573659, -152.4687500020483810 ) ) ;
#24017 = CARTESIAN_POINT ( 'NONE',  ( -9.999999999999998224, 1.224646799147353059E-15, -127.2499999999999716 ) ) ;
#24018 = CARTESIAN_POINT ( 'NONE',  ( 5.405949406249992428, -9.363379034771808662, -133.7812500020483810 ) ) ;
#24019 = CARTESIAN_POINT ( 'NONE',  ( 5.000000000000000000, 8.660254037844385522, -94.74999999999998579 ) ) ;
#24020 = CARTESIAN_POINT ( 'NONE',  ( -9.999999999999998224, 1.224646799147353059E-15, -80.74999999999998579 ) ) ;
#24021 = CARTESIAN_POINT ( 'NONE',  ( 10.81189881249999729, 0.000000000000000000, -16.53125000204835970 ) ) ;
#24022 = VERTEX_POINT ( 'NONE', #35862 ) ;
#24023 =( BOUNDED_CURVE ( )  B_SPLINE_CURVE ( 2, ( #15977, #35233, #35445, #6085, #35654, #5871, #42522 ),
 .UNSPECIFIED., .F., .F. ) 
 B_SPLINE_CURVE_WITH_KNOTS ( ( 3, 2, 2, 3 ),
 ( 0.007462686567164185901, 0.008706467661691551230, 0.009950248756218915691, 0.01119402985074628015 ),
 .UNSPECIFIED. ) 
 CURVE ( )  GEOMETRIC_REPRESENTATION_ITEM ( )  RATIONAL_B_SPLINE_CURVE ( ( 0.9999999999999993339, 0.8660254037844394848, 1.000000000000000000, 0.8660254037844387076, 1.000000000000000000, 0.8660254037844373753, 1.000000000000001332 ) ) 
 REPRESENTATION_ITEM ( '' )  );
#24024 = CARTESIAN_POINT ( 'NONE',  ( -5.405949406249996869, 9.363379034771805109, -110.5312500020483810 ) ) ;
#24025 = CARTESIAN_POINT ( 'NONE',  ( -2.121150477449813534E-15, -11.54700538379251284, -127.2500000040967905 ) ) ;
#24026 = CARTESIAN_POINT ( 'NONE',  ( -9.999999999999998224, 1.224646799147353059E-15, -154.2500000000000000 ) ) ;
#24027 = CARTESIAN_POINT ( 'NONE',  ( -9.999999999999998224, 1.224646799147353059E-15, -36.12500000409676915 ) ) ;
#24028 = EDGE_CURVE ( 'NONE', #24638, #32801, #12118, .T. ) ;
#24029 = DIRECTION ( 'NONE',  ( -0.000000000000000000, -0.000000000000000000, -1.000000000000000000 ) ) ;
#24030 = CARTESIAN_POINT ( 'NONE',  ( 7.644554776091147741E-16, 12.48450537969573659, -55.15625000204838102 ) ) ;
#24031 =( BOUNDED_CURVE ( )  B_SPLINE_CURVE ( 2, ( #4766, #27648, #14235, #37572, #10800, #34563, #8015 ),
 .UNSPECIFIED., .F., .F. ) 
 B_SPLINE_CURVE_WITH_KNOTS ( ( 3, 2, 2, 3 ),
 ( 0.1194029850746269744, 0.1206467661691543042, 0.1218905472636816062, 0.1231343283582089221 ),
 .UNSPECIFIED. ) 
 CURVE ( )  GEOMETRIC_REPRESENTATION_ITEM ( )  RATIONAL_B_SPLINE_CURVE ( ( 0.9999999999999880096, 0.8660254037844506980, 1.000000000000000000, 0.8660254037844387076, 1.000000000000000000, 0.8660254037844417052, 0.9999999999999970024 ) ) 
 REPRESENTATION_ITEM ( '' )  );
#24032 = CARTESIAN_POINT ( 'NONE',  ( 9.999999999999479527, 5.773502691896553074, -76.87499999999997158 ) ) ;
#24033 = CARTESIAN_POINT ( 'NONE',  ( -10.81189881249999729, 6.242252689847871849, -155.4062500020483810 ) ) ;
#24034 = CARTESIAN_POINT ( 'NONE',  ( 10.81189881249999551, -6.242252689847874514, -137.9687500020483810 ) ) ;
#24035 = CARTESIAN_POINT ( 'NONE',  ( 9.999999999999998224, 0.000000000000000000, -165.8750000040967905 ) ) ;
#24036 = VECTOR ( 'NONE', #19525, 1000.000000000000000 ) ;
#24037 = VERTEX_POINT ( 'NONE', #25729 ) ;
#24038 = CARTESIAN_POINT ( 'NONE',  ( -4.999999999999996447, 8.660254037844387298, -177.0000000000000000 ) ) ;
#24039 = ORIENTED_EDGE ( 'NONE', *, *, #1047, .F. ) ;
#24040 = ORIENTED_EDGE ( 'NONE', *, *, #28585, .F. ) ;
#24042 = VERTEX_POINT ( 'NONE', #6296 ) ;
#24041 = CARTESIAN_POINT ( 'NONE',  ( 5.405949406249992428, -9.363379034771808662, -108.0937500020483810 ) ) ;
#24043 = CARTESIAN_POINT ( 'NONE',  ( -2.293366432827344421E-15, -12.48450537969573659, -192.2187500020484379 ) ) ;
#24044 = CARTESIAN_POINT ( 'NONE',  ( -5.405949406249996869, 9.363379034771805109, -35.34375000204836681 ) ) ;
#24045 = CARTESIAN_POINT ( 'NONE',  ( 7.070501591499376803E-16, 11.54700538379251284, -153.5000000040967905 ) ) ;
#24046 = DIRECTION ( 'NONE',  ( 1.000000000000000000, 0.000000000000000000, 0.000000000000000000 ) ) ;
#24047 = CARTESIAN_POINT ( 'NONE',  ( -10.81189881249999729, 1.324075727343319199E-15, -170.0937500020484094 ) ) ;
#24048 = CARTESIAN_POINT ( 'NONE',  ( 10.81189881249999729, 0.000000000000000000, -161.8437500020484094 ) ) ;
#24049 = DIRECTION ( 'NONE',  ( -0.7071067811865451302, 0.000000000000000000, -0.7071067811865500152 ) ) ;
#24050 = CARTESIAN_POINT ( 'NONE',  ( -5.405949406249996869, 9.363379034771805109, -138.8437500020484094 ) ) ;
#24051 = CARTESIAN_POINT ( 'NONE',  ( 5.405949406249999534, 9.363379034771803333, -155.5937500020483810 ) ) ;
#24052 = CARTESIAN_POINT ( 'NONE',  ( -5.000000000000003553, -8.660254037844383745, -155.5000000000000000 ) ) ;
#24053 = CARTESIAN_POINT ( 'NONE',  ( -4.999999999999996447, 8.660254037844387298, -66.37500000409676204 ) ) ;
#24054 = CARTESIAN_POINT ( 'NONE',  ( 7.070501591499377789E-16, 11.54700538379251284, -175.6250000000000000 ) ) ;
#24055 = CARTESIAN_POINT ( 'NONE',  ( -10.81189881249999729, 1.324075727343319199E-15, -86.09375000204836681 ) ) ;
#24056 = CARTESIAN_POINT ( 'NONE',  ( 10.00000000000051159, -5.773502691895965988, -72.62499999999995737 ) ) ;
#24057 = CARTESIAN_POINT ( 'NONE',  ( 5.405949406249992428, -9.363379034771808662, -63.28125000204837391 ) ) ;
#24058 = CARTESIAN_POINT ( 'NONE',  ( 4.999999999999992006, -8.660254037844389075, -124.1250000040967905 ) ) ;
#24059 = CARTESIAN_POINT ( 'NONE',  ( 5.405949406249999534, 9.363379034771803333, -179.5937500020484094 ) ) ;
#24060 = CARTESIAN_POINT ( 'NONE',  ( -10.81189881249999729, 1.324075727343319199E-15, -125.2812500020483668 ) ) ;
#24061 = VECTOR ( 'NONE', #2368, 1000.000000000000000 ) ;
#24062 = CARTESIAN_POINT ( 'NONE',  ( 10.81189881249999729, 6.242252689847867408, -152.9062500020483810 ) ) ;
#24063 = CARTESIAN_POINT ( 'NONE',  ( 5.000000000000000000, 8.660254037844385522, -115.7499999999999858 ) ) ;
#24064 = CARTESIAN_POINT ( 'NONE',  ( -10.81189881249999907, -6.242252689847864744, -54.65625000204838102 ) ) ;
#24065 = CARTESIAN_POINT ( 'NONE',  ( -9.999999999999998224, 5.773502691896259087, -130.7500000040967905 ) ) ;
#24066 = CARTESIAN_POINT ( 'NONE',  ( 4.999999999999992006, -8.660254037844389075, -107.2499999999999858 ) ) ;
#24067 = ORIENTED_EDGE ( 'NONE', *, *, #269, .T. ) ;
#24068 = CARTESIAN_POINT ( 'NONE',  ( 7.644554776091147741E-16, 12.48450537969573659, -136.1562500020484094 ) ) ;
#24069 = CARTESIAN_POINT ( 'NONE',  ( 9.999999999999998224, 0.000000000000000000, -147.8750000040967905 ) ) ;
#24070 = CARTESIAN_POINT ( 'NONE',  ( 10.81189881249999551, -6.242252689847874514, -145.6562500020484094 ) ) ;
#24071 = VECTOR ( 'NONE', #33418, 1000.000000000000000 ) ;
#24072 = CARTESIAN_POINT ( 'NONE',  ( 7.644554776091147741E-16, 12.48450537969573659, -190.1562500020484094 ) ) ;
#24073 = ORIENTED_EDGE ( 'NONE', *, *, #18562, .T. ) ;
#24074 = CARTESIAN_POINT ( 'NONE',  ( -4.999999999999996447, 8.660254037844387298, -46.49999999999998579 ) ) ;
#24075 = CARTESIAN_POINT ( 'NONE',  ( 10.81189881249999551, -6.242252689847874514, -179.9687500020484094 ) ) ;
#24076 = CARTESIAN_POINT ( 'NONE',  ( -9.999999999999998224, 5.773502691896259087, -60.25000000409677625 ) ) ;
#24077 = EDGE_CURVE ( 'NONE', #28118, #258, #11011, .T. ) ;
#24078 = CARTESIAN_POINT ( 'NONE',  ( -4.999999999999996447, 8.660254037844387298, -178.8750000040967905 ) ) ;
#24079 = EDGE_CURVE ( 'NONE', #31861, #15525, #21487, .T. ) ;
#24080 = CARTESIAN_POINT ( 'NONE',  ( -10.81189881249999729, 1.324075727343319199E-15, -74.28125000204838102 ) ) ;
#24081 = CARTESIAN_POINT ( 'NONE',  ( -5.405949406250003975, -9.363379034771801557, -60.53125000204836681 ) ) ;
#24082 = CARTESIAN_POINT ( 'NONE',  ( -5.000000000000003553, -8.660254037844383745, -53.87500000409675494 ) ) ;
#24083 = VECTOR ( 'NONE', #32405, 1000.000000000000000 ) ;
#24084 = CARTESIAN_POINT ( 'NONE',  ( 10.81189881249999907, 6.242252689847868297, -10.21875000204835970 ) ) ;
#24085 = CARTESIAN_POINT ( 'NONE',  ( -9.999999999999998224, 1.224646799147353059E-15, -157.6250000040967905 ) ) ;
#24086 = CARTESIAN_POINT ( 'NONE',  ( 5.405949406249992428, -9.363379034771808662, -180.2812500020484094 ) ) ;
#24087 = CARTESIAN_POINT ( 'NONE',  ( -5.405949406249996869, 9.363379034771805109, -2.531250002048373915 ) ) ;
#24088 = CARTESIAN_POINT ( 'NONE',  ( -9.999999999999998224, 1.224646799147353059E-15, -137.7499999999999716 ) ) ;
#24089 = CARTESIAN_POINT ( 'NONE',  ( 5.000000000000000000, 8.660254037844385522, -138.6250000040967905 ) ) ;
#24090 = LINE ( 'NONE', #31212, #21076 ) ;
#24091 = CARTESIAN_POINT ( 'NONE',  ( -9.999999999999998224, 1.224646799147353059E-15, -200.0000000000000000 ) ) ;
#24093 = ORIENTED_EDGE ( 'NONE', *, *, #18806, .F. ) ;
#24092 = CARTESIAN_POINT ( 'NONE',  ( 10.81189881249999907, 6.242252689847868297, -83.90625000204836681 ) ) ;
#24094 = CARTESIAN_POINT ( 'NONE',  ( 0.000000000000000000, 0.000000000000000000, 0.000000000000000000 ) ) ;
#24095 = EDGE_CURVE ( 'NONE', #36957, #17005, #41644, .T. ) ;
#24097 = ORIENTED_EDGE ( 'NONE', *, *, #30528, .F. ) ;
#24096 = LINE ( 'NONE', #5089, #4098 ) ;
#24098 =( BOUNDED_CURVE ( )  B_SPLINE_CURVE ( 2, ( #26016, #35936, #29250, #29679, #7009, #6377, #3137 ),
 .UNSPECIFIED., .F., .F. ) 
 B_SPLINE_CURVE_WITH_KNOTS ( ( 3, 2, 2, 3 ),
 ( 0.8880597014925376564, 0.8893034825870650417, 0.8905472636815924270, 0.8917910447761197013 ),
 .UNSPECIFIED. ) 
 CURVE ( )  GEOMETRIC_REPRESENTATION_ITEM ( )  RATIONAL_B_SPLINE_CURVE ( ( 0.9999999999999641398, 0.8660254037844745678, 1.000000000000000000, 0.8660254037844387076, 1.000000000000000000, 0.8660254037844028474, 1.000000000000035971 ) ) 
 REPRESENTATION_ITEM ( '' )  );
#24099 = VERTEX_POINT ( 'NONE', #23754 ) ;
#24100 = CARTESIAN_POINT ( 'NONE',  ( 7.644554776091147741E-16, 12.48450537969573659, -39.96875000204835970 ) ) ;
#24101 = CARTESIAN_POINT ( 'NONE',  ( 5.405949406249992428, -9.363379034771808662, -27.09375000204835970 ) ) ;
#24102 = CARTESIAN_POINT ( 'NONE',  ( 5.405949406249992428, -9.363379034771808662, -16.78125000204835970 ) ) ;
#24103 = AXIS2_PLACEMENT_3D ( 'NONE', #11914, #38255, #28773 ) ;
#24104 = CARTESIAN_POINT ( 'NONE',  ( 5.405949406249992428, -9.363379034771808662, -63.09375000204836681 ) ) ;
#24105 = CARTESIAN_POINT ( 'NONE',  ( 4.999999999999992006, -8.660254037844389075, -131.2499999999999716 ) ) ;
#24106 = CARTESIAN_POINT ( 'NONE',  ( -2.121150477449813534E-15, -11.54700538379251284, -42.87499999999997158 ) ) ;
#24107 = EDGE_CURVE ( 'NONE', #39101, #41597, #15420, .T. ) ;
#24108 = CARTESIAN_POINT ( 'NONE',  ( -2.293366432827344421E-15, -12.48450537969573659, -184.7187500020484094 ) ) ;
#24109 = CARTESIAN_POINT ( 'NONE',  ( 7.644554776091147741E-16, 12.48450537969573659, -164.4687500020483810 ) ) ;
#24110 = CARTESIAN_POINT ( 'NONE',  ( -2.293366432827344421E-15, -12.48450537969573659, -3.218750002048363257 ) ) ;
#24111 = CARTESIAN_POINT ( 'NONE',  ( 9.999999999999998224, 0.000000000000000000, -192.5000000000000000 ) ) ;
#24112 = VECTOR ( 'NONE', #13310, 1000.000000000000000 ) ;
#24113 = CARTESIAN_POINT ( 'NONE',  ( -9.999999999999998224, 1.224646799147353059E-15, -146.7500000000000000 ) ) ;
#24114 = CARTESIAN_POINT ( 'NONE',  ( 10.00000000000000000, 5.773502691896255534, 0.7499999959032597197 ) ) ;
#24115 = CARTESIAN_POINT ( 'NONE',  ( 10.00000000000000000, 5.773502691896255534, -199.8750000000000284 ) ) ;
#24116 = CARTESIAN_POINT ( 'NONE',  ( 5.405949406249999534, 9.363379034771803333, -112.0937500020483810 ) ) ;
#24117 = CARTESIAN_POINT ( 'NONE',  ( 7.070501591499376803E-16, 11.54700538379251284, -15.12499999999997691 ) ) ;
#24118 = CARTESIAN_POINT ( 'NONE',  ( -5.405949406249996869, 9.363379034771805109, -89.53125000204838102 ) ) ;
#24119 = CARTESIAN_POINT ( 'NONE',  ( -5.405949406249996869, 9.363379034771805109, -102.8437500020483810 ) ) ;
#24120 = CARTESIAN_POINT ( 'NONE',  ( 10.81189881249999729, 0.000000000000000000, -70.34375000204836681 ) ) ;
#24121 = CARTESIAN_POINT ( 'NONE',  ( -5.405949406250003975, -9.363379034771801557, -80.03125000204838102 ) ) ;
#24122 = CARTESIAN_POINT ( 'NONE',  ( -4.999999999999996447, 8.660254037844387298, -151.8750000040967905 ) ) ;
#24123 = CARTESIAN_POINT ( 'NONE',  ( 9.999999999999996447, -5.773502691896262640, -131.1250000000000000 ) ) ;
#24124 = CARTESIAN_POINT ( 'NONE',  ( 5.405949406249992428, -9.363379034771808662, -156.2812500020484094 ) ) ;
#24125 = CARTESIAN_POINT ( 'NONE',  ( -10.81189881249999729, 6.242252689847871849, -171.9062500020484094 ) ) ;
#24126 = CARTESIAN_POINT ( 'NONE',  ( 9.999999999999998224, 0.000000000000000000, -153.8750000040967905 ) ) ;
#24127 = CARTESIAN_POINT ( 'NONE',  ( -10.81189881249999729, 6.242252689847871849, -105.7187500020483668 ) ) ;
#24128 = CARTESIAN_POINT ( 'NONE',  ( -10.00000000000154188, 5.773502691895366468, -10.37499999999991296 ) ) ;
#24129 = CARTESIAN_POINT ( 'NONE',  ( -9.999999999999998224, 1.224646799147353059E-15, -70.24999999999998579 ) ) ;
#24130 = CARTESIAN_POINT ( 'NONE',  ( -10.81189881249999907, -6.242252689847864744, -2.156250002048359704 ) ) ;
#24131 = CARTESIAN_POINT ( 'NONE',  ( -4.999999999999996447, 8.660254037844387298, -81.37500000409677625 ) ) ;
#24132 = ADVANCED_FACE ( 'NONE', ( #26567 ), #3266, .T. ) ;
#24133 = CARTESIAN_POINT ( 'NONE',  ( -9.999999999999479527, -5.773502691896549521, -96.00000000409677625 ) ) ;
#24134 = CARTESIAN_POINT ( 'NONE',  ( 10.81189881249999907, 6.242252689847868297, -97.40625000204839523 ) ) ;
#24135 = CARTESIAN_POINT ( 'NONE',  ( 7.644554776091147741E-16, 12.48450537969573659, -86.65625000204838102 ) ) ;
#24136 = ADVANCED_FACE ( 'NONE', ( #10152, #7136, #22911, #23333 ), #36907, .T. ) ;
#24137 = CARTESIAN_POINT ( 'NONE',  ( -4.999999999999996447, 8.660254037844387298, -72.37500000409677625 ) ) ;
#24138 = CARTESIAN_POINT ( 'NONE',  ( 9.999999999999479527, 5.773502691896553074, -113.2500000040967620 ) ) ;
#24139 = CARTESIAN_POINT ( 'NONE',  ( 10.81189881249999729, 0.000000000000000000, -37.34375000204836681 ) ) ;
#24140 = EDGE_LOOP ( 'NONE', ( #22645, #13968, #40399 ) ) ;
#24141 = CARTESIAN_POINT ( 'NONE',  ( 9.999999999999998224, 0.000000000000000000, -4.999999999999976907 ) ) ;
#24142 = CIRCLE ( 'NONE', #10333, 9.999999999999998224 ) ;
#24143 = EDGE_CURVE ( 'NONE', #25900, #5096, #19832, .T. ) ;
#24144 = CARTESIAN_POINT ( 'NONE',  ( -10.81189881249999907, -6.242252689847864744, -32.15625000204835970 ) ) ;
#24145 = CARTESIAN_POINT ( 'NONE',  ( 7.644554776091147741E-16, 12.48450537969573659, -12.96875000204836148 ) ) ;
#24146 = CARTESIAN_POINT ( 'NONE',  ( -2.121150477449813534E-15, -11.54700538379251284, -94.25000000409677625 ) ) ;
#24147 = CARTESIAN_POINT ( 'NONE',  ( 7.070501591499377789E-16, 11.54700538379251284, -8.000000004096758488 ) ) ;
#24148 = CARTESIAN_POINT ( 'NONE',  ( -10.81189881249999729, 1.324075727343319199E-15, -131.2812500020483810 ) ) ;
#24149 =( BOUNDED_CURVE ( )  B_SPLINE_CURVE ( 2, ( #10243, #39811, #36372, #23006, #29908, #23215, #29694 ),
 .UNSPECIFIED., .F., .F. ) 
 B_SPLINE_CURVE_WITH_KNOTS ( ( 3, 2, 2, 3 ),
 ( 0.7723880597014927130, 0.7736318407960200982, 0.7748756218905473725, 0.7761194029850747578 ),
 .UNSPECIFIED. ) 
 CURVE ( )  GEOMETRIC_REPRESENTATION_ITEM ( )  RATIONAL_B_SPLINE_CURVE ( ( 0.9999999999999761302, 0.8660254037844625774, 1.000000000000000000, 0.8660254037844387076, 1.000000000000000000, 0.8660254037844267172, 1.000000000000011990 ) ) 
 REPRESENTATION_ITEM ( '' )  );
#24150 = CARTESIAN_POINT ( 'NONE',  ( -2.121150477449813534E-15, -11.54700538379251284, -180.8750000000000000 ) ) ;
#24152 = EDGE_LOOP ( 'NONE', ( #15721, #14065, #18292, #1006 ) ) ;
#24151 = CARTESIAN_POINT ( 'NONE',  ( -10.81189881249999729, 1.324075727343319199E-15, -110.2812500020483810 ) ) ;
#24153 = CARTESIAN_POINT ( 'NONE',  ( -9.999999999999998224, 1.224646799147353059E-15, -154.6250000040967905 ) ) ;
#24154 = ORIENTED_EDGE ( 'NONE', *, *, #34175, .F. ) ;
#24155 = ORIENTED_EDGE ( 'NONE', *, *, #20273, .F. ) ;
#24156 = EDGE_CURVE ( 'NONE', #32999, #8390, #16824, .T. ) ;
#24157 = CARTESIAN_POINT ( 'NONE',  ( 5.405949406249999534, 9.363379034771803333, -37.28125000204837391 ) ) ;
#24158 = DATE_TIME_ROLE ( 'classification_date' ) ;
#24159 = CARTESIAN_POINT ( 'NONE',  ( -5.405949406250003975, -9.363379034771801557, -87.34375000204836681 ) ) ;
#24160 = CARTESIAN_POINT ( 'NONE',  ( 9.999999999999998224, 0.000000000000000000, -200.0000000000000000 ) ) ;
#24161 = FACE_OUTER_BOUND ( 'NONE', #13891, .T. ) ;
#24162 = CARTESIAN_POINT ( 'NONE',  ( -5.405949406249996869, 9.363379034771805109, -169.0312500020484094 ) ) ;
#24163 = CARTESIAN_POINT ( 'NONE',  ( 5.000000000000000000, 8.660254037844385522, -58.74999999999997158 ) ) ;
#24164 = CARTESIAN_POINT ( 'NONE',  ( 10.81189881249999729, 6.242252689847867408, -122.7187500020483952 ) ) ;
#24165 = CARTESIAN_POINT ( 'NONE',  ( -10.81189881249999907, -6.242252689847864744, -96.46875000204838102 ) ) ;
#24166 = CARTESIAN_POINT ( 'NONE',  ( 10.81189881249999551, -6.242252689847874514, -4.656250002048354375 ) ) ;
#24167 = CARTESIAN_POINT ( 'NONE',  ( 4.999999999999992006, -8.660254037844389075, -44.24999999999998579 ) ) ;
#24168 = CARTESIAN_POINT ( 'NONE',  ( 10.81189881249999551, -6.242252689847874514, -97.65625000204839523 ) ) ;
#24169 = CARTESIAN_POINT ( 'NONE',  ( 9.999999999999998224, 0.000000000000000000, -176.3750000040967905 ) ) ;
#24170 = CARTESIAN_POINT ( 'NONE',  ( 7.644554776091147741E-16, 12.48450537969573659, -108.9687500020483668 ) ) ;
#24171 = CARTESIAN_POINT ( 'NONE',  ( 10.81189881249999729, 0.000000000000000000, -178.5312500020483810 ) ) ;
#24172 = CARTESIAN_POINT ( 'NONE',  ( -10.00000000000076916, 5.773502691895813221, -107.8749999999999574 ) ) ;
#24173 = CARTESIAN_POINT ( 'NONE',  ( 5.405949406249999534, 9.363379034771803333, -179.7812500020484094 ) ) ;
#24174 = CARTESIAN_POINT ( 'NONE',  ( 9.999999999999996447, -5.773502691896262640, -0.6249999999999588107 ) ) ;
#24175 = CARTESIAN_POINT ( 'NONE',  ( 10.81189881249999551, -6.242252689847874514, -52.46875000204836681 ) ) ;
#24176 = CARTESIAN_POINT ( 'NONE',  ( 7.644554776091147741E-16, 12.48450537969573659, -42.96875000204835970 ) ) ;
#24177 = CARTESIAN_POINT ( 'NONE',  ( -9.999999999999998224, 5.773502691896259087, -175.7500000040967905 ) ) ;
#24178 = CARTESIAN_POINT ( 'NONE',  ( -10.81189881249999729, 1.324075727343319199E-15, -6.781250002048377468 ) ) ;
#24179 = CARTESIAN_POINT ( 'NONE',  ( -2.293366432827344421E-15, -12.48450537969573659, -19.71875000204837036 ) ) ;
#24180 = CARTESIAN_POINT ( 'NONE',  ( 7.070501591499376803E-16, 11.54700538379251284, -145.6250000000000000 ) ) ;
#24181 = CARTESIAN_POINT ( 'NONE',  ( -5.405949406250003975, -9.363379034771801557, -130.8437500020484094 ) ) ;
#24182 = CARTESIAN_POINT ( 'NONE',  ( 4.999999999999992006, -8.660254037844389075, -101.2499999999999858 ) ) ;
#24183 = CARTESIAN_POINT ( 'NONE',  ( -10.81189881249999729, 6.242252689847871849, -26.40625000204838102 ) ) ;
#24184 = CARTESIAN_POINT ( 'NONE',  ( 4.999999999999992006, -8.660254037844389075, -115.1250000040967905 ) ) ;
#24185 = CARTESIAN_POINT ( 'NONE',  ( -9.999999999999998224, 1.224646799147353059E-15, -169.2500000000000000 ) ) ;
#24186 = CARTESIAN_POINT ( 'NONE',  ( -10.00000000000000000, -5.773502691896251982, -59.62500000000000000 ) ) ;
#24187 = CARTESIAN_POINT ( 'NONE',  ( -5.405949406249996869, 9.363379034771805109, -127.0312500020483952 ) ) ;
#24188 = CARTESIAN_POINT ( 'NONE',  ( -5.405949406250003975, -9.363379034771801557, -110.0312500020483810 ) ) ;
#24189 = ORIENTED_EDGE ( 'NONE', *, *, #35192, .T. ) ;
#24190 = DIRECTION ( 'NONE',  ( -0.000000000000000000, -0.000000000000000000, 1.000000000000000000 ) ) ;
#24191 = CARTESIAN_POINT ( 'NONE',  ( 10.00000000000000000, 5.773502691896255534, -99.75000000409679046 ) ) ;
#24192 = LINE ( 'NONE', #11632, #23615 ) ;
#24193 = CARTESIAN_POINT ( 'NONE',  ( -10.81189881249999729, 6.242252689847871849, -164.4062500020484094 ) ) ;
#24194 = CARTESIAN_POINT ( 'NONE',  ( 5.405949406249992428, -9.363379034771808662, -61.59375000204836681 ) ) ;
#24195 = VERTEX_POINT ( 'NONE', #20500 ) ;
#24196 = CARTESIAN_POINT ( 'NONE',  ( 4.999999999999992006, -8.660254037844389075, -26.24999999999996803 ) ) ;
#24197 = CARTESIAN_POINT ( 'NONE',  ( -5.405949406250003975, -9.363379034771801557, -39.53125000204838102 ) ) ;
#24198 = CARTESIAN_POINT ( 'NONE',  ( -4.999999999999996447, 8.660254037844387298, -163.5000000000000000 ) ) ;
#24199 = DIRECTION ( 'NONE',  ( -0.000000000000000000, -0.000000000000000000, 1.000000000000000000 ) ) ;
#24200 = CARTESIAN_POINT ( 'NONE',  ( -9.999999999999998224, 1.224646799147353059E-15, -28.62500000409676204 ) ) ;
#24201 = ADVANCED_FACE ( 'NONE', ( #469 ), #13584, .T. ) ;
#24202 = CARTESIAN_POINT ( 'NONE',  ( -10.81189881249999729, 1.324075727343319199E-15, -135.7812500020483810 ) ) ;
#24203 = CARTESIAN_POINT ( 'NONE',  ( 7.232763097364098392, 7.658562690767763748, -5.257032284683799044E-15 ) ) ;
#24204 = AXIS2_PLACEMENT_3D ( 'NONE', #23227, #32731, #16294 ) ;
#24205 = DIRECTION ( 'NONE',  ( -0.000000000000000000, -0.000000000000000000, 1.000000000000000000 ) ) ;
#24206 = EDGE_LOOP ( 'NONE', ( #17960, #98, #20782, #11175 ) ) ;
#24208 = EDGE_LOOP ( 'NONE', ( #3649, #22755, #39099, #10059 ) ) ;
#24207 = EDGE_LOOP ( 'NONE', ( #17726, #32689, #5292, #5354 ) ) ;
#24209 = PLANE ( 'NONE',  #27991 ) ;
#24210 = CARTESIAN_POINT ( 'NONE',  ( 9.999999999999998224, 0.000000000000000000, -146.3750000040967905 ) ) ;
#24211 = CARTESIAN_POINT ( 'NONE',  ( 10.81189881249999907, 6.242252689847868297, -169.2187500020483810 ) ) ;
#24212 = CARTESIAN_POINT ( 'NONE',  ( -5.405949406249996869, 9.363379034771805109, -12.84375000204834905 ) ) ;
#24213 = CARTESIAN_POINT ( 'NONE',  ( 0.000000000000000000, 0.000000000000000000, -200.0000000000000000 ) ) ;
#24214 = CARTESIAN_POINT ( 'NONE',  ( 7.644554776091147741E-16, 12.48450537969573659, -147.9687500020484094 ) ) ;
#24215 = CARTESIAN_POINT ( 'NONE',  ( 10.81189881249999729, 0.000000000000000000, -139.3437500020484094 ) ) ;
#24216 = CARTESIAN_POINT ( 'NONE',  ( 5.405949406249999534, 9.363379034771803333, -104.7812500020483810 ) ) ;
#24217 = CARTESIAN_POINT ( 'NONE',  ( 10.81189881249999551, -6.242252689847874514, -121.4687500020484094 ) ) ;
#24218 = CARTESIAN_POINT ( 'NONE',  ( 5.000000000000000000, 8.660254037844385522, -198.6250000040967905 ) ) ;
#24219 = CARTESIAN_POINT ( 'NONE',  ( 10.81189881249999551, -6.242252689847874514, -123.1562500020483952 ) ) ;
#24220 = CARTESIAN_POINT ( 'NONE',  ( 5.405949406249992428, -9.363379034771808662, -12.09375000204834727 ) ) ;
#24221 = CARTESIAN_POINT ( 'NONE',  ( 5.405949406249992428, -9.363379034771808662, -130.5937500020483810 ) ) ;
#24222 = AXIS2_PLACEMENT_3D ( 'NONE', #25358, #1413, #8317 ) ;
#24223 = CARTESIAN_POINT ( 'NONE',  ( 5.405949406249999534, 9.363379034771803333, -199.2812500020484094 ) ) ;
#24224 = CARTESIAN_POINT ( 'NONE',  ( 10.00000000000000000, 5.773502691896255534, -159.3750000000000000 ) ) ;
#24225 = CARTESIAN_POINT ( 'NONE',  ( 9.999999999999996447, -5.773502691896262640, -17.12499999999997158 ) ) ;
#24226 = CC_DESIGN_APPROVAL ( #7210, ( #28392 ) ) ;
#24227 = CARTESIAN_POINT ( 'NONE',  ( 5.405949406249999534, 9.363379034771803333, -79.09375000204838102 ) ) ;
#24228 = CARTESIAN_POINT ( 'NONE',  ( 10.81189881249999907, 6.242252689847868297, -67.21875000204838102 ) ) ;
#24229 = PLANE ( 'NONE',  #25009 ) ;
#24230 = CARTESIAN_POINT ( 'NONE',  ( 7.644554776091147741E-16, 12.48450537969573659, -35.65625000204835260 ) ) ;
#24231 = CARTESIAN_POINT ( 'NONE',  ( 5.405949406249999534, 9.363379034771803333, -46.09375000204838102 ) ) ;
#24232 = CARTESIAN_POINT ( 'NONE',  ( -9.999999999999227285, -5.773502691896698735, -111.0000000040967620 ) ) ;
#24233 = CARTESIAN_POINT ( 'NONE',  ( -10.81189881249999729, 1.324075727343319199E-15, -150.5937500020483810 ) ) ;
#24234 = CARTESIAN_POINT ( 'NONE',  ( -9.999999999999998224, 1.224646799147353059E-15, -122.7500000000000000 ) ) ;
#24235 = CARTESIAN_POINT ( 'NONE',  ( -5.405949406250003975, -9.363379034771801557, -134.0312500020484094 ) ) ;
#24236 = DIRECTION ( 'NONE',  ( -0.000000000000000000, -0.000000000000000000, 1.000000000000000000 ) ) ;
#24237 = CARTESIAN_POINT ( 'NONE',  ( 9.999999999999996447, -5.773502691896262640, -84.62499999999998579 ) ) ;
#24238 = CARTESIAN_POINT ( 'NONE',  ( 10.81189881249999729, 6.242252689847867408, -14.90625000204837036 ) ) ;
#24239 = ORIENTED_EDGE ( 'NONE', *, *, #35719, .F. ) ;
#24240 = CARTESIAN_POINT ( 'NONE',  ( -5.405949406250003975, -9.363379034771801557, -105.5312500020483810 ) ) ;
#24241 = CARTESIAN_POINT ( 'NONE',  ( -9.999999999999998224, 5.773502691896259087, -126.2500000040967763 ) ) ;
#24242 = CARTESIAN_POINT ( 'NONE',  ( -9.999999999998969713, -5.773502691896847949, -57.00000000409674783 ) ) ;
#24243 = AXIS2_PLACEMENT_3D ( 'NONE', #37359, #7369, #34134 ) ;
#24244 = CARTESIAN_POINT ( 'NONE',  ( -4.999999999999996447, 8.660254037844387298, -36.37500000409676915 ) ) ;
#24245 = DIRECTION ( 'NONE',  ( -0.000000000000000000, -0.000000000000000000, 1.000000000000000000 ) ) ;
#24246 = CARTESIAN_POINT ( 'NONE',  ( 10.81189881249999907, 6.242252689847868297, -40.40625000204836681 ) ) ;
#24247 = EDGE_CURVE ( 'NONE', #3072, #9067, #24274, .T. ) ;
#24248 = CARTESIAN_POINT ( 'NONE',  ( 9.999999999999998224, 1.224646799147353059E-15, -99.99999999999998579 ) ) ;
#24249 = CARTESIAN_POINT ( 'NONE',  ( -10.81189881249999729, 6.242252689847871849, -152.4062500020483810 ) ) ;
#24250 = CARTESIAN_POINT ( 'NONE',  ( -10.81189881249999729, 1.324075727343319199E-15, -131.0937500020483810 ) ) ;
#24251 = CARTESIAN_POINT ( 'NONE',  ( 7.070501591499376803E-16, 11.54700538379251284, -144.1250000000000000 ) ) ;
#24252 = ORIENTED_EDGE ( 'NONE', *, *, #31320, .F. ) ;
#24253 = CARTESIAN_POINT ( 'NONE',  ( -4.999999999999996447, 8.660254037844387298, -22.49999999999996447 ) ) ;
#24254 = ORIENTED_EDGE ( 'NONE', *, *, #29121, .T. ) ;
#24255 = AXIS2_PLACEMENT_3D ( 'NONE', #7114, #30432, #6898 ) ;
#24256 = CC_DESIGN_APPROVAL ( #23837, ( #138 ) ) ;
#24257 = ORIENTED_EDGE ( 'NONE', *, *, #3826, .T. ) ;
#24259 = EDGE_LOOP ( 'NONE', ( #13290, #36606, #32310, #27691 ) ) ;
#24258 = CARTESIAN_POINT ( 'NONE',  ( -5.405949406250003975, -9.363379034771801557, -112.8437500020483810 ) ) ;
#24260 = EDGE_CURVE ( 'NONE', #37116, #30868, #5766, .T. ) ;
#24261 =( BOUNDED_CURVE ( )  B_SPLINE_CURVE ( 2, ( #37503, #5135, #11804, #24146, #7946, #21096, #31265 ),
 .UNSPECIFIED., .F., .F. ) 
 B_SPLINE_CURVE_WITH_KNOTS ( ( 3, 2, 2, 3 ),
 ( 0.5186567164179105571, 0.5199004975124379424, 0.5211442786069653277, 0.5223880597014926019 ),
 .UNSPECIFIED. ) 
 CURVE ( )  GEOMETRIC_REPRESENTATION_ITEM ( )  RATIONAL_B_SPLINE_CURVE ( ( 0.9999999999999880096, 0.8660254037844506980, 1.000000000000000000, 0.8660254037844387076, 1.000000000000000000, 0.8660254037844267172, 1.000000000000011990 ) ) 
 REPRESENTATION_ITEM ( '' )  );
#24262 = CARTESIAN_POINT ( 'NONE',  ( -2.121150477449813534E-15, -11.54700538379251284, -41.75000000409674783 ) ) ;
#24263 = CARTESIAN_POINT ( 'NONE',  ( -2.293366432827344421E-15, -12.48450537969573659, -186.2187500020484094 ) ) ;
#24264 = AXIS2_PLACEMENT_3D ( 'NONE', #28603, #8531, #31633 ) ;
#24265 = CARTESIAN_POINT ( 'NONE',  ( -10.81189881249999729, 6.242252689847871849, -41.21875000204834549 ) ) ;
#24266 = CYLINDRICAL_SURFACE ( 'NONE', #10885, 9.999999999999998224 ) ;
#24267 = CARTESIAN_POINT ( 'NONE',  ( 9.999999999999998224, 0.000000000000000000, -195.8750000040967905 ) ) ;
#24268 = CARTESIAN_POINT ( 'NONE',  ( -10.81189881249999729, 1.324075727343319199E-15, -171.5937500020484094 ) ) ;
#24269 = CARTESIAN_POINT ( 'NONE',  ( 10.81189881249999551, -6.242252689847874514, -161.9687500020484094 ) ) ;
#24270 = CARTESIAN_POINT ( 'NONE',  ( 10.00000000000051159, -5.773502691895965988, -122.5000000040967763 ) ) ;
#24271 = CARTESIAN_POINT ( 'NONE',  ( 5.405949406249992428, -9.363379034771808662, -141.0937500020483810 ) ) ;
#24272 = CARTESIAN_POINT ( 'NONE',  ( -10.81189881249999729, 6.242252689847871849, -153.7187500020483810 ) ) ;
#24273 = CARTESIAN_POINT ( 'NONE',  ( 9.999999999999998224, 0.000000000000000000, -87.49999999999998579 ) ) ;
#24274 =( BOUNDED_CURVE ( )  B_SPLINE_CURVE ( 2, ( #33687, #4113, #41783, #5549, #28652, #12009, #18701 ),
 .UNSPECIFIED., .F., .F. ) 
 B_SPLINE_CURVE_WITH_KNOTS ( ( 3, 2, 2, 3 ),
 ( 0.9291044776119405935, 0.9303482587064679787, 0.9315920398009952530, 0.9328358208955226383 ),
 .UNSPECIFIED. ) 
 CURVE ( )  GEOMETRIC_REPRESENTATION_ITEM ( )  RATIONAL_B_SPLINE_CURVE ( ( 0.9999999999999641398, 0.8660254037844745678, 1.000000000000000000, 0.8660254037844387076, 1.000000000000000000, 0.8660254037844148378, 1.000000000000023981 ) ) 
 REPRESENTATION_ITEM ( '' )  );
#24275 = CARTESIAN_POINT ( 'NONE',  ( -9.999999999999998224, 1.224646799147353059E-15, -121.2500000000000000 ) ) ;
#24276 = CARTESIAN_POINT ( 'NONE',  ( 10.00000000000000000, 5.773502691896255534, -181.8750000000000000 ) ) ;
#24277 = CARTESIAN_POINT ( 'NONE',  ( 5.405949406249992428, -9.363379034771808662, -88.59375000204838102 ) ) ;
#24278 = CARTESIAN_POINT ( 'NONE',  ( -5.000000000000003553, -8.660254037844383745, -82.37500000409676204 ) ) ;
#24279 = CARTESIAN_POINT ( 'NONE',  ( -5.405949406250003975, -9.363379034771801557, -57.53125000204836681 ) ) ;
#24280 = CYLINDRICAL_SURFACE ( 'NONE', #33003, 9.999999999999998224 ) ;
#24281 = CARTESIAN_POINT ( 'NONE',  ( -5.405949406250003975, -9.363379034771801557, -174.3437500020484094 ) ) ;
#24282 = CARTESIAN_POINT ( 'NONE',  ( 5.405949406249999534, 9.363379034771803333, -110.7812500020483810 ) ) ;
#24283 = CARTESIAN_POINT ( 'NONE',  ( -10.81189881249999729, 6.242252689847871849, -153.9062500020483810 ) ) ;
#24284 = FACE_OUTER_BOUND ( 'NONE', #16886, .T. ) ;
#24285 = CARTESIAN_POINT ( 'NONE',  ( 10.81189881249999729, 0.000000000000000000, -45.03125000204838102 ) ) ;
#24286 = CARTESIAN_POINT ( 'NONE',  ( 5.000000000000000000, 8.660254037844385522, -132.6250000040967620 ) ) ;
#24287 = CARTESIAN_POINT ( 'NONE',  ( -4.999999999999996447, 8.660254037844387298, -110.9999999999999858 ) ) ;
#24288 = VECTOR ( 'NONE', #7389, 1000.000000000000000 ) ;
#24289 = VERTEX_POINT ( 'NONE', #24996 ) ;
#24290 =( BOUNDED_CURVE ( )  B_SPLINE_CURVE ( 2, ( #33739, #17091, #23806, #20550, #7613, #20338, #3525 ),
 .UNSPECIFIED., .F., .F. ) 
 B_SPLINE_CURVE_WITH_KNOTS ( ( 3, 2, 2, 3 ),
 ( 0.07089552238805976736, 0.07213930348258713876, 0.07338308457711449628, 0.07462686567164185381 ),
 .UNSPECIFIED. ) 
 CURVE ( )  GEOMETRIC_REPRESENTATION_ITEM ( )  RATIONAL_B_SPLINE_CURVE ( ( 0.9999999999999925615, 0.8660254037844461461, 1.000000000000000000, 0.8660254037844387076, 1.000000000000000000, 0.8660254037844312691, 1.000000000000007550 ) ) 
 REPRESENTATION_ITEM ( '' )  );
#24291 = CARTESIAN_POINT ( 'NONE',  ( -5.405949406249996869, 9.363379034771805109, -122.5312500020483952 ) ) ;
#24292 = CARTESIAN_POINT ( 'NONE',  ( 4.999999999999992006, -8.660254037844389075, -151.1250000040967905 ) ) ;
#24293 = CARTESIAN_POINT ( 'NONE',  ( -5.405949406249996869, 9.363379034771805109, -188.5312500020484094 ) ) ;
#24294 = ORIENTED_EDGE ( 'NONE', *, *, #40189, .F. ) ;
#24295 = CARTESIAN_POINT ( 'NONE',  ( -10.00000000000000000, -5.773502691896251982, -50.62499999999997868 ) ) ;
#24296 = CARTESIAN_POINT ( 'NONE',  ( -10.81189881249999907, -6.242252689847864744, -177.4687500020484094 ) ) ;
#24297 = CARTESIAN_POINT ( 'NONE',  ( -5.000000000000003553, -8.660254037844383745, -58.37500000409676204 ) ) ;
#24298 = LINE ( 'NONE', #5072, #42365 ) ;
#24299 = FACE_OUTER_BOUND ( 'NONE', #36502, .T. ) ;
#24300 = CARTESIAN_POINT ( 'NONE',  ( -5.405949406250003975, -9.363379034771801557, -72.53125000204838102 ) ) ;
#24301 = CARTESIAN_POINT ( 'NONE',  ( 10.81189881249999729, 0.000000000000000000, -48.03125000204838813 ) ) ;
#24302 = CARTESIAN_POINT ( 'NONE',  ( -4.999999999999996447, 8.660254037844387298, -48.37500000409677625 ) ) ;
#24303 = CARTESIAN_POINT ( 'NONE',  ( 10.81189881249999729, 0.000000000000000000, -8.843750002048345493 ) ) ;
#24304 = CARTESIAN_POINT ( 'NONE',  ( -9.999999999999227285, -5.773502691896698735, -135.0000000040967620 ) ) ;
#24305 = CARTESIAN_POINT ( 'NONE',  ( 10.81189881249999729, 0.000000000000000000, -180.0312500020483810 ) ) ;
#24306 = AXIS2_PLACEMENT_3D ( 'NONE', #22220, #31950, #18549 ) ;
#24307 = CARTESIAN_POINT ( 'NONE',  ( -10.81189881249999729, 1.324075727343319199E-15, -2.281250002048373915 ) ) ;
#24308 = CYLINDRICAL_SURFACE ( 'NONE', #23584, 9.999999999999998224 ) ;
#24309 = CARTESIAN_POINT ( 'NONE',  ( -1.040834085586084257E-14, -145.0000000000000000, 22.49999999999999289 ) ) ;
#24310 = FACE_OUTER_BOUND ( 'NONE', #41095, .T. ) ;
#24311 = LINE ( 'NONE', #1639, #19683 ) ;
#24312 = CARTESIAN_POINT ( 'NONE',  ( -99.99999999999994316, -20.00000000000000355, -170.0000000000000000 ) ) ;
#24314 = ORIENTED_EDGE ( 'NONE', *, *, #1014, .F. ) ;
#24313 = CARTESIAN_POINT ( 'NONE',  ( 10.81189881249999551, -6.242252689847874514, -82.65625000204836681 ) ) ;
#24316 = ORIENTED_EDGE ( 'NONE', *, *, #38837, .T. ) ;
#24315 = CYLINDRICAL_SURFACE ( 'NONE', #10312, 9.999999999999998224 ) ;
#24317 = VERTEX_POINT ( 'NONE', #18490 ) ;
#24318 = CARTESIAN_POINT ( 'NONE',  ( -10.81189881249999729, 1.324075727343319199E-15, -39.59375000204837391 ) ) ;
#24319 = CARTESIAN_POINT ( 'NONE',  ( 7.644554776091147741E-16, 12.48450537969573659, -27.96875000204838457 ) ) ;
#24320 = CARTESIAN_POINT ( 'NONE',  ( -2.293366432827344421E-15, -12.48450537969573659, -12.40625000204835970 ) ) ;
#24321 = CARTESIAN_POINT ( 'NONE',  ( 5.405949406249992428, -9.363379034771808662, -61.59375000204836681 ) ) ;
#24322 = DIRECTION ( 'NONE',  ( 1.000000000000000000, 0.000000000000000000, 0.000000000000000000 ) ) ;
#24323 = EDGE_CURVE ( 'NONE', #36923, #18938, #18195, .T. ) ;
#24324 = CARTESIAN_POINT ( 'NONE',  ( 10.00000000000000000, 5.773502691896255534, -40.87499999999997158 ) ) ;
#24325 = CARTESIAN_POINT ( 'NONE',  ( -5.405949406249996869, 9.363379034771805109, -186.8437500020483810 ) ) ;
#24326 = PERSON ( 'NAUO-PER3', 'UNSPECIFIED', 'UNSPECIFIED', ('UNSPECIFIED'), ('UNSPECIFIED'), ('UNSPECIFIED') ) ;
#24327 = EDGE_CURVE ( 'NONE', #34592, #9953, #38347, .T. ) ;
#24328 = CARTESIAN_POINT ( 'NONE',  ( 5.405949406249992428, -9.363379034771808662, -165.0937500020484094 ) ) ;
#24329 = CARTESIAN_POINT ( 'NONE',  ( -5.405949406249996869, 9.363379034771805109, -176.3437500020483810 ) ) ;
#24330 = DIRECTION ( 'NONE',  ( -0.000000000000000000, -0.000000000000000000, -1.000000000000000000 ) ) ;
#24331 = CARTESIAN_POINT ( 'NONE',  ( -9.999999999999998224, 0.000000000000000000, -99.99999999999998579 ) ) ;
#24332 = AXIS2_PLACEMENT_3D ( 'NONE', #9000, #8791, #5553 ) ;
#24333 = DIRECTION ( 'NONE',  ( -0.000000000000000000, -0.000000000000000000, 1.000000000000000000 ) ) ;
#24334 = CARTESIAN_POINT ( 'NONE',  ( -5.405949406250003975, -9.363379034771801557, -112.8437500020483810 ) ) ;
#24335 = DIRECTION ( 'NONE',  ( -0.000000000000000000, 1.000000000000000000, -0.000000000000000000 ) ) ;
#24336 = CARTESIAN_POINT ( 'NONE',  ( 7.644554776091147741E-16, 12.48450537969573659, -83.65625000204838102 ) ) ;
#24337 = CARTESIAN_POINT ( 'NONE',  ( 10.81189881249999551, -6.242252689847874514, -97.46875000204838102 ) ) ;
#24338 = CARTESIAN_POINT ( 'NONE',  ( 10.81189881249999729, 0.000000000000000000, -61.34375000204836681 ) ) ;
#24339 = CARTESIAN_POINT ( 'NONE',  ( 10.81189881249999551, -6.242252689847874514, -66.15625000204839523 ) ) ;
#24340 = CARTESIAN_POINT ( 'NONE',  ( 10.00000000000000000, 5.773502691896255534, -150.7500000040967905 ) ) ;
#24341 = CARTESIAN_POINT ( 'NONE',  ( 9.999999999999998224, 0.000000000000000000, -132.5000000000000000 ) ) ;
#24342 = CARTESIAN_POINT ( 'NONE',  ( 10.81189881249999729, 0.000000000000000000, -154.5312500020484094 ) ) ;
#24343 = CARTESIAN_POINT ( 'NONE',  ( 5.405949406249999534, 9.363379034771803333, -169.2812500020484094 ) ) ;
#24344 = CYLINDRICAL_SURFACE ( 'NONE', #4770, 9.999999999999998224 ) ;
#24345 = CARTESIAN_POINT ( 'NONE',  ( 0.000000000000000000, 0.000000000000000000, -200.0000000000000000 ) ) ;
#24346 = CARTESIAN_POINT ( 'NONE',  ( -5.405949406250003975, -9.363379034771801557, -103.8437500020483810 ) ) ;
#24347 = FACE_OUTER_BOUND ( 'NONE', #12808, .T. ) ;
#24348 = CARTESIAN_POINT ( 'NONE',  ( 7.070501591499377789E-16, 11.54700538379251284, -70.62499999999998579 ) ) ;
#24349 = CARTESIAN_POINT ( 'NONE',  ( -10.81189881249999729, 6.242252689847871849, -8.406250002048365033 ) ) ;
#24350 = CARTESIAN_POINT ( 'NONE',  ( 5.000000000000000000, 8.660254037844385522, -83.12500000409676204 ) ) ;
#24351 = FACE_OUTER_BOUND ( 'NONE', #21951, .T. ) ;
#24352 = CARTESIAN_POINT ( 'NONE',  ( 5.405949406249992428, -9.363379034771808662, -99.28125000204839523 ) ) ;
#24353 = CARTESIAN_POINT ( 'NONE',  ( 10.81189881249999551, -6.242252689847874514, -75.15625000204838102 ) ) ;
#24354 = CARTESIAN_POINT ( 'NONE',  ( 10.00000000000000000, 5.773502691896255534, -75.75000000409679046 ) ) ;
#24355 = CARTESIAN_POINT ( 'NONE',  ( 9.999999999999998224, 0.000000000000000000, -135.5000000000000000 ) ) ;
#24356 = CARTESIAN_POINT ( 'NONE',  ( -10.81189881249999907, -6.242252689847864744, -36.46875000204835260 ) ) ;
#24357 = ORIENTED_EDGE ( 'NONE', *, *, #7506, .F. ) ;
#24358 = CARTESIAN_POINT ( 'NONE',  ( 10.81189881249999551, -6.242252689847874514, -198.1562500020484379 ) ) ;
#24359 = CARTESIAN_POINT ( 'NONE',  ( 10.81189881249999729, 0.000000000000000000, -30.03125000204837036 ) ) ;
#24360 = CARTESIAN_POINT ( 'NONE',  ( -10.81189881249999729, -6.242252689847864744, -15.46875000204835793 ) ) ;
#24361 = CARTESIAN_POINT ( 'NONE',  ( 9.999999999999998224, 0.000000000000000000, -117.8750000040967905 ) ) ;
#24362 =( BOUNDED_CURVE ( )  B_SPLINE_CURVE ( 2, ( #12196, #24975, #34892, #41336, #41762, #5958, #5316 ),
 .UNSPECIFIED., .F., .F. ) 
 B_SPLINE_CURVE_WITH_KNOTS ( ( 3, 2, 2, 3 ),
 ( 0.4813432835820896649, 0.4825870646766170502, 0.4838308457711443800, 0.4850746268656717652 ),
 .UNSPECIFIED. ) 
 CURVE ( )  GEOMETRIC_REPRESENTATION_ITEM ( )  RATIONAL_B_SPLINE_CURVE ( ( 0.9999999999999880096, 0.8660254037844506980, 1.000000000000000000, 0.8660254037844387076, 1.000000000000000000, 0.8660254037844267172, 1.000000000000011990 ) ) 
 REPRESENTATION_ITEM ( '' )  );
#24363 = CARTESIAN_POINT ( 'NONE',  ( -2.121150477449813534E-15, -11.54700538379251284, -4.250000004096754047 ) ) ;
#24364 = CARTESIAN_POINT ( 'NONE',  ( 5.405949406249999534, 9.363379034771803333, -127.2812500020483810 ) ) ;
#24365 = CARTESIAN_POINT ( 'NONE',  ( -9.999999999999998224, 5.773502691896259087, -179.8750000000000000 ) ) ;
#24366 = DIRECTION ( 'NONE',  ( 1.000000000000000000, 0.000000000000000000, 0.000000000000000000 ) ) ;
#24368 = ORIENTED_EDGE ( 'NONE', *, *, #3752, .F. ) ;
#24367 = CARTESIAN_POINT ( 'NONE',  ( -5.405949406250003975, -9.363379034771801557, -110.0312500020483810 ) ) ;
#24369 = DIRECTION ( 'NONE',  ( -0.000000000000000000, -0.000000000000000000, -1.000000000000000000 ) ) ;
#24370 = ORIENTED_EDGE ( 'NONE', *, *, #19569, .F. ) ;
#24371 = ORIENTED_EDGE ( 'NONE', *, *, #480, .T. ) ;
#24372 = CARTESIAN_POINT ( 'NONE',  ( -5.405949406249996869, 9.363379034771805109, -38.53125000204838102 ) ) ;
#24373 = CALENDAR_DATE ( 2026, 28, 9 ) ;
#24374 = CARTESIAN_POINT ( 'NONE',  ( -10.81189881249999907, -6.242252689847864744, -85.96875000204836681 ) ) ;
#24375 = CARTESIAN_POINT ( 'NONE',  ( 9.999999999999994671, -5.773502691896262640, -167.1250000000000000 ) ) ;
#24376 = EDGE_CURVE ( 'NONE', #20021, #34021, #2112, .T. ) ;
#24377 = EDGE_CURVE ( 'NONE', #28346, #7904, #3601, .T. ) ;
#24378 = CARTESIAN_POINT ( 'NONE',  ( 5.344739998537471948, 9.251476015204525893, -99.99999999999995737 ) ) ;
#24379 = ADVANCED_FACE ( 'NONE', ( #17674 ), #38555, .T. ) ;
#24380 = LINE ( 'NONE', #15052, #21900 ) ;
#24381 = CARTESIAN_POINT ( 'NONE',  ( -5.405949406250003975, -9.363379034771801557, -161.0312500020484094 ) ) ;
#24382 = LINE ( 'NONE', #1064, #5943 ) ;
#24383 = CARTESIAN_POINT ( 'NONE',  ( 10.81189881249999729, 0.000000000000000000, -125.8437500020483952 ) ) ;
#24384 = PRODUCT_DEFINITION ( 'UNKNOWN', '', #28392, #39072 ) ;
#24385 = CARTESIAN_POINT ( 'NONE',  ( -5.405949406250003975, -9.363379034771801557, -91.84375000204838102 ) ) ;
#24386 = CARTESIAN_POINT ( 'NONE',  ( -10.81189881249999729, 6.242252689847871849, -3.906250002048350822 ) ) ;
#24387 = CARTESIAN_POINT ( 'NONE',  ( 5.405949406249999534, 9.363379034771803333, -193.0937500020484094 ) ) ;
#24388 = CARTESIAN_POINT ( 'NONE',  ( -10.81189881249999729, 1.324075727343319199E-15, -96.78125000204839523 ) ) ;
#24389 = CARTESIAN_POINT ( 'NONE',  ( 7.070501591499377789E-16, 11.54700538379251284, -176.0000000040968189 ) ) ;
#24390 = CARTESIAN_POINT ( 'NONE',  ( 5.405949406249992428, -9.363379034771808662, -109.5937500020483810 ) ) ;
#24391 = CARTESIAN_POINT ( 'NONE',  ( 7.644554776091147741E-16, 12.48450537969573659, -175.1562500020484094 ) ) ;
#24392 = CARTESIAN_POINT ( 'NONE',  ( 5.000000000000000000, 8.660254037844385522, -108.2499999999999858 ) ) ;
#24393 = CARTESIAN_POINT ( 'NONE',  ( 7.644554776091147741E-16, 12.48450537969573659, -179.6562500020484094 ) ) ;
#24394 = CARTESIAN_POINT ( 'NONE',  ( -10.81189881249999907, -6.242252689847864744, -194.1562500020484094 ) ) ;
#24395 = CARTESIAN_POINT ( 'NONE',  ( 10.81189881249999729, 0.000000000000000000, -49.34375000204838102 ) ) ;
#24396 = CARTESIAN_POINT ( 'NONE',  ( 10.00000000000000000, 5.773502691896255534, -173.2500000040967905 ) ) ;
#24397 = CARTESIAN_POINT ( 'NONE',  ( 10.81189881249999907, 6.242252689847868297, -13.40625000204836326 ) ) ;
#24398 = CARTESIAN_POINT ( 'NONE',  ( 5.405949406249999534, 9.363379034771803333, -20.59375000204835615 ) ) ;
#24399 = CARTESIAN_POINT ( 'NONE',  ( -2.121150477449813534E-15, -11.54700538379251284, -158.7500000040968189 ) ) ;
#24400 = CARTESIAN_POINT ( 'NONE',  ( -2.293366432827344421E-15, -12.48450537969573659, -133.7187500020483810 ) ) ;
#24401 = CARTESIAN_POINT ( 'NONE',  ( 10.00000000000000000, 5.773502691896255534, -100.8750000000000000 ) ) ;
#24402 = CARTESIAN_POINT ( 'NONE',  ( -10.81189881249999907, -6.242252689847864744, -27.65625000204838457 ) ) ;
#24403 = CARTESIAN_POINT ( 'NONE',  ( -9.999999999999998224, 1.224646799147353059E-15, -108.1250000040967763 ) ) ;
#24404 = CARTESIAN_POINT ( 'NONE',  ( -9.999999999998456346, -5.773502691897145489, -49.50000000409673362 ) ) ;
#24405 = CARTESIAN_POINT ( 'NONE',  ( -10.00000000000000000, -5.773502691896251982, -52.12499999999997158 ) ) ;
#24406 = CARTESIAN_POINT ( 'NONE',  ( 10.81189881249999907, 6.242252689847868297, -125.9062500020483810 ) ) ;
#24407 = CARTESIAN_POINT ( 'NONE',  ( 10.81189881249999729, 0.000000000000000000, -99.03125000204839523 ) ) ;
#24408 = ORIENTED_EDGE ( 'NONE', *, *, #14304, .F. ) ;
#24409 =( BOUNDED_CURVE ( )  B_SPLINE_CURVE ( 2, ( #19682, #22943, #39538, #35891, #19473, #32658, #19261 ),
 .UNSPECIFIED., .F., .F. ) 
 B_SPLINE_CURVE_WITH_KNOTS ( ( 3, 2, 2, 3 ),
 ( 0.3619402985074628432, 0.3631840796019901729, 0.3644278606965175027, 0.3656716417910448325 ),
 .UNSPECIFIED. ) 
 CURVE ( )  GEOMETRIC_REPRESENTATION_ITEM ( )  RATIONAL_B_SPLINE_CURVE ( ( 0.9999999999999820144, 0.8660254037844566932, 1.000000000000000000, 0.8660254037844387076, 1.000000000000000000, 0.8660254037844327124, 1.000000000000005995 ) ) 
 REPRESENTATION_ITEM ( '' )  );
#24410 = CARTESIAN_POINT ( 'NONE',  ( -5.000000000000003553, -8.660254037844383745, -98.87500000409677625 ) ) ;
#24411 = CARTESIAN_POINT ( 'NONE',  ( 9.999999999999998224, 0.000000000000000000, -141.8750000040967905 ) ) ;
#24412 = CARTESIAN_POINT ( 'NONE',  ( 10.81189881249999907, 6.242252689847868297, -161.9062500020484094 ) ) ;
#24413 = CARTESIAN_POINT ( 'NONE',  ( -10.81189881249999729, 1.324075727343319199E-15, -60.59375000204836681 ) ) ;
#24415 = EDGE_CURVE ( 'NONE', #13534, #20251, #30662, .T. ) ;
#24414 = ORIENTED_EDGE ( 'NONE', *, *, #37545, .T. ) ;
#24416 = CARTESIAN_POINT ( 'NONE',  ( -2.121150477449813534E-15, -11.54700538379251284, -27.87499999999999289 ) ) ;
#24417 = CARTESIAN_POINT ( 'NONE',  ( -10.81189881249999729, 1.324075727343319199E-15, -33.78125000204837391 ) ) ;
#24418 = CARTESIAN_POINT ( 'NONE',  ( -2.121150477449813534E-15, -11.54700538379251284, -158.3750000000000000 ) ) ;
#24419 = DIRECTION ( 'NONE',  ( -1.000000000000000000, 0.000000000000000000, 0.000000000000000000 ) ) ;
#24420 = CARTESIAN_POINT ( 'NONE',  ( 7.070501591499377789E-16, 11.54700538379251284, -24.50000000409676915 ) ) ;
#24421 = CARTESIAN_POINT ( 'NONE',  ( 0.000000000000000000, 0.000000000000000000, -240.0000000000000000 ) ) ;
#24422 = CARTESIAN_POINT ( 'NONE',  ( 10.81189881249999907, 6.242252689847868297, -130.4062500020483810 ) ) ;
#24423 = DIRECTION ( 'NONE',  ( 1.000000000000000000, 0.000000000000000000, 0.000000000000000000 ) ) ;
#24424 = CARTESIAN_POINT ( 'NONE',  ( 10.00000000000000000, 5.773502691896255534, -167.2500000040967905 ) ) ;
#24425 = ORIENTED_EDGE ( 'NONE', *, *, #10185, .T. ) ;
#24427 = ORIENTED_EDGE ( 'NONE', *, *, #486, .T. ) ;
#24426 = ORIENTED_EDGE ( 'NONE', *, *, #9308, .T. ) ;
#24428 = CARTESIAN_POINT ( 'NONE',  ( 4.999999999999992006, -8.660254037844389075, -120.7500000000000000 ) ) ;
#24429 = CARTESIAN_POINT ( 'NONE',  ( 4.999999999999992006, -8.660254037844389075, -146.6250000040967905 ) ) ;
#24430 = CARTESIAN_POINT ( 'NONE',  ( -10.81189881249999729, 6.242252689847871849, -165.7187500020483810 ) ) ;
#24431 = CARTESIAN_POINT ( 'NONE',  ( -2.293366432827344421E-15, -12.48450537969573659, -198.4062500020484094 ) ) ;
#24432 = CARTESIAN_POINT ( 'NONE',  ( -5.405949406250003975, -9.363379034771801557, -18.34375000204835260 ) ) ;
#24433 = CARTESIAN_POINT ( 'NONE',  ( 0.000000000000000000, 0.000000000000000000, -200.0000000000000000 ) ) ;
#24434 = CARTESIAN_POINT ( 'NONE',  ( 10.81189881249999729, 6.242252689847867408, -145.2187500020484094 ) ) ;
#24435 = CARTESIAN_POINT ( 'NONE',  ( -10.81189881249999907, -6.242252689847864744, -138.4687500020484094 ) ) ;
#24436 = CARTESIAN_POINT ( 'NONE',  ( 5.405949406249992428, -9.363379034771808662, -109.7812500020483810 ) ) ;
#24437 = CARTESIAN_POINT ( 'NONE',  ( -10.81189881249999729, 1.324075727343319199E-15, -117.5937500020483810 ) ) ;
#24438 = CARTESIAN_POINT ( 'NONE',  ( 4.999999999999992006, -8.660254037844389075, -196.1250000040967905 ) ) ;
#24439 = CARTESIAN_POINT ( 'NONE',  ( -5.405949406249996869, 9.363379034771805109, -121.0312500020483952 ) ) ;
#24440 = CARTESIAN_POINT ( 'NONE',  ( -10.81189881249999907, -6.242252689847864744, -1.968750002048357262 ) ) ;
#24441 = CARTESIAN_POINT ( 'NONE',  ( 10.81189881249999551, -6.242252689847874514, -128.9687500020483810 ) ) ;
#24442 = CARTESIAN_POINT ( 'NONE',  ( 10.00000000000000000, 5.773502691896255534, -150.3750000000000000 ) ) ;
#24443 = CARTESIAN_POINT ( 'NONE',  ( 9.999999999999998224, 0.000000000000000000, -21.49999999999996447 ) ) ;
#24444 = EDGE_CURVE ( 'NONE', #31913, #29936, #1305, .T. ) ;
#24445 = CARTESIAN_POINT ( 'NONE',  ( 5.405949406249992428, -9.363379034771808662, -73.59375000204838102 ) ) ;
#24446 = CARTESIAN_POINT ( 'NONE',  ( 10.81189881249999551, -6.242252689847874514, -65.96875000204836681 ) ) ;
#24447 = CARTESIAN_POINT ( 'NONE',  ( -9.999999999999998224, 1.224646799147353059E-15, -116.7499999999999858 ) ) ;
#24448 = CARTESIAN_POINT ( 'NONE',  ( -10.81189881249999907, -6.242252689847864744, -36.65625000204835970 ) ) ;
#24449 = CARTESIAN_POINT ( 'NONE',  ( -10.81189881249999729, 6.242252689847871849, -47.21875000204836681 ) ) ;
#24450 = CARTESIAN_POINT ( 'NONE',  ( -10.81189881249999729, 6.242252689847871849, -152.2187500020483526 ) ) ;
#24451 = CARTESIAN_POINT ( 'NONE',  ( 4.999999999999992006, -8.660254037844389075, -117.7500000000000000 ) ) ;
#24452 = CARTESIAN_POINT ( 'NONE',  ( 10.81189881249999551, -6.242252689847874514, -133.6562500020483810 ) ) ;
#24453 = CARTESIAN_POINT ( 'NONE',  ( -4.637759744350153923, 8.887906374204987969, -179.9999999999999716 ) ) ;
#24454 = CARTESIAN_POINT ( 'NONE',  ( 7.070501591499377789E-16, 11.54700538379251284, -79.62500000000000000 ) ) ;
#24455 = CARTESIAN_POINT ( 'NONE',  ( -5.405949406250003975, -9.363379034771801557, -18.53125000204835970 ) ) ;
#24456 = VERTEX_POINT ( 'NONE', #28223 ) ;
#24457 = CARTESIAN_POINT ( 'NONE',  ( 5.405949406249999534, 9.363379034771803333, -103.2812500020483952 ) ) ;
#24458 = CARTESIAN_POINT ( 'NONE',  ( 9.999999999999998224, 0.000000000000000000, -125.3750000040967905 ) ) ;
#24459 = DIRECTION ( 'NONE',  ( -1.000000000000000000, 0.000000000000000000, 0.000000000000000000 ) ) ;
#24460 = CARTESIAN_POINT ( 'NONE',  ( -2.121150477449813534E-15, -11.54700538379251284, -37.25000000409676204 ) ) ;
#24461 = CARTESIAN_POINT ( 'NONE',  ( -1.040834085586084257E-14, 139.9999999999999716, 22.49999999999999289 ) ) ;
#24462 = CARTESIAN_POINT ( 'NONE',  ( -2.293366432827344421E-15, -12.48450537969573659, -46.90625000204837391 ) ) ;
#24463 = CARTESIAN_POINT ( 'NONE',  ( 9.999999999999998224, 1.224646799147353059E-15, -99.99999999999998579 ) ) ;
#24464 = CARTESIAN_POINT ( 'NONE',  ( 10.81189881249999907, 6.242252689847868297, -152.9062500020483810 ) ) ;
#24465 = CARTESIAN_POINT ( 'NONE',  ( -10.81189881249999907, -6.242252689847864744, -127.9687500020483810 ) ) ;
#24466 = CARTESIAN_POINT ( 'NONE',  ( 9.999999999999998224, 0.000000000000000000, -144.5000000000000000 ) ) ;
#24467 = VERTEX_POINT ( 'NONE', #38137 ) ;
#24468 = CYLINDRICAL_SURFACE ( 'NONE', #13445, 9.999999999999998224 ) ;
#24469 = ORIENTED_EDGE ( 'NONE', *, *, #21677, .F. ) ;
#24470 = AXIS2_PLACEMENT_3D ( 'NONE', #31409, #34860, #5282 ) ;
#24471 = ORIENTED_EDGE ( 'NONE', *, *, #4603, .F. ) ;
#24472 = VERTEX_POINT ( 'NONE', #33903 ) ;
#24473 = CARTESIAN_POINT ( 'NONE',  ( -5.405949406249996869, 9.363379034771805109, -189.8437500020483810 ) ) ;
#24474 = CARTESIAN_POINT ( 'NONE',  ( 10.81189881249999551, -6.242252689847874514, -37.46875000204836681 ) ) ;
#24475 = CARTESIAN_POINT ( 'NONE',  ( -3.753323245683507281, -9.574262767213205905, 1.142019215729699996E-14 ) ) ;
#24476 = CARTESIAN_POINT ( 'NONE',  ( -9.999999999999998224, 1.224646799147353059E-15, -133.2499999999999716 ) ) ;
#24477 = CARTESIAN_POINT ( 'NONE',  ( 10.81189881249999729, 6.242252689847867408, -170.7187500020483810 ) ) ;
#24478 = CARTESIAN_POINT ( 'NONE',  ( 5.405949406249999534, 9.363379034771803333, -164.5937500020484094 ) ) ;
#24479 = CARTESIAN_POINT ( 'NONE',  ( -9.999999999999998224, 1.224646799147353059E-15, -200.0000000000000000 ) ) ;
#24480 = CARTESIAN_POINT ( 'NONE',  ( -10.81189881249999729, 1.324075727343319199E-15, -143.0937500020483810 ) ) ;
#24481 = CARTESIAN_POINT ( 'NONE',  ( -5.405949406249996869, 9.363379034771805109, -149.5312500020483810 ) ) ;
#24482 = CARTESIAN_POINT ( 'NONE',  ( -2.293366432827344421E-15, -12.48450537969573659, -153.2187500020483810 ) ) ;
#24483 = CARTESIAN_POINT ( 'NONE',  ( 0.000000000000000000, 0.000000000000000000, -200.0000000000000000 ) ) ;
#24484 = CARTESIAN_POINT ( 'NONE',  ( -9.999999999999479527, -5.773502691896549521, -139.5000000040967620 ) ) ;
#24485 = CARTESIAN_POINT ( 'NONE',  ( 10.00000000000000000, 5.773502691896255534, -168.3750000000000000 ) ) ;
#24486 = CARTESIAN_POINT ( 'NONE',  ( 10.81189881249999729, 0.000000000000000000, -91.34375000204838102 ) ) ;
#24487 = CARTESIAN_POINT ( 'NONE',  ( -5.405949406249996869, 9.363379034771805109, -55.03125000204836681 ) ) ;
#24488 = CARTESIAN_POINT ( 'NONE',  ( -9.999999999999479527, -5.773502691896549521, -124.5000000040967620 ) ) ;
#24489 = CARTESIAN_POINT ( 'NONE',  ( -10.81189881249999729, 6.242252689847871849, -177.7187500020483810 ) ) ;
#24490 = CARTESIAN_POINT ( 'NONE',  ( -5.405949406250003975, -9.363379034771801557, -114.5312500020483952 ) ) ;
#24491 = CARTESIAN_POINT ( 'NONE',  ( -5.405949406249996869, 9.363379034771805109, -157.0312500020484094 ) ) ;
#24492 = DIRECTION ( 'NONE',  ( -0.000000000000000000, -0.000000000000000000, -1.000000000000000000 ) ) ;
#24493 = CARTESIAN_POINT ( 'NONE',  ( -5.405949406249996869, 9.363379034771805109, -46.03125000204838813 ) ) ;
#24494 = CARTESIAN_POINT ( 'NONE',  ( -5.000000000000003553, -8.660254037844383745, -130.3750000040967905 ) ) ;
#24495 = CARTESIAN_POINT ( 'NONE',  ( -9.999999999999998224, 5.773502691896259087, -107.8749999999999858 ) ) ;
#24496 = ORIENTED_EDGE ( 'NONE', *, *, #38294, .T. ) ;
#24497 = CIRCLE ( 'NONE', #24470, 14.99999999999998579 ) ;
#24498 = CARTESIAN_POINT ( 'NONE',  ( 5.405949406249992428, -9.363379034771808662, -124.7812500020483952 ) ) ;
#24499 = CARTESIAN_POINT ( 'NONE',  ( -9.999999999999998224, 5.773502691896259087, -144.2500000040967905 ) ) ;
#24500 = CARTESIAN_POINT ( 'NONE',  ( -5.405949406249996869, 9.363379034771805109, -182.5312500020484094 ) ) ;
#24501 = VERTEX_POINT ( 'NONE', #10996 ) ;
#24502 = CARTESIAN_POINT ( 'NONE',  ( -2.121150477449813534E-15, -11.54700538379251284, -51.87499999999997158 ) ) ;
#24503 = CARTESIAN_POINT ( 'NONE',  ( -2.293366432827344421E-15, -12.48450537969573659, -171.2187500020484094 ) ) ;
#24504 = CARTESIAN_POINT ( 'NONE',  ( 5.000000000000000000, 8.660254037844385522, -54.62500000409675494 ) ) ;
#24505 = CARTESIAN_POINT ( 'NONE',  ( -9.999999999999998224, 1.224646799147353059E-15, -19.24999999999996092 ) ) ;
#24506 = CARTESIAN_POINT ( 'NONE',  ( -10.81189881249999729, 6.242252689847871849, -71.40625000204839523 ) ) ;
#24507 = CARTESIAN_POINT ( 'NONE',  ( 7.644554776091147741E-16, 12.48450537969573659, -50.65625000204838102 ) ) ;
#24508 = ADVANCED_FACE ( 'NONE', ( #21731 ), #8581, .T. ) ;
#24509 = CARTESIAN_POINT ( 'NONE',  ( -9.999999999999998224, 5.773502691896259087, -45.25000000409676915 ) ) ;
#24510 = CARTESIAN_POINT ( 'NONE',  ( -10.81189881249999729, 1.324075727343319199E-15, -3.593750002048368142 ) ) ;
#24511 = CARTESIAN_POINT ( 'NONE',  ( 7.070501591499376803E-16, 11.54700538379251284, -88.62500000000000000 ) ) ;
#24512 = CARTESIAN_POINT ( 'NONE',  ( 5.405949406249992428, -9.363379034771808662, -177.2812500020484094 ) ) ;
#24513 = CARTESIAN_POINT ( 'NONE',  ( -9.999999999999479527, -5.773502691896549521, -73.50000000409674783 ) ) ;
#24514 = CARTESIAN_POINT ( 'NONE',  ( 4.999999999999992006, -8.660254037844389075, -81.74999999999998579 ) ) ;
#24515 = ORIENTED_EDGE ( 'NONE', *, *, #23598, .T. ) ;
#24516 = LINE ( 'NONE', #26887, #7696 ) ;
#24517 = CARTESIAN_POINT ( 'NONE',  ( 10.00000000000102318, -5.773502691895667560, -60.62499999999995026 ) ) ;
#24518 = AXIS2_PLACEMENT_3D ( 'NONE', #14437, #24190, #23973 ) ;
#24519 =( BOUNDED_CURVE ( )  B_SPLINE_CURVE ( 2, ( #42220, #25840, #17369, #16732, #23879, #33803, #10056 ),
 .UNSPECIFIED., .F., .F. ) 
 B_SPLINE_CURVE_WITH_KNOTS ( ( 3, 2, 2, 3 ),
 ( 0.1455223880597014963, 0.1467661691542288538, 0.1480099502487562391, 0.1492537313432835966 ),
 .UNSPECIFIED. ) 
 CURVE ( )  GEOMETRIC_REPRESENTATION_ITEM ( )  RATIONAL_B_SPLINE_CURVE ( ( 1.000000000000000000, 0.8660254037844387076, 1.000000000000000000, 0.8660254037844387076, 1.000000000000000000, 0.8660254037844357100, 1.000000000000003109 ) ) 
 REPRESENTATION_ITEM ( '' )  );
#24520 = DIRECTION ( 'NONE',  ( -0.000000000000000000, -0.000000000000000000, 1.000000000000000000 ) ) ;
#24522 = ORIENTED_EDGE ( 'NONE', *, *, #39892, .F. ) ;
#24521 = CARTESIAN_POINT ( 'NONE',  ( -10.81189881249999729, 6.242252689847871849, -89.40625000204838102 ) ) ;
#24524 = ORIENTED_EDGE ( 'NONE', *, *, #17760, .T. ) ;
#24523 = CARTESIAN_POINT ( 'NONE',  ( 4.999999999999992006, -8.660254037844389075, -122.6250000040967905 ) ) ;
#24525 = AXIS2_PLACEMENT_3D ( 'NONE', #29188, #20090, #39938 ) ;
#24526 = ORIENTED_EDGE ( 'NONE', *, *, #19360, .T. ) ;
#24527 = CARTESIAN_POINT ( 'NONE',  ( -10.81189881249999729, 6.242252689847871849, -38.21875000204837391 ) ) ;
#24528 = CARTESIAN_POINT ( 'NONE',  ( -10.81189881249999907, -6.242252689847864744, -24.46875000204836681 ) ) ;
#24529 = CARTESIAN_POINT ( 'NONE',  ( -2.293366432827344421E-15, -12.48450537969573659, -16.90625000204838102 ) ) ;
#24531 = ORIENTED_EDGE ( 'NONE', *, *, #27009, .F. ) ;
#24530 = CARTESIAN_POINT ( 'NONE',  ( -5.405949406249996869, 9.363379034771805109, -65.34375000204836681 ) ) ;
#24532 = CYLINDRICAL_SURFACE ( 'NONE', #36677, 9.999999999999998224 ) ;
#24533 = EDGE_CURVE ( 'NONE', #5420, #7881, #28444, .T. ) ;
#24534 = CARTESIAN_POINT ( 'NONE',  ( -4.999999999999996447, 8.660254037844387298, -32.99999999999997158 ) ) ;
#24535 = CARTESIAN_POINT ( 'NONE',  ( 7.644554776091147741E-16, 12.48450537969573659, -186.9687500020483810 ) ) ;
#24536 = CARTESIAN_POINT ( 'NONE',  ( 5.405949406249999534, 9.363379034771803333, -164.5937500020484094 ) ) ;
#24537 = CARTESIAN_POINT ( 'NONE',  ( -9.999999999999998224, 1.224646799147353059E-15, -183.1250000040967905 ) ) ;
#24538 = LINE ( 'NONE', #1442, #3323 ) ;
#24539 = CARTESIAN_POINT ( 'NONE',  ( 7.070501591499376803E-16, 11.54700538379251284, -126.1249999999999858 ) ) ;
#24540 = LINE ( 'NONE', #17820, #3967 ) ;
#24541 = CARTESIAN_POINT ( 'NONE',  ( 7.644554776091147741E-16, 12.48450537969573659, -116.4687500020483952 ) ) ;
#24542 = DIRECTION ( 'NONE',  ( -0.000000000000000000, -0.000000000000000000, 1.000000000000000000 ) ) ;
#24543 = CARTESIAN_POINT ( 'NONE',  ( -5.405949406249996869, 9.363379034771805109, -82.03125000204839523 ) ) ;
#24544 = CARTESIAN_POINT ( 'NONE',  ( -5.405949406249996869, 9.363379034771805109, -98.34375000204838102 ) ) ;
#24545 = CARTESIAN_POINT ( 'NONE',  ( 5.405949406249992428, -9.363379034771808662, -58.59375000204835970 ) ) ;
#24546 = CIRCLE ( 'NONE', #5935, 5.000000000000002665 ) ;
#24547 = CARTESIAN_POINT ( 'NONE',  ( -10.81189881249999729, 1.324075727343319199E-15, -65.28125000204838102 ) ) ;
#24548 = CARTESIAN_POINT ( 'NONE',  ( 10.00000000000000000, 5.773502691896255534, -155.2500000040967905 ) ) ;
#24549 = CARTESIAN_POINT ( 'NONE',  ( 7.070501591499377789E-16, 11.54700538379251284, -133.6250000000000000 ) ) ;
#24550 = VECTOR ( 'NONE', #6095, 1000.000000000000000 ) ;
#24551 = CARTESIAN_POINT ( 'NONE',  ( 7.644554776091147741E-16, 12.48450537969573659, -151.1562500020484094 ) ) ;
#24552 = CARTESIAN_POINT ( 'NONE',  ( -10.81189881249999729, 6.242252689847871849, -167.4062500020483810 ) ) ;
#24553 = CARTESIAN_POINT ( 'NONE',  ( 9.999999999999998224, 0.000000000000000000, -200.0000000000000000 ) ) ;
#24554 = CARTESIAN_POINT ( 'NONE',  ( -9.999999999999998224, 1.224646799147353059E-15, -200.0000000000000000 ) ) ;
#24555 = CARTESIAN_POINT ( 'NONE',  ( -5.405949406250003975, -9.363379034771801557, -100.8437500020483810 ) ) ;
#24556 = CARTESIAN_POINT ( 'NONE',  ( 7.070501591499376803E-16, 11.54700538379251284, -42.50000000409675494 ) ) ;
#24557 = CARTESIAN_POINT ( 'NONE',  ( 5.000000000000000000, 8.660254037844385522, -76.74999999999998579 ) ) ;
#24558 = CARTESIAN_POINT ( 'NONE',  ( -10.81189881249999729, 1.324075727343319199E-15, -192.5937500020484094 ) ) ;
#24559 = CARTESIAN_POINT ( 'NONE',  ( 7.070501591499377789E-16, 11.54700538379251284, -81.50000000409677625 ) ) ;
#24560 = VECTOR ( 'NONE', #21114, 1000.000000000000000 ) ;
#24561 = LINE ( 'NONE', #37710, #14787 ) ;
#24562 = CARTESIAN_POINT ( 'NONE',  ( 10.81189881249999729, 0.000000000000000000, -91.53125000204838102 ) ) ;
#24563 = CARTESIAN_POINT ( 'NONE',  ( 10.81189881249999729, 6.242252689847867408, -79.40625000204836681 ) ) ;
#24564 = CARTESIAN_POINT ( 'NONE',  ( 9.999999999999996447, -5.773502691896262640, -74.50000000409677625 ) ) ;
#24565 = CARTESIAN_POINT ( 'NONE',  ( 8.660254037844444142, 15.00000000000011191, 49.99999999999998579 ) ) ;
#24566 = CARTESIAN_POINT ( 'NONE',  ( -10.81189881249999729, 6.242252689847871849, -23.21875000204837036 ) ) ;
#24567 = VERTEX_POINT ( 'NONE', #11793 ) ;
#24568 = CARTESIAN_POINT ( 'NONE',  ( 5.405949406249992428, -9.363379034771808662, -198.2812500020484094 ) ) ;
#24569 = CARTESIAN_POINT ( 'NONE',  ( -5.405949406249996869, 9.363379034771805109, -31.03125000204837036 ) ) ;
#24570 = EDGE_CURVE ( 'NONE', #17801, #8961, #37231, .T. ) ;
#24571 = CARTESIAN_POINT ( 'NONE',  ( -10.81189881249999729, 6.242252689847871849, -17.21875000204836681 ) ) ;
#24572 = PLANE ( 'NONE',  #23452 ) ;
#24573 = CARTESIAN_POINT ( 'NONE',  ( 10.00000000000000000, 5.773502691896255534, -6.750000004096756712 ) ) ;
#24574 = CARTESIAN_POINT ( 'NONE',  ( 7.071067811865472841, -7.071067811865472841, -200.0000000000000000 ) ) ;
#24575 = CARTESIAN_POINT ( 'NONE',  ( 10.81189881249999729, 0.000000000000000000, -127.5312500020483952 ) ) ;
#24576 = CARTESIAN_POINT ( 'NONE',  ( -2.121150477449813534E-15, -11.54700538379251284, -185.3750000000000284 ) ) ;
#24577 = DIRECTION ( 'NONE',  ( -1.000000000000000000, 0.000000000000000000, 0.000000000000000000 ) ) ;
#24579 = ORIENTED_EDGE ( 'NONE', *, *, #11173, .T. ) ;
#24578 = CARTESIAN_POINT ( 'NONE',  ( 10.81189881249999907, 6.242252689847868297, -106.4062500020483952 ) ) ;
#24580 = DIRECTION ( 'NONE',  ( -0.000000000000000000, -0.000000000000000000, 1.000000000000000000 ) ) ;
#24581 = ORIENTED_EDGE ( 'NONE', *, *, #33696, .T. ) ;
#24582 = VECTOR ( 'NONE', #31706, 1000.000000000000000 ) ;
#24583 = ORIENTED_EDGE ( 'NONE', *, *, #26212, .F. ) ;
#24584 = CARTESIAN_POINT ( 'NONE',  ( -5.405949406249996869, 9.363379034771805109, -37.03125000204837391 ) ) ;
#24585 = CALENDAR_DATE ( 2026, 28, 9 ) ;
#24586 = CARTESIAN_POINT ( 'NONE',  ( 10.81189881249999729, 0.000000000000000000, -85.34375000204836681 ) ) ;
#24587 = DIRECTION ( 'NONE',  ( -0.000000000000000000, -0.000000000000000000, -1.000000000000000000 ) ) ;
#24588 = LINE ( 'NONE', #1059, #15577 ) ;
#24589 = CARTESIAN_POINT ( 'NONE',  ( -4.999999999999996447, 8.660254037844387298, -169.8750000040967905 ) ) ;
#24590 = CARTESIAN_POINT ( 'NONE',  ( -2.293366432827344421E-15, -12.48450537969573659, -165.4062500020483810 ) ) ;
#24591 = CARTESIAN_POINT ( 'NONE',  ( -2.293366432827344421E-15, -12.48450537969573659, -127.7187500020483952 ) ) ;
#24592 = CARTESIAN_POINT ( 'NONE',  ( -10.81189881249999729, 1.324075727343319199E-15, -86.09375000204836681 ) ) ;
#24593 = CARTESIAN_POINT ( 'NONE',  ( 5.405949406249999534, 9.363379034771803333, -2.781250002048374359 ) ) ;
#24594 = CARTESIAN_POINT ( 'NONE',  ( 7.644554776091147741E-16, 12.48450537969573659, -194.4687500020484094 ) ) ;
#24595 = CARTESIAN_POINT ( 'NONE',  ( 10.81189881249999907, 6.242252689847868297, -94.40625000204836681 ) ) ;
#24596 = CARTESIAN_POINT ( 'NONE',  ( -9.999999999999998224, 5.773502691896259087, -175.7500000040967905 ) ) ;
#24597 = CARTESIAN_POINT ( 'NONE',  ( 5.405949406249999534, 9.363379034771803333, -173.7812500020484094 ) ) ;
#24598 = CARTESIAN_POINT ( 'NONE',  ( -9.999999999999998224, 1.224646799147353059E-15, -1.625000004096766038 ) ) ;
#24599 = CARTESIAN_POINT ( 'NONE',  ( -5.405949406249996869, 9.363379034771805109, -170.5312500020484094 ) ) ;
#24600 = CARTESIAN_POINT ( 'NONE',  ( 5.405949406249992428, -9.363379034771808662, -187.7812500020484094 ) ) ;
#24601 = CARTESIAN_POINT ( 'NONE',  ( -10.81189881249999729, 1.324075727343319199E-15, -53.09375000204835970 ) ) ;
#24602 = CARTESIAN_POINT ( 'NONE',  ( 4.999999999999992006, -8.660254037844389075, -161.6250000040967905 ) ) ;
#24603 = CARTESIAN_POINT ( 'NONE',  ( -10.81189881249999907, -6.242252689847864744, -11.15625000204838457 ) ) ;
#24604 = CARTESIAN_POINT ( 'NONE',  ( 10.81189881249999907, 6.242252689847868297, -11.71875000204836148 ) ) ;
#24605 = CARTESIAN_POINT ( 'NONE',  ( 9.999999999999998224, 0.000000000000000000, -152.3750000040967905 ) ) ;
#24606 = CARTESIAN_POINT ( 'NONE',  ( 7.644554776091147741E-16, 12.48450537969573659, -122.4687500020483952 ) ) ;
#24607 = CARTESIAN_POINT ( 'NONE',  ( -4.999999999999996447, 8.660254037844387298, -98.99999999999998579 ) ) ;
#24608 = CARTESIAN_POINT ( 'NONE',  ( -10.81189881249999729, 6.242252689847871849, -30.90625000204835615 ) ) ;
#24609 = CARTESIAN_POINT ( 'NONE',  ( -9.999999999999998224, 1.224646799147353059E-15, -105.1250000040967763 ) ) ;
#24610 =( BOUNDED_CURVE ( )  B_SPLINE_CURVE ( 2, ( #38419, #38206, #8223, #25063, #34985, #28511, #35193 ),
 .UNSPECIFIED., .F., .F. ) 
 B_SPLINE_CURVE_WITH_KNOTS ( ( 3, 2, 2, 3 ),
 ( 0.7649253731343285123, 0.7661691542288557866, 0.7674129353233831718, 0.7686567164179105571 ),
 .UNSPECIFIED. ) 
 CURVE ( )  GEOMETRIC_REPRESENTATION_ITEM ( )  RATIONAL_B_SPLINE_CURVE ( ( 0.9999999999999880096, 0.8660254037844506980, 1.000000000000000000, 0.8660254037844387076, 1.000000000000000000, 0.8660254037844267172, 1.000000000000011990 ) ) 
 REPRESENTATION_ITEM ( '' )  );
#24611 = CARTESIAN_POINT ( 'NONE',  ( 9.999999999999998224, 0.000000000000000000, -189.8750000040967905 ) ) ;
#24612 = CARTESIAN_POINT ( 'NONE',  ( 9.999999999999996447, -5.773502691896262640, -51.62499999999998579 ) ) ;
#24613 = CARTESIAN_POINT ( 'NONE',  ( 7.644554776091147741E-16, 12.48450537969573659, -125.6562500020483810 ) ) ;
#24614 = CARTESIAN_POINT ( 'NONE',  ( -2.293366432827344421E-15, -12.48450537969573659, -96.40625000204838102 ) ) ;
#24615 = ORIENTED_EDGE ( 'NONE', *, *, #11920, .F. ) ;
#24616 = CARTESIAN_POINT ( 'NONE',  ( 7.070501591499377789E-16, 11.54700538379251284, -96.50000000409679046 ) ) ;
#24617 = CARTESIAN_POINT ( 'NONE',  ( -9.999999999999742428, -5.773502691896402084, -151.5000000040967620 ) ) ;
#24618 = CC_DESIGN_APPROVAL ( #29638, ( #25992 ) ) ;
#24619 = CARTESIAN_POINT ( 'NONE',  ( -10.81189881249999729, 1.324075727343319199E-15, -162.7812500020484094 ) ) ;
#24620 = CARTESIAN_POINT ( 'NONE',  ( 5.405949406249992428, -9.363379034771808662, -57.09375000204835970 ) ) ;
#24621 = ORIENTED_EDGE ( 'NONE', *, *, #9588, .F. ) ;
#24622 = CARTESIAN_POINT ( 'NONE',  ( -9.999999999999998224, 1.224646799147353059E-15, -22.24999999999996447 ) ) ;
#24623 = ADVANCED_FACE ( 'NONE', ( #35961 ), #25827, .T. ) ;
#24624 = EDGE_CURVE ( 'NONE', #134, #15029, #39192, .T. ) ;
#24625 = CARTESIAN_POINT ( 'NONE',  ( 10.81189881249999729, 6.242252689847867408, -29.90625000204835970 ) ) ;
#24626 = CARTESIAN_POINT ( 'NONE',  ( 10.00000000000000000, 5.773502691896255534, -157.8749999999999716 ) ) ;
#24627 = CARTESIAN_POINT ( 'NONE',  ( -9.999999999999479527, -5.773502691896549521, -92.62499999999997158 ) ) ;
#24628 = CARTESIAN_POINT ( 'NONE',  ( 9.999999999999996447, -5.773502691896262640, -29.50000000409674783 ) ) ;
#24629 = EDGE_CURVE ( 'NONE', #40862, #36973, #5979, .T. ) ;
#24630 = EDGE_CURVE ( 'NONE', #24022, #5784, #8009, .T. ) ;
#24631 = CARTESIAN_POINT ( 'NONE',  ( 10.00000000000154010, -5.773502691895370020, -23.12499999999993605 ) ) ;
#24632 = CARTESIAN_POINT ( 'NONE',  ( -10.81189881249999729, 6.242252689847871849, -137.4062500020484094 ) ) ;
#24633 = CARTESIAN_POINT ( 'NONE',  ( -3.495063195231654873, 9.449490074020786778, 7.031793886498072016E-15 ) ) ;
#24634 = CARTESIAN_POINT ( 'NONE',  ( -9.999999999999998224, 1.224646799147353059E-15, -142.6250000040967905 ) ) ;
#24635 = ORIENTED_EDGE ( 'NONE', *, *, #4580, .F. ) ;
#24636 = CARTESIAN_POINT ( 'NONE',  ( 10.81189881249999551, -6.242252689847874514, -63.15625000204837391 ) ) ;
#24637 = APPROVAL_STATUS ( 'not_yet_approved' ) ;
#24639 = ORIENTED_EDGE ( 'NONE', *, *, #21511, .T. ) ;
#24638 = VERTEX_POINT ( 'NONE', #26040 ) ;
#24640 = ADVANCED_FACE ( 'NONE', ( #19542 ), #22372, .T. ) ;
#24641 = DIRECTION ( 'NONE',  ( 0.000000000000000000, -1.000000000000000000, 0.000000000000000000 ) ) ;
#24642 = CARTESIAN_POINT ( 'NONE',  ( -2.121150477449813534E-15, -11.54700538379251284, -55.25000000409677625 ) ) ;
#24643 = CARTESIAN_POINT ( 'NONE',  ( 7.644554776091147741E-16, 12.48450537969573659, -159.9687500020483810 ) ) ;
#24644 = EDGE_CURVE ( 'NONE', #26035, #3072, #35872, .T. ) ;
#24645 = CARTESIAN_POINT ( 'NONE',  ( -5.405949406249996869, 9.363379034771805109, -188.5312500020484094 ) ) ;
#24646 = CARTESIAN_POINT ( 'NONE',  ( 5.405949406249992428, -9.363379034771808662, -18.09375000204835260 ) ) ;
#24647 = EDGE_CURVE ( 'NONE', #13289, #20204, #12392, .T. ) ;
#24648 = CARTESIAN_POINT ( 'NONE',  ( -5.405949406249996869, 9.363379034771805109, -149.3437500020483810 ) ) ;
#24649 = CARTESIAN_POINT ( 'NONE',  ( 5.405949406249992428, -9.363379034771808662, -132.0937500020483810 ) ) ;
#24650 = CARTESIAN_POINT ( 'NONE',  ( -2.293366432827344421E-15, -12.48450537969573659, -103.9062500020483810 ) ) ;
#24651 = CARTESIAN_POINT ( 'NONE',  ( 5.405949406249992428, -9.363379034771808662, -109.5937500020483810 ) ) ;
#24652 = FACE_OUTER_BOUND ( 'NONE', #16252, .T. ) ;
#24653 = CARTESIAN_POINT ( 'NONE',  ( -2.293366432827344421E-15, -12.48450537969573659, -114.4062500020483952 ) ) ;
#24654 = CARTESIAN_POINT ( 'NONE',  ( -10.81189881249999729, 6.242252689847871849, -3.718750002048365477 ) ) ;
#24655 = CARTESIAN_POINT ( 'NONE',  ( 7.644554776091147741E-16, 12.48450537969573659, -132.9687500020483810 ) ) ;
#24656 = CARTESIAN_POINT ( 'NONE',  ( -10.81189881249999729, -6.242252689847864744, -192.6562500020484094 ) ) ;
#24657 =( BOUNDED_CURVE ( )  B_SPLINE_CURVE ( 2, ( #35883, #29616, #19253, #36509, #9754, #19465, #25959 ),
 .UNSPECIFIED., .F., .F. ) 
 B_SPLINE_CURVE_WITH_KNOTS ( ( 3, 2, 2, 3 ),
 ( 0.6828358208955226383, 0.6840796019900500236, 0.6853233830845772978, 0.6865671641791046831 ),
 .UNSPECIFIED. ) 
 CURVE ( )  GEOMETRIC_REPRESENTATION_ITEM ( )  RATIONAL_B_SPLINE_CURVE ( ( 0.9999999999999761302, 0.8660254037844625774, 1.000000000000000000, 0.8660254037844387076, 1.000000000000000000, 0.8660254037844148378, 1.000000000000023981 ) ) 
 REPRESENTATION_ITEM ( '' )  );
#24658 = FACE_OUTER_BOUND ( 'NONE', #39551, .T. ) ;
#24659 = CARTESIAN_POINT ( 'NONE',  ( 10.00000000000000000, 5.773502691896255534, -147.3750000000000000 ) ) ;
#24660 = CARTESIAN_POINT ( 'NONE',  ( -10.00000000000000000, -5.773502691896251982, -22.12499999999997868 ) ) ;
#24661 = CARTESIAN_POINT ( 'NONE',  ( -2.293366432827344421E-15, -12.48450537969573659, -72.21875000204835260 ) ) ;
#24662 = CARTESIAN_POINT ( 'NONE',  ( -10.81189881249999907, -6.242252689847864744, -54.46875000204838102 ) ) ;
#24663 = CARTESIAN_POINT ( 'NONE',  ( -9.999999999999998224, 1.224646799147353059E-15, -200.0000000000000000 ) ) ;
#24664 = CARTESIAN_POINT ( 'NONE',  ( 5.405949406249999534, 9.363379034771803333, -37.28125000204837391 ) ) ;
#24665 = CARTESIAN_POINT ( 'NONE',  ( -10.81189881249999907, -6.242252689847864744, -46.96875000204835970 ) ) ;
#24666 = CARTESIAN_POINT ( 'NONE',  ( -4.999999999999996447, 8.660254037844387298, -94.87500000409677625 ) ) ;
#24667 = CARTESIAN_POINT ( 'NONE',  ( -10.81189881249999729, 1.324075727343319199E-15, -158.0937500020483810 ) ) ;
#24668 = CARTESIAN_POINT ( 'NONE',  ( -10.00000000000000000, -5.773502691896251982, -119.6249999999999858 ) ) ;
#24669 = CARTESIAN_POINT ( 'NONE',  ( 3.157157116567558486, 9.864526434127757426, -180.0000000000001137 ) ) ;
#24670 = CARTESIAN_POINT ( 'NONE',  ( 9.999999999999998224, 0.000000000000000000, -73.99999999999998579 ) ) ;
#24671 = CARTESIAN_POINT ( 'NONE',  ( -10.81189881249999729, 6.242252689847871849, -8.406250002048372139 ) ) ;
#24672 = ORIENTED_EDGE ( 'NONE', *, *, #29446, .F. ) ;
#24673 = CARTESIAN_POINT ( 'NONE',  ( 10.81189881249999729, 0.000000000000000000, -100.5312500020483952 ) ) ;
#24674 = CARTESIAN_POINT ( 'NONE',  ( -9.999999999999998224, 5.773502691896259087, -121.7500000040967905 ) ) ;
#24675 = CARTESIAN_POINT ( 'NONE',  ( -9.999999999999998224, 1.224646799147353059E-15, -124.2500000000000000 ) ) ;
#24676 = CARTESIAN_POINT ( 'NONE',  ( 10.81189881249999729, 0.000000000000000000, -83.84375000204836681 ) ) ;
#24677 = CARTESIAN_POINT ( 'NONE',  ( 9.999999999999998224, 0.000000000000000000, -30.87500000409676559 ) ) ;
#24678 = CARTESIAN_POINT ( 'NONE',  ( 10.00000000000154010, -5.773502691895370020, -14.12499999999992895 ) ) ;
#24679 = CARTESIAN_POINT ( 'NONE',  ( -5.405949406250003975, -9.363379034771801557, -42.53125000204838102 ) ) ;
#24680 = EDGE_CURVE ( 'NONE', #6263, #15924, #16795, .T. ) ;
#24681 = CARTESIAN_POINT ( 'NONE',  ( 5.405949406249992428, -9.363379034771808662, -142.7812500020483810 ) ) ;
#24682 = ADVANCED_FACE ( 'NONE', ( #10040 ), #36382, .T. ) ;
#24683 = CARTESIAN_POINT ( 'NONE',  ( 5.405949406249999534, 9.363379034771803333, -124.0937500020483952 ) ) ;
#24684 = CARTESIAN_POINT ( 'NONE',  ( -4.999999999999996447, 8.660254037844387298, -103.8750000040967763 ) ) ;
#24685 = FACE_OUTER_BOUND ( 'NONE', #6312, .T. ) ;
#24686 = ORIENTED_EDGE ( 'NONE', *, *, #17633, .F. ) ;
#24687 = EDGE_LOOP ( 'NONE', ( #34395, #26370, #39939, #27912 ) ) ;
#24688 = AXIS2_PLACEMENT_3D ( 'NONE', #40363, #33293, #908 ) ;
#24689 = ORIENTED_EDGE ( 'NONE', *, *, #26728, .T. ) ;
#24690 = VECTOR ( 'NONE', #16472, 1000.000000000000000 ) ;
#24691 = ADVANCED_FACE ( 'NONE', ( #9203 ), #16079, .T. ) ;
#24692 = DIRECTION ( 'NONE',  ( -0.000000000000000000, -0.000000000000000000, 1.000000000000000000 ) ) ;
#24693 = CARTESIAN_POINT ( 'NONE',  ( -10.81189881249999729, 6.242252689847871849, -192.7187500020483810 ) ) ;
#24694 = CARTESIAN_POINT ( 'NONE',  ( 10.81189881249999729, 0.000000000000000000, -40.34375000204837391 ) ) ;
#24695 = CARTESIAN_POINT ( 'NONE',  ( 7.070501591499376803E-16, 11.54700538379251284, -110.0000000040968047 ) ) ;
#24696 = CARTESIAN_POINT ( 'NONE',  ( 4.999999999999992006, -8.660254037844389075, -74.24999999999998579 ) ) ;
#24697 = CARTESIAN_POINT ( 'NONE',  ( 10.81189881249999729, 6.242252689847867408, -169.2187500020483810 ) ) ;
#24698 = CARTESIAN_POINT ( 'NONE',  ( 7.644554776091147741E-16, 12.48450537969573659, -152.4687500020483810 ) ) ;
#24699 = CARTESIAN_POINT ( 'NONE',  ( 9.999999999999998224, 0.000000000000000000, -24.87500000409675849 ) ) ;
#24700 = CARTESIAN_POINT ( 'NONE',  ( 10.81189881249999729, 0.000000000000000000, -142.3437500020483810 ) ) ;
#24701 = CARTESIAN_POINT ( 'NONE',  ( 7.644554776091147741E-16, 12.48450537969573659, -146.6562500020484379 ) ) ;
#24702 = CARTESIAN_POINT ( 'NONE',  ( -5.405949406250003975, -9.363379034771801557, -157.8437500020483810 ) ) ;
#24703 = CARTESIAN_POINT ( 'NONE',  ( -10.00000000000102496, 5.773502691895664007, -86.87499999999997158 ) ) ;
#24704 = CARTESIAN_POINT ( 'NONE',  ( 7.070501591499376803E-16, 11.54700538379251284, -70.62499999999998579 ) ) ;
#24705 = CARTESIAN_POINT ( 'NONE',  ( 4.999999999999992006, -8.660254037844389075, -174.7500000000000284 ) ) ;
#24706 = CARTESIAN_POINT ( 'NONE',  ( 5.405949406249992428, -9.363379034771808662, -90.09375000204838102 ) ) ;
#24707 = CARTESIAN_POINT ( 'NONE',  ( -5.000000000000003553, -8.660254037844383745, -136.0000000000000000 ) ) ;
#24708 = CARTESIAN_POINT ( 'NONE',  ( -10.81189881249999907, -6.242252689847864744, -54.65625000204838102 ) ) ;
#24709 = CARTESIAN_POINT ( 'NONE',  ( -8.973374131346412597, -4.922417620657181914, -99.99999999999995737 ) ) ;
#24710 = CARTESIAN_POINT ( 'NONE',  ( 7.644554776091147741E-16, 12.48450537969573659, -177.9687500020483810 ) ) ;
#24711 = CARTESIAN_POINT ( 'NONE',  ( 7.644554776091147741E-16, 12.48450537969573659, -115.1562500020483952 ) ) ;
#24712 = CARTESIAN_POINT ( 'NONE',  ( 7.644554776091147741E-16, 12.48450537969573659, -157.1562500020484094 ) ) ;
#24713 = CARTESIAN_POINT ( 'NONE',  ( 9.999999999999998224, 0.000000000000000000, -134.0000000000000000 ) ) ;
#24714 = CARTESIAN_POINT ( 'NONE',  ( 10.81189881249999907, 6.242252689847868297, -41.90625000204836681 ) ) ;
#24715 = CARTESIAN_POINT ( 'NONE',  ( 4.999999999999992006, -8.660254037844389075, -127.1250000040967620 ) ) ;
#24716 = CARTESIAN_POINT ( 'NONE',  ( -9.999999999999998224, 5.773502691896259087, -101.8749999999999858 ) ) ;
#24717 = ORIENTED_EDGE ( 'NONE', *, *, #28025, .F. ) ;
#24718 = CARTESIAN_POINT ( 'NONE',  ( 10.81189881249999729, 0.000000000000000000, -126.0312500020483952 ) ) ;
#24719 = CARTESIAN_POINT ( 'NONE',  ( -2.121150477449813534E-15, -11.54700538379251284, -149.7500000040968189 ) ) ;
#24720 = CARTESIAN_POINT ( 'NONE',  ( -5.321294541346989426, 0.000000000000000000, -220.0000000000000000 ) ) ;
#24721 = CARTESIAN_POINT ( 'NONE',  ( 7.644554776091147741E-16, 12.48450537969573659, -182.6562500020484094 ) ) ;
#24722 = VERTEX_POINT ( 'NONE', #37014 ) ;
#24723 = CARTESIAN_POINT ( 'NONE',  ( -10.81189881249999729, 1.324075727343319199E-15, -176.0937500020484094 ) ) ;
#24724 = CARTESIAN_POINT ( 'NONE',  ( -9.999999999999998224, 1.224646799147353059E-15, -55.62500000409676204 ) ) ;
#24725 = VECTOR ( 'NONE', #22142, 1000.000000000000000 ) ;
#24726 = CARTESIAN_POINT ( 'NONE',  ( -9.999999999999998224, 1.836970198721029589E-15, 0.000000000000000000 ) ) ;
#24727 = CARTESIAN_POINT ( 'NONE',  ( 0.000000000000000000, 0.000000000000000000, -200.0000000000000000 ) ) ;
#24728 = CARTESIAN_POINT ( 'NONE',  ( -5.405949406249996869, 9.363379034771805109, -70.03125000204838102 ) ) ;
#24729 = CARTESIAN_POINT ( 'NONE',  ( -10.81189881249999729, 6.242252689847871849, -53.40625000204837391 ) ) ;
#24730 = CARTESIAN_POINT ( 'NONE',  ( 10.00000000000000000, 5.773502691896255534, -42.75000000409676204 ) ) ;
#24731 = CARTESIAN_POINT ( 'NONE',  ( -10.81189881249999729, 6.242252689847871849, -0.7187500020483517105 ) ) ;
#24732 = LINE ( 'NONE', #14550, #17950 ) ;
#24733 = CARTESIAN_POINT ( 'NONE',  ( -5.405949406250003975, -9.363379034771801557, -180.5312500020483810 ) ) ;
#24734 = FACE_OUTER_BOUND ( 'NONE', #13810, .T. ) ;
#24735 = CARTESIAN_POINT ( 'NONE',  ( 9.999999999999998224, 0.000000000000000000, -44.37500000409677625 ) ) ;
#24736 = ORIENTED_EDGE ( 'NONE', *, *, #25479, .F. ) ;
#24737 = CARTESIAN_POINT ( 'NONE',  ( 9.999999999998969713, 5.773502691896851502, -84.75000000409677625 ) ) ;
#24738 = CARTESIAN_POINT ( 'NONE',  ( 4.999999999999992006, -8.660254037844389075, -60.74999999999997158 ) ) ;
#24739 = CARTESIAN_POINT ( 'NONE',  ( -5.000000000000003553, -8.660254037844383745, -20.49999999999996447 ) ) ;
#24740 = EDGE_CURVE ( 'NONE', #14676, #18615, #33580, .T. ) ;
#24742 = ORIENTED_EDGE ( 'NONE', *, *, #21916, .F. ) ;
#24741 = CARTESIAN_POINT ( 'NONE',  ( 7.644554776091147741E-16, 12.48450537969573659, -76.15625000204839523 ) ) ;
#24743 = CARTESIAN_POINT ( 'NONE',  ( 0.000000000000000000, 0.000000000000000000, 0.000000000000000000 ) ) ;
#24745 = ORIENTED_EDGE ( 'NONE', *, *, #5686, .T. ) ;
#24744 = CARTESIAN_POINT ( 'NONE',  ( 9.999999999999479527, 5.773502691896553074, -81.37499999999997158 ) ) ;
#24746 = ORIENTED_EDGE ( 'NONE', *, *, #7477, .T. ) ;
#24747 = CARTESIAN_POINT ( 'NONE',  ( -5.405949406249996869, 9.363379034771805109, -41.34375000204837391 ) ) ;
#24748 = CARTESIAN_POINT ( 'NONE',  ( 9.999999999999998224, 0.000000000000000000, -186.5000000000000000 ) ) ;
#24749 = CARTESIAN_POINT ( 'NONE',  ( -5.405949406249996869, 9.363379034771805109, -11.53125000204835438 ) ) ;
#24751 = ORIENTED_EDGE ( 'NONE', *, *, #32830, .T. ) ;
#24750 = CARTESIAN_POINT ( 'NONE',  ( 10.81189881249999551, -6.242252689847874514, -59.96875000204837391 ) ) ;
#24752 = DIRECTION ( 'NONE',  ( -1.734723475976807094E-16, -1.000000000000000000, -0.000000000000000000 ) ) ;
#24753 = CARTESIAN_POINT ( 'NONE',  ( 10.00000000000000000, 5.773502691896255534, -37.87499999999996447 ) ) ;
#24754 = CARTESIAN_POINT ( 'NONE',  ( -5.405949406250003975, -9.363379034771801557, -193.8437500020484094 ) ) ;
#24755 = CARTESIAN_POINT ( 'NONE',  ( -10.81189881249999729, 6.242252689847871849, -188.2187500020483810 ) ) ;
#24756 = CARTESIAN_POINT ( 'NONE',  ( -5.405949406250003975, -9.363379034771801557, -168.3437500020484094 ) ) ;
#24757 = EDGE_CURVE ( 'NONE', #1539, #35906, #36586, .T. ) ;
#24758 = CARTESIAN_POINT ( 'NONE',  ( -10.81189881249999729, -6.242252689847864744, -175.9687500020483526 ) ) ;
#24759 = CARTESIAN_POINT ( 'NONE',  ( 10.00000000000031619, -5.773502691896077010, -182.5000000040967620 ) ) ;
#24760 = CARTESIAN_POINT ( 'NONE',  ( -5.000000000000003553, -8.660254037844383745, -167.8750000040967905 ) ) ;
#24761 = CARTESIAN_POINT ( 'NONE',  ( 9.999999999999998224, 0.000000000000000000, -103.9999999999999858 ) ) ;
#24762 = CARTESIAN_POINT ( 'NONE',  ( 9.999999999999998224, 0.000000000000000000, -194.0000000000000000 ) ) ;
#24763 = VECTOR ( 'NONE', #19963, 1000.000000000000000 ) ;
#24764 = CARTESIAN_POINT ( 'NONE',  ( -5.405949406249996869, 9.363379034771805109, -110.3437500020483810 ) ) ;
#24765 = CARTESIAN_POINT ( 'NONE',  ( -9.999999999999998224, 1.224646799147353059E-15, -166.2500000000000000 ) ) ;
#24766 = CARTESIAN_POINT ( 'NONE',  ( -5.405949406249996869, 9.363379034771805109, -79.03125000204838102 ) ) ;
#24767 = CARTESIAN_POINT ( 'NONE',  ( -10.81189881249999729, -6.242252689847864744, -88.96875000204838102 ) ) ;
#24768 = CARTESIAN_POINT ( 'NONE',  ( -10.81189881249999907, -6.242252689847864744, -58.96875000204838102 ) ) ;
#24769 = CARTESIAN_POINT ( 'NONE',  ( -5.405949406250003975, -9.363379034771801557, -66.53125000204838102 ) ) ;
#24770 = CARTESIAN_POINT ( 'NONE',  ( 9.999999999999998224, 0.000000000000000000, -155.3750000040967905 ) ) ;
#24771 = CARTESIAN_POINT ( 'NONE',  ( 9.999999999999996447, -5.773502691896262640, -134.1250000000000000 ) ) ;
#24772 = CARTESIAN_POINT ( 'NONE',  ( -5.405949406249996869, 9.363379034771805109, -151.0312500020483810 ) ) ;
#24773 = CARTESIAN_POINT ( 'NONE',  ( -5.405949406250003975, -9.363379034771801557, -167.0312500020484094 ) ) ;
#24774 = CARTESIAN_POINT ( 'NONE',  ( 9.999999999999998224, 0.000000000000000000, -12.87500000409674783 ) ) ;
#24775 = CARTESIAN_POINT ( 'NONE',  ( 10.81189881249999907, 6.242252689847868297, -95.71875000204838102 ) ) ;
#24776 = VERTEX_POINT ( 'NONE', #3795 ) ;
#24777 = CARTESIAN_POINT ( 'NONE',  ( 9.999999999999996447, -5.773502691896262640, -71.12499999999997158 ) ) ;
#24778 = CARTESIAN_POINT ( 'NONE',  ( 7.644554776091147741E-16, 12.48450537969573659, -194.4687500020484094 ) ) ;
#24779 = CARTESIAN_POINT ( 'NONE',  ( -9.999999999999998224, 1.224646799147353059E-15, -78.12500000409677625 ) ) ;
#24780 = CARTESIAN_POINT ( 'NONE',  ( -1.306318075773550857, -10.33130266446697831, -180.0000000000000284 ) ) ;
#24781 = CARTESIAN_POINT ( 'NONE',  ( 10.81189881249999551, -6.242252689847874514, -91.65625000204838102 ) ) ;
#24782 = CARTESIAN_POINT ( 'NONE',  ( 10.81189881249999551, -6.242252689847874514, -78.15625000204838102 ) ) ;
#24783 =( BOUNDED_CURVE ( )  B_SPLINE_CURVE ( 2, ( #97, #10208, #310, #27053, #6355, #13220, #40197 ),
 .UNSPECIFIED., .F., .F. ) 
 B_SPLINE_CURVE_WITH_KNOTS ( ( 3, 2, 2, 3 ),
 ( 0.01865671641791046345, 0.01990049751243783138, 0.02114427860696519584, 0.02238805970149256030 ),
 .UNSPECIFIED. ) 
 CURVE ( )  GEOMETRIC_REPRESENTATION_ITEM ( )  RATIONAL_B_SPLINE_CURVE ( ( 0.9999999999999981126, 0.8660254037844405950, 1.000000000000000000, 0.8660254037844387076, 1.000000000000000000, 0.8660254037844360431, 1.000000000000002665 ) ) 
 REPRESENTATION_ITEM ( '' )  );
#24784 = CARTESIAN_POINT ( 'NONE',  ( -2.121150477449813534E-15, -11.54700538379251284, -71.75000000409674783 ) ) ;
#24785 = CARTESIAN_POINT ( 'NONE',  ( 9.999999999999998224, 0.000000000000000000, -21.49999999999996447 ) ) ;
#24786 = CARTESIAN_POINT ( 'NONE',  ( 10.81189881249999551, -6.242252689847874514, -29.96875000204834905 ) ) ;
#24787 = EDGE_LOOP ( 'NONE', ( #24884, #9261, #34182, #2650 ) ) ;
#24788 = CARTESIAN_POINT ( 'NONE',  ( -4.999999999999996447, 8.660254037844387298, -1.499999999999973577 ) ) ;
#24789 = CARTESIAN_POINT ( 'NONE',  ( -2.293366432827344421E-15, -12.48450537969573659, -22.90625000204837747 ) ) ;
#24790 = CARTESIAN_POINT ( 'NONE',  ( 10.81189881249999551, -6.242252689847874514, -11.96875000204837214 ) ) ;
#24791 = CARTESIAN_POINT ( 'NONE',  ( -5.405949406250003975, -9.363379034771801557, -139.8437500020484094 ) ) ;
#24792 = CARTESIAN_POINT ( 'NONE',  ( -2.121150477449813534E-15, -11.54700538379251284, -37.25000000409676204 ) ) ;
#24793 = CARTESIAN_POINT ( 'NONE',  ( 5.405949406249992428, -9.363379034771808662, -132.2812500020483810 ) ) ;
#24794 = ADVANCED_FACE ( 'NONE', ( #3586 ), #1198, .T. ) ;
#24795 = CARTESIAN_POINT ( 'NONE',  ( -9.999999999999998224, 5.773502691896259087, -181.3750000000000000 ) ) ;
#24796 = CARTESIAN_POINT ( 'NONE',  ( 10.00000000000051159, -5.773502691895965988, -35.50000000409674072 ) ) ;
#24797 = AXIS2_PLACEMENT_3D ( 'NONE', #16736, #6418, #10479 ) ;
#24799 = ORIENTED_EDGE ( 'NONE', *, *, #12451, .T. ) ;
#24798 = CARTESIAN_POINT ( 'NONE',  ( -2.293366432827344421E-15, -12.48450537969573659, -109.9062500020483952 ) ) ;
#24800 = CARTESIAN_POINT ( 'NONE',  ( 7.070501591499376803E-16, 11.54700538379251284, -195.1250000000000284 ) ) ;
#24801 = ORIENTED_EDGE ( 'NONE', *, *, #25160, .T. ) ;
#24802 = ORIENTED_EDGE ( 'NONE', *, *, #39110, .T. ) ;
#24803 = AXIS2_PLACEMENT_3D ( 'NONE', #37205, #37429, #6856 ) ;
#24804 = CARTESIAN_POINT ( 'NONE',  ( -5.405949406250003975, -9.363379034771801557, -41.03125000204838102 ) ) ;
#24805 = CALENDAR_DATE ( 2026, 28, 9 ) ;
#24806 = CARTESIAN_POINT ( 'NONE',  ( -10.81189881249999729, 1.324075727343319199E-15, -87.59375000204836681 ) ) ;
#24807 = CYLINDRICAL_SURFACE ( 'NONE', #168, 9.999999999999998224 ) ;
#24808 = EDGE_CURVE ( 'NONE', #8991, #37209, #34491, .T. ) ;
#24809 = DIRECTION ( 'NONE',  ( 1.000000000000000000, 0.000000000000000000, 0.000000000000000000 ) ) ;
#24810 = DIRECTION ( 'NONE',  ( -0.000000000000000000, -0.000000000000000000, -1.000000000000000000 ) ) ;
#24811 = CARTESIAN_POINT ( 'NONE',  ( -5.405949406249996869, 9.363379034771805109, -164.5312500020484094 ) ) ;
#24812 = CARTESIAN_POINT ( 'NONE',  ( -9.999999999999998224, 1.224646799147353059E-15, -106.6250000040967763 ) ) ;
#24813 = CARTESIAN_POINT ( 'NONE',  ( 10.81189881249999729, 6.242252689847867408, -112.2187500020483810 ) ) ;
#24814 = CARTESIAN_POINT ( 'NONE',  ( -5.405949406249996869, 9.363379034771805109, -81.84375000204838102 ) ) ;
#24815 = CARTESIAN_POINT ( 'NONE',  ( -10.81189881249999729, -6.242252689847864744, -0.6562500020483670315 ) ) ;
#24816 = CARTESIAN_POINT ( 'NONE',  ( -10.81189881249999729, 1.324075727343319199E-15, -191.0937500020484094 ) ) ;
#24817 = CARTESIAN_POINT ( 'NONE',  ( 5.405949406249992428, -9.363379034771808662, -94.78125000204838102 ) ) ;
#24818 = CARTESIAN_POINT ( 'NONE',  ( 5.000000000000000000, 8.660254037844385522, -179.1250000040968189 ) ) ;
#24819 = CARTESIAN_POINT ( 'NONE',  ( -10.81189881249999729, 6.242252689847871849, -170.4062500020484094 ) ) ;
#24820 = CARTESIAN_POINT ( 'NONE',  ( -10.00000000000051337, 5.773502691895962435, -103.3749999999999858 ) ) ;
#24821 = CARTESIAN_POINT ( 'NONE',  ( 10.81189881249999551, -6.242252689847874514, -174.1562500020484094 ) ) ;
#24822 = CARTESIAN_POINT ( 'NONE',  ( 10.81189881249999907, 6.242252689847868297, -190.4062500020484094 ) ) ;
#24823 = CARTESIAN_POINT ( 'NONE',  ( -10.81189881249999729, 6.242252689847871849, -53.21875000204838102 ) ) ;
#24824 = CARTESIAN_POINT ( 'NONE',  ( -2.121150477449813534E-15, -11.54700538379251284, -164.7500000040967620 ) ) ;
#24825 = CARTESIAN_POINT ( 'NONE',  ( 10.81189881249999729, 0.000000000000000000, -10.53125000204835260 ) ) ;
#24826 = CARTESIAN_POINT ( 'NONE',  ( -5.405949406249996869, 9.363379034771805109, -9.843750002048345493 ) ) ;
#24827 = CARTESIAN_POINT ( 'NONE',  ( 4.999999999999992006, -8.660254037844389075, -164.6250000040967905 ) ) ;
#24828 = CARTESIAN_POINT ( 'NONE',  ( -5.405949406249996869, 9.363379034771805109, -122.3437500020483952 ) ) ;
#24829 = CARTESIAN_POINT ( 'NONE',  ( 10.00000000000000000, 5.773502691896255534, -99.37499999999998579 ) ) ;
#24830 = CARTESIAN_POINT ( 'NONE',  ( 10.81189881249999907, 6.242252689847868297, -22.40625000204838102 ) ) ;
#24831 = CARTESIAN_POINT ( 'NONE',  ( 10.00000000000000000, 5.773502691896255534, -108.7500000040967905 ) ) ;
#24832 = CARTESIAN_POINT ( 'NONE',  ( 9.999999999999998224, 0.000000000000000000, -82.99999999999997158 ) ) ;
#24833 = CARTESIAN_POINT ( 'NONE',  ( -10.00000000000000000, -5.773502691896251982, -49.12499999999997158 ) ) ;
#24834 = CARTESIAN_POINT ( 'NONE',  ( -5.405949406250003975, -9.363379034771801557, -116.0312500020483952 ) ) ;
#24835 = CARTESIAN_POINT ( 'NONE',  ( 10.81189881249999729, 6.242252689847867408, -95.90625000204839523 ) ) ;
#24836 = ORIENTED_EDGE ( 'NONE', *, *, #38668, .T. ) ;
#24837 = CARTESIAN_POINT ( 'NONE',  ( 5.000000000000000000, 8.660254037844385522, -95.12500000409677625 ) ) ;
#24838 = CARTESIAN_POINT ( 'NONE',  ( -5.405949406250003975, -9.363379034771801557, -158.0312500020484094 ) ) ;
#24839 = CARTESIAN_POINT ( 'NONE',  ( 10.81189881249999551, -6.242252689847874514, -46.46875000204836681 ) ) ;
#24840 = ORIENTED_EDGE ( 'NONE', *, *, #37524, .F. ) ;
#24841 = CARTESIAN_POINT ( 'NONE',  ( -5.000000000000003553, -8.660254037844383745, -26.49999999999996803 ) ) ;
#24842 = CARTESIAN_POINT ( 'NONE',  ( -2.293366432827344421E-15, -12.48450537969573659, -30.40625000204834549 ) ) ;
#24843 = CARTESIAN_POINT ( 'NONE',  ( 9.999999999999998224, 0.000000000000000000, -161.0000000000000000 ) ) ;
#24844 = CARTESIAN_POINT ( 'NONE',  ( -9.999999999999998224, 1.224646799147353059E-15, -92.74999999999998579 ) ) ;
#24845 = CARTESIAN_POINT ( 'NONE',  ( -4.999999999999996447, 8.660254037844387298, -25.87500000409675849 ) ) ;
#24846 = DIRECTION ( 'NONE',  ( 1.000000000000000000, 0.000000000000000000, 0.000000000000000000 ) ) ;
#24847 = CARTESIAN_POINT ( 'NONE',  ( -10.81189881249999907, -6.242252689847864744, -134.1562500020483810 ) ) ;
#24848 = CARTESIAN_POINT ( 'NONE',  ( 9.599872686178903436, 4.697423173897816717, 5.369687683974984427E-15 ) ) ;
#24849 = ORIENTED_EDGE ( 'NONE', *, *, #27172, .T. ) ;
#24850 = CARTESIAN_POINT ( 'NONE',  ( 5.405949406249992428, -9.363379034771808662, -58.78125000204836681 ) ) ;
#24851 = COORDINATED_UNIVERSAL_TIME_OFFSET ( 6, 0, .AHEAD. ) ;
#24853 = ORIENTED_EDGE ( 'NONE', *, *, #19452, .F. ) ;
#24852 = ORIENTED_EDGE ( 'NONE', *, *, #42564, .T. ) ;
#24854 = CARTESIAN_POINT ( 'NONE',  ( 9.999999999999998224, 0.000000000000000000, -45.87500000409677625 ) ) ;
#24855 = CARTESIAN_POINT ( 'NONE',  ( 10.81189881249999907, 6.242252689847868297, -161.7187500020483810 ) ) ;
#24856 = CARTESIAN_POINT ( 'NONE',  ( -2.293366432827344421E-15, -12.48450537969573659, -189.4062500020484094 ) ) ;
#24857 = CARTESIAN_POINT ( 'NONE',  ( -10.81189881249999729, 1.324075727343319199E-15, -6.593750002048370362 ) ) ;
#24858 = EDGE_CURVE ( 'NONE', #32685, #7196, #13901, .T. ) ;
#24859 = CARTESIAN_POINT ( 'NONE',  ( -10.81189881249999729, 1.324075727343319199E-15, -152.0937500020483810 ) ) ;
#24860 =( BOUNDED_CURVE ( )  B_SPLINE_CURVE ( 2, ( #2354, #38589, #15481, #11824, #37955, #25024, #31495 ),
 .UNSPECIFIED., .F., .F. ) 
 B_SPLINE_CURVE_WITH_KNOTS ( ( 3, 2, 2, 3 ),
 ( 0.5634328358208957610, 0.5646766169154231463, 0.5659203980099504205, 0.5671641791044778058 ),
 .UNSPECIFIED. ) 
 CURVE ( )  GEOMETRIC_REPRESENTATION_ITEM ( )  RATIONAL_B_SPLINE_CURVE ( ( 0.9999999999999761302, 0.8660254037844625774, 1.000000000000000000, 0.8660254037844387076, 1.000000000000000000, 0.8660254037844148378, 1.000000000000023981 ) ) 
 REPRESENTATION_ITEM ( '' )  );
#24861 = ADVANCED_FACE ( 'NONE', ( #24299 ), #17356, .F. ) ;
#24862 = CARTESIAN_POINT ( 'NONE',  ( -2.293366432827344421E-15, -12.48450537969573659, -102.4062500020483952 ) ) ;
#24863 = CARTESIAN_POINT ( 'NONE',  ( -5.405949406249996869, 9.363379034771805109, -107.3437500020483810 ) ) ;
#24864 = CARTESIAN_POINT ( 'NONE',  ( -10.00000000000102496, 5.773502691895664007, -55.37499999999994316 ) ) ;
#24865 = CARTESIAN_POINT ( 'NONE',  ( 10.81189881249999729, 0.000000000000000000, -117.0312500020483952 ) ) ;
#24866 = CARTESIAN_POINT ( 'NONE',  ( -2.293366432827344421E-15, -12.48450537969573659, -3.218750002048363257 ) ) ;
#24867 = CARTESIAN_POINT ( 'NONE',  ( 5.405949406249999534, 9.363379034771803333, -127.0937500020483668 ) ) ;
#24868 = CARTESIAN_POINT ( 'NONE',  ( -2.293366432827344421E-15, -12.48450537969573659, -198.4062500020484094 ) ) ;
#24869 = LINE ( 'NONE', #1774, #37148 ) ;
#24870 = CARTESIAN_POINT ( 'NONE',  ( 5.000000000000000000, 8.660254037844385522, -147.2500000000000000 ) ) ;
#24871 = CARTESIAN_POINT ( 'NONE',  ( -9.999999999999998224, 1.224646799147353059E-15, -11.74999999999995559 ) ) ;
#24872 = CARTESIAN_POINT ( 'NONE',  ( 5.405949406249992428, -9.363379034771808662, -75.09375000204838102 ) ) ;
#24873 = CARTESIAN_POINT ( 'NONE',  ( -5.405949406249996869, 9.363379034771805109, -59.34375000204835970 ) ) ;
#24874 = CARTESIAN_POINT ( 'NONE',  ( -10.00000000000000000, -5.773502691896251982, -186.0000000040967905 ) ) ;
#24875 = CARTESIAN_POINT ( 'NONE',  ( 7.644554776091147741E-16, 12.48450537969573659, -31.15625000204835260 ) ) ;
#24876 = CARTESIAN_POINT ( 'NONE',  ( -10.81189881249999907, -6.242252689847864744, -34.96875000204835260 ) ) ;
#24877 = CARTESIAN_POINT ( 'NONE',  ( -9.999999999999479527, -5.773502691896549521, -108.0000000040967478 ) ) ;
#24878 = CARTESIAN_POINT ( 'NONE',  ( 7.644554776091147741E-16, 12.48450537969573659, -143.4687500020483810 ) ) ;
#24879 = CARTESIAN_POINT ( 'NONE',  ( 4.999999999999992006, -8.660254037844389075, -119.2500000000000000 ) ) ;
#24880 = CYLINDRICAL_SURFACE ( 'NONE', #36889, 60.00000000000000711 ) ;
#24881 = CARTESIAN_POINT ( 'NONE',  ( -9.999999999999998224, 5.773502691896259087, -71.87500000000000000 ) ) ;
#24882 = CARTESIAN_POINT ( 'NONE',  ( 7.644554776091147741E-16, 12.48450537969573659, -140.6562500020484094 ) ) ;
#24883 = CARTESIAN_POINT ( 'NONE',  ( 5.405949406249992428, -9.363379034771808662, -7.781250002048350822 ) ) ;
#24884 = ORIENTED_EDGE ( 'NONE', *, *, #1916, .T. ) ;
#24885 = CARTESIAN_POINT ( 'NONE',  ( 10.81189881249999551, -6.242252689847874514, -103.6562500020483810 ) ) ;
#24886 = CARTESIAN_POINT ( 'NONE',  ( -9.999999999999998224, 5.773502691896259087, -124.7500000040967763 ) ) ;
#24887 = CARTESIAN_POINT ( 'NONE',  ( 9.999999999999998224, 0.000000000000000000, -156.8750000040967905 ) ) ;
#24888 = CARTESIAN_POINT ( 'NONE',  ( 10.81189881249999907, 6.242252689847868297, -76.21875000204836681 ) ) ;
#24889 = AXIS2_PLACEMENT_3D ( 'NONE', #29079, #32533, #42006 ) ;
#24890 = CARTESIAN_POINT ( 'NONE',  ( 10.00000000000000000, 5.773502691896255534, -26.25000000409677270 ) ) ;
#24891 = CARTESIAN_POINT ( 'NONE',  ( 4.999999999999992006, -8.660254037844389075, -14.24999999999995737 ) ) ;
#24892 = CARTESIAN_POINT ( 'NONE',  ( 10.81189881249999729, 0.000000000000000000, -46.53125000204838813 ) ) ;
#24893 = CARTESIAN_POINT ( 'NONE',  ( 11.54700538379253416, -19.99999999999999289, 45.00000000000009237 ) ) ;
#24894 = CARTESIAN_POINT ( 'NONE',  ( -10.81189881249999729, 6.242252689847871849, -147.9062500020483810 ) ) ;
#24895 = CARTESIAN_POINT ( 'NONE',  ( 10.81189881249999907, 6.242252689847868297, -128.7187500020483810 ) ) ;
#24896 = CARTESIAN_POINT ( 'NONE',  ( -9.999999999999998224, 1.224646799147353059E-15, -50.74999999999996447 ) ) ;
#24897 = CARTESIAN_POINT ( 'NONE',  ( -9.999999999999998224, 1.224646799147353059E-15, -127.6250000040967620 ) ) ;
#24898 = ORIENTED_EDGE ( 'NONE', *, *, #11302, .T. ) ;
#24899 = ORIENTED_EDGE ( 'NONE', *, *, #9783, .F. ) ;
#24900 = ORIENTED_EDGE ( 'NONE', *, *, #6705, .T. ) ;
#24901 = VECTOR ( 'NONE', #24245, 1000.000000000000000 ) ;
#24902 = CARTESIAN_POINT ( 'NONE',  ( -4.999999999999996447, 8.660254037844387298, -103.5000000000000000 ) ) ;
#24903 =( BOUNDED_CURVE ( )  B_SPLINE_CURVE ( 2, ( #5989, #12436, #12230, #31691, #32115, #2751, #19140 ),
 .UNSPECIFIED., .F., .F. ) 
 B_SPLINE_CURVE_WITH_KNOTS ( ( 3, 2, 2, 3 ),
 ( 0.09328358208955218889, 0.09452736318407958804, 0.09577114427860700108, 0.09701492537313441411 ),
 .UNSPECIFIED. ) 
 CURVE ( )  GEOMETRIC_REPRESENTATION_ITEM ( )  RATIONAL_B_SPLINE_CURVE ( ( 1.000000000000005995, 0.8660254037844327124, 1.000000000000000000, 0.8660254037844387076, 1.000000000000000000, 0.8660254037844297148, 1.000000000000008882 ) ) 
 REPRESENTATION_ITEM ( '' )  );
#24904 = CARTESIAN_POINT ( 'NONE',  ( 5.405949406249992428, -9.363379034771808662, -181.5937500020483810 ) ) ;
#24905 = LOCAL_TIME ( 11, 57, 6.000000000000000000, #31540 ) ;
#24906 = CARTESIAN_POINT ( 'NONE',  ( -10.81189881249999907, -6.242252689847864744, -28.96875000204835615 ) ) ;
#24907 = CARTESIAN_POINT ( 'NONE',  ( 0.000000000000000000, 0.000000000000000000, -200.0000000000000000 ) ) ;
#24908 = EDGE_CURVE ( 'NONE', #41855, #32122, #7751, .T. ) ;
#24909 = CARTESIAN_POINT ( 'NONE',  ( 7.644554776091147741E-16, 12.48450537969573659, -171.9687500020483810 ) ) ;
#24910 = CARTESIAN_POINT ( 'NONE',  ( 10.81189881249999551, -6.242252689847874514, -152.9687500020484094 ) ) ;
#24911 = CARTESIAN_POINT ( 'NONE',  ( 9.999999999999998224, 0.000000000000000000, -75.87500000409677625 ) ) ;
#24912 = CARTESIAN_POINT ( 'NONE',  ( -5.405949406250003975, -9.363379034771801557, -130.8437500020484094 ) ) ;
#24913 = CARTESIAN_POINT ( 'NONE',  ( -5.405949406249996869, 9.363379034771805109, -143.5312500020483810 ) ) ;
#24915 = EDGE_CURVE ( 'NONE', #41753, #17257, #38890, .T. ) ;
#24914 = CARTESIAN_POINT ( 'NONE',  ( -10.81189881249999729, 6.242252689847871849, -156.7187500020483810 ) ) ;
#24916 = CARTESIAN_POINT ( 'NONE',  ( 9.999999999999998224, 0.000000000000000000, -135.5000000000000000 ) ) ;
#24917 =( BOUNDED_CURVE ( )  B_SPLINE_CURVE ( 2, ( #5181, #18335, #31524, #14439, #10785, #37552, #23975 ),
 .UNSPECIFIED., .F., .F. ) 
 B_SPLINE_CURVE_WITH_KNOTS ( ( 3, 2, 2, 3 ),
 ( 0.5373134328358210032, 0.5385572139303483885, 0.5398009950248757738, 0.5410447761194030480 ),
 .UNSPECIFIED. ) 
 CURVE ( )  GEOMETRIC_REPRESENTATION_ITEM ( )  RATIONAL_B_SPLINE_CURVE ( ( 0.9999999999999880096, 0.8660254037844506980, 1.000000000000000000, 0.8660254037844387076, 1.000000000000000000, 0.8660254037844267172, 1.000000000000011990 ) ) 
 REPRESENTATION_ITEM ( '' )  );
#24918 = CARTESIAN_POINT ( 'NONE',  ( 10.00000000000000000, 5.773502691896255534, -171.3750000000000000 ) ) ;
#24919 = EDGE_CURVE ( 'NONE', #28187, #17582, #27306, .T. ) ;
#24920 = CARTESIAN_POINT ( 'NONE',  ( 5.405949406249999534, 9.363379034771803333, -79.09375000204838102 ) ) ;
#24921 = CARTESIAN_POINT ( 'NONE',  ( 7.070501591499376803E-16, 11.54700538379251284, -180.5000000040967905 ) ) ;
#24922 = CARTESIAN_POINT ( 'NONE',  ( -10.81189881249999729, 1.324075727343319199E-15, -59.28125000204836681 ) ) ;
#24923 = CARTESIAN_POINT ( 'NONE',  ( -5.000000000000003553, -8.660254037844383745, -149.5000000000000000 ) ) ;
#24924 = CARTESIAN_POINT ( 'NONE',  ( 10.81189881249999551, -6.242252689847874514, -172.4687500020484094 ) ) ;
#24925 = CARTESIAN_POINT ( 'NONE',  ( -10.81189881249999729, 1.324075727343319199E-15, -116.2812500020483952 ) ) ;
#24926 = CARTESIAN_POINT ( 'NONE',  ( -10.81189881249999729, -6.242252689847864744, -155.1562500020484663 ) ) ;
#24927 = CC_DESIGN_DATE_AND_TIME_ASSIGNMENT ( #29235, #16249, ( #20040 ) ) ;
#24928 = FACE_OUTER_BOUND ( 'NONE', #35141, .T. ) ;
#24929 = CARTESIAN_POINT ( 'NONE',  ( 10.81189881249999729, 0.000000000000000000, -43.53125000204838102 ) ) ;
#24930 = CARTESIAN_POINT ( 'NONE',  ( -10.00000000000000000, -5.773502691896251982, -118.5000000040967905 ) ) ;
#24931 = CARTESIAN_POINT ( 'NONE',  ( -9.999999999999998224, 1.224646799147353059E-15, -97.24999999999998579 ) ) ;
#24932 = VERTEX_POINT ( 'NONE', #355 ) ;
#24933 = CARTESIAN_POINT ( 'NONE',  ( 10.81189881249999729, 6.242252689847867408, -124.4062500020483810 ) ) ;
#24934 = CARTESIAN_POINT ( 'NONE',  ( -9.999999999999998224, 5.773502691896259087, -150.2500000040968189 ) ) ;
#24935 = CARTESIAN_POINT ( 'NONE',  ( -9.999999999999998224, 1.224646799147353059E-15, -167.7500000000000000 ) ) ;
#24936 = CARTESIAN_POINT ( 'NONE',  ( 10.81189881249999551, -6.242252689847874514, -177.1562500020484094 ) ) ;
#24937 = EDGE_LOOP ( 'NONE', ( #10029, #40232, #6589, #19617, #16355, #39623 ) ) ;
#24938 = CARTESIAN_POINT ( 'NONE',  ( 10.81189881249999551, -6.242252689847874514, -170.9687500020483810 ) ) ;
#24939 = CARTESIAN_POINT ( 'NONE',  ( -9.999999999999998224, 1.224646799147353059E-15, -58.62500000409676204 ) ) ;
#24940 = DIRECTION ( 'NONE',  ( -1.000000000000000000, 0.000000000000000000, 0.000000000000000000 ) ) ;
#24941 = LINE ( 'NONE', #34224, #100 ) ;
#24942 = CARTESIAN_POINT ( 'NONE',  ( 10.81189881249999907, 6.242252689847868297, -70.40625000204839523 ) ) ;
#24943 = VECTOR ( 'NONE', #10160, 1000.000000000000000 ) ;
#24944 = CARTESIAN_POINT ( 'NONE',  ( -10.00000000000000000, -5.773502691896251982, -43.50000000409675494 ) ) ;
#24945 = CARTESIAN_POINT ( 'NONE',  ( 10.81189881249999551, -6.242252689847874514, -1.468750002048352377 ) ) ;
#24946 = CARTESIAN_POINT ( 'NONE',  ( -2.121150477449813534E-15, -11.54700538379251284, -148.2500000040968189 ) ) ;
#24947 = CARTESIAN_POINT ( 'NONE',  ( -5.405949406250003975, -9.363379034771801557, -167.0312500020484094 ) ) ;
#24948 = PRODUCT_DEFINITION_FORMATION_WITH_SPECIFIED_SOURCE ( 'ANY', '', #1498, .NOT_KNOWN. ) ;
#24949 = CARTESIAN_POINT ( 'NONE',  ( -4.999999999999996447, 8.660254037844387298, -198.0000000000000000 ) ) ;
#24950 = ORIENTED_EDGE ( 'NONE', *, *, #15533, .T. ) ;
#24951 = CYLINDRICAL_SURFACE ( 'NONE', #4967, 9.999999999999998224 ) ;
#24952 = FACE_OUTER_BOUND ( 'NONE', #25489, .T. ) ;
#24953 = CARTESIAN_POINT ( 'NONE',  ( 9.999999999999998224, 0.000000000000000000, -195.8750000040967905 ) ) ;
#24954 = VECTOR ( 'NONE', #13392, 1000.000000000000000 ) ;
#24956 = ORIENTED_EDGE ( 'NONE', *, *, #3752, .T. ) ;
#24955 = CARTESIAN_POINT ( 'NONE',  ( -10.81189881249999907, -6.242252689847864744, -74.15625000204835260 ) ) ;
#24957 = DIRECTION ( 'NONE',  ( 0.000000000000000000, 0.000000000000000000, 1.000000000000000000 ) ) ;
#24959 = VERTEX_POINT ( 'NONE', #10887 ) ;
#24958 = CARTESIAN_POINT ( 'NONE',  ( -2.121150477449813534E-15, -11.54700538379251284, -140.3750000000000000 ) ) ;
#24960 = PRODUCT_DEFINITION_SHAPE ( 'NONE', 'NONE',  #15921 ) ;
#24961 = VERTEX_POINT ( 'NONE', #37443 ) ;
#24962 = CARTESIAN_POINT ( 'NONE',  ( -10.81189881249999729, 1.324075727343319199E-15, -36.59375000204836681 ) ) ;
#24963 = CARTESIAN_POINT ( 'NONE',  ( -10.00000000000051337, 5.773502691895962435, -73.75000000409674783 ) ) ;
#24964 = CARTESIAN_POINT ( 'NONE',  ( -2.293366432827344421E-15, -12.48450537969573659, -7.906250002048370362 ) ) ;
#24966 = VERTEX_POINT ( 'NONE', #7886 ) ;
#24965 = CARTESIAN_POINT ( 'NONE',  ( -10.81189881249999729, 1.324075727343319199E-15, -65.09375000204836681 ) ) ;
#24967 = CARTESIAN_POINT ( 'NONE',  ( -9.999999999999998224, 1.224646799147353059E-15, -112.2499999999999858 ) ) ;
#24968 = CARTESIAN_POINT ( 'NONE',  ( 9.999999999999998224, 0.000000000000000000, -36.49999999999997868 ) ) ;
#24969 = CARTESIAN_POINT ( 'NONE',  ( -5.405949406249996869, 9.363379034771805109, -197.3437500020484094 ) ) ;
#24970 = CARTESIAN_POINT ( 'NONE',  ( -10.81189881249999729, 1.324075727343319199E-15, -174.5937500020484094 ) ) ;
#24971 = CARTESIAN_POINT ( 'NONE',  ( 10.81189881249999907, 6.242252689847868297, -154.2187500020483810 ) ) ;
#24972 = VECTOR ( 'NONE', #25837, 1000.000000000000000 ) ;
#24973 = CARTESIAN_POINT ( 'NONE',  ( -5.405949406250003975, -9.363379034771801557, -175.8437500020483810 ) ) ;
#24974 = CARTESIAN_POINT ( 'NONE',  ( 100.0000000000000284, -20.00000000000001066, -160.0000000000000000 ) ) ;
#24975 = CARTESIAN_POINT ( 'NONE',  ( -9.999999999999479527, -5.773502691896549521, -102.0000000040967620 ) ) ;
#24976 = CARTESIAN_POINT ( 'NONE',  ( 4.999999999999992006, -8.660254037844389075, -194.2500000000000000 ) ) ;
#24977 = CARTESIAN_POINT ( 'NONE',  ( 10.81189881249999907, 6.242252689847868297, -103.2187500020483810 ) ) ;
#24978 = DIRECTION ( 'NONE',  ( -0.000000000000000000, -0.000000000000000000, 1.000000000000000000 ) ) ;
#24979 = CARTESIAN_POINT ( 'NONE',  ( 7.644554776091147741E-16, 12.48450537969573659, -82.15625000204838102 ) ) ;
#24980 = CARTESIAN_POINT ( 'NONE',  ( 5.405949406249999534, 9.363379034771803333, -91.09375000204838102 ) ) ;
#24981 = CARTESIAN_POINT ( 'NONE',  ( 7.644554776091147741E-16, 12.48450537969573659, -71.65625000204836681 ) ) ;
#24982 = CARTESIAN_POINT ( 'NONE',  ( -9.999999999999998224, 5.773502691896259087, -153.2500000040967620 ) ) ;
#24983 = CARTESIAN_POINT ( 'NONE',  ( -9.999999999999998224, 1.224646799147353059E-15, -122.7500000000000000 ) ) ;
#24984 = CARTESIAN_POINT ( 'NONE',  ( -5.405949406249996869, 9.363379034771805109, -146.5312500020483810 ) ) ;
#24985 = CARTESIAN_POINT ( 'NONE',  ( -10.81189881249999729, 1.324075727343319199E-15, -162.7812500020484094 ) ) ;
#24986 = CIRCLE ( 'NONE', #6358, 57.00000000000002132 ) ;
#24987 = ADVANCED_FACE ( 'NONE', ( #36800 ), #30130, .F. ) ;
#24988 = CARTESIAN_POINT ( 'NONE',  ( 9.999999999999998224, 0.000000000000000000, -91.99999999999998579 ) ) ;
#24989 = CARTESIAN_POINT ( 'NONE',  ( -5.405949406249996869, 9.363379034771805109, -95.34375000204838102 ) ) ;
#24990 = ORIENTED_EDGE ( 'NONE', *, *, #1993, .F. ) ;
#24991 = CARTESIAN_POINT ( 'NONE',  ( 4.999999999999992006, -8.660254037844389075, -66.74999999999997158 ) ) ;
#24992 = CARTESIAN_POINT ( 'NONE',  ( 10.81189881249999907, 6.242252689847868297, -194.7187500020484094 ) ) ;
#24993 = CARTESIAN_POINT ( 'NONE',  ( 4.999999999999992006, -8.660254037844389075, -83.62500000409677625 ) ) ;
#24994 =( BOUNDED_CURVE ( )  B_SPLINE_CURVE ( 2, ( #4320, #17458, #30656, #14211, #37332, #18755, #5601 ),
 .UNSPECIFIED., .F., .F. ) 
 B_SPLINE_CURVE_WITH_KNOTS ( ( 3, 2, 2, 3 ),
 ( 0.2014925373134328901, 0.2027363184079602476, 0.2039800995024875774, 0.2052238805970149627 ),
 .UNSPECIFIED. ) 
 CURVE ( )  GEOMETRIC_REPRESENTATION_ITEM ( )  RATIONAL_B_SPLINE_CURVE ( ( 0.9999999999999940048, 0.8660254037844447028, 1.000000000000000000, 0.8660254037844387076, 1.000000000000000000, 0.8660254037844357100, 1.000000000000002887 ) ) 
 REPRESENTATION_ITEM ( '' )  );
#24995 = CARTESIAN_POINT ( 'NONE',  ( 0.4008866336925647755, -10.45073322229274915, -180.0000000000001421 ) ) ;
#24996 = CARTESIAN_POINT ( 'NONE',  ( -9.999999999999998224, 1.224646799147353059E-15, -108.1250000040967763 ) ) ;
#24997 = CARTESIAN_POINT ( 'NONE',  ( 5.405949406249992428, -9.363379034771808662, -90.28125000204838102 ) ) ;
#24998 = CARTESIAN_POINT ( 'NONE',  ( 10.81189881249999729, 6.242252689847867408, -73.40625000204838102 ) ) ;
#24999 = CARTESIAN_POINT ( 'NONE',  ( -9.999999999999998224, 5.773502691896259087, -70.75000000409677625 ) ) ;
#25000 = DIRECTION ( 'NONE',  ( -0.000000000000000000, -0.000000000000000000, 1.000000000000000000 ) ) ;
#25001 = CARTESIAN_POINT ( 'NONE',  ( 5.405949406249992428, -9.363379034771808662, -30.09375000204836326 ) ) ;
#25002 = EDGE_LOOP ( 'NONE', ( #37614, #6828, #19556, #41103 ) ) ;
#25003 = CARTESIAN_POINT ( 'NONE',  ( 7.644554776091147741E-16, 12.48450537969573659, -190.1562500020484094 ) ) ;
#25004 = CARTESIAN_POINT ( 'NONE',  ( 10.81189881249999729, 0.000000000000000000, -21.03125000204836326 ) ) ;
#25005 = CARTESIAN_POINT ( 'NONE',  ( -10.81189881249999729, -6.242252689847864744, -7.968750002048352599 ) ) ;
#25006 = CARTESIAN_POINT ( 'NONE',  ( 9.999999999999998224, 0.000000000000000000, -122.0000000000000000 ) ) ;
#25007 = CARTESIAN_POINT ( 'NONE',  ( 10.81189881249999907, 6.242252689847868297, -146.7187500020484094 ) ) ;
#25008 = CARTESIAN_POINT ( 'NONE',  ( 7.070501591499376803E-16, 11.54700538379251284, -133.6250000000000000 ) ) ;
#25009 = AXIS2_PLACEMENT_3D ( 'NONE', #4148, #17292, #27029 ) ;
#25010 = CARTESIAN_POINT ( 'NONE',  ( 5.000000000000000000, 8.660254037844385522, -180.2500000000000284 ) ) ;
#25011 = CARTESIAN_POINT ( 'NONE',  ( -4.999999999999996447, 8.660254037844387298, -106.4999999999999858 ) ) ;
#25013 = ORIENTED_EDGE ( 'NONE', *, *, #37146, .T. ) ;
#25012 = CARTESIAN_POINT ( 'NONE',  ( 10.81189881249999729, 0.000000000000000000, -103.5312500020483810 ) ) ;
#25014 = CARTESIAN_POINT ( 'NONE',  ( 9.999999999999742428, 5.773502691896404748, -138.7500000040967905 ) ) ;
#25015 = ORIENTED_EDGE ( 'NONE', *, *, #21578, .F. ) ;
#25016 = ORIENTED_EDGE ( 'NONE', *, *, #12166, .T. ) ;
#25017 = CARTESIAN_POINT ( 'NONE',  ( 5.405949406249992428, -9.363379034771808662, -39.28125000204838102 ) ) ;
#25018 = CALENDAR_DATE ( 2026, 28, 9 ) ;
#25019 = CARTESIAN_POINT ( 'NONE',  ( 10.81189881249999907, 6.242252689847868297, -88.21875000204838102 ) ) ;
#25020 = CARTESIAN_POINT ( 'NONE',  ( 9.999999999999998224, 0.000000000000000000, -156.5000000000000000 ) ) ;
#25021 = CARTESIAN_POINT ( 'NONE',  ( 9.057408897214770604, 5.192877711771748395, -100.0000000000000000 ) ) ;
#25022 = CARTESIAN_POINT ( 'NONE',  ( -9.999999999999996447, 5.773502691896259975, -169.7500000040967905 ) ) ;
#25023 = CARTESIAN_POINT ( 'NONE',  ( 10.81189881249999551, -6.242252689847874514, -162.1562500020484379 ) ) ;
#25024 = CARTESIAN_POINT ( 'NONE',  ( 10.00000000000102318, -5.773502691895667560, -86.12499999999992895 ) ) ;
#25025 = CARTESIAN_POINT ( 'NONE',  ( 5.405949406249992428, -9.363379034771808662, -115.5937500020483810 ) ) ;
#25026 = CARTESIAN_POINT ( 'NONE',  ( 5.405949406249999534, 9.363379034771803333, -83.59375000204836681 ) ) ;
#25027 = CARTESIAN_POINT ( 'NONE',  ( -10.81189881249999729, -6.242252689847864744, -2.156250002048374359 ) ) ;
#25028 = CARTESIAN_POINT ( 'NONE',  ( -10.81189881249999907, -6.242252689847864744, -196.9687500020484379 ) ) ;
#25029 = CARTESIAN_POINT ( 'NONE',  ( -2.293366432827344421E-15, -12.48450537969573659, -96.40625000204839523 ) ) ;
#25030 = CARTESIAN_POINT ( 'NONE',  ( -2.121150477449813534E-15, -11.54700538379251284, -175.2500000040968189 ) ) ;
#25031 = CARTESIAN_POINT ( 'NONE',  ( 7.644554776091147741E-16, 12.48450537969573659, -172.1562500020484094 ) ) ;
#25032 =( BOUNDED_CURVE ( )  B_SPLINE_CURVE ( 2, ( #15622, #19090, #34876, #25166, #32274, #35720, #5299 ),
 .UNSPECIFIED., .F., .F. ) 
 B_SPLINE_CURVE_WITH_KNOTS ( ( 3, 2, 2, 3 ),
 ( 0.8432835820895525636, 0.8445273631840799489, 0.8457711442786073341, 0.8470149253731346084 ),
 .UNSPECIFIED. ) 
 CURVE ( )  GEOMETRIC_REPRESENTATION_ITEM ( )  RATIONAL_B_SPLINE_CURVE ( ( 0.9999999999999641398, 0.8660254037844745678, 1.000000000000000000, 0.8660254037844387076, 1.000000000000000000, 0.8660254037844028474, 1.000000000000035971 ) ) 
 REPRESENTATION_ITEM ( '' )  );
#25033 = CARTESIAN_POINT ( 'NONE',  ( 9.999999999999998224, 0.000000000000000000, -69.49999999999997158 ) ) ;
#25034 = CARTESIAN_POINT ( 'NONE',  ( 5.405949406249992428, -9.363379034771808662, -177.2812500020484094 ) ) ;
#25035 = CARTESIAN_POINT ( 'NONE',  ( 10.81189881249999907, 6.242252689847868297, -185.9062500020484094 ) ) ;
#25036 = CARTESIAN_POINT ( 'NONE',  ( -10.81189881249999729, -6.242252689847864744, -42.46875000204835260 ) ) ;
#25037 = CARTESIAN_POINT ( 'NONE',  ( -5.000000000000003553, -8.660254037844383745, -167.8750000040967905 ) ) ;
#25038 = CARTESIAN_POINT ( 'NONE',  ( -5.405949406250003975, -9.363379034771801557, -2.031250002048373915 ) ) ;
#25039 = CARTESIAN_POINT ( 'NONE',  ( 10.81189881249999907, 6.242252689847868297, -14.71875000204836326 ) ) ;
#25040 = CARTESIAN_POINT ( 'NONE',  ( -2.121150477449813534E-15, -11.54700538379251284, -164.7500000040968189 ) ) ;
#25041 = CARTESIAN_POINT ( 'NONE',  ( 10.81189881249999729, 0.000000000000000000, -122.8437500020483952 ) ) ;
#25042 = CARTESIAN_POINT ( 'NONE',  ( 4.999999999999992006, -8.660254037844389075, -86.24999999999998579 ) ) ;
#25043 = CARTESIAN_POINT ( 'NONE',  ( 5.405949406249999534, 9.363379034771803333, -19.28125000204835970 ) ) ;
#25044 = CARTESIAN_POINT ( 'NONE',  ( 9.999999999999998224, 0.000000000000000000, -107.3750000040967763 ) ) ;
#25045 = CARTESIAN_POINT ( 'NONE',  ( 11.54700538379253416, -19.99999999999999289, 0.000000000000000000 ) ) ;
#25046 = CARTESIAN_POINT ( 'NONE',  ( -10.00000000000000000, -5.773502691896251982, -55.12499999999997868 ) ) ;
#25047 = CARTESIAN_POINT ( 'NONE',  ( -5.405949406249996869, 9.363379034771805109, -116.5312500020483952 ) ) ;
#25048 = CARTESIAN_POINT ( 'NONE',  ( -10.81189881249999729, -6.242252689847864744, -101.1562500020483952 ) ) ;
#25049 = ORIENTED_EDGE ( 'NONE', *, *, #38833, .T. ) ;
#25050 = CARTESIAN_POINT ( 'NONE',  ( -4.999999999999996447, 8.660254037844387298, -90.37500000409677625 ) ) ;
#25051 = CARTESIAN_POINT ( 'NONE',  ( -4.999999999999996447, 8.660254037844387298, -4.499999999999976019 ) ) ;
#25052 = CARTESIAN_POINT ( 'NONE',  ( -10.81189881249999907, -6.242252689847864744, -155.1562500020484094 ) ) ;
#25053 = CARTESIAN_POINT ( 'NONE',  ( -10.81189881249999729, 6.242252689847871849, -48.71875000204836681 ) ) ;
#25054 = ORIENTED_EDGE ( 'NONE', *, *, #21859, .T. ) ;
#25055 = CARTESIAN_POINT ( 'NONE',  ( 9.999999999999996447, -5.773502691896262640, -26.12499999999998224 ) ) ;
#25056 = CARTESIAN_POINT ( 'NONE',  ( -10.81189881249999729, -6.242252689847864744, -29.15625000204835970 ) ) ;
#25057 = CARTESIAN_POINT ( 'NONE',  ( -10.00000000000000000, -5.773502691896251982, -161.6250000000000284 ) ) ;
#25058 = CARTESIAN_POINT ( 'NONE',  ( 5.000000000000000000, 8.660254037844385522, -17.12500000409675138 ) ) ;
#25059 = EDGE_CURVE ( 'NONE', #1756, #33113, #22624, .T. ) ;
#25060 = CARTESIAN_POINT ( 'NONE',  ( 80.00000000000004263, -40.00000000000001421, -160.0000000000000000 ) ) ;
#25061 = CARTESIAN_POINT ( 'NONE',  ( -2.293366432827344421E-15, -12.48450537969573659, -127.9062500020483952 ) ) ;
#25062 = CARTESIAN_POINT ( 'NONE',  ( -3.096741045364464817, 9.605691705790990298, 4.524943085473206850E-15 ) ) ;
#25063 = CARTESIAN_POINT ( 'NONE',  ( -2.121150477449813534E-15, -11.54700538379251284, -44.75000000409676204 ) ) ;
#25064 = ORIENTED_EDGE ( 'NONE', *, *, #37835, .F. ) ;
#25065 = CARTESIAN_POINT ( 'NONE',  ( -5.405949406250003975, -9.363379034771801557, -65.03125000204838102 ) ) ;
#25066 = APPROVAL_DATE_TIME ( #34989, #28088 ) ;
#25067 = CARTESIAN_POINT ( 'NONE',  ( 10.81189881249999729, 0.000000000000000000, -107.8437500020483810 ) ) ;
#25069 = ORIENTED_EDGE ( 'NONE', *, *, #13251, .T. ) ;
#25068 = ORIENTED_EDGE ( 'NONE', *, *, #19874, .F. ) ;
#25070 = CARTESIAN_POINT ( 'NONE',  ( -9.999999999999676703, -5.773502691896437611, -184.1249999999999716 ) ) ;
#25071 = CARTESIAN_POINT ( 'NONE',  ( 10.81189881249999551, -6.242252689847874514, -154.4687500020484094 ) ) ;
#25072 = CARTESIAN_POINT ( 'NONE',  ( 5.405949406249992428, -9.363379034771808662, -190.7812500020484094 ) ) ;
#25073 = CARTESIAN_POINT ( 'NONE',  ( -10.81189881249999729, 1.324075727343319199E-15, -11.09375000204834727 ) ) ;
#25074 = CARTESIAN_POINT ( 'NONE',  ( 10.81189881249999729, 0.000000000000000000, -140.8437500020483810 ) ) ;
#25075 = CARTESIAN_POINT ( 'NONE',  ( 10.81189881249999551, -6.242252689847874514, -97.65625000204839523 ) ) ;
#25076 = CARTESIAN_POINT ( 'NONE',  ( 10.81189881249999551, -6.242252689847874514, -109.4687500020483810 ) ) ;
#25077 = CARTESIAN_POINT ( 'NONE',  ( -4.999999999999996447, 8.660254037844387298, -187.5000000000000000 ) ) ;
#25078 = CARTESIAN_POINT ( 'NONE',  ( -10.81189881249999729, 1.324075727343319199E-15, -116.2812500020483952 ) ) ;
#25079 = CARTESIAN_POINT ( 'NONE',  ( -10.81189881249999907, -6.242252689847864744, -4.968750002048339276 ) ) ;
#25080 = CARTESIAN_POINT ( 'NONE',  ( 10.81189881249999729, 0.000000000000000000, -122.8437500020483952 ) ) ;
#25081 = CARTESIAN_POINT ( 'NONE',  ( -10.81189881249999729, 6.242252689847871849, -191.4062500020484094 ) ) ;
#25082 = CARTESIAN_POINT ( 'NONE',  ( 10.00000000000102318, -5.773502691895667560, -5.500000004096742501 ) ) ;
#25083 = CARTESIAN_POINT ( 'NONE',  ( -9.999999999999998224, 5.773502691896259087, -148.3750000000000000 ) ) ;
#25084 = CARTESIAN_POINT ( 'NONE',  ( -2.121150477449813534E-15, -11.54700538379251284, -14.37499999999997158 ) ) ;
#25085 = CARTESIAN_POINT ( 'NONE',  ( 10.81189881249999729, 6.242252689847867408, -64.21875000204838102 ) ) ;
#25086 = CARTESIAN_POINT ( 'NONE',  ( 7.644554776091147741E-16, 12.48450537969573659, -59.46875000204837391 ) ) ;
#25087 = CARTESIAN_POINT ( 'NONE',  ( -4.999999999999996447, 8.660254037844387298, -186.3750000040967905 ) ) ;
#25088 = CARTESIAN_POINT ( 'NONE',  ( 10.81189881249999729, 0.000000000000000000, -27.03125000204836681 ) ) ;
#25089 = CARTESIAN_POINT ( 'NONE',  ( -5.405949406249996869, 9.363379034771805109, -39.84375000204837391 ) ) ;
#25090 = DIRECTION ( 'NONE',  ( 1.000000000000000000, 0.000000000000000000, 0.000000000000000000 ) ) ;
#25091 = CARTESIAN_POINT ( 'NONE',  ( -10.81189881249999729, 1.324075727343319199E-15, -143.0937500020483810 ) ) ;
#25092 = CARTESIAN_POINT ( 'NONE',  ( 9.999999999999998224, 0.000000000000000000, -119.0000000000000000 ) ) ;
#25093 = CARTESIAN_POINT ( 'NONE',  ( -9.999999999999998224, 1.224646799147353059E-15, -148.2500000000000000 ) ) ;
#25094 = CARTESIAN_POINT ( 'NONE',  ( -9.999999999999998224, 1.224646799147353059E-15, -74.74999999999998579 ) ) ;
#25095 = CARTESIAN_POINT ( 'NONE',  ( 10.81189881249999551, -6.242252689847874514, -141.1562500020484094 ) ) ;
#25096 = CARTESIAN_POINT ( 'NONE',  ( 10.81189881249999729, 0.000000000000000000, -13.53125000204835615 ) ) ;
#25097 = ORIENTED_EDGE ( 'NONE', *, *, #30417, .T. ) ;
#25098 = CARTESIAN_POINT ( 'NONE',  ( 5.405949406249992428, -9.363379034771808662, -100.7812500020483952 ) ) ;
#25099 = CARTESIAN_POINT ( 'NONE',  ( 9.999999999999998224, 0.000000000000000000, -113.3750000040967763 ) ) ;
#25100 = CARTESIAN_POINT ( 'NONE',  ( 10.00000000000025402, -5.773502691896113426, -140.1250000000000000 ) ) ;
#25101 = CARTESIAN_POINT ( 'NONE',  ( 5.405949406249999534, 9.363379034771803333, -77.59375000204838102 ) ) ;
#25102 = CARTESIAN_POINT ( 'NONE',  ( 7.070501591499377789E-16, 11.54700538379251284, -26.00000000409676915 ) ) ;
#25103 = DIRECTION ( 'NONE',  ( 0.000000000000000000, 0.000000000000000000, 1.000000000000000000 ) ) ;
#25104 = CARTESIAN_POINT ( 'NONE',  ( -10.81189881249999729, 1.324075727343319199E-15, -41.28125000204838102 ) ) ;
#25105 = CARTESIAN_POINT ( 'NONE',  ( -2.121150477449813534E-15, -11.54700538379251284, -105.8749999999999858 ) ) ;
#25106 = CARTESIAN_POINT ( 'NONE',  ( 10.81189881249999729, 0.000000000000000000, -148.5312500020483810 ) ) ;
#25107 = CARTESIAN_POINT ( 'NONE',  ( -10.81189881249999907, -6.242252689847864744, -124.9687500020483810 ) ) ;
#25109 = EDGE_CURVE ( 'NONE', #42437, #30972, #27041, .T. ) ;
#25108 = CARTESIAN_POINT ( 'NONE',  ( 7.070501591499376803E-16, 11.54700538379251284, -153.1250000000000000 ) ) ;
#25110 = CARTESIAN_POINT ( 'NONE',  ( 9.999999999999998224, 0.000000000000000000, -57.49999999999996447 ) ) ;
#25111 = ORIENTED_EDGE ( 'NONE', *, *, #29515, .T. ) ;
#25112 = ORIENTED_EDGE ( 'NONE', *, *, #29095, .F. ) ;
#25113 =( REPRESENTATION_RELATIONSHIP ('NONE','NONE', #21658, #10057 ) REPRESENTATION_RELATIONSHIP_WITH_TRANSFORMATION ( #2558 )SHAPE_REPRESENTATION_RELATIONSHIP( ) );
#25114 = VERTEX_POINT ( 'NONE', #34646 ) ;
#25115 =( BOUNDED_CURVE ( )  B_SPLINE_CURVE ( 2, ( #7754, #34301, #17867, #859, #14840, #4718, #18089 ),
 .UNSPECIFIED., .F., .F. ) 
 B_SPLINE_CURVE_WITH_KNOTS ( ( 3, 2, 2, 3 ),
 ( 0.6529850746268659467, 0.6542288557213932210, 0.6554726368159206062, 0.6567164179104479915 ),
 .UNSPECIFIED. ) 
 CURVE ( )  GEOMETRIC_REPRESENTATION_ITEM ( )  RATIONAL_B_SPLINE_CURVE ( ( 0.9999999999999761302, 0.8660254037844625774, 1.000000000000000000, 0.8660254037844387076, 1.000000000000000000, 0.8660254037844148378, 1.000000000000023981 ) ) 
 REPRESENTATION_ITEM ( '' )  );
#25116 = DIRECTION ( 'NONE',  ( -0.000000000000000000, -0.000000000000000000, 1.000000000000000000 ) ) ;
#25117 = CARTESIAN_POINT ( 'NONE',  ( -10.81189881249999729, 1.324075727343319199E-15, -179.0937500020484094 ) ) ;
#25118 = CARTESIAN_POINT ( 'NONE',  ( -10.81189881249999729, 1.324075727343319199E-15, -30.59375000204836326 ) ) ;
#25119 = CARTESIAN_POINT ( 'NONE',  ( 9.999999999999998224, 0.000000000000000000, -200.0000000000000000 ) ) ;
#25120 = CARTESIAN_POINT ( 'NONE',  ( 10.81189881249999729, 6.242252689847867408, -160.2187500020483810 ) ) ;
#25121 = CARTESIAN_POINT ( 'NONE',  ( 10.81189881249999551, -6.242252689847874514, -151.4687500020483810 ) ) ;
#25122 = CARTESIAN_POINT ( 'NONE',  ( -5.405949406249996869, 9.363379034771805109, -135.8437500020484094 ) ) ;
#25123 = CARTESIAN_POINT ( 'NONE',  ( -5.405949406250003975, -9.363379034771801557, -143.0312500020483810 ) ) ;
#25124 = CARTESIAN_POINT ( 'NONE',  ( -2.293366432827344421E-15, -12.48450537969573659, -147.2187500020484094 ) ) ;
#25125 = FACE_OUTER_BOUND ( 'NONE', #33443, .T. ) ;
#25126 = CARTESIAN_POINT ( 'NONE',  ( 9.999999999999998224, 0.000000000000000000, -158.0000000000000000 ) ) ;
#25127 = CARTESIAN_POINT ( 'NONE',  ( 9.999999999999996447, -5.773502691896262640, -174.6250000000000000 ) ) ;
#25128 = CARTESIAN_POINT ( 'NONE',  ( -10.81189881249999729, 6.242252689847871849, -80.21875000204838102 ) ) ;
#25129 = CARTESIAN_POINT ( 'NONE',  ( -9.999999999999998224, 1.224646799147353059E-15, -200.0000000000000000 ) ) ;
#25130 = CARTESIAN_POINT ( 'NONE',  ( -2.293366432827344421E-15, -12.48450537969573659, -49.90625000204838102 ) ) ;
#25131 = CARTESIAN_POINT ( 'NONE',  ( -10.30115550912761968, -1.362735121981329067, -99.99999999999994316 ) ) ;
#25132 = CARTESIAN_POINT ( 'NONE',  ( 5.405949406249999534, 9.363379034771803333, -167.5937500020484094 ) ) ;
#25133 = CARTESIAN_POINT ( 'NONE',  ( -2.293366432827344421E-15, -12.48450537969573659, -112.9062500020483952 ) ) ;
#25134 = CARTESIAN_POINT ( 'NONE',  ( 10.81189881249999729, 0.000000000000000000, -150.0312500020483810 ) ) ;
#25135 = CARTESIAN_POINT ( 'NONE',  ( 0.000000000000000000, 0.000000000000000000, -200.0000000000000000 ) ) ;
#25136 = CARTESIAN_POINT ( 'NONE',  ( 10.81189881249999907, 6.242252689847868297, -43.40625000204836681 ) ) ;
#25137 = CARTESIAN_POINT ( 'NONE',  ( -10.00000000000000000, -5.773502691896251982, -123.0000000040968047 ) ) ;
#25138 = CARTESIAN_POINT ( 'NONE',  ( -2.121150477449813534E-15, -11.54700538379251284, -102.8749999999999858 ) ) ;
#25139 = VERTEX_POINT ( 'NONE', #18220 ) ;
#25140 = CARTESIAN_POINT ( 'NONE',  ( -5.405949406250003975, -9.363379034771801557, -123.5312500020483952 ) ) ;
#25141 = CARTESIAN_POINT ( 'NONE',  ( 5.000000000000000000, 8.660254037844385522, -141.6250000040967905 ) ) ;
#25142 = DIRECTION ( 'NONE',  ( -0.000000000000000000, -0.000000000000000000, 1.000000000000000000 ) ) ;
#25143 = CARTESIAN_POINT ( 'NONE',  ( -10.81189881249999729, 6.242252689847871849, -177.9062500020484094 ) ) ;
#25144 = ORIENTED_EDGE ( 'NONE', *, *, #35571, .T. ) ;
#25145 = CARTESIAN_POINT ( 'NONE',  ( -10.81189881249999729, 1.324075727343319199E-15, -171.5937500020484094 ) ) ;
#25146 = CARTESIAN_POINT ( 'NONE',  ( 5.000000000000000000, 8.660254037844385522, -48.62500000409678336 ) ) ;
#25147 = CARTESIAN_POINT ( 'NONE',  ( -2.121150477449813534E-15, -11.54700538379251284, -155.3750000000000000 ) ) ;
#25148 = CARTESIAN_POINT ( 'NONE',  ( -5.405949406250003975, -9.363379034771801557, -65.03125000204838102 ) ) ;
#25149 = CARTESIAN_POINT ( 'NONE',  ( 7.070501591499377789E-16, 11.54700538379251284, -41.00000000409676204 ) ) ;
#25150 = CARTESIAN_POINT ( 'NONE',  ( 9.999999999999998224, 0.000000000000000000, -147.8750000040967905 ) ) ;
#25151 = CARTESIAN_POINT ( 'NONE',  ( 10.81189881249999729, 0.000000000000000000, -168.0312500020484094 ) ) ;
#25152 = CARTESIAN_POINT ( 'NONE',  ( -4.999999999999996447, 8.660254037844387298, -1.875000004096766260 ) ) ;
#25154 = ADVANCED_FACE ( 'NONE', ( #14543 ), #38295, .T. ) ;
#25153 = CARTESIAN_POINT ( 'NONE',  ( -2.121150477449813534E-15, -11.54700538379251284, -56.37499999999997868 ) ) ;
#25155 = VERTEX_POINT ( 'NONE', #11742 ) ;
#25156 = CARTESIAN_POINT ( 'NONE',  ( 9.999999999999998224, 0.000000000000000000, -161.0000000000000000 ) ) ;
#25157 = EDGE_CURVE ( 'NONE', #26580, #4606, #24941, .T. ) ;
#25158 = ADVANCED_FACE ( 'NONE', ( #37872 ), #34861, .T. ) ;
#25159 = CARTESIAN_POINT ( 'NONE',  ( -9.999999999999998224, 1.224646799147353059E-15, -176.7500000000000284 ) ) ;
#25160 = EDGE_CURVE ( 'NONE', #7201, #41736, #38016, .T. ) ;
#25161 =( BOUNDED_CURVE ( )  B_SPLINE_CURVE ( 2, ( #42217, #26261, #29496, #6613, #7045, #19979, #33168 ),
 .UNSPECIFIED., .F., .F. ) 
 B_SPLINE_CURVE_WITH_KNOTS ( ( 3, 2, 2, 3 ),
 ( 0.4179104477611941260, 0.4191542288557215112, 0.4203980099502488965, 0.4216417910447762818 ),
 .UNSPECIFIED. ) 
 CURVE ( )  GEOMETRIC_REPRESENTATION_ITEM ( )  RATIONAL_B_SPLINE_CURVE ( ( 0.9999999999999880096, 0.8660254037844506980, 1.000000000000000000, 0.8660254037844387076, 1.000000000000000000, 0.8660254037844207220, 1.000000000000017986 ) ) 
 REPRESENTATION_ITEM ( '' )  );
#25162 = LINE ( 'NONE', #16997, #22071 ) ;
#25164 = ORIENTED_EDGE ( 'NONE', *, *, #2444, .F. ) ;
#25163 = CARTESIAN_POINT ( 'NONE',  ( -10.81189881249999729, 6.242252689847871849, -75.90625000204838102 ) ) ;
#25165 =( NAMED_UNIT ( * ) SI_UNIT ( $, .STERADIAN. ) SOLID_ANGLE_UNIT ( ) );
#25167 = ORIENTED_EDGE ( 'NONE', *, *, #4816, .T. ) ;
#25166 = CARTESIAN_POINT ( 'NONE',  ( 7.070501591499376803E-16, 11.54700538379251284, -30.12499999999995026 ) ) ;
#25168 = CC_DESIGN_DATE_AND_TIME_ASSIGNMENT ( #5572, #20623, ( #27695 ) ) ;
#25169 = ORIENTED_EDGE ( 'NONE', *, *, #12999, .F. ) ;
#25170 = CARTESIAN_POINT ( 'NONE',  ( -5.405949406249996869, 9.363379034771805109, -26.34375000204835970 ) ) ;
#25171 = CYLINDRICAL_SURFACE ( 'NONE', #2489, 9.999999999999998224 ) ;
#25172 = CARTESIAN_POINT ( 'NONE',  ( 10.81189881249999907, 6.242252689847868297, -7.406250002048366810 ) ) ;
#25173 =( BOUNDED_CURVE ( )  B_SPLINE_CURVE ( 2, ( #17042, #20077, #30242, #16826, #16397, #13163, #30025 ),
 .UNSPECIFIED., .F., .F. ) 
 B_SPLINE_CURVE_WITH_KNOTS ( ( 3, 2, 2, 3 ),
 ( 0.4589552238805971740, 0.4601990049751245593, 0.4614427860696518890, 0.4626865671641792743 ),
 .UNSPECIFIED. ) 
 CURVE ( )  GEOMETRIC_REPRESENTATION_ITEM ( )  RATIONAL_B_SPLINE_CURVE ( ( 0.9999999999999820144, 0.8660254037844566932, 1.000000000000000000, 0.8660254037844387076, 1.000000000000000000, 0.8660254037844207220, 1.000000000000017986 ) ) 
 REPRESENTATION_ITEM ( '' )  );
#25175 = ORIENTED_EDGE ( 'NONE', *, *, #13341, .T. ) ;
#25174 = CARTESIAN_POINT ( 'NONE',  ( -5.405949406250003975, -9.363379034771801557, -54.34375000204835970 ) ) ;
#25176 = CARTESIAN_POINT ( 'NONE',  ( 0.000000000000000000, 0.000000000000000000, -200.0000000000000000 ) ) ;
#25177 = CARTESIAN_POINT ( 'NONE',  ( 5.000000000000000000, 8.660254037844385522, -39.24999999999997868 ) ) ;
#25178 = ADVANCED_FACE ( 'NONE', ( #18649 ), #5073, .T. ) ;
#25179 = CARTESIAN_POINT ( 'NONE',  ( -10.81189881249999729, 1.324075727343319199E-15, -194.0937500020484094 ) ) ;
#25180 = CARTESIAN_POINT ( 'NONE',  ( -5.405949406249996869, 9.363379034771805109, -179.3437500020483810 ) ) ;
#25181 = CARTESIAN_POINT ( 'NONE',  ( 5.405949406249992428, -9.363379034771808662, -160.5937500020484094 ) ) ;
#25182 = CARTESIAN_POINT ( 'NONE',  ( 7.644554776091147741E-16, 12.48450537969573659, -170.4687500020483810 ) ) ;
#25183 = CARTESIAN_POINT ( 'NONE',  ( -9.999999999999998224, 1.224646799147353059E-15, -200.0000000000000000 ) ) ;
#25184 = LINE ( 'NONE', #38325, #31589 ) ;
#25185 = ADVANCED_FACE ( 'NONE', ( #41527 ), #15189, .T. ) ;
#25186 = CARTESIAN_POINT ( 'NONE',  ( 10.00000000000000000, 5.773502691896255534, -196.8750000000000284 ) ) ;
#25187 = CARTESIAN_POINT ( 'NONE',  ( -5.405949406249996869, 9.363379034771805109, -102.8437500020483810 ) ) ;
#25188 = CARTESIAN_POINT ( 'NONE',  ( 5.405949406249992428, -9.363379034771808662, -79.78125000204838102 ) ) ;
#25189 = CARTESIAN_POINT ( 'NONE',  ( -10.81189881249999729, 1.324075727343319199E-15, -89.09375000204838102 ) ) ;
#25190 = EDGE_CURVE ( 'NONE', #34698, #33370, #25412, .T. ) ;
#25191 = CARTESIAN_POINT ( 'NONE',  ( 5.405949406249992428, -9.363379034771808662, -64.78125000204838102 ) ) ;
#25192 = CARTESIAN_POINT ( 'NONE',  ( 9.999999999999996447, -5.773502691896262640, -143.5000000040967905 ) ) ;
#25193 = CARTESIAN_POINT ( 'NONE',  ( 5.000000000000000000, 8.660254037844385522, -120.2500000000000000 ) ) ;
#25194 = EDGE_LOOP ( 'NONE', ( #20127, #23563, #9072, #22127 ) ) ;
#25195 = CARTESIAN_POINT ( 'NONE',  ( -2.293366432827344421E-15, -12.48450537969573659, -153.4062500020483810 ) ) ;
#25196 = CARTESIAN_POINT ( 'NONE',  ( 10.81189881249999729, 0.000000000000000000, -165.0312500020484094 ) ) ;
#25197 = CARTESIAN_POINT ( 'NONE',  ( -25.00000000000000000, 0.000000000000000000, -170.0000000000000000 ) ) ;
#25198 = CARTESIAN_POINT ( 'NONE',  ( 9.999999999999998224, 0.000000000000000000, -37.99999999999997868 ) ) ;
#25199 = CARTESIAN_POINT ( 'NONE',  ( -10.81189881249999729, 1.324075727343319199E-15, -96.59375000204838102 ) ) ;
#25200 = VERTEX_POINT ( 'NONE', #31843 ) ;
#25201 = CARTESIAN_POINT ( 'NONE',  ( 10.00000000000000000, 5.773502691896255534, -67.87500000000000000 ) ) ;
#25202 = CARTESIAN_POINT ( 'NONE',  ( 10.81189881249999729, 0.000000000000000000, -0.03125000204837191653 ) ) ;
#25203 = CARTESIAN_POINT ( 'NONE',  ( 4.999999999999992006, -8.660254037844389075, -70.12500000409677625 ) ) ;
#25204 = EDGE_CURVE ( 'NONE', #20043, #6102, #8268, .T. ) ;
#25205 = CARTESIAN_POINT ( 'NONE',  ( -5.000000000000003553, -8.660254037844383745, -142.3750000040967905 ) ) ;
#25206 = CARTESIAN_POINT ( 'NONE',  ( -10.81189881249999729, 1.324075727343319199E-15, -90.78125000204838102 ) ) ;
#25207 = CARTESIAN_POINT ( 'NONE',  ( -10.81189881249999729, 6.242252689847871849, -75.90625000204838102 ) ) ;
#25208 = CARTESIAN_POINT ( 'NONE',  ( 9.999999999999998224, 0.000000000000000000, -69.87500000409677625 ) ) ;
#25209 = CYLINDRICAL_SURFACE ( 'NONE', #13479, 9.999999999999998224 ) ;
#25210 = CARTESIAN_POINT ( 'NONE',  ( 10.81189881249999907, 6.242252689847868297, -29.71875000204834549 ) ) ;
#25211 = VERTEX_POINT ( 'NONE', #41304 ) ;
#25212 = CARTESIAN_POINT ( 'NONE',  ( -10.81189881249999907, -6.242252689847864744, -194.1562500020484094 ) ) ;
#25213 = CARTESIAN_POINT ( 'NONE',  ( -10.81189881249999907, -6.242252689847864744, -17.15625000204837391 ) ) ;
#25214 = CARTESIAN_POINT ( 'NONE',  ( 7.644554776091147741E-16, 12.48450537969573659, -5.468750002048341941 ) ) ;
#25215 = CARTESIAN_POINT ( 'NONE',  ( -9.999999999999998224, 1.224646799147353059E-15, -186.1250000040967905 ) ) ;
#25216 = CARTESIAN_POINT ( 'NONE',  ( 10.81189881249999729, 0.000000000000000000, -145.3437500020483810 ) ) ;
#25217 = CARTESIAN_POINT ( 'NONE',  ( 9.999999999999998224, 0.000000000000000000, 0.6249999959032359609 ) ) ;
#25218 = DIRECTION ( 'NONE',  ( -0.000000000000000000, -0.000000000000000000, 1.000000000000000000 ) ) ;
#25219 = CARTESIAN_POINT ( 'NONE',  ( 4.999999999999992006, -8.660254037844389075, -176.2500000000000284 ) ) ;
#25221 = ORIENTED_EDGE ( 'NONE', *, *, #18057, .F. ) ;
#25220 = CARTESIAN_POINT ( 'NONE',  ( -2.293366432827344421E-15, -12.48450537969573659, -103.9062500020483810 ) ) ;
#25222 = ORIENTED_EDGE ( 'NONE', *, *, #15218, .T. ) ;
#25223 = ORIENTED_EDGE ( 'NONE', *, *, #18562, .F. ) ;
#25224 = CARTESIAN_POINT ( 'NONE',  ( -2.293366432827344421E-15, -12.48450537969573659, -28.90625000204835615 ) ) ;
#25225 = CALENDAR_DATE ( 2026, 28, 9 ) ;
#25226 = CARTESIAN_POINT ( 'NONE',  ( -10.81189881249999907, -6.242252689847864744, -75.46875000204836681 ) ) ;
#25227 = CARTESIAN_POINT ( 'NONE',  ( -1.040834085586084257E-14, -125.0000000000000000, 22.49999999999999289 ) ) ;
#25228 = CYLINDRICAL_SURFACE ( 'NONE', #29374, 9.999999999999998224 ) ;
#25229 = AXIS2_PLACEMENT_3D ( 'NONE', #1543, #4765, #5199 ) ;
#25230 = CIRCLE ( 'NONE', #2490, 20.00000000000000355 ) ;
#25231 = DIRECTION ( 'NONE',  ( 1.000000000000000000, 0.000000000000000000, 0.000000000000000000 ) ) ;
#25232 = CARTESIAN_POINT ( 'NONE',  ( 5.405949406249999534, 9.363379034771803333, -164.7812500020484094 ) ) ;
#25233 = CARTESIAN_POINT ( 'NONE',  ( -2.121150477449813534E-15, -11.54700538379251284, -14.75000000409676737 ) ) ;
#25234 = CARTESIAN_POINT ( 'NONE',  ( -5.000000000000003553, -8.660254037844383745, -172.3750000040968189 ) ) ;
#25235 = CARTESIAN_POINT ( 'NONE',  ( -10.81189881249999729, 1.324075727343319199E-15, -119.0937500020483810 ) ) ;
#25236 = VECTOR ( 'NONE', #30301, 1000.000000000000000 ) ;
#25237 =( BOUNDED_CURVE ( )  B_SPLINE_CURVE ( 2, ( #41697, #35252, #5687, #28779, #15366, #5889, #19046 ),
 .UNSPECIFIED., .F., .F. ) 
 B_SPLINE_CURVE_WITH_KNOTS ( ( 3, 2, 2, 3 ),
 ( 0.4888059701492538101, 0.4900497512437811398, 0.4912935323383085806, 0.4925373134328359104 ),
 .UNSPECIFIED. ) 
 CURVE ( )  GEOMETRIC_REPRESENTATION_ITEM ( )  RATIONAL_B_SPLINE_CURVE ( ( 0.9999999999999940048, 0.8660254037844447028, 1.000000000000000000, 0.8660254037844387076, 1.000000000000000000, 0.8660254037844267172, 1.000000000000011990 ) ) 
 REPRESENTATION_ITEM ( '' )  );
#25238 = CARTESIAN_POINT ( 'NONE',  ( -5.405949406249996869, 9.363379034771805109, -86.34375000204836681 ) ) ;
#25239 = CARTESIAN_POINT ( 'NONE',  ( -10.81189881249999729, 1.324075727343319199E-15, -194.0937500020484094 ) ) ;
#25240 = CARTESIAN_POINT ( 'NONE',  ( 5.405949406249992428, -9.363379034771808662, -96.28125000204838102 ) ) ;
#25241 = CARTESIAN_POINT ( 'NONE',  ( 5.000000000000000000, 8.660254037844385522, -167.1250000040967905 ) ) ;
#25242 = CARTESIAN_POINT ( 'NONE',  ( -10.81189881249999729, -6.242252689847864744, -168.6562500020484094 ) ) ;
#25243 = CARTESIAN_POINT ( 'NONE',  ( 4.999999999999992006, -8.660254037844389075, -150.7500000000000000 ) ) ;
#25244 = CARTESIAN_POINT ( 'NONE',  ( -5.405949406249996869, 9.363379034771805109, -172.0312500020484094 ) ) ;
#25245 = CARTESIAN_POINT ( 'NONE',  ( -10.81189881249999729, 6.242252689847871849, -191.4062500020484094 ) ) ;
#25246 = CARTESIAN_POINT ( 'NONE',  ( 10.81189881249999729, 0.000000000000000000, -41.84375000204837391 ) ) ;
#25247 = CARTESIAN_POINT ( 'NONE',  ( 5.000000000000000000, 8.660254037844385522, -165.6250000040967905 ) ) ;
#25248 = CARTESIAN_POINT ( 'NONE',  ( 5.405949406249999534, 9.363379034771803333, -1.281250002048373027 ) ) ;
#25249 = CARTESIAN_POINT ( 'NONE',  ( 10.81189881249999729, 0.000000000000000000, -11.84375000204834727 ) ) ;
#25250 = CARTESIAN_POINT ( 'NONE',  ( -2.121150477449813534E-15, -11.54700538379251284, -152.7500000040967620 ) ) ;
#25251 = CARTESIAN_POINT ( 'NONE',  ( -2.293366432827344421E-15, -12.48450537969573659, -123.2187500020483952 ) ) ;
#25252 = CARTESIAN_POINT ( 'NONE',  ( 5.000000000000000000, 8.660254037844385522, -88.74999999999998579 ) ) ;
#25253 = CARTESIAN_POINT ( 'NONE',  ( 7.644554776091147741E-16, 12.48450537969573659, -22.15625000204837747 ) ) ;
#25254 = CARTESIAN_POINT ( 'NONE',  ( -10.00000000000000000, -5.773502691896251982, -105.0000000040967763 ) ) ;
#25255 = CARTESIAN_POINT ( 'NONE',  ( 0.000000000000000000, 0.000000000000000000, -99.99999999999998579 ) ) ;
#25256 = CARTESIAN_POINT ( 'NONE',  ( 10.81189881249999729, 0.000000000000000000, -114.0312500020483952 ) ) ;
#25257 = CARTESIAN_POINT ( 'NONE',  ( 10.81189881249999729, 6.242252689847867408, -100.4062500020483952 ) ) ;
#25258 = ORIENTED_EDGE ( 'NONE', *, *, #26241, .F. ) ;
#25259 = CARTESIAN_POINT ( 'NONE',  ( -9.999999999999998224, 5.773502691896259087, -88.75000000409677625 ) ) ;
#25260 = CARTESIAN_POINT ( 'NONE',  ( 9.999999999998456346, 5.773502691897149042, -29.25000000409671941 ) ) ;
#25261 = CARTESIAN_POINT ( 'NONE',  ( 10.81189881249999907, 6.242252689847868297, -160.4062500020484094 ) ) ;
#25262 = CARTESIAN_POINT ( 'NONE',  ( 10.81189881249999551, -6.242252689847874514, -49.46875000204836681 ) ) ;
#25263 = ORIENTED_EDGE ( 'NONE', *, *, #37286, .F. ) ;
#25264 = CARTESIAN_POINT ( 'NONE',  ( -2.121150477449813534E-15, -11.54700538379251284, -20.37499999999996803 ) ) ;
#25265 = CARTESIAN_POINT ( 'NONE',  ( -5.405949406249996869, 9.363379034771805109, -28.03125000204837036 ) ) ;
#25266 = CARTESIAN_POINT ( 'NONE',  ( -5.000000000000003553, -8.660254037844383745, -154.0000000000000000 ) ) ;
#25267 = CARTESIAN_POINT ( 'NONE',  ( 10.00000000000000000, 5.773502691896255534, -20.25000000409676915 ) ) ;
#25268 = VECTOR ( 'NONE', #17602, 1000.000000000000000 ) ;
#25269 = CARTESIAN_POINT ( 'NONE',  ( 4.999999999999992006, -8.660254037844389075, -195.7500000000000000 ) ) ;
#25271 = EDGE_LOOP ( 'NONE', ( #26836, #39595, #33953, #23398 ) ) ;
#25270 = CARTESIAN_POINT ( 'NONE',  ( 10.81189881249999551, -6.242252689847874514, -127.6562500020483952 ) ) ;
#25272 = FACE_OUTER_BOUND ( 'NONE', #22292, .T. ) ;
#25273 = CARTESIAN_POINT ( 'NONE',  ( 9.999999999999479527, 5.773502691896553074, -143.2500000040967905 ) ) ;
#25274 = VERTEX_POINT ( 'NONE', #28170 ) ;
#25275 = CARTESIAN_POINT ( 'NONE',  ( -10.81189881249999729, 1.324075727343319199E-15, -56.28125000204836681 ) ) ;
#25276 = APPROVAL_STATUS ( 'not_yet_approved' ) ;
#25277 = EDGE_CURVE ( 'NONE', #15872, #26632, #40249, .T. ) ;
#25278 = CARTESIAN_POINT ( 'NONE',  ( 5.405949406249992428, -9.363379034771808662, -112.5937500020483810 ) ) ;
#25280 = ORIENTED_EDGE ( 'NONE', *, *, #38356, .F. ) ;
#25279 = ORIENTED_EDGE ( 'NONE', *, *, #3276, .T. ) ;
#25281 = DIRECTION ( 'NONE',  ( -0.000000000000000000, -0.000000000000000000, -1.000000000000000000 ) ) ;
#25282 =( BOUNDED_CURVE ( )  B_SPLINE_CURVE ( 2, ( #25460, #28700, #41827, #22847, #32771, #28907, #5809 ),
 .UNSPECIFIED., .F., .F. ) 
 B_SPLINE_CURVE_WITH_KNOTS ( ( 3, 2, 2, 3 ),
 ( 0.2126865671641791633, 0.2139303482587065208, 0.2151741293532339061, 0.2164179104477612636 ),
 .UNSPECIFIED. ) 
 CURVE ( )  GEOMETRIC_REPRESENTATION_ITEM ( )  RATIONAL_B_SPLINE_CURVE ( ( 0.9999999999999940048, 0.8660254037844447028, 1.000000000000000000, 0.8660254037844387076, 1.000000000000000000, 0.8660254037844297148, 1.000000000000008882 ) ) 
 REPRESENTATION_ITEM ( '' )  );
#25283 = CARTESIAN_POINT ( 'NONE',  ( -10.81189881249999729, 6.242252689847871849, -158.2187500020483810 ) ) ;
#25284 = CARTESIAN_POINT ( 'NONE',  ( -5.405949406250003975, -9.363379034771801557, -189.5312500020484094 ) ) ;
#25285 = CARTESIAN_POINT ( 'NONE',  ( 7.644554776091147741E-16, 12.48450537969573659, -6.968750002048349046 ) ) ;
#25286 = CARTESIAN_POINT ( 'NONE',  ( -5.405949406250003975, -9.363379034771801557, -136.8437500020484094 ) ) ;
#25287 = CARTESIAN_POINT ( 'NONE',  ( -10.81189881249999907, -6.242252689847864744, -106.9687500020483668 ) ) ;
#25288 = CARTESIAN_POINT ( 'NONE',  ( -9.999999999999998224, 1.224646799147353059E-15, -187.2500000000000000 ) ) ;
#25289 = CARTESIAN_POINT ( 'NONE',  ( 10.81189881249999551, -6.242252689847874514, -114.1562500020483952 ) ) ;
#25290 = CARTESIAN_POINT ( 'NONE',  ( 10.81189881249999907, 6.242252689847868297, 0.2812499979516534521 ) ) ;
#25292 = ADVANCED_FACE ( 'NONE', ( #28812 ), #9364, .T. ) ;
#25291 = CARTESIAN_POINT ( 'NONE',  ( 5.405949406249992428, -9.363379034771808662, -123.0937500020483952 ) ) ;
#25293 = CARTESIAN_POINT ( 'NONE',  ( -10.81189881249999729, 1.324075727343319199E-15, -195.7812500020484094 ) ) ;
#25294 = CARTESIAN_POINT ( 'NONE',  ( -2.121150477449813534E-15, -11.54700538379251284, -5.750000004096771811 ) ) ;
#25295 = CARTESIAN_POINT ( 'NONE',  ( -9.999999999999998224, 5.773502691896259087, -143.8750000000000000 ) ) ;
#25296 = CARTESIAN_POINT ( 'NONE',  ( -9.999999999999998224, 1.224646799147353059E-15, -13.24999999999995559 ) ) ;
#25297 = CARTESIAN_POINT ( 'NONE',  ( -10.81189881249999729, -6.242252689847864744, -67.96875000204838102 ) ) ;
#25298 = CARTESIAN_POINT ( 'NONE',  ( 5.405949406249992428, -9.363379034771808662, -60.09375000204835970 ) ) ;
#25299 = CARTESIAN_POINT ( 'NONE',  ( -2.121150477449813534E-15, -11.54700538379251284, -188.7500000040967905 ) ) ;
#25300 = CARTESIAN_POINT ( 'NONE',  ( 10.81189881249999551, -6.242252689847874514, -25.65625000204839168 ) ) ;
#25301 = CARTESIAN_POINT ( 'NONE',  ( -10.81189881249999907, -6.242252689847864744, -40.96875000204835260 ) ) ;
#25302 = CARTESIAN_POINT ( 'NONE',  ( 7.070501591499376803E-16, 11.54700538379251284, -32.00000000409674783 ) ) ;
#25303 = CARTESIAN_POINT ( 'NONE',  ( -5.405949406250003975, -9.363379034771801557, -148.8437500020483810 ) ) ;
#25304 = CARTESIAN_POINT ( 'NONE',  ( -10.00000000000000000, -5.773502691896251982, -115.1249999999999858 ) ) ;
#25305 = CARTESIAN_POINT ( 'NONE',  ( -5.000000000000003553, -8.660254037844383745, -170.5000000000000000 ) ) ;
#25306 = CARTESIAN_POINT ( 'NONE',  ( -5.000000000000003553, -8.660254037844383745, -77.49999999999998579 ) ) ;
#25307 = CARTESIAN_POINT ( 'NONE',  ( 10.81189881249999907, 6.242252689847868297, -143.9062500020484094 ) ) ;
#25308 = CARTESIAN_POINT ( 'NONE',  ( 10.81189881249999729, 6.242252689847867408, -13.40625000204836326 ) ) ;
#25309 = ORIENTED_EDGE ( 'NONE', *, *, #18345, .T. ) ;
#25310 = CARTESIAN_POINT ( 'NONE',  ( -4.999999999999996447, 8.660254037844387298, -121.5000000000000000 ) ) ;
#25311 = CARTESIAN_POINT ( 'NONE',  ( 9.999999999999998224, 0.000000000000000000, -114.8750000040967905 ) ) ;
#25312 = CARTESIAN_POINT ( 'NONE',  ( 5.000000000000000000, 8.660254037844385522, -169.7500000000000000 ) ) ;
#25313 = CARTESIAN_POINT ( 'NONE',  ( -10.81189881249999907, -6.242252689847864744, -75.46875000204836681 ) ) ;
#25314 = CARTESIAN_POINT ( 'NONE',  ( -5.000000000000003553, -8.660254037844383745, -38.49999999999997868 ) ) ;
#25315 = CARTESIAN_POINT ( 'NONE',  ( -9.999999999999998224, 1.224646799147353059E-15, -22.62500000409675849 ) ) ;
#25316 = CYLINDRICAL_SURFACE ( 'NONE', #803, 9.999999999999998224 ) ;
#25317 = CARTESIAN_POINT ( 'NONE',  ( 7.644554776091147741E-16, 12.48450537969573659, -35.65625000204835970 ) ) ;
#25318 = CARTESIAN_POINT ( 'NONE',  ( -9.999999999999998224, 1.224646799147353059E-15, -78.12500000409677625 ) ) ;
#25319 = CARTESIAN_POINT ( 'NONE',  ( 7.644554776091147741E-16, 12.48450537969573659, -148.1562500020484094 ) ) ;
#25320 = CARTESIAN_POINT ( 'NONE',  ( 10.81189881249999729, 0.000000000000000000, -151.5312500020484094 ) ) ;
#25321 = CARTESIAN_POINT ( 'NONE',  ( -10.00000000000154188, 5.773502691895366468, -50.87499999999994316 ) ) ;
#25322 = CARTESIAN_POINT ( 'NONE',  ( 9.999999999999998224, 0.000000000000000000, -171.8750000040968189 ) ) ;
#25323 = ORIENTED_EDGE ( 'NONE', *, *, #30717, .T. ) ;
#25324 = EDGE_CURVE ( 'NONE', #16951, #40108, #17055, .T. ) ;
#25325 = ORIENTED_EDGE ( 'NONE', *, *, #2221, .F. ) ;
#25326 = CLOSED_SHELL ( 'NONE', ( #28078, #7469, #41143, #32960, #20890, #18014, #7230, #12340, #27771, #9592, #13514, #41382 ) ) ;
#25327 = ORIENTED_EDGE ( 'NONE', *, *, #25918, .F. ) ;
#25328 = FACE_OUTER_BOUND ( 'NONE', #42280, .T. ) ;
#25329 = CARTESIAN_POINT ( 'NONE',  ( 5.405949406249992428, -9.363379034771808662, -180.0937500020484094 ) ) ;
#25330 = CARTESIAN_POINT ( 'NONE',  ( -10.81189881249999729, 1.324075727343319199E-15, -27.59375000204836326 ) ) ;
#25331 = CYLINDRICAL_SURFACE ( 'NONE', #6079, 9.999999999999998224 ) ;
#25332 = CARTESIAN_POINT ( 'NONE',  ( 5.405949406249999534, 9.363379034771803333, -164.5937500020484094 ) ) ;
#25333 = CARTESIAN_POINT ( 'NONE',  ( -2.293366432827344421E-15, -12.48450537969573659, -153.2187500020483810 ) ) ;
#25334 = CARTESIAN_POINT ( 'NONE',  ( 0.000000000000000000, 0.000000000000000000, -169.9999999999999716 ) ) ;
#25335 = CARTESIAN_POINT ( 'NONE',  ( 5.405949406249992428, -9.363379034771808662, -136.5937500020483810 ) ) ;
#25336 = CARTESIAN_POINT ( 'NONE',  ( -2.293366432827344421E-15, -12.48450537969573659, -136.9062500020484094 ) ) ;
#25337 = CARTESIAN_POINT ( 'NONE',  ( 10.81189881249999729, 0.000000000000000000, -149.8437500020483810 ) ) ;
#25338 = CARTESIAN_POINT ( 'NONE',  ( 60.00000000000000711, 0.000000000000000000, -236.9999999999999716 ) ) ;
#25339 = CARTESIAN_POINT ( 'NONE',  ( -4.999999999999996447, 8.660254037844387298, -174.0000000000000284 ) ) ;
#25340 = CARTESIAN_POINT ( 'NONE',  ( 10.81189881249999907, 6.242252689847868297, -77.71875000204838102 ) ) ;
#25341 = CARTESIAN_POINT ( 'NONE',  ( -10.00000000000031797, 5.773502691896072569, -184.7500000040968189 ) ) ;
#25342 = CARTESIAN_POINT ( 'NONE',  ( -10.81189881249999907, -6.242252689847864744, -53.15625000204837391 ) ) ;
#25343 = CARTESIAN_POINT ( 'NONE',  ( -6.652853726956784897, 8.522716305231336165, -100.0000000000000142 ) ) ;
#25344 = EDGE_CURVE ( 'NONE', #12182, #17690, #38932, .T. ) ;
#25345 = CARTESIAN_POINT ( 'NONE',  ( 10.81189881249999907, 6.242252689847868297, -166.2187500020484094 ) ) ;
#25346 = CARTESIAN_POINT ( 'NONE',  ( -5.000000000000003553, -8.660254037844383745, -137.5000000000000000 ) ) ;
#25347 = CARTESIAN_POINT ( 'NONE',  ( 10.81189881249999551, -6.242252689847874514, -150.1562500020484094 ) ) ;
#25348 = CARTESIAN_POINT ( 'NONE',  ( 9.999999999999998224, 0.000000000000000000, -173.0000000000000284 ) ) ;
#25349 = CARTESIAN_POINT ( 'NONE',  ( -2.293366432827344421E-15, -12.48450537969573659, -39.40625000204836681 ) ) ;
#25350 = CARTESIAN_POINT ( 'NONE',  ( -2.121150477449813534E-15, -11.54700538379251284, -121.2500000040967905 ) ) ;
#25351 = CARTESIAN_POINT ( 'NONE',  ( 7.070501591499377789E-16, 11.54700538379251284, -100.6250000000000000 ) ) ;
#25352 = EDGE_LOOP ( 'NONE', ( #24426, #34709 ) ) ;
#25353 = CARTESIAN_POINT ( 'NONE',  ( -10.81189881249999729, 6.242252689847871849, -116.4062500020483952 ) ) ;
#25354 = CARTESIAN_POINT ( 'NONE',  ( -9.999999999999998224, 5.773502691896259087, -139.7500000040967905 ) ) ;
#25355 = CARTESIAN_POINT ( 'NONE',  ( 7.070501591499376803E-16, 11.54700538379251284, -52.62499999999997868 ) ) ;
#25356 = CARTESIAN_POINT ( 'NONE',  ( -2.293366432827344421E-15, -12.48450537969573659, -174.4062500020483810 ) ) ;
#25357 = CARTESIAN_POINT ( 'NONE',  ( -9.999999999999998224, 5.773502691896259087, -46.75000000409677625 ) ) ;
#25358 = CARTESIAN_POINT ( 'NONE',  ( 0.000000000000000000, 0.000000000000000000, -200.0000000000000000 ) ) ;
#25359 = CARTESIAN_POINT ( 'NONE',  ( -10.81189881249999729, 6.242252689847871849, -65.40625000204838102 ) ) ;
#25360 = CARTESIAN_POINT ( 'NONE',  ( 9.999999999999998224, 0.000000000000000000, -43.99999999999998579 ) ) ;
#25361 = CARTESIAN_POINT ( 'NONE',  ( -10.81189881249999729, 1.324075727343319199E-15, -168.7812500020484094 ) ) ;
#25362 = APPLICATION_CONTEXT ( 'configuration controlled 3d designs of mechanical parts and assemblies' ) ;
#25363 = CARTESIAN_POINT ( 'NONE',  ( 4.999999999999992006, -8.660254037844389075, -162.7500000000000000 ) ) ;
#25364 = DIRECTION ( 'NONE',  ( -0.000000000000000000, -0.000000000000000000, 1.000000000000000000 ) ) ;
#25365 = ORIENTED_EDGE ( 'NONE', *, *, #28344, .F. ) ;
#25366 = DIRECTION ( 'NONE',  ( 1.000000000000000000, 0.000000000000000000, 0.000000000000000000 ) ) ;
#25367 =( BOUNDED_CURVE ( )  B_SPLINE_CURVE ( 2, ( #4382, #33744, #10837, #27473, #1149, #23811, #26830 ),
 .UNSPECIFIED., .F., .F. ) 
 B_SPLINE_CURVE_WITH_KNOTS ( ( 3, 2, 2, 3 ),
 ( 0.3171641791044778058, 0.3184079601990050801, 0.3196517412935324653, 0.3208955223880597396 ),
 .UNSPECIFIED. ) 
 CURVE ( )  GEOMETRIC_REPRESENTATION_ITEM ( )  RATIONAL_B_SPLINE_CURVE ( ( 0.9999999999999820144, 0.8660254037844566932, 1.000000000000000000, 0.8660254037844387076, 1.000000000000000000, 0.8660254037844327124, 1.000000000000005995 ) ) 
 REPRESENTATION_ITEM ( '' )  );
#25368 = CARTESIAN_POINT ( 'NONE',  ( -9.999999999999998224, 1.224646799147353059E-15, -12.12500000409674783 ) ) ;
#25369 = CARTESIAN_POINT ( 'NONE',  ( 9.999999999999998224, 0.000000000000000000, -27.49999999999996803 ) ) ;
#25371 = VERTEX_POINT ( 'NONE', #19493 ) ;
#25370 = CARTESIAN_POINT ( 'NONE',  ( 10.81189881249999729, 0.000000000000000000, -81.03125000204839523 ) ) ;
#25373 = VERTEX_POINT ( 'NONE', #91 ) ;
#25372 = CARTESIAN_POINT ( 'NONE',  ( 9.999999999999998224, 0.000000000000000000, -140.0000000000000000 ) ) ;
#25374 = VERTEX_POINT ( 'NONE', #41944 ) ;
#25375 = CARTESIAN_POINT ( 'NONE',  ( -10.81189881249999729, 1.324075727343319199E-15, -30.59375000204836326 ) ) ;
#25376 = CARTESIAN_POINT ( 'NONE',  ( -9.999999999999998224, 1.224646799147353059E-15, -76.62500000409677625 ) ) ;
#25377 = CARTESIAN_POINT ( 'NONE',  ( 7.644554776091147741E-16, 12.48450537969573659, -2.656250002048344161 ) ) ;
#25379 = VERTEX_POINT ( 'NONE', #42155 ) ;
#25378 = CARTESIAN_POINT ( 'NONE',  ( 10.81189881249999551, -6.242252689847874514, -56.96875000204838102 ) ) ;
#25380 = DIRECTION ( 'NONE',  ( 1.000000000000000000, 0.000000000000000000, 0.000000000000000000 ) ) ;
#25381 = CARTESIAN_POINT ( 'NONE',  ( 7.070501591499377789E-16, 11.54700538379251284, -33.12499999999995737 ) ) ;
#25382 = CARTESIAN_POINT ( 'NONE',  ( -5.405949406249996869, 9.363379034771805109, -189.8437500020483810 ) ) ;
#25383 = CARTESIAN_POINT ( 'NONE',  ( 10.81189881249999907, 6.242252689847868297, -175.2187500020484094 ) ) ;
#25384 = CARTESIAN_POINT ( 'NONE',  ( -5.405949406249996869, 9.363379034771805109, -158.3437500020483810 ) ) ;
#25385 = CARTESIAN_POINT ( 'NONE',  ( 10.81189881249999729, 6.242252689847867408, -167.7187500020483526 ) ) ;
#25386 = CARTESIAN_POINT ( 'NONE',  ( 10.00000000000154010, -5.773502691895370020, -24.62499999999995026 ) ) ;
#25387 = CARTESIAN_POINT ( 'NONE',  ( -9.999999999999998224, 1.224646799147353059E-15, -194.7500000000000000 ) ) ;
#25388 = CARTESIAN_POINT ( 'NONE',  ( 7.644554776091147741E-16, 12.48450537969573659, -104.4687500020483668 ) ) ;
#25389 = CARTESIAN_POINT ( 'NONE',  ( 4.999999999999992006, -8.660254037844389075, -47.62500000409677625 ) ) ;
#25390 = AXIS2_PLACEMENT_3D ( 'NONE', #17818, #15638, #22353 ) ;
#25391 = CARTESIAN_POINT ( 'NONE',  ( 7.644554776091147741E-16, 12.48450537969573659, -74.65625000204838102 ) ) ;
#25392 = ADVANCED_FACE ( 'NONE', ( #29649 ), #22964, .T. ) ;
#25393 = CARTESIAN_POINT ( 'NONE',  ( 10.81189881249999729, 6.242252689847867408, -91.21875000204838102 ) ) ;
#25394 = ADVANCED_FACE ( 'NONE', ( #18871 ), #13213, .F. ) ;
#25395 = CARTESIAN_POINT ( 'NONE',  ( -5.405949406249996869, 9.363379034771805109, -61.03125000204837391 ) ) ;
#25396 = CARTESIAN_POINT ( 'NONE',  ( 9.999999999999996447, -5.773502691896262640, -149.5000000040968189 ) ) ;
#25397 = CARTESIAN_POINT ( 'NONE',  ( 9.999999999999998224, 0.000000000000000000, -123.5000000000000000 ) ) ;
#25398 = ORIENTED_EDGE ( 'NONE', *, *, #30362, .T. ) ;
#25399 = CARTESIAN_POINT ( 'NONE',  ( -10.81189881249999729, -6.242252689847864744, -147.6562500020483810 ) ) ;
#25400 = CARTESIAN_POINT ( 'NONE',  ( -10.81189881249999907, -6.242252689847864744, -165.6562500020483810 ) ) ;
#25401 = DIRECTION ( 'NONE',  ( -0.000000000000000000, -0.000000000000000000, 1.000000000000000000 ) ) ;
#25402 = CARTESIAN_POINT ( 'NONE',  ( 9.999999999999998224, 0.000000000000000000, -200.0000000000000000 ) ) ;
#25403 = CARTESIAN_POINT ( 'NONE',  ( 10.81189881249999907, 6.242252689847868297, -101.7187500020483810 ) ) ;
#25404 = ORIENTED_EDGE ( 'NONE', *, *, #8237, .T. ) ;
#25405 = CARTESIAN_POINT ( 'NONE',  ( 9.999999999999996447, -5.773502691896262640, -62.12499999999997868 ) ) ;
#25406 = CARTESIAN_POINT ( 'NONE',  ( 10.81189881249999729, 0.000000000000000000, -193.3437500020484094 ) ) ;
#25407 = CARTESIAN_POINT ( 'NONE',  ( -5.000000000000003553, -8.660254037844383745, -73.37500000409677625 ) ) ;
#25408 = CARTESIAN_POINT ( 'NONE',  ( 0.000000000000000000, 0.000000000000000000, -219.9999999999999716 ) ) ;
#25409 = CARTESIAN_POINT ( 'NONE',  ( 9.999999999999998224, 0.000000000000000000, -144.5000000000000000 ) ) ;
#25410 = CARTESIAN_POINT ( 'NONE',  ( 10.81189881249999551, -6.242252689847874514, -88.65625000204838102 ) ) ;
#25411 = CARTESIAN_POINT ( 'NONE',  ( -10.81189881249999729, -6.242252689847864744, -69.65625000204839523 ) ) ;
#25412 =( BOUNDED_CURVE ( )  B_SPLINE_CURVE ( 2, ( #4640, #4856, #11524, #17787, #31410, #28386, #30984 ),
 .UNSPECIFIED., .F., .F. ) 
 B_SPLINE_CURVE_WITH_KNOTS ( ( 3, 2, 2, 3 ),
 ( 0.1343283582089551953, 0.1355721393034825528, 0.1368159203980099381, 0.1380597014925373234 ),
 .UNSPECIFIED. ) 
 CURVE ( )  GEOMETRIC_REPRESENTATION_ITEM ( )  RATIONAL_B_SPLINE_CURVE ( ( 1.000000000000003109, 0.8660254037844358210, 1.000000000000000000, 0.8660254037844387076, 1.000000000000000000, 0.8660254037844387076, 1.000000000000000000 ) ) 
 REPRESENTATION_ITEM ( '' )  );
#25413 = CARTESIAN_POINT ( 'NONE',  ( -9.999999999999998224, 5.773502691896259087, -66.25000000409677625 ) ) ;
#25414 = CARTESIAN_POINT ( 'NONE',  ( -5.000000000000003553, -8.660254037844383745, -77.87500000409677625 ) ) ;
#25415 = CARTESIAN_POINT ( 'NONE',  ( -10.81189881249999907, -6.242252689847864744, -25.96875000204837391 ) ) ;
#25416 = CARTESIAN_POINT ( 'NONE',  ( 0.000000000000000000, 0.000000000000000000, -200.0000000000000000 ) ) ;
#25417 = CARTESIAN_POINT ( 'NONE',  ( -10.81189881249999907, -6.242252689847864744, -189.6562500020484094 ) ) ;
#25418 = CARTESIAN_POINT ( 'NONE',  ( 5.405949406249999534, 9.363379034771803333, -20.78125000204836326 ) ) ;
#25419 = CARTESIAN_POINT ( 'NONE',  ( 7.644554776091147741E-16, 12.48450537969573659, -3.968750002048366810 ) ) ;
#25420 = DIRECTION ( 'NONE',  ( 1.000000000000000000, 0.000000000000000000, 0.000000000000000000 ) ) ;
#25421 = EDGE_CURVE ( 'NONE', #26946, #29087, #29017, .T. ) ;
#25422 = CARTESIAN_POINT ( 'NONE',  ( -5.000000000000003553, -8.660254037844383745, -50.49999999999998579 ) ) ;
#25423 = CARTESIAN_POINT ( 'NONE',  ( -9.999999999999998224, 1.224646799147353059E-15, -159.1250000040967905 ) ) ;
#25424 =( BOUNDED_CURVE ( )  B_SPLINE_CURVE ( 2, ( #38510, #1852, #5504, #2284, #18653, #32263, #38730 ),
 .UNSPECIFIED., .F., .F. ) 
 B_SPLINE_CURVE_WITH_KNOTS ( ( 3, 2, 2, 3 ),
 ( 0.9552238805970153512, 0.9564676616915426255, 0.9577114427860698997, 0.9589552238805971740 ),
 .UNSPECIFIED. ) 
 CURVE ( )  GEOMETRIC_REPRESENTATION_ITEM ( )  RATIONAL_B_SPLINE_CURVE ( ( 0.9999999999999521494, 0.8660254037844865582, 1.000000000000000000, 0.8660254037844387076, 1.000000000000000000, 0.8660254037844267172, 1.000000000000011990 ) ) 
 REPRESENTATION_ITEM ( '' )  );
#25425 = CARTESIAN_POINT ( 'NONE',  ( -5.000000000000003553, -8.660254037844383745, -173.5000000000000284 ) ) ;
#25426 = CARTESIAN_POINT ( 'NONE',  ( -4.999999999999996447, 8.660254037844387298, -166.5000000000000000 ) ) ;
#25428 = ORIENTED_EDGE ( 'NONE', *, *, #14835, .F. ) ;
#25427 = CARTESIAN_POINT ( 'NONE',  ( 5.405949406249992428, -9.363379034771808662, -105.2812500020483810 ) ) ;
#25429 = CYLINDRICAL_SURFACE ( 'NONE', #21411, 9.999999999999998224 ) ;
#25430 = EDGE_CURVE ( 'NONE', #38098, #42101, #23763, .T. ) ;
#25431 = VECTOR ( 'NONE', #6911, 1000.000000000000000 ) ;
#25432 = ORIENTED_EDGE ( 'NONE', *, *, #6580, .F. ) ;
#25433 = EDGE_LOOP ( 'NONE', ( #13896, #28615, #5782, #26420 ) ) ;
#25434 = CARTESIAN_POINT ( 'NONE',  ( 10.81189881249999551, -6.242252689847874514, -28.65625000204838813 ) ) ;
#25435 = CONTEXT_DEPENDENT_SHAPE_REPRESENTATION ( #5577, #5301 ) ;
#25436 = CARTESIAN_POINT ( 'NONE',  ( 5.405949406249999534, 9.363379034771803333, -82.09375000204836681 ) ) ;
#25437 = CARTESIAN_POINT ( 'NONE',  ( 9.999999999999998224, 0.000000000000000000, -173.0000000000000284 ) ) ;
#25438 = CARTESIAN_POINT ( 'NONE',  ( 10.81189881249999907, 6.242252689847868297, -197.7187500020484094 ) ) ;
#25439 = CARTESIAN_POINT ( 'NONE',  ( -5.000000000000003553, -8.660254037844383745, -130.3750000040967905 ) ) ;
#25440 = DIRECTION ( 'NONE',  ( -1.000000000000000000, 0.000000000000000000, 0.000000000000000000 ) ) ;
#25441 = CARTESIAN_POINT ( 'NONE',  ( -2.293366432827344421E-15, -12.48450537969573659, -153.4062500020483810 ) ) ;
#25442 = CARTESIAN_POINT ( 'NONE',  ( 5.000000000000000000, 8.660254037844385522, -9.625000004096746054 ) ) ;
#25443 = CARTESIAN_POINT ( 'NONE',  ( -9.999999999999998224, 1.224646799147353059E-15, -172.6250000040968189 ) ) ;
#25444 = CARTESIAN_POINT ( 'NONE',  ( 7.644554776091147741E-16, 12.48450537969573659, -128.4687500020483810 ) ) ;
#25445 = ADVANCED_FACE ( 'NONE', ( #12796 ), #5719, .T. ) ;
#25446 = CARTESIAN_POINT ( 'NONE',  ( -2.293366432827344421E-15, -12.48450537969573659, -115.7187500020483668 ) ) ;
#25447 = CARTESIAN_POINT ( 'NONE',  ( 5.405949406249999534, 9.363379034771803333, -86.59375000204836681 ) ) ;
#25448 = CARTESIAN_POINT ( 'NONE',  ( -10.81189881249999729, 1.324075727343319199E-15, -90.78125000204838102 ) ) ;
#25449 = CARTESIAN_POINT ( 'NONE',  ( -4.999999999999996447, 8.660254037844387298, -172.8750000040968189 ) ) ;
#25450 = CARTESIAN_POINT ( 'NONE',  ( -10.81189881249999729, -6.242252689847864744, -171.6562500020484094 ) ) ;
#25451 = EDGE_CURVE ( 'NONE', #37898, #19247, #26786, .T. ) ;
#25452 = CARTESIAN_POINT ( 'NONE',  ( 9.999999999999994671, -5.773502691896262640, -133.0000000040967905 ) ) ;
#25453 = CARTESIAN_POINT ( 'NONE',  ( -5.405949406249996869, 9.363379034771805109, -173.5312500020484094 ) ) ;
#25454 = CARTESIAN_POINT ( 'NONE',  ( -5.405949406250003975, -9.363379034771801557, -186.5312500020484094 ) ) ;
#25455 = CARTESIAN_POINT ( 'NONE',  ( 10.81189881249999551, -6.242252689847874514, -44.96875000204836681 ) ) ;
#25456 = EDGE_CURVE ( 'NONE', #40819, #32901, #42363, .T. ) ;
#25457 = CARTESIAN_POINT ( 'NONE',  ( 4.999999999999992006, -8.660254037844389075, -163.1250000040967905 ) ) ;
#25458 = CARTESIAN_POINT ( 'NONE',  ( 10.81189881249999729, 0.000000000000000000, -0.03125000204837191653 ) ) ;
#25459 = CARTESIAN_POINT ( 'NONE',  ( -5.405949406249996869, 9.363379034771805109, -14.34375000204834905 ) ) ;
#25460 = CARTESIAN_POINT ( 'NONE',  ( -9.999999999999998224, 1.224646799147353059E-15, -157.2500000000000000 ) ) ;
#25461 = CARTESIAN_POINT ( 'NONE',  ( -10.81189881249999907, -6.242252689847864744, -118.9687500020483810 ) ) ;
#25462 = CARTESIAN_POINT ( 'NONE',  ( -2.121150477449813534E-15, -11.54700538379251284, -89.37499999999997158 ) ) ;
#25463 = CARTESIAN_POINT ( 'NONE',  ( 10.81189881249999551, -6.242252689847874514, -18.15625000204837391 ) ) ;
#25464 = CARTESIAN_POINT ( 'NONE',  ( -5.000000000000003553, -8.660254037844383745, -98.87500000409677625 ) ) ;
#25465 = AXIS2_PLACEMENT_3D ( 'NONE', #2507, #15213, #35095 ) ;
#25466 = CYLINDRICAL_SURFACE ( 'NONE', #30004, 9.999999999999998224 ) ;
#25467 = CARTESIAN_POINT ( 'NONE',  ( 5.405949406249999534, 9.363379034771803333, -119.7812500020483952 ) ) ;
#25468 = CARTESIAN_POINT ( 'NONE',  ( 10.81189881249999729, 0.000000000000000000, -91.53125000204838102 ) ) ;
#25469 = ORIENTED_EDGE ( 'NONE', *, *, #23660, .F. ) ;
#25470 = CARTESIAN_POINT ( 'NONE',  ( 9.999999999999996447, -5.773502691896262640, -95.50000000409677625 ) ) ;
#25471 = CARTESIAN_POINT ( 'NONE',  ( 9.999999999999998224, 0.000000000000000000, -200.0000000000000000 ) ) ;
#25472 = CARTESIAN_POINT ( 'NONE',  ( 5.405949406249999534, 9.363379034771803333, -158.7812500020484094 ) ) ;
#25473 = CARTESIAN_POINT ( 'NONE',  ( 10.81189881249999729, 0.000000000000000000, -47.84375000204838102 ) ) ;
#25474 = ORIENTED_EDGE ( 'NONE', *, *, #26996, .F. ) ;
#25475 = CARTESIAN_POINT ( 'NONE',  ( 5.000000000000000000, 8.660254037844385522, -13.74999999999995737 ) ) ;
#25476 = CARTESIAN_POINT ( 'NONE',  ( 10.81189881249999551, -6.242252689847874514, -24.15625000204838102 ) ) ;
#25477 = CARTESIAN_POINT ( 'NONE',  ( 9.999999999999998224, 0.000000000000000000, -150.5000000000000000 ) ) ;
#25478 = CARTESIAN_POINT ( 'NONE',  ( -5.000000000000003553, -8.660254037844383745, -23.87500000409675849 ) ) ;
#25479 = EDGE_CURVE ( 'NONE', #5730, #28672, #35364, .T. ) ;
#25480 = CARTESIAN_POINT ( 'NONE',  ( 7.070501591499377789E-16, 11.54700538379251284, -199.6250000000000000 ) ) ;
#25482 = ORIENTED_EDGE ( 'NONE', *, *, #11078, .F. ) ;
#25481 = CARTESIAN_POINT ( 'NONE',  ( -10.81189881249999729, 6.242252689847871849, -128.4062500020484094 ) ) ;
#25483 = CARTESIAN_POINT ( 'NONE',  ( 9.999999999999998224, 0.000000000000000000, -117.8750000040967905 ) ) ;
#25484 = VERTEX_POINT ( 'NONE', #17093 ) ;
#25485 = CARTESIAN_POINT ( 'NONE',  ( 10.81189881249999551, -6.242252689847874514, -54.15625000204837391 ) ) ;
#25486 = APPROVAL_ROLE ( '' ) ;
#25487 = CARTESIAN_POINT ( 'NONE',  ( -5.405949406249996869, 9.363379034771805109, -101.3437500020483810 ) ) ;
#25489 = EDGE_LOOP ( 'NONE', ( #16784, #33648, #19932, #20237 ) ) ;
#25488 = VERTEX_POINT ( 'NONE', #938 ) ;
#25490 =( BOUNDED_CURVE ( )  B_SPLINE_CURVE ( 2, ( #34954, #12047, #21986, #37965, #25243, #1506, #31719 ),
 .UNSPECIFIED., .F., .F. ) 
 B_SPLINE_CURVE_WITH_KNOTS ( ( 3, 2, 2, 3 ),
 ( 0.2425373134328359381, 0.2437810945273632957, 0.2450248756218906532, 0.2462686567164180107 ),
 .UNSPECIFIED. ) 
 CURVE ( )  GEOMETRIC_REPRESENTATION_ITEM ( )  RATIONAL_B_SPLINE_CURVE ( ( 0.9999999999999880096, 0.8660254037844506980, 1.000000000000000000, 0.8660254037844387076, 1.000000000000000000, 0.8660254037844267172, 1.000000000000011990 ) ) 
 REPRESENTATION_ITEM ( '' )  );
#25491 = CARTESIAN_POINT ( 'NONE',  ( -9.999999999999998224, 1.224646799147353059E-15, -200.0000000000000000 ) ) ;
#25492 = CARTESIAN_POINT ( 'NONE',  ( 5.000000000000000000, 8.660254037844385522, -171.2500000000000000 ) ) ;
#25493 = CARTESIAN_POINT ( 'NONE',  ( 7.644554776091147741E-16, 12.48450537969573659, -156.9687500020484094 ) ) ;
#25494 = CARTESIAN_POINT ( 'NONE',  ( 5.405949406249992428, -9.363379034771808662, -186.2812500020484094 ) ) ;
#25495 = CARTESIAN_POINT ( 'NONE',  ( 7.644554776091147741E-16, 12.48450537969573659, -3.968750002048366810 ) ) ;
#25496 = FACE_OUTER_BOUND ( 'NONE', #29378, .T. ) ;
#25497 = CARTESIAN_POINT ( 'NONE',  ( -10.81189881249999729, -6.242252689847864744, -141.4687500020483810 ) ) ;
#25498 = CARTESIAN_POINT ( 'NONE',  ( 10.81189881249999907, 6.242252689847868297, -106.2187500020483668 ) ) ;
#25499 = CARTESIAN_POINT ( 'NONE',  ( 4.999999999999992006, -8.660254037844389075, -149.6250000040967905 ) ) ;
#25500 = CARTESIAN_POINT ( 'NONE',  ( -2.293366432827344421E-15, -12.48450537969573659, -117.4062500020483952 ) ) ;
#25501 = CARTESIAN_POINT ( 'NONE',  ( -2.121150477449813534E-15, -11.54700538379251284, -196.2500000040967905 ) ) ;
#25502 = CARTESIAN_POINT ( 'NONE',  ( 10.81189881249999551, -6.242252689847874514, -124.4687500020483952 ) ) ;
#25503 = CARTESIAN_POINT ( 'NONE',  ( 10.81189881249999729, 0.000000000000000000, -195.0312500020484094 ) ) ;
#25504 = VECTOR ( 'NONE', #36528, 1000.000000000000000 ) ;
#25505 = CYLINDRICAL_SURFACE ( 'NONE', #28212, 9.999999999999998224 ) ;
#25506 = CARTESIAN_POINT ( 'NONE',  ( 7.070501591499377789E-16, 11.54700538379251284, -138.1250000000000000 ) ) ;
#25507 = CARTESIAN_POINT ( 'NONE',  ( -10.00000000000000000, -5.773502691896251982, -11.62499999999996803 ) ) ;
#25508 = CARTESIAN_POINT ( 'NONE',  ( 7.644554776091147741E-16, 12.48450537969573659, -71.46875000204836681 ) ) ;
#25509 = CARTESIAN_POINT ( 'NONE',  ( -10.81189881249999729, 6.242252689847871849, -56.21875000204837391 ) ) ;
#25510 = CARTESIAN_POINT ( 'NONE',  ( -9.999999999999998224, 5.773502691896259087, -187.7500000040967905 ) ) ;
#25511 = CARTESIAN_POINT ( 'NONE',  ( 10.81189881249999729, 0.000000000000000000, -28.53125000204837036 ) ) ;
#25512 = CARTESIAN_POINT ( 'NONE',  ( -5.405949406249996869, 9.363379034771805109, -36.84375000204836681 ) ) ;
#25513 = CARTESIAN_POINT ( 'NONE',  ( 9.999999999999998224, 0.000000000000000000, -105.4999999999999858 ) ) ;
#25514 = CARTESIAN_POINT ( 'NONE',  ( 10.81189881249999729, 0.000000000000000000, -145.3437500020483810 ) ) ;
#25515 = CARTESIAN_POINT ( 'NONE',  ( 4.999999999999992006, -8.660254037844389075, -113.2499999999999858 ) ) ;
#25516 = CARTESIAN_POINT ( 'NONE',  ( 0.000000000000000000, 0.000000000000000000, -99.99999999999998579 ) ) ;
#25517 = CARTESIAN_POINT ( 'NONE',  ( -2.121150477449813534E-15, -11.54700538379251284, -75.87500000000000000 ) ) ;
#25518 = CARTESIAN_POINT ( 'NONE',  ( 5.405949406249999534, 9.363379034771803333, -139.2812500020483810 ) ) ;
#25519 = CARTESIAN_POINT ( 'NONE',  ( 10.81189881249999729, 6.242252689847867408, -10.40625000204838102 ) ) ;
#25520 = EDGE_LOOP ( 'NONE', ( #2530, #34722, #12288, #32692 ) ) ;
#25521 = CARTESIAN_POINT ( 'NONE',  ( 9.999999999999742428, 5.773502691896404748, -120.7500000040967905 ) ) ;
#25522 = CARTESIAN_POINT ( 'NONE',  ( -10.00000000000000000, -5.773502691896251982, -117.0000000040967905 ) ) ;
#25523 = CARTESIAN_POINT ( 'NONE',  ( -5.000000000000003553, -8.660254037844383745, -38.87500000409676915 ) ) ;
#25524 = CARTESIAN_POINT ( 'NONE',  ( -5.405949406250003975, -9.363379034771801557, -73.84375000204838102 ) ) ;
#25525 = CARTESIAN_POINT ( 'NONE',  ( 9.999999999999996447, -5.773502691896262640, -41.12499999999997158 ) ) ;
#25526 = ADVANCED_FACE ( 'NONE', ( #27250 ), #37168, .F. ) ;
#25527 = CARTESIAN_POINT ( 'NONE',  ( -2.121150477449813534E-15, -11.54700538379251284, -22.25000000409676915 ) ) ;
#25528 = CARTESIAN_POINT ( 'NONE',  ( 5.405949406249992428, -9.363379034771808662, -51.28125000204835970 ) ) ;
#25529 = CARTESIAN_POINT ( 'NONE',  ( -9.999999999999998224, 1.224646799147353059E-15, -22.62500000409675849 ) ) ;
#25530 = CARTESIAN_POINT ( 'NONE',  ( -10.81189881249999907, -6.242252689847864744, -39.65625000204836681 ) ) ;
#25531 = CARTESIAN_POINT ( 'NONE',  ( -9.999999999999479527, -5.773502691896549521, -106.1249999999999716 ) ) ;
#25532 = CARTESIAN_POINT ( 'NONE',  ( 7.644554776091147741E-16, 12.48450537969573659, -146.6562500020484379 ) ) ;
#25533 = CARTESIAN_POINT ( 'NONE',  ( 7.644554776091147741E-16, 12.48450537969573659, -148.1562500020484094 ) ) ;
#25534 = CYLINDRICAL_SURFACE ( 'NONE', #8271, 9.999999999999998224 ) ;
#25535 = CYLINDRICAL_SURFACE ( 'NONE', #22445, 9.999999999999998224 ) ;
#25536 = ORIENTED_EDGE ( 'NONE', *, *, #35256, .T. ) ;
#25537 =( BOUNDED_CURVE ( )  B_SPLINE_CURVE ( 2, ( #509, #4151, #7392, #23795, #23374, #30499, #30280 ),
 .UNSPECIFIED., .F., .F. ) 
 B_SPLINE_CURVE_WITH_KNOTS ( ( 3, 2, 2, 3 ),
 ( 0.2873134328358210032, 0.2885572139303483885, 0.2898009950248757183, 0.2910447761194031036 ),
 .UNSPECIFIED. ) 
 CURVE ( )  GEOMETRIC_REPRESENTATION_ITEM ( )  RATIONAL_B_SPLINE_CURVE ( ( 0.9999999999999880096, 0.8660254037844506980, 1.000000000000000000, 0.8660254037844387076, 1.000000000000000000, 0.8660254037844267172, 1.000000000000011990 ) ) 
 REPRESENTATION_ITEM ( '' )  );
#25538 = VERTEX_POINT ( 'NONE', #23808 ) ;
#25539 = VERTEX_POINT ( 'NONE', #33741 ) ;
#25540 = CARTESIAN_POINT ( 'NONE',  ( -2.121150477449813534E-15, -11.54700538379251284, -176.7500000040967620 ) ) ;
#25541 = CARTESIAN_POINT ( 'NONE',  ( -10.81189881249999729, 1.324075727343319199E-15, -185.0937500020483810 ) ) ;
#25542 = CARTESIAN_POINT ( 'NONE',  ( -2.293366432827344421E-15, -12.48450537969573659, -34.71875000204835260 ) ) ;
#25543 = CARTESIAN_POINT ( 'NONE',  ( 10.00000000000025402, -5.773502691896113426, -130.0000000040967905 ) ) ;
#25544 = CARTESIAN_POINT ( 'NONE',  ( 5.405949406249992428, -9.363379034771808662, -165.0937500020484094 ) ) ;
#25545 = CARTESIAN_POINT ( 'NONE',  ( 7.644554776091147741E-16, 12.48450537969573659, -155.4687500020484094 ) ) ;
#25546 = DIRECTION ( 'NONE',  ( -0.000000000000000000, -0.000000000000000000, 1.000000000000000000 ) ) ;
#25547 = CARTESIAN_POINT ( 'NONE',  ( 7.644554776091147741E-16, 12.48450537969573659, -135.9687500020483810 ) ) ;
#25548 = CARTESIAN_POINT ( 'NONE',  ( 5.405949406249992428, -9.363379034771808662, -141.2812500020483810 ) ) ;
#25549 = CARTESIAN_POINT ( 'NONE',  ( -5.405949406250003975, -9.363379034771801557, -19.84375000204835615 ) ) ;
#25550 = CARTESIAN_POINT ( 'NONE',  ( 5.405949406249992428, -9.363379034771808662, -145.5937500020483810 ) ) ;
#25551 = CARTESIAN_POINT ( 'NONE',  ( -10.00000000000154188, 5.773502691895366468, -10.75000000409672118 ) ) ;
#25552 = CARTESIAN_POINT ( 'NONE',  ( -10.00000000000000000, -5.773502691896251982, -160.1250000000000284 ) ) ;
#25553 = VECTOR ( 'NONE', #33174, 1000.000000000000000 ) ;
#25554 = CARTESIAN_POINT ( 'NONE',  ( 10.81189881249999551, -6.242252689847874514, -83.96875000204838102 ) ) ;
#25555 = CARTESIAN_POINT ( 'NONE',  ( 9.999999999999998224, 0.000000000000000000, -200.0000000000000000 ) ) ;
#25556 = CARTESIAN_POINT ( 'NONE',  ( -5.405949406249996869, 9.363379034771805109, -53.53125000204836681 ) ) ;
#25557 = CARTESIAN_POINT ( 'NONE',  ( 10.81189881249999907, 6.242252689847868297, -61.21875000204836681 ) ) ;
#25558 = CARTESIAN_POINT ( 'NONE',  ( 5.405949406249992428, -9.363379034771808662, -166.5937500020484094 ) ) ;
#25559 = AXIS2_PLACEMENT_3D ( 'NONE', #2282, #2064, #38089 ) ;
#25560 = CARTESIAN_POINT ( 'NONE',  ( -5.000000000000003553, -8.660254037844383745, -136.0000000000000000 ) ) ;
#25561 = CARTESIAN_POINT ( 'NONE',  ( 5.405949406249992428, -9.363379034771808662, -144.2812500020483810 ) ) ;
#25562 = CARTESIAN_POINT ( 'NONE',  ( 9.999999999999998224, 0.000000000000000000, -15.87500000409675138 ) ) ;
#25563 = CARTESIAN_POINT ( 'NONE',  ( -5.405949406249996869, 9.363379034771805109, -35.53125000204837391 ) ) ;
#25564 = CARTESIAN_POINT ( 'NONE',  ( -4.999999999999996447, 8.660254037844387298, -124.8750000040967763 ) ) ;
#25565 = CARTESIAN_POINT ( 'NONE',  ( 9.999999999999996447, -5.773502691896262640, -102.6249999999999858 ) ) ;
#25566 = ORIENTED_EDGE ( 'NONE', *, *, #269, .F. ) ;
#25567 = CARTESIAN_POINT ( 'NONE',  ( 5.405949406249992428, -9.363379034771808662, -120.2812500020483952 ) ) ;
#25568 = CARTESIAN_POINT ( 'NONE',  ( -5.000000000000003553, -8.660254037844383745, -143.8750000040967905 ) ) ;
#25569 = CARTESIAN_POINT ( 'NONE',  ( 4.999999999999992006, -8.660254037844389075, -22.12500000409675494 ) ) ;
#25570 = CARTESIAN_POINT ( 'NONE',  ( 10.81189881249999551, -6.242252689847874514, -169.6562500020484094 ) ) ;
#25571 = CARTESIAN_POINT ( 'NONE',  ( 9.999999999999998224, 0.000000000000000000, -51.87500000409675494 ) ) ;
#25572 = CARTESIAN_POINT ( 'NONE',  ( 5.405949406249999534, 9.363379034771803333, -64.28125000204836681 ) ) ;
#25573 = CARTESIAN_POINT ( 'NONE',  ( 5.000000000000000000, 8.660254037844385522, -147.6250000040967905 ) ) ;
#25574 = CARTESIAN_POINT ( 'NONE',  ( 5.405949406249992428, -9.363379034771808662, -172.7812500020484094 ) ) ;
#25575 = CARTESIAN_POINT ( 'NONE',  ( -9.999999999999998224, 1.224646799147353059E-15, -82.24999999999998579 ) ) ;
#25576 = DIRECTION ( 'NONE',  ( -0.000000000000000000, -0.000000000000000000, 1.000000000000000000 ) ) ;
#25578 = ORIENTED_EDGE ( 'NONE', *, *, #39156, .F. ) ;
#25577 = ADVANCED_FACE ( 'NONE', ( #30293 ), #30511, .F. ) ;
#25579 = CARTESIAN_POINT ( 'NONE',  ( 10.00000000000012790, 5.773502691896179151, -173.2500000040967905 ) ) ;
#25580 = DIRECTION ( 'NONE',  ( 1.000000000000000000, 0.000000000000000000, 0.000000000000000000 ) ) ;
#25581 = CC_DESIGN_SECURITY_CLASSIFICATION ( #20040, ( #2849 ) ) ;
#25583 = VERTEX_POINT ( 'NONE', #27471 ) ;
#25582 = CARTESIAN_POINT ( 'NONE',  ( -10.81189881249999729, 1.324075727343319199E-15, -74.28125000204838102 ) ) ;
#25585 = ORIENTED_EDGE ( 'NONE', *, *, #23826, .F. ) ;
#25584 = CARTESIAN_POINT ( 'NONE',  ( -9.999999999999998224, 1.224646799147353059E-15, -100.6250000040967905 ) ) ;
#25586 = ORIENTED_EDGE ( 'NONE', *, *, #22769, .F. ) ;
#25587 = CARTESIAN_POINT ( 'NONE',  ( 10.81189881249999729, 0.000000000000000000, -29.84375000204836326 ) ) ;
#25588 = CARTESIAN_POINT ( 'NONE',  ( -10.81189881249999729, 6.242252689847871849, -8.406250002048372139 ) ) ;
#25590 = ORIENTED_EDGE ( 'NONE', *, *, #3279, .F. ) ;
#25589 = CARTESIAN_POINT ( 'NONE',  ( 7.644554776091147741E-16, 12.48450537969573659, -56.46875000204837391 ) ) ;
#25591 = CARTESIAN_POINT ( 'NONE',  ( -9.999999999999998224, 1.224646799147353059E-15, -179.7500000000000284 ) ) ;
#25592 = CARTESIAN_POINT ( 'NONE',  ( -5.000000000000003553, -8.660254037844383745, -27.99999999999996803 ) ) ;
#25593 = CARTESIAN_POINT ( 'NONE',  ( 5.405949406249992428, -9.363379034771808662, -186.0937500020483810 ) ) ;
#25594 = CARTESIAN_POINT ( 'NONE',  ( -10.81189881249999907, -6.242252689847864744, -175.9687500020483526 ) ) ;
#25595 = CARTESIAN_POINT ( 'NONE',  ( 10.81189881249999729, 0.000000000000000000, -158.8437500020483810 ) ) ;
#25596 = CARTESIAN_POINT ( 'NONE',  ( 10.81189881249999551, -6.242252689847874514, -173.9687500020483810 ) ) ;
#25597 = CARTESIAN_POINT ( 'NONE',  ( 9.999999999999479527, 5.773502691896553074, -41.25000000409674783 ) ) ;
#25598 = CARTESIAN_POINT ( 'NONE',  ( 10.00000000000015632, -5.773502691896169381, -191.5000000040968757 ) ) ;
#25599 = CARTESIAN_POINT ( 'NONE',  ( 4.999999999999992006, -8.660254037844389075, -195.7500000000000000 ) ) ;
#25600 = CARTESIAN_POINT ( 'NONE',  ( 5.405949406249999534, 9.363379034771803333, -106.0937500020483810 ) ) ;
#25601 = CARTESIAN_POINT ( 'NONE',  ( -2.275517850991317657E-15, -20.00000000000000000, -232.0000000000000000 ) ) ;
#25602 = CARTESIAN_POINT ( 'NONE',  ( 5.405949406249999534, 9.363379034771803333, -73.28125000204838102 ) ) ;
#25603 = CARTESIAN_POINT ( 'NONE',  ( 5.405949406249992428, -9.363379034771808662, -88.59375000204838102 ) ) ;
#25604 = CARTESIAN_POINT ( 'NONE',  ( 10.81189881249999907, 6.242252689847868297, -58.40625000204838102 ) ) ;
#25605 = CARTESIAN_POINT ( 'NONE',  ( -5.000000000000003553, -8.660254037844383745, -145.3750000040967905 ) ) ;
#25606 = CARTESIAN_POINT ( 'NONE',  ( -9.999999999999998224, 1.224646799147353059E-15, -119.7500000000000000 ) ) ;
#25607 = ORIENTED_EDGE ( 'NONE', *, *, #32743, .F. ) ;
#25608 = CARTESIAN_POINT ( 'NONE',  ( 10.81189881249999729, 0.000000000000000000, -141.0312500020483810 ) ) ;
#25609 = CARTESIAN_POINT ( 'NONE',  ( 7.644554776091147741E-16, 12.48450537969573659, -157.1562500020484094 ) ) ;
#25610 = APPROVAL_PERSON_ORGANIZATION ( #42278, #19346, #25486 ) ;
#25611 = CARTESIAN_POINT ( 'NONE',  ( 10.81189881249999907, 6.242252689847868297, -194.9062500020484379 ) ) ;
#25612 = FACE_OUTER_BOUND ( 'NONE', #3479, .T. ) ;
#25613 = CARTESIAN_POINT ( 'NONE',  ( -5.405949406249996869, 9.363379034771805109, -86.34375000204836681 ) ) ;
#25614 = VERTEX_POINT ( 'NONE', #17519 ) ;
#25615 = CARTESIAN_POINT ( 'NONE',  ( 4.999999999999992006, -8.660254037844389075, -65.24999999999997158 ) ) ;
#25616 = CARTESIAN_POINT ( 'NONE',  ( 7.644554776091147741E-16, 12.48450537969573659, -191.4687500020484094 ) ) ;
#25617 = CARTESIAN_POINT ( 'NONE',  ( 9.999999999999998224, 0.000000000000000000, -77.37500000409677625 ) ) ;
#25618 = CARTESIAN_POINT ( 'NONE',  ( 9.999999999999998224, 0.000000000000000000, -66.49999999999997158 ) ) ;
#25619 =( BOUNDED_CURVE ( )  B_SPLINE_CURVE ( 2, ( #19035, #25531, #5881, #25105, #34816, #38680, #32009 ),
 .UNSPECIFIED., .F., .F. ) 
 B_SPLINE_CURVE_WITH_KNOTS ( ( 3, 2, 2, 3 ),
 ( 0.4664179104477613191, 0.4676616915422886489, 0.4689054726368160342, 0.4701492537313434195 ),
 .UNSPECIFIED. ) 
 CURVE ( )  GEOMETRIC_REPRESENTATION_ITEM ( )  RATIONAL_B_SPLINE_CURVE ( ( 0.9999999999999880096, 0.8660254037844506980, 1.000000000000000000, 0.8660254037844387076, 1.000000000000000000, 0.8660254037844267172, 1.000000000000011990 ) ) 
 REPRESENTATION_ITEM ( '' )  );
#25620 = DIRECTION ( 'NONE',  ( 0.000000000000000000, 0.08715574274765837404, -0.9961946980917455452 ) ) ;
#25621 = CARTESIAN_POINT ( 'NONE',  ( -5.405949406249996869, 9.363379034771805109, -86.53125000204838102 ) ) ;
#25622 = CARTESIAN_POINT ( 'NONE',  ( -5.405949406249996869, 9.363379034771805109, -64.03125000204836681 ) ) ;
#25623 = CARTESIAN_POINT ( 'NONE',  ( -9.999999999999998224, 5.773502691896259087, -69.25000000409677625 ) ) ;
#25624 = CARTESIAN_POINT ( 'NONE',  ( 10.00000000000051159, -5.773502691895965988, -77.50000000409677625 ) ) ;
#25625 = CARTESIAN_POINT ( 'NONE',  ( -10.81189881249999907, -6.242252689847864744, -16.96875000204836681 ) ) ;
#25626 = CARTESIAN_POINT ( 'NONE',  ( 9.999999999999998224, 0.000000000000000000, -33.87500000409676915 ) ) ;
#25627 = CARTESIAN_POINT ( 'NONE',  ( 5.405949406249999534, 9.363379034771803333, -191.7812500020484094 ) ) ;
#25628 = CARTESIAN_POINT ( 'NONE',  ( -2.293366432827344421E-15, -12.48450537969573659, -18.40625000204837391 ) ) ;
#25629 = CARTESIAN_POINT ( 'NONE',  ( -5.405949406250003975, -9.363379034771801557, -4.843750002048369474 ) ) ;
#25630 = CARTESIAN_POINT ( 'NONE',  ( 7.070501591499376803E-16, 11.54700538379251284, -140.0000000040967905 ) ) ;
#25631 = CARTESIAN_POINT ( 'NONE',  ( 9.999999999999998224, 0.000000000000000000, -170.0000000000000000 ) ) ;
#25632 = CARTESIAN_POINT ( 'NONE',  ( -9.999999999999998224, 1.224646799147353059E-15, -125.7499999999999716 ) ) ;
#25633 = CARTESIAN_POINT ( 'NONE',  ( -9.999999999999998224, 1.224646799147353059E-15, -172.2500000000000000 ) ) ;
#25635 = VERTEX_POINT ( 'NONE', #10621 ) ;
#25634 = CARTESIAN_POINT ( 'NONE',  ( 10.81189881249999907, 6.242252689847868297, -98.90625000204839523 ) ) ;
#25636 = CARTESIAN_POINT ( 'NONE',  ( 9.999999999999998224, 0.000000000000000000, -37.99999999999997868 ) ) ;
#25637 = EDGE_CURVE ( 'NONE', #19402, #24501, #7405, .T. ) ;
#25638 = ORIENTED_EDGE ( 'NONE', *, *, #1835, .T. ) ;
#25639 = ADVANCED_FACE ( 'NONE', ( #14270 ), #9988, .T. ) ;
#25640 = VERTEX_POINT ( 'NONE', #23167 ) ;
#25641 = VECTOR ( 'NONE', #7250, 1000.000000000000000 ) ;
#25642 = CARTESIAN_POINT ( 'NONE',  ( -10.81189881249999729, 6.242252689847871849, -26.40625000204837747 ) ) ;
#25643 = CARTESIAN_POINT ( 'NONE',  ( 10.81189881249999907, 6.242252689847868297, -80.71875000204838102 ) ) ;
#25644 = CARTESIAN_POINT ( 'NONE',  ( -4.999999999999996447, 8.660254037844387298, -126.0000000000000000 ) ) ;
#25645 =( BOUNDED_CURVE ( )  B_SPLINE_CURVE ( 2, ( #37936, #8381, #18500, #21531, #20880, #34067, #8591 ),
 .UNSPECIFIED., .F., .F. ) 
 B_SPLINE_CURVE_WITH_KNOTS ( ( 3, 2, 2, 3 ),
 ( 0.3992537313432836799, 0.4004975124378110651, 0.4017412935323383949, 0.4029850746268657802 ),
 .UNSPECIFIED. ) 
 CURVE ( )  GEOMETRIC_REPRESENTATION_ITEM ( )  RATIONAL_B_SPLINE_CURVE ( ( 0.9999999999999880096, 0.8660254037844506980, 1.000000000000000000, 0.8660254037844387076, 1.000000000000000000, 0.8660254037844267172, 1.000000000000011990 ) ) 
 REPRESENTATION_ITEM ( '' )  );
#25646 = CARTESIAN_POINT ( 'NONE',  ( -2.121150477449813534E-15, -11.54700538379251284, -130.2500000040967905 ) ) ;
#25647 = CARTESIAN_POINT ( 'NONE',  ( -9.999999999999998224, 1.224646799147353059E-15, -200.0000000000000000 ) ) ;
#25648 = CARTESIAN_POINT ( 'NONE',  ( -10.81189881249999729, 1.324075727343319199E-15, -155.2812500020484094 ) ) ;
#25649 = CARTESIAN_POINT ( 'NONE',  ( -10.00000000000000000, -5.773502691896251982, -7.500000004096747830 ) ) ;
#25650 = AXIS2_PLACEMENT_3D ( 'NONE', #6859, #42461, #20011 ) ;
#25651 = CARTESIAN_POINT ( 'NONE',  ( -9.999999999999479527, -5.773502691896549521, -77.62499999999995737 ) ) ;
#25652 = CARTESIAN_POINT ( 'NONE',  ( 7.644554776091147741E-16, 12.48450537969573659, -131.4687500020483810 ) ) ;
#25653 = CARTESIAN_POINT ( 'NONE',  ( -5.405949406250003975, -9.363379034771801557, -114.3437500020483810 ) ) ;
#25654 = CARTESIAN_POINT ( 'NONE',  ( -10.81189881249999907, -6.242252689847864744, -76.96875000204836681 ) ) ;
#25655 = CARTESIAN_POINT ( 'NONE',  ( -5.405949406249996869, 9.363379034771805109, -85.03125000204838102 ) ) ;
#25656 = CARTESIAN_POINT ( 'NONE',  ( -9.999999999999998224, 5.773502691896259087, -166.7500000040967905 ) ) ;
#25657 =( BOUNDED_CURVE ( )  B_SPLINE_CURVE ( 2, ( #3140, #35939, #18681, #12828, #12199, #22356, #2517 ),
 .UNSPECIFIED., .F., .F. ) 
 B_SPLINE_CURVE_WITH_KNOTS ( ( 3, 2, 2, 3 ),
 ( 0.5708955223880599616, 0.5721393034825872359, 0.5733830845771146212, 0.5746268656716420065 ),
 .UNSPECIFIED. ) 
 CURVE ( )  GEOMETRIC_REPRESENTATION_ITEM ( )  RATIONAL_B_SPLINE_CURVE ( ( 0.9999999999999761302, 0.8660254037844625774, 1.000000000000000000, 0.8660254037844387076, 1.000000000000000000, 0.8660254037844148378, 1.000000000000023981 ) ) 
 REPRESENTATION_ITEM ( '' )  );
#25658 = CARTESIAN_POINT ( 'NONE',  ( -10.00000000000051337, 5.773502691895962435, -81.25000000409677625 ) ) ;
#25659 = CARTESIAN_POINT ( 'NONE',  ( 10.81189881249999551, -6.242252689847874514, -165.1562500020483526 ) ) ;
#25660 = CARTESIAN_POINT ( 'NONE',  ( -5.405949406249996869, 9.363379034771805109, -179.5312500020483810 ) ) ;
#25661 = CARTESIAN_POINT ( 'NONE',  ( -2.293366432827344421E-15, -12.48450537969573659, -45.21875000204837391 ) ) ;
#25662 = CARTESIAN_POINT ( 'NONE',  ( -9.999999999999998224, 1.224646799147353059E-15, -156.1250000040967905 ) ) ;
#25663 = CARTESIAN_POINT ( 'NONE',  ( -10.81189881249999729, 1.324075727343319199E-15, -0.7812500020483725827 ) ) ;
#25664 = CARTESIAN_POINT ( 'NONE',  ( -5.405949406250003975, -9.363379034771801557, -1.843750002048366587 ) ) ;
#25665 = CARTESIAN_POINT ( 'NONE',  ( 10.00000000000102318, -5.773502691895667560, -59.50000000409674072 ) ) ;
#25666 = CARTESIAN_POINT ( 'NONE',  ( -10.81189881249999907, -6.242252689847864744, -111.4687500020483810 ) ) ;
#25667 = CARTESIAN_POINT ( 'NONE',  ( 9.999999999999998224, 0.000000000000000000, -91.99999999999998579 ) ) ;
#25668 = CARTESIAN_POINT ( 'NONE',  ( -10.81189881249999729, 1.324075727343319199E-15, -12.78125000204835615 ) ) ;
#25669 = CARTESIAN_POINT ( 'NONE',  ( -4.999999999999996447, 8.660254037844387298, -94.87500000409677625 ) ) ;
#25670 = CARTESIAN_POINT ( 'NONE',  ( -57.00000000000002132, 0.000000000000000000, -220.0000000000000000 ) ) ;
#25671 = CARTESIAN_POINT ( 'NONE',  ( 7.644554776091147741E-16, 12.48450537969573659, -115.1562500020483952 ) ) ;
#25672 = CARTESIAN_POINT ( 'NONE',  ( 10.81189881249999729, 0.000000000000000000, -90.03125000204838102 ) ) ;
#25673 = EDGE_LOOP ( 'NONE', ( #29904, #27160, #16987, #29661 ) ) ;
#25674 = VECTOR ( 'NONE', #41381, 1000.000000000000000 ) ;
#25675 =( BOUNDED_CURVE ( )  B_SPLINE_CURVE ( 2, ( #23164, #16446, #7184, #3953, #936, #19912, #10832 ),
 .UNSPECIFIED., .F., .F. ) 
 B_SPLINE_CURVE_WITH_KNOTS ( ( 3, 2, 2, 3 ),
 ( 0.7985074626865673597, 0.7997512437810947450, 0.8009950248756220192, 0.8022388059701494045 ),
 .UNSPECIFIED. ) 
 CURVE ( )  GEOMETRIC_REPRESENTATION_ITEM ( )  RATIONAL_B_SPLINE_CURVE ( ( 0.9999999999999761302, 0.8660254037844625774, 1.000000000000000000, 0.8660254037844387076, 1.000000000000000000, 0.8660254037844267172, 1.000000000000011990 ) ) 
 REPRESENTATION_ITEM ( '' )  );
#25676 = CARTESIAN_POINT ( 'NONE',  ( -9.999999999999998224, 1.224646799147353059E-15, -90.12500000409677625 ) ) ;
#25677 = DIRECTION ( 'NONE',  ( 1.000000000000000000, 0.000000000000000000, 0.000000000000000000 ) ) ;
#25678 = CARTESIAN_POINT ( 'NONE',  ( -5.405949406250003975, -9.363379034771801557, -51.34375000204835260 ) ) ;
#25679 = ORIENTED_EDGE ( 'NONE', *, *, #34402, .F. ) ;
#25680 = CARTESIAN_POINT ( 'NONE',  ( 7.070501591499377789E-16, 11.54700538379251284, -16.62499999999996447 ) ) ;
#25681 = CARTESIAN_POINT ( 'NONE',  ( 5.405949406249999534, 9.363379034771803333, -22.28125000204836326 ) ) ;
#25682 = CARTESIAN_POINT ( 'NONE',  ( -9.999999999999998224, 1.224646799147353059E-15, -149.7500000000000000 ) ) ;
#25683 = CARTESIAN_POINT ( 'NONE',  ( -9.999999999999998224, 5.773502691896259087, -22.75000000409677270 ) ) ;
#25684 = CIRCLE ( 'NONE', #17389, 57.00000000000002132 ) ;
#25685 = CARTESIAN_POINT ( 'NONE',  ( 9.999999999999998224, 0.000000000000000000, -195.5000000000000000 ) ) ;
#25687 = VERTEX_POINT ( 'NONE', #6761 ) ;
#25686 = CARTESIAN_POINT ( 'NONE',  ( 7.644554776091147741E-16, 12.48450537969573659, -127.1562500020483952 ) ) ;
#25689 = EDGE_CURVE ( 'NONE', #6874, #25274, #34235, .T. ) ;
#25688 = CARTESIAN_POINT ( 'NONE',  ( 10.00000000000051159, -5.773502691895965988, -152.1250000000000000 ) ) ;
#25690 = EDGE_CURVE ( 'NONE', #37716, #12293, #10412, .T. ) ;
#25691 = VERTEX_POINT ( 'NONE', #40191 ) ;
#25692 = ADVANCED_FACE ( 'NONE', ( #40390 ), #3529, .T. ) ;
#25693 = CARTESIAN_POINT ( 'NONE',  ( -10.81189881249999907, -6.242252689847864744, -53.15625000204837391 ) ) ;
#25694 = PERSON_AND_ORGANIZATION_ROLE ( 'design_supplier' ) ;
#25695 = CARTESIAN_POINT ( 'NONE',  ( -10.81189881249999729, 1.324075727343319199E-15, -101.0937500020483810 ) ) ;
#25697 = ORIENTED_EDGE ( 'NONE', *, *, #37512, .F. ) ;
#25696 = VERTEX_POINT ( 'NONE', #7616 ) ;
#25698 = LINE ( 'NONE', #22030, #42445 ) ;
#25699 = CC_DESIGN_PERSON_AND_ORGANIZATION_ASSIGNMENT ( #36242, #17431, ( #26987 ) ) ;
#25700 = CARTESIAN_POINT ( 'NONE',  ( 9.999999999999998224, 0.000000000000000000, -119.0000000000000000 ) ) ;
#25701 = CARTESIAN_POINT ( 'NONE',  ( 10.81189881249999729, 0.000000000000000000, -151.3437500020483810 ) ) ;
#25702 = CARTESIAN_POINT ( 'NONE',  ( -10.81189881249999729, 6.242252689847871849, -183.9062500020484094 ) ) ;
#25703 = CARTESIAN_POINT ( 'NONE',  ( -10.81189881249999729, 1.324075727343319199E-15, -9.593750002048345493 ) ) ;
#25704 = DIRECTION ( 'NONE',  ( 1.000000000000000000, 0.000000000000000000, 0.000000000000000000 ) ) ;
#25705 = CARTESIAN_POINT ( 'NONE',  ( 10.81189881249999729, 6.242252689847867408, -143.7187500020484094 ) ) ;
#25706 = CARTESIAN_POINT ( 'NONE',  ( -10.81189881249999729, 6.242252689847871849, -98.21875000204838102 ) ) ;
#25707 = CARTESIAN_POINT ( 'NONE',  ( -5.000000000000003553, -8.660254037844383745, -148.0000000000000000 ) ) ;
#25708 = CARTESIAN_POINT ( 'NONE',  ( 10.81189881249999907, 6.242252689847868297, -107.9062500020483668 ) ) ;
#25709 = CARTESIAN_POINT ( 'NONE',  ( -2.121150477449813534E-15, -11.54700538379251284, -194.7500000040967905 ) ) ;
#25710 = CARTESIAN_POINT ( 'NONE',  ( -10.81189881249999729, 1.324075727343319199E-15, -123.5937500020483952 ) ) ;
#25711 = CARTESIAN_POINT ( 'NONE',  ( 5.405949406249992428, -9.363379034771808662, -186.2812500020484094 ) ) ;
#25712 = CARTESIAN_POINT ( 'NONE',  ( 4.999999999999992006, -8.660254037844389075, -47.24999999999998579 ) ) ;
#25713 = CARTESIAN_POINT ( 'NONE',  ( -2.121150477449813534E-15, -11.54700538379251284, -138.8750000000000000 ) ) ;
#25714 = CARTESIAN_POINT ( 'NONE',  ( 9.999999999999996447, -5.773502691896262640, -14.12499999999997158 ) ) ;
#25715 = EDGE_CURVE ( 'NONE', #41597, #34758, #7186, .T. ) ;
#25716 = CARTESIAN_POINT ( 'NONE',  ( -5.405949406249996869, 9.363379034771805109, -66.84375000204836681 ) ) ;
#25717 = CARTESIAN_POINT ( 'NONE',  ( -5.405949406250003975, -9.363379034771801557, -45.34375000204838102 ) ) ;
#25718 = CARTESIAN_POINT ( 'NONE',  ( 9.999999999999998224, 0.000000000000000000, -185.3750000040967905 ) ) ;
#25719 = CARTESIAN_POINT ( 'NONE',  ( -5.405949406249996869, 9.363379034771805109, -23.53125000204836681 ) ) ;
#25720 = CARTESIAN_POINT ( 'NONE',  ( -5.405949406249996869, 9.363379034771805109, -38.34375000204837391 ) ) ;
#25721 = DIRECTION ( 'NONE',  ( 1.000000000000000000, 0.000000000000000000, 0.000000000000000000 ) ) ;
#25722 = CARTESIAN_POINT ( 'NONE',  ( 10.81189881249999551, -6.242252689847874514, -137.9687500020483810 ) ) ;
#25723 = CARTESIAN_POINT ( 'NONE',  ( 7.070501591499377789E-16, 11.54700538379251284, -111.1249999999999716 ) ) ;
#25724 = LINE ( 'NONE', #12111, #3818 ) ;
#25725 = CARTESIAN_POINT ( 'NONE',  ( 5.000000000000000000, 8.660254037844385522, -69.24999999999997158 ) ) ;
#25726 = CARTESIAN_POINT ( 'NONE',  ( -10.81189881249999729, 1.324075727343319199E-15, -137.2812500020483810 ) ) ;
#25727 = CARTESIAN_POINT ( 'NONE',  ( -10.81189881249999729, 6.242252689847871849, -119.4062500020483952 ) ) ;
#25728 = ORIENTED_EDGE ( 'NONE', *, *, #30976, .F. ) ;
#25729 = CARTESIAN_POINT ( 'NONE',  ( -9.999999999999998224, 1.224646799147353059E-15, -104.7499999999999858 ) ) ;
#25730 = CARTESIAN_POINT ( 'NONE',  ( 9.999999999999996447, -5.773502691896262640, -118.0000000040967905 ) ) ;
#25731 = DIRECTION ( 'NONE',  ( -1.000000000000000000, 0.000000000000000000, 0.000000000000000000 ) ) ;
#25732 = CARTESIAN_POINT ( 'NONE',  ( 10.81189881249999907, 6.242252689847868297, -70.21875000204838102 ) ) ;
#25733 = CARTESIAN_POINT ( 'NONE',  ( 9.999999999999996447, -5.773502691896262640, -38.12499999999995737 ) ) ;
#25734 = CARTESIAN_POINT ( 'NONE',  ( -2.121150477449813534E-15, -11.54700538379251284, -29.75000000409675849 ) ) ;
#25735 = CARTESIAN_POINT ( 'NONE',  ( -10.81189881249999729, -6.242252689847864744, -44.15625000204838102 ) ) ;
#25736 = EDGE_CURVE ( 'NONE', #2293, #17414, #28181, .T. ) ;
#25737 = CARTESIAN_POINT ( 'NONE',  ( 10.00000000000051159, -5.773502691895965988, -141.6250000000000000 ) ) ;
#25738 = CARTESIAN_POINT ( 'NONE',  ( 5.405949406249992428, -9.363379034771808662, -34.78125000204837391 ) ) ;
#25739 = CARTESIAN_POINT ( 'NONE',  ( 9.999999999999998224, 0.000000000000000000, -185.0000000000000000 ) ) ;
#25740 = CARTESIAN_POINT ( 'NONE',  ( 5.405949406249992428, -9.363379034771808662, -133.7812500020483810 ) ) ;
#25741 = CARTESIAN_POINT ( 'NONE',  ( -10.81189881249999907, -6.242252689847864744, -153.6562500020484094 ) ) ;
#25742 = CARTESIAN_POINT ( 'NONE',  ( -9.999999999999998224, 1.224646799147353059E-15, -152.7500000000000000 ) ) ;
#25743 =( BOUNDED_CURVE ( )  B_SPLINE_CURVE ( 2, ( #25126, #35266, #5261, #32239, #32031, #18413, #15590 ),
 .UNSPECIFIED., .F., .F. ) 
 B_SPLINE_CURVE_WITH_KNOTS ( ( 3, 2, 2, 3 ),
 ( 0.2089552238805970630, 0.2101990049751244205, 0.2114427860696518058, 0.2126865671641791633 ),
 .UNSPECIFIED. ) 
 CURVE ( )  GEOMETRIC_REPRESENTATION_ITEM ( )  RATIONAL_B_SPLINE_CURVE ( ( 0.9999999999999940048, 0.8660254037844447028, 1.000000000000000000, 0.8660254037844387076, 1.000000000000000000, 0.8660254037844327124, 1.000000000000005995 ) ) 
 REPRESENTATION_ITEM ( '' )  );
#25744 = CARTESIAN_POINT ( 'NONE',  ( 0.000000000000000000, 0.000000000000000000, -99.99999999999998579 ) ) ;
#25745 = ORIENTED_EDGE ( 'NONE', *, *, #4288, .T. ) ;
#25746 = EDGE_LOOP ( 'NONE', ( #31758, #41572, #1484, #34777 ) ) ;
#25747 = ORIENTED_EDGE ( 'NONE', *, *, #18589, .T. ) ;
#25748 = CARTESIAN_POINT ( 'NONE',  ( 10.00000000000044764, -5.773502691896004180, -176.5000000040967905 ) ) ;
#25749 = CARTESIAN_POINT ( 'NONE',  ( 7.644554776091147741E-16, 12.48450537969573659, -180.9687500020484094 ) ) ;
#25751 = ADVANCED_FACE ( 'NONE', ( #16878 ), #36538, .T. ) ;
#25750 = CARTESIAN_POINT ( 'NONE',  ( 5.405949406249992428, -9.363379034771808662, -34.59375000204836681 ) ) ;
#25752 = LINE ( 'NONE', #38905, #4675 ) ;
#25753 = CARTESIAN_POINT ( 'NONE',  ( -5.405949406250003975, -9.363379034771801557, -163.8437500020484094 ) ) ;
#25754 = CARTESIAN_POINT ( 'NONE',  ( -5.405949406250003975, -9.363379034771801557, -144.3437500020483810 ) ) ;
#25755 = CARTESIAN_POINT ( 'NONE',  ( 9.999999999999998224, 0.000000000000000000, -131.0000000000000000 ) ) ;
#25756 = CARTESIAN_POINT ( 'NONE',  ( 5.405949406249999534, 9.363379034771803333, -130.0937500020483810 ) ) ;
#25757 = CARTESIAN_POINT ( 'NONE',  ( 5.405949406249992428, -9.363379034771808662, -144.2812500020483810 ) ) ;
#25758 = CARTESIAN_POINT ( 'NONE',  ( -5.405949406250003975, -9.363379034771801557, -18.34375000204835260 ) ) ;
#25759 = CARTESIAN_POINT ( 'NONE',  ( -5.405949406250003975, -9.363379034771801557, -142.8437500020483810 ) ) ;
#25760 = DIRECTION ( 'NONE',  ( 1.000000000000000000, 0.000000000000000000, 0.000000000000000000 ) ) ;
#25761 = LINE ( 'NONE', #10182, #3398 ) ;
#25762 = CARTESIAN_POINT ( 'NONE',  ( -2.121150477449813534E-15, -11.54700538379251284, -159.8750000000000000 ) ) ;
#25763 = CARTESIAN_POINT ( 'NONE',  ( 5.405949406249999534, 9.363379034771803333, -80.59375000204838102 ) ) ;
#25764 = CARTESIAN_POINT ( 'NONE',  ( -2.293366432827344421E-15, -12.48450537969573659, -51.40625000204838102 ) ) ;
#25765 = CARTESIAN_POINT ( 'NONE',  ( 10.81189881249999729, 0.000000000000000000, -58.34375000204835970 ) ) ;
#25766 = LINE ( 'NONE', #16015, #41261 ) ;
#25767 = CARTESIAN_POINT ( 'NONE',  ( 10.81189881249999907, 6.242252689847868297, -173.7187500020484094 ) ) ;
#25768 = CARTESIAN_POINT ( 'NONE',  ( 9.999999999999998224, 0.000000000000000000, -137.0000000000000000 ) ) ;
#25769 = CARTESIAN_POINT ( 'NONE',  ( 10.81189881249999729, 0.000000000000000000, -144.0312500020483810 ) ) ;
#25770 = DIRECTION ( 'NONE',  ( -1.000000000000000000, 0.000000000000000000, 0.000000000000000000 ) ) ;
#25771 = CARTESIAN_POINT ( 'NONE',  ( 10.00000000000000000, 5.773502691896255534, -122.2500000040968047 ) ) ;
#25772 = CARTESIAN_POINT ( 'NONE',  ( 9.999999999999996447, -5.773502691896262640, -95.12499999999998579 ) ) ;
#25773 = ORIENTED_EDGE ( 'NONE', *, *, #2979, .T. ) ;
#25774 = CARTESIAN_POINT ( 'NONE',  ( 7.644554776091147741E-16, 12.48450537969573659, -115.1562500020483952 ) ) ;
#25775 = CARTESIAN_POINT ( 'NONE',  ( 4.999999999999992006, -8.660254037844389075, -137.6250000040967620 ) ) ;
#25776 = CARTESIAN_POINT ( 'NONE',  ( 9.999999999999998224, 0.000000000000000000, -159.5000000000000000 ) ) ;
#25777 = CARTESIAN_POINT ( 'NONE',  ( 7.644554776091147741E-16, 12.48450537969573659, -169.1562500020484094 ) ) ;
#25778 = CARTESIAN_POINT ( 'NONE',  ( -2.121150477449813534E-15, -11.54700538379251284, -53.75000000409677625 ) ) ;
#25779 = CARTESIAN_POINT ( 'NONE',  ( -5.000000000000003553, -8.660254037844383745, -160.0000000000000000 ) ) ;
#25780 = CARTESIAN_POINT ( 'NONE',  ( -10.81189881249999729, 6.242252689847871849, -59.40625000204838813 ) ) ;
#25781 =( BOUNDED_CURVE ( )  B_SPLINE_CURVE ( 2, ( #20897, #30045, #11602, #8180, #1925, #34299, #17646 ),
 .UNSPECIFIED., .F., .F. ) 
 B_SPLINE_CURVE_WITH_KNOTS ( ( 3, 2, 2, 3 ),
 ( 0.8246268656716420065, 0.8258706467661693917, 0.8271144278606967770, 0.8283582089552240513 ),
 .UNSPECIFIED. ) 
 CURVE ( )  GEOMETRIC_REPRESENTATION_ITEM ( )  RATIONAL_B_SPLINE_CURVE ( ( 0.9999999999999761302, 0.8660254037844625774, 1.000000000000000000, 0.8660254037844387076, 1.000000000000000000, 0.8660254037844148378, 1.000000000000023981 ) ) 
 REPRESENTATION_ITEM ( '' )  );
#25782 = FACE_OUTER_BOUND ( 'NONE', #14215, .T. ) ;
#25783 = CARTESIAN_POINT ( 'NONE',  ( 5.405949406249999534, 9.363379034771803333, -169.2812500020484094 ) ) ;
#25784 = ORIENTED_EDGE ( 'NONE', *, *, #31748, .T. ) ;
#25785 = FACE_OUTER_BOUND ( 'NONE', #2075, .T. ) ;
#25786 = DIRECTION ( 'NONE',  ( 0.000000000000000000, 0.000000000000000000, -1.000000000000000000 ) ) ;
#25788 = EDGE_LOOP ( 'NONE', ( #34668, #34778, #35653, #5146 ) ) ;
#25787 = CARTESIAN_POINT ( 'NONE',  ( 10.81189881249999551, -6.242252689847874514, -69.15625000204839523 ) ) ;
#25789 = DIRECTION ( 'NONE',  ( 1.000000000000000000, 0.000000000000000000, 0.000000000000000000 ) ) ;
#25791 = ORIENTED_EDGE ( 'NONE', *, *, #9853, .T. ) ;
#25790 = CARTESIAN_POINT ( 'NONE',  ( -5.000000000000003553, -8.660254037844383745, -143.5000000000000000 ) ) ;
#25792 = ORIENTED_EDGE ( 'NONE', *, *, #2500, .F. ) ;
#25793 = CARTESIAN_POINT ( 'NONE',  ( 10.81189881249999551, -6.242252689847874514, -31.46875000204835260 ) ) ;
#25794 = LINE ( 'NONE', #20304, #14144 ) ;
#25795 = CARTESIAN_POINT ( 'NONE',  ( -5.405949406250003975, -9.363379034771801557, -5.031250002048376579 ) ) ;
#25797 = EDGE_LOOP ( 'NONE', ( #3024, #19965, #35461, #13328 ) ) ;
#25796 = CARTESIAN_POINT ( 'NONE',  ( -10.81189881249999729, 6.242252689847871849, -51.71875000204836681 ) ) ;
#25798 = CYLINDRICAL_SURFACE ( 'NONE', #3386, 9.999999999999998224 ) ;
#25799 = CARTESIAN_POINT ( 'NONE',  ( -10.00000000000000000, -5.773502691896251982, -28.12499999999998579 ) ) ;
#25800 = CARTESIAN_POINT ( 'NONE',  ( 10.81189881249999729, 0.000000000000000000, -188.8437500020483810 ) ) ;
#25801 = CARTESIAN_POINT ( 'NONE',  ( 10.81189881249999729, 0.000000000000000000, -167.8437500020484094 ) ) ;
#25802 = CARTESIAN_POINT ( 'NONE',  ( 10.81189881249999907, 6.242252689847868297, -155.7187500020483810 ) ) ;
#25803 = CARTESIAN_POINT ( 'NONE',  ( 7.644554776091147741E-16, 12.48450537969573659, -168.9687500020483810 ) ) ;
#25804 = CARTESIAN_POINT ( 'NONE',  ( -9.999999999999998224, 1.224646799147353059E-15, -124.2500000000000000 ) ) ;
#25805 = CARTESIAN_POINT ( 'NONE',  ( 4.999999999999992006, -8.660254037844389075, -24.74999999999996803 ) ) ;
#25806 = CARTESIAN_POINT ( 'NONE',  ( 7.070501591499377789E-16, 11.54700538379251284, -186.1250000000000000 ) ) ;
#25807 = CARTESIAN_POINT ( 'NONE',  ( -10.81189881249999729, 6.242252689847871849, -108.7187500020483810 ) ) ;
#25808 = CARTESIAN_POINT ( 'NONE',  ( -4.999999999999996447, 8.660254037844387298, -196.5000000000000000 ) ) ;
#25809 = CARTESIAN_POINT ( 'NONE',  ( 10.81189881249999729, 0.000000000000000000, -76.53125000204838102 ) ) ;
#25810 = CARTESIAN_POINT ( 'NONE',  ( 9.999999999999998224, 0.000000000000000000, -131.3750000040967905 ) ) ;
#25811 = CARTESIAN_POINT ( 'NONE',  ( 7.644554776091147741E-16, 12.48450537969573659, -87.96875000204838102 ) ) ;
#25812 = CARTESIAN_POINT ( 'NONE',  ( -5.405949406249996869, 9.363379034771805109, -64.03125000204836681 ) ) ;
#25813 = CARTESIAN_POINT ( 'NONE',  ( -9.999999999999998224, 1.224646799147353059E-15, -145.6250000040967905 ) ) ;
#25814 = CARTESIAN_POINT ( 'NONE',  ( -10.00000000000000000, -5.773502691896251982, -113.6249999999999858 ) ) ;
#25815 = EDGE_CURVE ( 'NONE', #39684, #26894, #38632, .T. ) ;
#25816 = ORIENTED_EDGE ( 'NONE', *, *, #30940, .F. ) ;
#25817 = CARTESIAN_POINT ( 'NONE',  ( 10.81189881249999551, -6.242252689847874514, -139.6562500020484094 ) ) ;
#25818 = CARTESIAN_POINT ( 'NONE',  ( 7.644554776091147741E-16, 12.48450537969573659, -154.1562500020484094 ) ) ;
#25819 = CARTESIAN_POINT ( 'NONE',  ( 10.81189881249999551, -6.242252689847874514, -193.6562500020484379 ) ) ;
#25820 = CARTESIAN_POINT ( 'NONE',  ( 9.999999999999479527, 5.773502691896553074, -105.3749999999999716 ) ) ;
#25821 = CARTESIAN_POINT ( 'NONE',  ( -10.81189881249999729, 1.324075727343319199E-15, -92.09375000204838102 ) ) ;
#25822 = ORIENTED_EDGE ( 'NONE', *, *, #40984, .T. ) ;
#25823 = CARTESIAN_POINT ( 'NONE',  ( 4.999999999999992006, -8.660254037844389075, -68.24999999999997158 ) ) ;
#25824 = CARTESIAN_POINT ( 'NONE',  ( -10.81189881249999729, 1.324075727343319199E-15, -189.5937500020483810 ) ) ;
#25825 = CARTESIAN_POINT ( 'NONE',  ( 10.00000000000000000, 5.773502691896255534, -71.25000000409676204 ) ) ;
#25826 = DIRECTION ( 'NONE',  ( -0.000000000000000000, -0.000000000000000000, 1.000000000000000000 ) ) ;
#25827 = CYLINDRICAL_SURFACE ( 'NONE', #35551, 9.999999999999998224 ) ;
#25828 = CARTESIAN_POINT ( 'NONE',  ( 5.405949406249992428, -9.363379034771808662, -85.78125000204838102 ) ) ;
#25829 = CARTESIAN_POINT ( 'NONE',  ( -2.293366432827344421E-15, -12.48450537969573659, -67.90625000204840944 ) ) ;
#25830 = CARTESIAN_POINT ( 'NONE',  ( 10.00000000000000000, 5.773502691896255534, -59.25000000409677625 ) ) ;
#25831 = CARTESIAN_POINT ( 'NONE',  ( 5.405949406249992428, -9.363379034771808662, -16.59375000204835260 ) ) ;
#25832 = VERTEX_POINT ( 'NONE', #11908 ) ;
#25833 = CARTESIAN_POINT ( 'NONE',  ( -10.81189881249999907, -6.242252689847864744, -197.1562500020484379 ) ) ;
#25834 = CARTESIAN_POINT ( 'NONE',  ( 5.405949406249992428, -9.363379034771808662, -12.28125000204835438 ) ) ;
#25835 = CARTESIAN_POINT ( 'NONE',  ( 5.405949406249992428, -9.363379034771808662, -6.093750002048370362 ) ) ;
#25836 = CARTESIAN_POINT ( 'NONE',  ( 4.999999999999992006, -8.660254037844389075, -110.6250000040967763 ) ) ;
#25837 = DIRECTION ( 'NONE',  ( -0.000000000000000000, -0.000000000000000000, -1.000000000000000000 ) ) ;
#25838 = CARTESIAN_POINT ( 'NONE',  ( -5.000000000000003553, -8.660254037844383745, -112.3750000040967763 ) ) ;
#25839 = CARTESIAN_POINT ( 'NONE',  ( -9.999999999999998224, 1.224646799147353059E-15, -176.7500000000000284 ) ) ;
#25840 = CARTESIAN_POINT ( 'NONE',  ( -10.00000000000000000, -5.773502691896252870, -169.5000000040967905 ) ) ;
#25842 = ORIENTED_EDGE ( 'NONE', *, *, #7454, .T. ) ;
#25841 = CARTESIAN_POINT ( 'NONE',  ( -10.81189881249999729, 6.242252689847871849, -99.90625000204838102 ) ) ;
#25843 = EDGE_CURVE ( 'NONE', #34451, #38572, #34575, .T. ) ;
#25844 = LINE ( 'NONE', #12863, #35895 ) ;
#25845 = ORIENTED_EDGE ( 'NONE', *, *, #30964, .F. ) ;
#25846 = ORIENTED_EDGE ( 'NONE', *, *, #1370, .F. ) ;
#25847 = EDGE_CURVE ( 'NONE', #5096, #1917, #16039, .T. ) ;
#25848 = CARTESIAN_POINT ( 'NONE',  ( -5.405949406249996869, 9.363379034771805109, -35.34375000204836681 ) ) ;
#25849 = VECTOR ( 'NONE', #23272, 1000.000000000000000 ) ;
#25850 = CARTESIAN_POINT ( 'NONE',  ( -10.81189881249999729, 6.242252689847871849, -27.90625000204838102 ) ) ;
#25851 = APPROVAL_ROLE ( '' ) ;
#25852 = CARTESIAN_POINT ( 'NONE',  ( -10.81189881249999729, 1.324075727343319199E-15, -77.09375000204838102 ) ) ;
#25853 = DIRECTION ( 'NONE',  ( -0.000000000000000000, -0.000000000000000000, -1.000000000000000000 ) ) ;
#25854 = CARTESIAN_POINT ( 'NONE',  ( 8.393774332151281214, 6.297795101496888925, -99.99999999999998579 ) ) ;
#25855 = CARTESIAN_POINT ( 'NONE',  ( -10.00000000000051337, 5.773502691895962435, -69.25000000409677625 ) ) ;
#25856 = CARTESIAN_POINT ( 'NONE',  ( 0.000000000000000000, 0.000000000000000000, -99.99999999999998579 ) ) ;
#25857 = CARTESIAN_POINT ( 'NONE',  ( 7.644554776091147741E-16, 12.48450537969573659, -158.6562500020484094 ) ) ;
#25858 = CARTESIAN_POINT ( 'NONE',  ( -10.00000000000000000, -5.773502691896251982, -15.00000000409676737 ) ) ;
#25859 = CARTESIAN_POINT ( 'NONE',  ( -9.999999999999998224, 1.224646799147353059E-15, -80.74999999999998579 ) ) ;
#25860 = CARTESIAN_POINT ( 'NONE',  ( -5.405949406250003975, -9.363379034771801557, -126.3437500020483952 ) ) ;
#25861 = CARTESIAN_POINT ( 'NONE',  ( -10.81189881249999729, 1.324075727343319199E-15, -98.28125000204839523 ) ) ;
#25862 = CARTESIAN_POINT ( 'NONE',  ( 5.405949406249999534, 9.363379034771803333, -112.0937500020483810 ) ) ;
#25863 = CARTESIAN_POINT ( 'NONE',  ( 5.405949406249992428, -9.363379034771808662, -79.59375000204838102 ) ) ;
#25864 = AXIS2_PLACEMENT_3D ( 'NONE', #967, #20580, #7012 ) ;
#25865 = CARTESIAN_POINT ( 'NONE',  ( 7.644554776091147741E-16, 12.48450537969573659, -80.65625000204839523 ) ) ;
#25866 = CARTESIAN_POINT ( 'NONE',  ( -10.00000000000000000, -5.773502691896251982, -166.5000000040967905 ) ) ;
#25867 = CARTESIAN_POINT ( 'NONE',  ( -4.999999999999996447, 8.660254037844387298, -81.37500000409677625 ) ) ;
#25868 = CARTESIAN_POINT ( 'NONE',  ( -5.405949406250003975, -9.363379034771801557, -168.5312500020484094 ) ) ;
#25869 = CARTESIAN_POINT ( 'NONE',  ( 10.81189881249999729, 0.000000000000000000, -181.5312500020483810 ) ) ;
#25870 = CARTESIAN_POINT ( 'NONE',  ( 10.00000000000000000, 5.773502691896255534, -152.2500000040967620 ) ) ;
#25871 = LINE ( 'NONE', #9462, #852 ) ;
#25872 = CARTESIAN_POINT ( 'NONE',  ( -10.81189881249999729, 1.324075727343319199E-15, -8.093750002048343717 ) ) ;
#25873 = CARTESIAN_POINT ( 'NONE',  ( 9.999999999999998224, 0.000000000000000000, -162.5000000000000000 ) ) ;
#25874 = CARTESIAN_POINT ( 'NONE',  ( -5.405949406249996869, 9.363379034771805109, -113.3437500020483810 ) ) ;
#25875 = ADVANCED_FACE ( 'NONE', ( #41476 ), #1798, .T. ) ;
#25876 = CARTESIAN_POINT ( 'NONE',  ( -9.999999999999998224, 5.773502691896259087, -88.37499999999998579 ) ) ;
#25877 = CARTESIAN_POINT ( 'NONE',  ( -5.405949406249996869, 9.363379034771805109, -11.53125000204835438 ) ) ;
#25878 = CARTESIAN_POINT ( 'NONE',  ( -4.999999999999996447, 8.660254037844387298, -97.87500000409677625 ) ) ;
#25879 = CARTESIAN_POINT ( 'NONE',  ( -2.121150477449813534E-15, -11.54700538379251284, -170.7500000040968189 ) ) ;
#25880 = CARTESIAN_POINT ( 'NONE',  ( 10.81189881249999729, 0.000000000000000000, -106.5312500020483810 ) ) ;
#25881 = CARTESIAN_POINT ( 'NONE',  ( 5.405949406249999534, 9.363379034771803333, -92.78125000204838102 ) ) ;
#25882 = ORIENTED_EDGE ( 'NONE', *, *, #15907, .T. ) ;
#25883 = CIRCLE ( 'NONE', #23810, 9.999999999999998224 ) ;
#25884 = CARTESIAN_POINT ( 'NONE',  ( -10.00000000000000000, -5.773502691896251982, -82.50000000409677625 ) ) ;
#25885 = CARTESIAN_POINT ( 'NONE',  ( -10.81189881249999729, 1.324075727343319199E-15, -42.59375000204837391 ) ) ;
#25886 = ORIENTED_EDGE ( 'NONE', *, *, #15852, .F. ) ;
#25887 = CARTESIAN_POINT ( 'NONE',  ( 9.999999999999996447, -5.773502691896262640, -17.12499999999997158 ) ) ;
#25888 = CARTESIAN_POINT ( 'NONE',  ( 5.000000000000000000, 8.660254037844385522, -156.2500000000000000 ) ) ;
#25889 = CARTESIAN_POINT ( 'NONE',  ( -2.121150477449813534E-15, -11.54700538379251284, -20.75000000409676915 ) ) ;
#25890 = CARTESIAN_POINT ( 'NONE',  ( 9.999999999999998224, 0.000000000000000000, -84.49999999999997158 ) ) ;
#25892 = ORIENTED_EDGE ( 'NONE', *, *, #18751, .F. ) ;
#25891 = CARTESIAN_POINT ( 'NONE',  ( -10.81189881249999907, -6.242252689847864744, -128.1562500020483810 ) ) ;
#25893 = CARTESIAN_POINT ( 'NONE',  ( -2.121150477449813534E-15, -11.54700538379251284, -21.87499999999997513 ) ) ;
#25894 = EDGE_LOOP ( 'NONE', ( #32902, #28883, #15625, #8094 ) ) ;
#25895 =( BOUNDED_CURVE ( )  B_SPLINE_CURVE ( 2, ( #18930, #39201, #41587, #12019, #5988, #38565, #32324 ),
 .UNSPECIFIED., .F., .F. ) 
 B_SPLINE_CURVE_WITH_KNOTS ( ( 3, 2, 2, 3 ),
 ( 0.3059701492537313383, 0.3072139303482587791, 0.3084577114427861644, 0.3097014925373136052 ),
 .UNSPECIFIED. ) 
 CURVE ( )  GEOMETRIC_REPRESENTATION_ITEM ( )  RATIONAL_B_SPLINE_CURVE ( ( 1.000000000000000000, 0.8660254037844387076, 1.000000000000000000, 0.8660254037844387076, 1.000000000000000000, 0.8660254037844207220, 1.000000000000017986 ) ) 
 REPRESENTATION_ITEM ( '' )  );
#25896 = CARTESIAN_POINT ( 'NONE',  ( -10.81189881249999729, 1.324075727343319199E-15, -54.78125000204836681 ) ) ;
#25897 = COORDINATED_UNIVERSAL_TIME_OFFSET ( 6, 0, .AHEAD. ) ;
#25898 = CARTESIAN_POINT ( 'NONE',  ( 10.81189881249999907, 6.242252689847868297, -101.7187500020483810 ) ) ;
#25900 = VERTEX_POINT ( 'NONE', #5030 ) ;
#25899 = ORIENTED_EDGE ( 'NONE', *, *, #35462, .T. ) ;
#25901 = AXIS2_PLACEMENT_3D ( 'NONE', #9996, #10420, #33329 ) ;
#25902 = FACE_OUTER_BOUND ( 'NONE', #1259, .T. ) ;
#25903 = CARTESIAN_POINT ( 'NONE',  ( -4.999999999999996447, 8.660254037844387298, -77.99999999999998579 ) ) ;
#25904 =( BOUNDED_CURVE ( )  B_SPLINE_CURVE ( 2, ( #23418, #36359, #13879, #36781, #33136, #40218, #13247 ),
 .UNSPECIFIED., .F., .F. ) 
 B_SPLINE_CURVE_WITH_KNOTS ( ( 3, 2, 2, 3 ),
 ( 0.3059701492537313383, 0.3072139303482587791, 0.3084577114427861644, 0.3097014925373136052 ),
 .UNSPECIFIED. ) 
 CURVE ( )  GEOMETRIC_REPRESENTATION_ITEM ( )  RATIONAL_B_SPLINE_CURVE ( ( 1.000000000000000000, 0.8660254037844387076, 1.000000000000000000, 0.8660254037844387076, 1.000000000000000000, 0.8660254037844207220, 1.000000000000017986 ) ) 
 REPRESENTATION_ITEM ( '' )  );
#25905 = CARTESIAN_POINT ( 'NONE',  ( 5.405949406249992428, -9.363379034771808662, -183.2812500020484094 ) ) ;
#25906 = CARTESIAN_POINT ( 'NONE',  ( -4.999999999999996447, 8.660254037844387298, -175.5000000000000284 ) ) ;
#25907 = CARTESIAN_POINT ( 'NONE',  ( 0.000000000000000000, 0.000000000000000000, -200.0000000000000000 ) ) ;
#25908 = CARTESIAN_POINT ( 'NONE',  ( 10.81189881249999729, 6.242252689847867408, -137.7187500020483810 ) ) ;
#25909 = CARTESIAN_POINT ( 'NONE',  ( -2.293366432827344421E-15, -12.48450537969573659, -100.7187500020483952 ) ) ;
#25910 = CYLINDRICAL_SURFACE ( 'NONE', #6351, 9.999999999999998224 ) ;
#25911 = CARTESIAN_POINT ( 'NONE',  ( -10.81189881249999729, 6.242252689847871849, -105.9062500020483810 ) ) ;
#25912 = CARTESIAN_POINT ( 'NONE',  ( -2.121150477449813534E-15, -11.54700538379251284, -190.2500000040967905 ) ) ;
#25913 = CARTESIAN_POINT ( 'NONE',  ( 7.644554776091147741E-16, 12.48450537969573659, -110.4687500020483668 ) ) ;
#25914 = CARTESIAN_POINT ( 'NONE',  ( 10.81189881249999729, 6.242252689847867408, -184.4062500020484094 ) ) ;
#25915 = CARTESIAN_POINT ( 'NONE',  ( 10.00000000000051159, -5.773502691895965988, -95.12499999999997158 ) ) ;
#25916 = CARTESIAN_POINT ( 'NONE',  ( 9.999999999999998224, 0.000000000000000000, -143.0000000000000000 ) ) ;
#25917 = CARTESIAN_POINT ( 'NONE',  ( -9.999999999999998224, 1.224646799147353059E-15, -5.749999999999976907 ) ) ;
#25918 = EDGE_CURVE ( 'NONE', #42281, #15678, #2011, .T. ) ;
#25919 = CARTESIAN_POINT ( 'NONE',  ( 10.81189881249999729, 6.242252689847867408, -67.21875000204838102 ) ) ;
#25920 = CARTESIAN_POINT ( 'NONE',  ( 10.81189881249999907, 6.242252689847868297, -49.21875000204835260 ) ) ;
#25921 = CARTESIAN_POINT ( 'NONE',  ( -2.121150477449813534E-15, -11.54700538379251284, -176.7500000040967620 ) ) ;
#25922 = CARTESIAN_POINT ( 'NONE',  ( 5.405949406249999534, 9.363379034771803333, -29.78125000204837036 ) ) ;
#25923 = CARTESIAN_POINT ( 'NONE',  ( 5.405949406249999534, 9.363379034771803333, -32.59375000204836681 ) ) ;
#25924 = CARTESIAN_POINT ( 'NONE',  ( 7.070501591499376803E-16, 11.54700538379251284, -27.50000000409677980 ) ) ;
#25925 = CARTESIAN_POINT ( 'NONE',  ( 5.405949406249999534, 9.363379034771803333, -134.5937500020483810 ) ) ;
#25926 = EDGE_CURVE ( 'NONE', #39297, #33849, #27914, .T. ) ;
#25927 = CARTESIAN_POINT ( 'NONE',  ( 4.999999999999992006, -8.660254037844389075, -116.2499999999999858 ) ) ;
#25928 = CARTESIAN_POINT ( 'NONE',  ( 4.999999999999992006, -8.660254037844389075, -114.7499999999999858 ) ) ;
#25929 = EDGE_CURVE ( 'NONE', #6727, #38512, #4217, .T. ) ;
#25930 = AXIS2_PLACEMENT_3D ( 'NONE', #18995, #31760, #28937 ) ;
#25931 = CARTESIAN_POINT ( 'NONE',  ( 10.00000000000000000, 5.773502691896255534, -66.37499999999998579 ) ) ;
#25932 = CARTESIAN_POINT ( 'NONE',  ( -10.81189881249999907, -6.242252689847864744, -135.6562500020484094 ) ) ;
#25933 = CARTESIAN_POINT ( 'NONE',  ( -5.405949406250003975, -9.363379034771801557, -117.5312500020483952 ) ) ;
#25934 = EDGE_LOOP ( 'NONE', ( #5274, #36397, #3474, #39991 ) ) ;
#25935 = CARTESIAN_POINT ( 'NONE',  ( -4.999999999999996447, 8.660254037844387298, -120.3750000040967905 ) ) ;
#25936 = CARTESIAN_POINT ( 'NONE',  ( 9.999999999999996447, -5.773502691896262640, -104.5000000040967763 ) ) ;
#25937 = PLANE ( 'NONE',  #20145 ) ;
#25938 = CARTESIAN_POINT ( 'NONE',  ( 10.81189881249999551, -6.242252689847874514, -64.46875000204838102 ) ) ;
#25939 = ORIENTED_EDGE ( 'NONE', *, *, #36120, .T. ) ;
#25940 = CARTESIAN_POINT ( 'NONE',  ( -10.00000000000000000, -5.773502691896251982, -43.12499999999997868 ) ) ;
#25941 = CARTESIAN_POINT ( 'NONE',  ( 4.999999999999992006, -8.660254037844389075, -16.12500000409675138 ) ) ;
#25942 = CARTESIAN_POINT ( 'NONE',  ( 10.81189881249999729, 6.242252689847867408, -43.40625000204837391 ) ) ;
#25943 = DIRECTION ( 'NONE',  ( -0.000000000000000000, -0.000000000000000000, 1.000000000000000000 ) ) ;
#25944 = CARTESIAN_POINT ( 'NONE',  ( -9.999999999999998224, 1.224646799147353059E-15, -45.12500000409677625 ) ) ;
#25945 = CARTESIAN_POINT ( 'NONE',  ( -10.81189881249999729, 6.242252689847871849, -32.40625000204835970 ) ) ;
#25946 = CARTESIAN_POINT ( 'NONE',  ( -4.999999999999996447, 8.660254037844387298, -156.3750000040967905 ) ) ;
#25947 = CARTESIAN_POINT ( 'NONE',  ( 10.81189881249999551, -6.242252689847874514, -141.1562500020484094 ) ) ;
#25948 = CARTESIAN_POINT ( 'NONE',  ( -10.81189881249999907, -6.242252689847864744, -146.1562500020484094 ) ) ;
#25949 = EDGE_CURVE ( 'NONE', #23986, #35200, #13270, .T. ) ;
#25950 = CARTESIAN_POINT ( 'NONE',  ( 4.999999999999992006, -8.660254037844389075, -110.2499999999999858 ) ) ;
#25951 = ORIENTED_EDGE ( 'NONE', *, *, #14883, .T. ) ;
#25952 = EDGE_LOOP ( 'NONE', ( #4081, #7575, #37234, #16468 ) ) ;
#25953 = ORIENTED_EDGE ( 'NONE', *, *, #1153, .F. ) ;
#25954 = EDGE_CURVE ( 'NONE', #3545, #1841, #11694, .T. ) ;
#25955 = AXIS2_PLACEMENT_3D ( 'NONE', #18472, #28205, #17822 ) ;
#25956 = CARTESIAN_POINT ( 'NONE',  ( 10.00000000000102318, -5.773502691895667560, -104.1249999999999432 ) ) ;
#25957 = CARTESIAN_POINT ( 'NONE',  ( 10.81189881249999907, 6.242252689847868297, -173.7187500020484094 ) ) ;
#25958 = CARTESIAN_POINT ( 'NONE',  ( -10.81189881249999907, -6.242252689847864744, -19.96875000204838102 ) ) ;
#25959 = CARTESIAN_POINT ( 'NONE',  ( 9.999999999999998224, 0.000000000000000000, -60.87500000409676204 ) ) ;
#25960 = CARTESIAN_POINT ( 'NONE',  ( -10.81189881249999729, 1.324075727343319199E-15, -162.5937500020484094 ) ) ;
#25961 = CARTESIAN_POINT ( 'NONE',  ( -2.293366432827344421E-15, -12.48450537969573659, -144.2187500020483810 ) ) ;
#25962 = CARTESIAN_POINT ( 'NONE',  ( 8.614196012143711556, -6.533971456633876684, 2.775557561562891351E-14 ) ) ;
#25963 = CARTESIAN_POINT ( 'NONE',  ( 10.81189881249999729, 0.000000000000000000, -124.3437500020483952 ) ) ;
#25964 = CARTESIAN_POINT ( 'NONE',  ( -10.81189881249999729, 1.324075727343319199E-15, -131.2812500020483810 ) ) ;
#25965 = CARTESIAN_POINT ( 'NONE',  ( -5.405949406250003975, -9.363379034771801557, -15.34375000204835082 ) ) ;
#25966 = CARTESIAN_POINT ( 'NONE',  ( -10.81189881249999729, -6.242252689847864744, -147.4687500020484094 ) ) ;
#25967 = CARTESIAN_POINT ( 'NONE',  ( 9.046166897582494926, -5.964473731795716382, -179.9999999999999716 ) ) ;
#25968 = CARTESIAN_POINT ( 'NONE',  ( -9.999999999999998224, 1.224646799147353059E-15, -25.24999999999996803 ) ) ;
#25969 = CARTESIAN_POINT ( 'NONE',  ( 9.999999999999996447, -5.773502691896262640, -162.6250000000000284 ) ) ;
#25970 = CARTESIAN_POINT ( 'NONE',  ( 10.81189881249999907, 6.242252689847868297, 0.09374999795164208616 ) ) ;
#25971 = CARTESIAN_POINT ( 'NONE',  ( 10.81189881249999907, 6.242252689847868297, -76.21875000204836681 ) ) ;
#25972 = CARTESIAN_POINT ( 'NONE',  ( 7.644554776091147741E-16, 12.48450537969573659, -47.65625000204836681 ) ) ;
#25973 = CARTESIAN_POINT ( 'NONE',  ( 5.405949406249999534, 9.363379034771803333, -52.09375000204835260 ) ) ;
#25974 = FACE_OUTER_BOUND ( 'NONE', #37565, .T. ) ;
#25975 = CARTESIAN_POINT ( 'NONE',  ( 5.405949406249999534, 9.363379034771803333, -158.5937500020483810 ) ) ;
#25976 = CARTESIAN_POINT ( 'NONE',  ( 10.00000000000000000, 5.773502691896255534, -141.3750000000000000 ) ) ;
#25977 = CARTESIAN_POINT ( 'NONE',  ( -5.405949406250003975, -9.363379034771801557, -141.5312500020483810 ) ) ;
#25978 = CYLINDRICAL_SURFACE ( 'NONE', #1372, 9.999999999999998224 ) ;
#25979 = CARTESIAN_POINT ( 'NONE',  ( 9.999999999999996447, -5.773502691896262640, -110.5000000040967763 ) ) ;
#25980 = CARTESIAN_POINT ( 'NONE',  ( 4.999999999999992006, -8.660254037844389075, -93.74999999999998579 ) ) ;
#25981 = EDGE_CURVE ( 'NONE', #41327, #36343, #10504, .T. ) ;
#25982 = ORIENTED_EDGE ( 'NONE', *, *, #18927, .F. ) ;
#25983 = CARTESIAN_POINT ( 'NONE',  ( -10.81189881249999729, 1.324075727343319199E-15, -117.7812500020483952 ) ) ;
#25984 = CARTESIAN_POINT ( 'NONE',  ( -2.121150477449813534E-15, -11.54700538379251284, -137.7500000040967905 ) ) ;
#25985 = CARTESIAN_POINT ( 'NONE',  ( 0.000000000000000000, 0.000000000000000000, -200.0000000000000000 ) ) ;
#25986 = EDGE_CURVE ( 'NONE', #31643, #6545, #1581, .T. ) ;
#25987 = CARTESIAN_POINT ( 'NONE',  ( -5.405949406250003975, -9.363379034771801557, -173.0312500020484094 ) ) ;
#25988 = CARTESIAN_POINT ( 'NONE',  ( 10.00000000000000000, 5.773502691896255534, -50.25000000409675494 ) ) ;
#25989 =( BOUNDED_CURVE ( )  B_SPLINE_CURVE ( 2, ( #34035, #27983, #4245, #31232, #27124, #1230, #14577 ),
 .UNSPECIFIED., .F., .F. ) 
 B_SPLINE_CURVE_WITH_KNOTS ( ( 3, 2, 2, 3 ),
 ( 0.2910447761194031036, 0.2922885572139304333, 0.2935323383084578186, 0.2947761194029852039 ),
 .UNSPECIFIED. ) 
 CURVE ( )  GEOMETRIC_REPRESENTATION_ITEM ( )  RATIONAL_B_SPLINE_CURVE ( ( 0.9999999999999880096, 0.8660254037844506980, 1.000000000000000000, 0.8660254037844387076, 1.000000000000000000, 0.8660254037844267172, 1.000000000000011990 ) ) 
 REPRESENTATION_ITEM ( '' )  );
#25990 = CARTESIAN_POINT ( 'NONE',  ( -9.999999999999479527, -5.773502691896549521, -91.50000000409676204 ) ) ;
#25991 = CARTESIAN_POINT ( 'NONE',  ( -10.81189881249999729, 1.324075727343319199E-15, -59.28125000204836681 ) ) ;
#25992 = SECURITY_CLASSIFICATION ( '', '', #10485 ) ;
#25993 = LINE ( 'NONE', #39143, #12435 ) ;
#25994 = CARTESIAN_POINT ( 'NONE',  ( -10.81189881249999907, -6.242252689847864744, -158.1562500020484094 ) ) ;
#25995 = CARTESIAN_POINT ( 'NONE',  ( -10.81189881249999729, 6.242252689847871849, -141.7187500020483810 ) ) ;
#25996 = CARTESIAN_POINT ( 'NONE',  ( 9.999999999999998224, 0.000000000000000000, -50.37500000409675494 ) ) ;
#25997 = FACE_OUTER_BOUND ( 'NONE', #8546, .T. ) ;
#25998 = VERTEX_POINT ( 'NONE', #32007 ) ;
#25999 = EDGE_CURVE ( 'NONE', #32995, #3335, #13859, .T. ) ;
#26001 = ORIENTED_EDGE ( 'NONE', *, *, #34409, .F. ) ;
#26000 = CARTESIAN_POINT ( 'NONE',  ( 5.405949406249999534, 9.363379034771803333, -71.78125000204838102 ) ) ;
#26002 = COORDINATED_UNIVERSAL_TIME_OFFSET ( 6, 0, .AHEAD. ) ;
#26004 = ORIENTED_EDGE ( 'NONE', *, *, #3396, .T. ) ;
#26003 = CARTESIAN_POINT ( 'NONE',  ( -2.293366432827344421E-15, -12.48450537969573659, -123.2187500020483952 ) ) ;
#26005 = ORIENTED_EDGE ( 'NONE', *, *, #4875, .T. ) ;
#26006 = CARTESIAN_POINT ( 'NONE',  ( -5.405949406250003975, -9.363379034771801557, -27.34375000204835970 ) ) ;
#26007 = CARTESIAN_POINT ( 'NONE',  ( 9.999999999999742428, 5.773502691896404748, -159.3749999999999716 ) ) ;
#26008 = CARTESIAN_POINT ( 'NONE',  ( 10.81189881249999551, -6.242252689847874514, -194.9687500020484094 ) ) ;
#26009 = CARTESIAN_POINT ( 'NONE',  ( 10.81189881249999729, 0.000000000000000000, -53.84375000204835970 ) ) ;
#26010 = CARTESIAN_POINT ( 'NONE',  ( 7.070501591499377789E-16, 11.54700538379251284, -31.62499999999995737 ) ) ;
#26011 = CARTESIAN_POINT ( 'NONE',  ( 10.81189881249999729, 6.242252689847867408, -191.7187500020484094 ) ) ;
#26012 = CARTESIAN_POINT ( 'NONE',  ( 10.81189881249999907, 6.242252689847868297, -172.2187500020483810 ) ) ;
#26013 = CARTESIAN_POINT ( 'NONE',  ( 7.644554776091147741E-16, 12.48450537969573659, -149.4687500020484094 ) ) ;
#26014 = CARTESIAN_POINT ( 'NONE',  ( 10.81189881249999729, 0.000000000000000000, -172.3437500020484094 ) ) ;
#26015 = DIRECTION ( 'NONE',  ( -0.000000000000000000, -0.000000000000000000, 1.000000000000000000 ) ) ;
#26016 = CARTESIAN_POINT ( 'NONE',  ( 9.999999999999998224, 0.000000000000000000, -20.37500000409675494 ) ) ;
#26017 = CARTESIAN_POINT ( 'NONE',  ( 5.000000000000000000, 8.660254037844385522, -190.7500000000000000 ) ) ;
#26018 = CARTESIAN_POINT ( 'NONE',  ( 10.81189881249999551, -6.242252689847874514, -95.96875000204838102 ) ) ;
#26019 = CARTESIAN_POINT ( 'NONE',  ( -10.00000000000154188, 5.773502691895366468, -17.87499999999993250 ) ) ;
#26020 = CARTESIAN_POINT ( 'NONE',  ( 10.81189881249999907, 6.242252689847868297, -73.40625000204836681 ) ) ;
#26021 = DIRECTION ( 'NONE',  ( -0.000000000000000000, -0.000000000000000000, -1.000000000000000000 ) ) ;
#26022 = CARTESIAN_POINT ( 'NONE',  ( -5.405949406250003975, -9.363379034771801557, -186.3437500020483810 ) ) ;
#26023 = CARTESIAN_POINT ( 'NONE',  ( 5.405949406249992428, -9.363379034771808662, -82.59375000204836681 ) ) ;
#26024 = CARTESIAN_POINT ( 'NONE',  ( -10.81189881249999729, 6.242252689847871849, -57.90625000204838813 ) ) ;
#26025 = CARTESIAN_POINT ( 'NONE',  ( 9.999999999999998224, 0.000000000000000000, -146.3750000040967905 ) ) ;
#26026 = CARTESIAN_POINT ( 'NONE',  ( 4.999999999999992006, -8.660254037844389075, -116.2499999999999858 ) ) ;
#26027 =( BOUNDED_CURVE ( )  B_SPLINE_CURVE ( 2, ( #27600, #10381, #37306, #5153, #18304, #11394, #34081 ),
 .UNSPECIFIED., .F., .F. ) 
 B_SPLINE_CURVE_WITH_KNOTS ( ( 3, 2, 2, 3 ),
 ( 0.2089552238805970630, 0.2101990049751244205, 0.2114427860696518058, 0.2126865671641791633 ),
 .UNSPECIFIED. ) 
 CURVE ( )  GEOMETRIC_REPRESENTATION_ITEM ( )  RATIONAL_B_SPLINE_CURVE ( ( 0.9999999999999940048, 0.8660254037844447028, 1.000000000000000000, 0.8660254037844387076, 1.000000000000000000, 0.8660254037844327124, 1.000000000000005995 ) ) 
 REPRESENTATION_ITEM ( '' )  );
#26028 = ORIENTED_EDGE ( 'NONE', *, *, #31921, .T. ) ;
#26029 = CARTESIAN_POINT ( 'NONE',  ( -5.405949406249996869, 9.363379034771805109, -145.0312500020483810 ) ) ;
#26030 = CARTESIAN_POINT ( 'NONE',  ( -5.405949406250003975, -9.363379034771801557, -159.5312500020484094 ) ) ;
#26031 = CARTESIAN_POINT ( 'NONE',  ( 0.000000000000000000, 0.000000000000000000, -200.0000000000000000 ) ) ;
#26032 = CARTESIAN_POINT ( 'NONE',  ( 4.999999999999992006, -8.660254037844389075, -38.24999999999997868 ) ) ;
#26033 = CARTESIAN_POINT ( 'NONE',  ( -10.81189881249999729, 6.242252689847871849, -87.71875000204838102 ) ) ;
#26034 = VECTOR ( 'NONE', #38380, 1000.000000000000000 ) ;
#26035 = VERTEX_POINT ( 'NONE', #12330 ) ;
#26036 = CARTESIAN_POINT ( 'NONE',  ( 5.000000000000000000, 8.660254037844385522, -60.24999999999997158 ) ) ;
#26037 = CARTESIAN_POINT ( 'NONE',  ( -5.405949406249996869, 9.363379034771805109, -189.8437500020483810 ) ) ;
#26038 = CARTESIAN_POINT ( 'NONE',  ( 7.070501591499377789E-16, 11.54700538379251284, -77.00000000409677625 ) ) ;
#26039 = CARTESIAN_POINT ( 'NONE',  ( -2.121150477449813534E-15, -11.54700538379251284, -169.2500000040968189 ) ) ;
#26040 = CARTESIAN_POINT ( 'NONE',  ( 7.071067811865472841, 7.071067811865472841, -200.0000000000000000 ) ) ;
#26041 = CARTESIAN_POINT ( 'NONE',  ( -5.405949406249996869, 9.363379034771805109, -88.03125000204838102 ) ) ;
#26042 = CARTESIAN_POINT ( 'NONE',  ( -10.81189881249999729, -6.242252689847864744, -66.65625000204839523 ) ) ;
#26043 = CARTESIAN_POINT ( 'NONE',  ( -4.999999999999996447, 8.660254037844387298, -57.37500000409676204 ) ) ;
#26044 = CARTESIAN_POINT ( 'NONE',  ( 7.644554776091147741E-16, 12.48450537969573659, -20.46875000204837036 ) ) ;
#26045 = CARTESIAN_POINT ( 'NONE',  ( -9.999999999999742428, -5.773502691896402084, -151.5000000040967620 ) ) ;
#26046 = CARTESIAN_POINT ( 'NONE',  ( 10.81189881249999729, 0.000000000000000000, -181.5312500020483810 ) ) ;
#26047 = ADVANCED_FACE ( 'NONE', ( #5672 ), #6092, .F. ) ;
#26048 = CARTESIAN_POINT ( 'NONE',  ( 10.81189881249999907, 6.242252689847868297, -13.40625000204837036 ) ) ;
#26049 = CARTESIAN_POINT ( 'NONE',  ( 9.999999999998969713, 5.773502691896851502, -79.87499999999997158 ) ) ;
#26050 = CARTESIAN_POINT ( 'NONE',  ( -9.999999999999998224, 1.224646799147353059E-15, -200.0000000000000000 ) ) ;
#26051 = CARTESIAN_POINT ( 'NONE',  ( -9.999999999999998224, 1.836970198721029589E-15, 0.000000000000000000 ) ) ;
#26052 = CARTESIAN_POINT ( 'NONE',  ( 9.999999999999998224, 0.000000000000000000, -200.0000000000000000 ) ) ;
#26053 = CARTESIAN_POINT ( 'NONE',  ( 7.070501591499377789E-16, 11.54700538379251284, -177.1250000000000000 ) ) ;
#26054 = CARTESIAN_POINT ( 'NONE',  ( 9.999999999999998224, 0.000000000000000000, -114.4999999999999858 ) ) ;
#26056 = VERTEX_POINT ( 'NONE', #2852 ) ;
#26055 = CARTESIAN_POINT ( 'NONE',  ( -5.405949406249996869, 9.363379034771805109, -94.03125000204838102 ) ) ;
#26057 = CARTESIAN_POINT ( 'NONE',  ( -10.00000000000076916, 5.773502691895813221, -106.7500000040967620 ) ) ;
#26058 = EDGE_LOOP ( 'NONE', ( #12179, #23758, #11471, #15206 ) ) ;
#26059 = VERTEX_POINT ( 'NONE', #22701 ) ;
#26060 = EDGE_CURVE ( 'NONE', #12598, #12994, #320, .T. ) ;
#26061 = CARTESIAN_POINT ( 'NONE',  ( 5.405949406249999534, 9.363379034771803333, -35.59375000204836681 ) ) ;
#26062 = CARTESIAN_POINT ( 'NONE',  ( -2.293366432827344421E-15, -12.48450537969573659, -18.40625000204837036 ) ) ;
#26063 = PERSON_AND_ORGANIZATION_ROLE ( 'classification_officer' ) ;
#26064 = CARTESIAN_POINT ( 'NONE',  ( -10.81189881249999907, -6.242252689847864744, -76.96875000204836681 ) ) ;
#26065 = CARTESIAN_POINT ( 'NONE',  ( 9.999999999999998224, 0.000000000000000000, -105.4999999999999858 ) ) ;
#26066 = AXIS2_PLACEMENT_3D ( 'NONE', #23407, #7002, #32697 ) ;
#26067 = CARTESIAN_POINT ( 'NONE',  ( -10.81189881249999729, 6.242252689847871849, -191.2187500020484663 ) ) ;
#26068 = CARTESIAN_POINT ( 'NONE',  ( 7.070501591499376803E-16, 11.54700538379251284, -69.50000000409679046 ) ) ;
#26069 = CARTESIAN_POINT ( 'NONE',  ( 10.00000000000051159, -5.773502691895965988, -143.5000000040967905 ) ) ;
#26070 = CARTESIAN_POINT ( 'NONE',  ( 10.81189881249999551, -6.242252689847874514, -157.6562500020484094 ) ) ;
#26071 = CARTESIAN_POINT ( 'NONE',  ( 5.000000000000000000, 8.660254037844385522, -0.6250000040967651493 ) ) ;
#26072 = CARTESIAN_POINT ( 'NONE',  ( -9.999999999999998224, 1.224646799147353059E-15, -103.6250000040967763 ) ) ;
#26073 = CARTESIAN_POINT ( 'NONE',  ( 10.81189881249999907, 6.242252689847868297, -125.7187500020483810 ) ) ;
#26074 = CARTESIAN_POINT ( 'NONE',  ( -2.293366432827344421E-15, -12.48450537969573659, -100.9062500020483952 ) ) ;
#26075 = CARTESIAN_POINT ( 'NONE',  ( 5.405949406249999534, 9.363379034771803333, -107.5937500020483810 ) ) ;
#26076 = CARTESIAN_POINT ( 'NONE',  ( -10.81189881249999729, 1.324075727343319199E-15, -80.09375000204838102 ) ) ;
#26077 = CARTESIAN_POINT ( 'NONE',  ( 5.405949406249999534, 9.363379034771803333, -82.28125000204838102 ) ) ;
#26078 = CARTESIAN_POINT ( 'NONE',  ( 9.999999999999996447, -5.773502691896262640, -172.0000000040967905 ) ) ;
#26079 = CARTESIAN_POINT ( 'NONE',  ( -9.183694056713487929E-15, -20.00000000000000355, 12.49999999999999112 ) ) ;
#26080 = CARTESIAN_POINT ( 'NONE',  ( -5.405949406250003975, -9.363379034771801557, -164.0312500020484094 ) ) ;
#26081 = CARTESIAN_POINT ( 'NONE',  ( 7.644554776091147741E-16, 12.48450537969573659, -181.1562500020484094 ) ) ;
#26082 = CARTESIAN_POINT ( 'NONE',  ( 4.999999999999992006, -8.660254037844389075, -157.1250000040967905 ) ) ;
#26083 = FACE_OUTER_BOUND ( 'NONE', #11174, .T. ) ;
#26084 = CARTESIAN_POINT ( 'NONE',  ( 10.81189881249999907, 6.242252689847868297, -7.218750002048357040 ) ) ;
#26085 = DIRECTION ( 'NONE',  ( 1.000000000000000000, 0.000000000000000000, 0.000000000000000000 ) ) ;
#26086 = CARTESIAN_POINT ( 'NONE',  ( 7.644554776091147741E-16, 12.48450537969573659, -116.4687500020483952 ) ) ;
#26087 = CARTESIAN_POINT ( 'NONE',  ( -9.999999999999998224, 5.773502691896259087, -85.37499999999997158 ) ) ;
#26088 = CARTESIAN_POINT ( 'NONE',  ( 7.644554776091147741E-16, 12.48450537969573659, -14.65625000204837214 ) ) ;
#26089 = CARTESIAN_POINT ( 'NONE',  ( -5.000000000000003553, -8.660254037844383745, -95.87500000409677625 ) ) ;
#26090 = CARTESIAN_POINT ( 'NONE',  ( 4.999999999999992006, -8.660254037844389075, -170.6250000040968189 ) ) ;
#26091 = CARTESIAN_POINT ( 'NONE',  ( 5.405949406249999534, 9.363379034771803333, -106.2812500020483810 ) ) ;
#26092 = CARTESIAN_POINT ( 'NONE',  ( -10.81189881249999729, 6.242252689847871849, -92.40625000204838102 ) ) ;
#26093 = VERTEX_POINT ( 'NONE', #22281 ) ;
#26094 = EDGE_CURVE ( 'NONE', #1002, #31616, #22920, .T. ) ;
#26095 = CARTESIAN_POINT ( 'NONE',  ( 4.999999999999992006, -8.660254037844389075, -85.12500000409677625 ) ) ;
#26096 = CARTESIAN_POINT ( 'NONE',  ( 9.999999999999998224, 1.224646799147353059E-15, -99.99999999999998579 ) ) ;
#26097 = CARTESIAN_POINT ( 'NONE',  ( 5.405949406249999534, 9.363379034771803333, -41.59375000204837391 ) ) ;
#26098 = ORIENTED_EDGE ( 'NONE', *, *, #38885, .F. ) ;
#26099 = CARTESIAN_POINT ( 'NONE',  ( -10.00000000000000000, -5.773502691896251982, -14.62499999999997335 ) ) ;
#26100 = CARTESIAN_POINT ( 'NONE',  ( -9.999999999999998224, 5.773502691896259087, -143.8750000000000000 ) ) ;
#26101 = CARTESIAN_POINT ( 'NONE',  ( -9.999999999999998224, 5.773502691896259087, -15.25000000409676382 ) ) ;
#26102 = CARTESIAN_POINT ( 'NONE',  ( -9.999999999999998224, 5.773502691896259087, -197.8750000000000000 ) ) ;
#26104 = VERTEX_POINT ( 'NONE', #25529 ) ;
#26103 = CARTESIAN_POINT ( 'NONE',  ( -5.405949406249996869, 9.363379034771805109, -119.5312500020483952 ) ) ;
#26105 = CARTESIAN_POINT ( 'NONE',  ( 10.70731569305672615, 1.500182182589836044, 0.000000000000000000 ) ) ;
#26106 = EDGE_CURVE ( 'NONE', #36911, #17741, #39996, .T. ) ;
#26107 = EDGE_LOOP ( 'NONE', ( #377, #1645, #5837, #14705 ) ) ;
#26108 = CARTESIAN_POINT ( 'NONE',  ( 5.405949406249999534, 9.363379034771803333, -52.28125000204835970 ) ) ;
#26109 = APPROVAL_DATE_TIME ( #2393, #37034 ) ;
#26110 = CARTESIAN_POINT ( 'NONE',  ( -10.81189881249999729, 1.324075727343319199E-15, -99.59375000204838102 ) ) ;
#26111 = ORIENTED_EDGE ( 'NONE', *, *, #15084, .T. ) ;
#26112 = CARTESIAN_POINT ( 'NONE',  ( -10.00000000000051337, 5.773502691895962435, -77.87499999999997158 ) ) ;
#26113 = CARTESIAN_POINT ( 'NONE',  ( 10.81189881249999907, 6.242252689847868297, -178.4062500020484094 ) ) ;
#26114 = CARTESIAN_POINT ( 'NONE',  ( 7.644554776091147741E-16, 12.48450537969573659, -0.9687500020483524876 ) ) ;
#26115 = CARTESIAN_POINT ( 'NONE',  ( -4.999999999999996447, 8.660254037844387298, -0.3750000040967649273 ) ) ;
#26116 = CARTESIAN_POINT ( 'NONE',  ( 5.405949406249992428, -9.363379034771808662, -132.0937500020483810 ) ) ;
#26117 = AXIS2_PLACEMENT_3D ( 'NONE', #13991, #459, #3896 ) ;
#26118 = CARTESIAN_POINT ( 'NONE',  ( -10.81189881249999729, 1.324075727343319199E-15, -105.5937500020483810 ) ) ;
#26119 = DIRECTION ( 'NONE',  ( 0.000000000000000000, -0.000000000000000000, 1.000000000000000000 ) ) ;
#26120 = CARTESIAN_POINT ( 'NONE',  ( 5.405949406249999534, 9.363379034771803333, -107.7812500020483810 ) ) ;
#26121 = CARTESIAN_POINT ( 'NONE',  ( 10.00000000000000000, 5.773502691896255534, -194.2500000040968189 ) ) ;
#26122 = CARTESIAN_POINT ( 'NONE',  ( 10.81189881249999729, 6.242252689847867408, -113.7187500020483952 ) ) ;
#26123 = CARTESIAN_POINT ( 'NONE',  ( 10.81189881249999729, 0.000000000000000000, -187.5312500020484094 ) ) ;
#26124 = FACE_OUTER_BOUND ( 'NONE', #17912, .T. ) ;
#26125 = CARTESIAN_POINT ( 'NONE',  ( 9.999999999999996447, -5.773502691896262640, -138.6250000000000000 ) ) ;
#26126 = CARTESIAN_POINT ( 'NONE',  ( 9.999999999999998224, 0.000000000000000000, -3.499999999999975131 ) ) ;
#26127 = CARTESIAN_POINT ( 'NONE',  ( 10.81189881249999551, -6.242252689847874514, -62.96875000204839523 ) ) ;
#26128 = AXIS2_PLACEMENT_3D ( 'NONE', #39947, #11232, #30477 ) ;
#26129 = CARTESIAN_POINT ( 'NONE',  ( 10.81189881249999907, 6.242252689847868297, -47.71875000204835970 ) ) ;
#26130 = DESIGN_CONTEXT ( 'detailed design', #20100, 'design' ) ;
#26131 = CARTESIAN_POINT ( 'NONE',  ( 9.999999999999996447, -5.773502691896262640, -182.5000000040968189 ) ) ;
#26132 = CARTESIAN_POINT ( 'NONE',  ( 7.644554776091147741E-16, 12.48450537969573659, -19.15625000204837391 ) ) ;
#26133 = CARTESIAN_POINT ( 'NONE',  ( -10.81189881249999729, 1.324075727343319199E-15, -26.09375000204835970 ) ) ;
#26134 = CARTESIAN_POINT ( 'NONE',  ( 9.999999999999742428, 5.773502691896404748, -117.3749999999999716 ) ) ;
#26135 = CARTESIAN_POINT ( 'NONE',  ( 10.81189881249999551, -6.242252689847874514, -136.4687500020483810 ) ) ;
#26136 = CARTESIAN_POINT ( 'NONE',  ( -9.999999999999998224, 1.224646799147353059E-15, -116.7499999999999858 ) ) ;
#26137 = CARTESIAN_POINT ( 'NONE',  ( -9.999999999999998224, 1.224646799147353059E-15, -28.24999999999996803 ) ) ;
#26138 = CARTESIAN_POINT ( 'NONE',  ( -4.999999999999996447, 8.660254037844387298, -68.99999999999997158 ) ) ;
#26139 = CARTESIAN_POINT ( 'NONE',  ( -5.405949406249996869, 9.363379034771805109, -136.0312500020484094 ) ) ;
#26140 = CARTESIAN_POINT ( 'NONE',  ( -10.81189881249999729, 6.242252689847871849, -114.9062500020483952 ) ) ;
#26141 = VERTEX_POINT ( 'NONE', #19447 ) ;
#26142 = CARTESIAN_POINT ( 'NONE',  ( -9.999999999999998224, 1.224646799147353059E-15, -176.7500000000000284 ) ) ;
#26143 = CARTESIAN_POINT ( 'NONE',  ( -4.999999999999996447, 8.660254037844387298, -109.8750000040967763 ) ) ;
#26144 = CARTESIAN_POINT ( 'NONE',  ( 9.999999999999998224, 0.000000000000000000, -123.8750000040967905 ) ) ;
#26145 = CARTESIAN_POINT ( 'NONE',  ( 10.81189881249999729, 0.000000000000000000, -67.34375000204836681 ) ) ;
#26146 = ORIENTED_EDGE ( 'NONE', *, *, #5364, .F. ) ;
#26147 = CARTESIAN_POINT ( 'NONE',  ( -9.999999999999998224, 5.773502691896259087, -40.37499999999997158 ) ) ;
#26148 = CARTESIAN_POINT ( 'NONE',  ( 7.070501591499377789E-16, 11.54700538379251284, -17.00000000409675849 ) ) ;
#26149 = CARTESIAN_POINT ( 'NONE',  ( -5.405949406250003975, -9.363379034771801557, -42.53125000204838102 ) ) ;
#26150 = CARTESIAN_POINT ( 'NONE',  ( 9.999999999999998224, 0.000000000000000000, -200.0000000000000000 ) ) ;
#26151 = CARTESIAN_POINT ( 'NONE',  ( 9.999999999999998224, 0.000000000000000000, -33.87500000409676915 ) ) ;
#26152 = CARTESIAN_POINT ( 'NONE',  ( 5.405949406249992428, -9.363379034771808662, -39.28125000204838102 ) ) ;
#26153 =( BOUNDED_CURVE ( )  B_SPLINE_CURVE ( 2, ( #6143, #38301, #31634, #21899, #9161, #22330, #35506 ),
 .UNSPECIFIED., .F., .F. ) 
 B_SPLINE_CURVE_WITH_KNOTS ( ( 3, 2, 2, 3 ),
 ( 0.6716417910447763928, 0.6728855721393036671, 0.6741293532338310523, 0.6753731343283584376 ),
 .UNSPECIFIED. ) 
 CURVE ( )  GEOMETRIC_REPRESENTATION_ITEM ( )  RATIONAL_B_SPLINE_CURVE ( ( 0.9999999999999761302, 0.8660254037844625774, 1.000000000000000000, 0.8660254037844387076, 1.000000000000000000, 0.8660254037844148378, 1.000000000000023981 ) ) 
 REPRESENTATION_ITEM ( '' )  );
#26154 = DIRECTION ( 'NONE',  ( -0.3779644730092265315, 0.6546536707079755324, 0.6546536707079790851 ) ) ;
#26155 = CARTESIAN_POINT ( 'NONE',  ( 5.405949406249999534, 9.363379034771803333, -136.2812500020483810 ) ) ;
#26156 = CARTESIAN_POINT ( 'NONE',  ( -5.405949406249996869, 9.363379034771805109, -151.0312500020483810 ) ) ;
#26157 = CARTESIAN_POINT ( 'NONE',  ( -9.999999999999998224, 1.224646799147353059E-15, -168.1250000040967905 ) ) ;
#26158 = ORIENTED_EDGE ( 'NONE', *, *, #39645, .T. ) ;
#26159 = VECTOR ( 'NONE', #4872, 1000.000000000000000 ) ;
#26160 = ORIENTED_EDGE ( 'NONE', *, *, #26481, .T. ) ;
#26161 = EDGE_CURVE ( 'NONE', #6469, #25139, #31213, .T. ) ;
#26162 = ORIENTED_EDGE ( 'NONE', *, *, #16876, .T. ) ;
#26163 = EDGE_CURVE ( 'NONE', #17527, #7578, #20464, .T. ) ;
#26164 = CARTESIAN_POINT ( 'NONE',  ( -5.000000000000003553, -8.660254037844383745, -121.3750000040967905 ) ) ;
#26165 = CARTESIAN_POINT ( 'NONE',  ( 10.81189881249999551, -6.242252689847874514, -175.4687500020484094 ) ) ;
#26166 = AXIS2_PLACEMENT_3D ( 'NONE', #25135, #8512, #18860 ) ;
#26167 = CARTESIAN_POINT ( 'NONE',  ( -2.293366432827344421E-15, -12.48450537969573659, -27.21875000204838102 ) ) ;
#26168 = CARTESIAN_POINT ( 'NONE',  ( -9.999999999999998224, 0.000000000000000000, -99.99999999999998579 ) ) ;
#26169 = CARTESIAN_POINT ( 'NONE',  ( -5.405949406250003975, -9.363379034771801557, -156.3437500020483810 ) ) ;
#26170 = CARTESIAN_POINT ( 'NONE',  ( -2.293366432827344421E-15, -12.48450537969573659, -147.2187500020484094 ) ) ;
#26171 = CARTESIAN_POINT ( 'NONE',  ( 4.999999999999992006, -8.660254037844389075, -8.625000004096744277 ) ) ;
#26172 = CARTESIAN_POINT ( 'NONE',  ( 7.644554776091147741E-16, 12.48450537969573659, -128.4687500020483810 ) ) ;
#26173 = CARTESIAN_POINT ( 'NONE',  ( 10.81189881249999551, -6.242252689847874514, -132.1562500020484094 ) ) ;
#26174 = CARTESIAN_POINT ( 'NONE',  ( -10.81189881249999907, -6.242252689847864744, -19.96875000204838102 ) ) ;
#26175 = CARTESIAN_POINT ( 'NONE',  ( -5.405949406250003975, -9.363379034771801557, -141.3437500020483810 ) ) ;
#26176 = DIRECTION ( 'NONE',  ( 1.000000000000000000, 0.000000000000000000, 0.000000000000000000 ) ) ;
#26177 = LINE ( 'NONE', #3507, #29594 ) ;
#26178 = CARTESIAN_POINT ( 'NONE',  ( 9.999999999999998224, 0.000000000000000000, -159.5000000000000000 ) ) ;
#26179 = CARTESIAN_POINT ( 'NONE',  ( 5.405949406249999534, 9.363379034771803333, 0.2187499979516283055 ) ) ;
#26180 = CARTESIAN_POINT ( 'NONE',  ( 10.81189881249999551, -6.242252689847874514, -74.96875000204838102 ) ) ;
#26181 = CARTESIAN_POINT ( 'NONE',  ( 5.405949406249999534, 9.363379034771803333, -38.78125000204838102 ) ) ;
#26182 = CARTESIAN_POINT ( 'NONE',  ( -2.293366432827344421E-15, -12.48450537969573659, -55.71875000204837391 ) ) ;
#26183 = CARTESIAN_POINT ( 'NONE',  ( -9.999999999999998224, 1.224646799147353059E-15, -175.2500000000000284 ) ) ;
#26184 = CARTESIAN_POINT ( 'NONE',  ( 10.81189881249999729, 0.000000000000000000, -164.8437500020484094 ) ) ;
#26185 = CARTESIAN_POINT ( 'NONE',  ( 9.999999999999998224, 0.000000000000000000, -135.5000000000000000 ) ) ;
#26186 = CARTESIAN_POINT ( 'NONE',  ( -5.405949406249996869, 9.363379034771805109, -136.0312500020484094 ) ) ;
#26187 = CYLINDRICAL_SURFACE ( 'NONE', #10693, 9.999999999999998224 ) ;
#26188 = CARTESIAN_POINT ( 'NONE',  ( 5.000000000000000000, 8.660254037844385522, -110.1250000040967763 ) ) ;
#26189 = CARTESIAN_POINT ( 'NONE',  ( -10.00000000000000000, -5.773502691896251982, -88.12499999999998579 ) ) ;
#26190 = EDGE_LOOP ( 'NONE', ( #23332, #25016, #29504, #8602 ) ) ;
#26191 = CARTESIAN_POINT ( 'NONE',  ( -10.81189881249999729, -6.242252689847864744, -120.6562500020483810 ) ) ;
#26192 = CARTESIAN_POINT ( 'NONE',  ( -9.999999999999998224, 1.224646799147353059E-15, -130.6250000040967620 ) ) ;
#26193 = VECTOR ( 'NONE', #13493, 1000.000000000000000 ) ;
#26194 = CARTESIAN_POINT ( 'NONE',  ( 10.81189881249999551, -6.242252689847874514, -175.6562500020484094 ) ) ;
#26195 = CARTESIAN_POINT ( 'NONE',  ( 5.000000000000000000, 8.660254037844385522, -44.12500000409677625 ) ) ;
#26196 = CARTESIAN_POINT ( 'NONE',  ( -4.999999999999996447, 8.660254037844387298, -48.37500000409677625 ) ) ;
#26197 = CARTESIAN_POINT ( 'NONE',  ( 10.81189881249999729, 0.000000000000000000, -63.03125000204837391 ) ) ;
#26198 = CARTESIAN_POINT ( 'NONE',  ( 4.999999999999992006, -8.660254037844389075, -63.74999999999997158 ) ) ;
#26199 = CARTESIAN_POINT ( 'NONE',  ( -2.293366432827344421E-15, -12.48450537969573659, -162.4062500020483810 ) ) ;
#26200 = CARTESIAN_POINT ( 'NONE',  ( 10.81189881249999729, 0.000000000000000000, -140.8437500020483810 ) ) ;
#26201 = FACE_OUTER_BOUND ( 'NONE', #14120, .T. ) ;
#26202 = CARTESIAN_POINT ( 'NONE',  ( -9.999999999999998224, 1.224646799147353059E-15, -115.6250000040967905 ) ) ;
#26203 = ORIENTED_EDGE ( 'NONE', *, *, #15983, .F. ) ;
#26204 = CARTESIAN_POINT ( 'NONE',  ( 9.999999999999998224, 0.000000000000000000, -42.49999999999998579 ) ) ;
#26206 = ORIENTED_EDGE ( 'NONE', *, *, #23342, .F. ) ;
#26205 = CARTESIAN_POINT ( 'NONE',  ( -2.293366432827344421E-15, -12.48450537969573659, -69.40625000204838102 ) ) ;
#26207 = DIRECTION ( 'NONE',  ( 0.000000000000000000, 0.000000000000000000, 1.000000000000000000 ) ) ;
#26208 = ADVANCED_FACE ( 'NONE', ( #22067 ), #25316, .T. ) ;
#26210 = ORIENTED_EDGE ( 'NONE', *, *, #27661, .T. ) ;
#26209 = CARTESIAN_POINT ( 'NONE',  ( 7.644554776091147741E-16, 12.48450537969573659, -119.4687500020483952 ) ) ;
#26211 = ORIENTED_EDGE ( 'NONE', *, *, #31977, .F. ) ;
#26212 = EDGE_CURVE ( 'NONE', #10842, #318, #11902, .T. ) ;
#26213 = CARTESIAN_POINT ( 'NONE',  ( 10.81189881249999551, -6.242252689847874514, -22.46875000204837391 ) ) ;
#26214 = CARTESIAN_POINT ( 'NONE',  ( -10.81189881249999729, 6.242252689847871849, -198.7187500020484379 ) ) ;
#26215 = AXIS2_PLACEMENT_3D ( 'NONE', #11172, #24369, #37511 ) ;
#26217 = EDGE_CURVE ( 'NONE', #414, #39570, #16291, .T. ) ;
#26216 = CARTESIAN_POINT ( 'NONE',  ( -5.405949406250003975, -9.363379034771801557, -46.84375000204838102 ) ) ;
#26218 = DIRECTION ( 'NONE',  ( -0.000000000000000000, -0.000000000000000000, 1.000000000000000000 ) ) ;
#26219 = CARTESIAN_POINT ( 'NONE',  ( 4.999999999999992006, -8.660254037844389075, -26.24999999999996803 ) ) ;
#26220 = CARTESIAN_POINT ( 'NONE',  ( 10.81189881249999729, 0.000000000000000000, -185.8437500020483810 ) ) ;
#26221 = CARTESIAN_POINT ( 'NONE',  ( -5.405949406250003975, -9.363379034771801557, -165.3437500020484094 ) ) ;
#26222 = APPROVAL ( #2604, 'UNSPECIFIED' ) ;
#26223 = CARTESIAN_POINT ( 'NONE',  ( -5.405949406249996869, 9.363379034771805109, -149.3437500020483810 ) ) ;
#26224 = CARTESIAN_POINT ( 'NONE',  ( -10.81189881249999729, 1.324075727343319199E-15, -165.5937500020484094 ) ) ;
#26225 = CARTESIAN_POINT ( 'NONE',  ( -2.121150477449813534E-15, -11.54700538379251284, -118.2500000040968189 ) ) ;
#26226 = CARTESIAN_POINT ( 'NONE',  ( 9.999999999999742428, 5.773502691896404748, -188.2500000040968189 ) ) ;
#26227 = CARTESIAN_POINT ( 'NONE',  ( 9.999999999999996447, -5.773502691896262640, -185.1250000000000284 ) ) ;
#26228 = CARTESIAN_POINT ( 'NONE',  ( -5.405949406249996869, 9.363379034771805109, -95.34375000204838102 ) ) ;
#26229 = DIRECTION ( 'NONE',  ( 0.000000000000000000, 0.000000000000000000, 1.000000000000000000 ) ) ;
#26230 = CARTESIAN_POINT ( 'NONE',  ( -2.293366432827344421E-15, -12.48450537969573659, -73.90625000204836681 ) ) ;
#26231 = CARTESIAN_POINT ( 'NONE',  ( 4.999999999999992006, -8.660254037844389075, -131.6250000040967620 ) ) ;
#26232 = CARTESIAN_POINT ( 'NONE',  ( -5.405949406250003975, -9.363379034771801557, -189.3437500020483810 ) ) ;
#26233 = CARTESIAN_POINT ( 'NONE',  ( 5.405949406249999534, 9.363379034771803333, -164.7812500020484094 ) ) ;
#26234 =( BOUNDED_CURVE ( )  B_SPLINE_CURVE ( 2, ( #38896, #9325, #18178, #14932, #41263, #8702, #28130 ),
 .UNSPECIFIED., .F., .F. ) 
 B_SPLINE_CURVE_WITH_KNOTS ( ( 3, 2, 2, 3 ),
 ( 0.3917910447761194792, 0.3930348258706468090, 0.3942786069651742498, 0.3955223880597015795 ),
 .UNSPECIFIED. ) 
 CURVE ( )  GEOMETRIC_REPRESENTATION_ITEM ( )  RATIONAL_B_SPLINE_CURVE ( ( 0.9999999999999940048, 0.8660254037844447028, 1.000000000000000000, 0.8660254037844387076, 1.000000000000000000, 0.8660254037844267172, 1.000000000000011990 ) ) 
 REPRESENTATION_ITEM ( '' )  );
#26235 = CARTESIAN_POINT ( 'NONE',  ( -5.405949406250003975, -9.363379034771801557, -60.53125000204836681 ) ) ;
#26236 = CARTESIAN_POINT ( 'NONE',  ( -10.00000000000000000, -5.773502691896251982, -136.5000000040967905 ) ) ;
#26237 = CARTESIAN_POINT ( 'NONE',  ( 10.00000000000000000, 5.773502691896255534, -112.8749999999999858 ) ) ;
#26238 = ORIENTED_EDGE ( 'NONE', *, *, #1695, .T. ) ;
#26239 = CARTESIAN_POINT ( 'NONE',  ( -10.81189881249999729, 1.324075727343319199E-15, -143.2812500020483810 ) ) ;
#26240 = CARTESIAN_POINT ( 'NONE',  ( -5.405949406250003975, -9.363379034771801557, -155.0312500020484094 ) ) ;
#26241 = EDGE_CURVE ( 'NONE', #28547, #21458, #14009, .T. ) ;
#26242 = CARTESIAN_POINT ( 'NONE',  ( -10.81189881249999729, 6.242252689847871849, -198.9062500020484094 ) ) ;
#26243 = LINE ( 'NONE', #39392, #36472 ) ;
#26244 = CARTESIAN_POINT ( 'NONE',  ( -2.293366432827344421E-15, -12.48450537969573659, -88.71875000204838102 ) ) ;
#26245 = ORIENTED_EDGE ( 'NONE', *, *, #39381, .T. ) ;
#26246 = CARTESIAN_POINT ( 'NONE',  ( 5.000000000000000000, 8.660254037844385522, -58.74999999999997158 ) ) ;
#26247 = CARTESIAN_POINT ( 'NONE',  ( 10.81189881249999551, -6.242252689847874514, -185.9687500020484094 ) ) ;
#26248 = CARTESIAN_POINT ( 'NONE',  ( -2.121150477449813534E-15, -11.54700538379251284, -64.25000000409677625 ) ) ;
#26249 = CARTESIAN_POINT ( 'NONE',  ( -5.000000000000003553, -8.660254037844383745, -116.8750000040967905 ) ) ;
#26250 = CARTESIAN_POINT ( 'NONE',  ( 10.81189881249999551, -6.242252689847874514, -85.65625000204838102 ) ) ;
#26251 = CARTESIAN_POINT ( 'NONE',  ( -5.405949406249996869, 9.363379034771805109, -71.53125000204838102 ) ) ;
#26252 = CARTESIAN_POINT ( 'NONE',  ( -9.999999999999998224, 1.224646799147353059E-15, -57.12500000409676204 ) ) ;
#26253 =( REPRESENTATION_RELATIONSHIP ('NONE','NONE', #21658, #12816 ) REPRESENTATION_RELATIONSHIP_WITH_TRANSFORMATION ( #6836 )SHAPE_REPRESENTATION_RELATIONSHIP( ) );
#26254 = CARTESIAN_POINT ( 'NONE',  ( 5.405949406249992428, -9.363379034771808662, -19.59375000204835615 ) ) ;
#26255 = CARTESIAN_POINT ( 'NONE',  ( 7.070501591499376803E-16, 11.54700538379251284, -38.00000000409676204 ) ) ;
#26256 = CARTESIAN_POINT ( 'NONE',  ( 5.405949406249992428, -9.363379034771808662, -186.2812500020484094 ) ) ;
#26257 = LOCAL_TIME ( 11, 57, 6.000000000000000000, #13229 ) ;
#26258 = CARTESIAN_POINT ( 'NONE',  ( -10.81189881249999729, 6.242252689847871849, -14.40625000204837036 ) ) ;
#26259 = CARTESIAN_POINT ( 'NONE',  ( 9.999999999999998224, 0.000000000000000000, -171.8750000040968189 ) ) ;
#26260 = CARTESIAN_POINT ( 'NONE',  ( 7.070501591499376803E-16, 11.54700538379251284, -165.1250000000000000 ) ) ;
#26261 = CARTESIAN_POINT ( 'NONE',  ( 9.999999999999479527, 5.773502691896553074, -114.7500000040967620 ) ) ;
#26262 = CARTESIAN_POINT ( 'NONE',  ( -7.071067811865472841, -7.071067811865472841, -200.0000000000000000 ) ) ;
#26263 = CARTESIAN_POINT ( 'NONE',  ( 9.999999999999998224, 0.000000000000000000, -167.0000000000000000 ) ) ;
#26264 = CYLINDRICAL_SURFACE ( 'NONE', #35837, 9.999999999999998224 ) ;
#26266 = EDGE_LOOP ( 'NONE', ( #41209, #23351, #24154, #21584 ) ) ;
#26265 = CARTESIAN_POINT ( 'NONE',  ( 5.405949406249992428, -9.363379034771808662, -91.78125000204838102 ) ) ;
#26267 = FACE_OUTER_BOUND ( 'NONE', #20261, .T. ) ;
#26269 = ORIENTED_EDGE ( 'NONE', *, *, #35621, .F. ) ;
#26268 = CARTESIAN_POINT ( 'NONE',  ( 10.81189881249999729, 0.000000000000000000, -103.3437500020483668 ) ) ;
#26270 = ORIENTED_EDGE ( 'NONE', *, *, #28598, .T. ) ;
#26271 = CARTESIAN_POINT ( 'NONE',  ( 10.81189881249999729, 0.000000000000000000, -34.34375000204836681 ) ) ;
#26272 = CARTESIAN_POINT ( 'NONE',  ( 5.405949406249992428, -9.363379034771808662, -21.28125000204836326 ) ) ;
#26273 = CALENDAR_DATE ( 2026, 28, 9 ) ;
#26274 = CARTESIAN_POINT ( 'NONE',  ( -10.81189881249999729, 6.242252689847871849, -74.21875000204836681 ) ) ;
#26275 = DIRECTION ( 'NONE',  ( -1.000000000000000000, 0.000000000000000000, -0.000000000000000000 ) ) ;
#26276 = CARTESIAN_POINT ( 'NONE',  ( 10.81189881249999551, -6.242252689847874514, -190.4687500020484094 ) ) ;
#26277 = VECTOR ( 'NONE', #34121, 1000.000000000000000 ) ;
#26278 =( BOUNDED_CURVE ( )  B_SPLINE_CURVE ( 2, ( #9960, #19887, #60, #16000, #9334, #42335, #22935 ),
 .UNSPECIFIED., .F., .F. ) 
 B_SPLINE_CURVE_WITH_KNOTS ( ( 3, 2, 2, 3 ),
 ( 0.3470149253731344974, 0.3482587064676618271, 0.3495024875621891569, 0.3507462686567164867 ),
 .UNSPECIFIED. ) 
 CURVE ( )  GEOMETRIC_REPRESENTATION_ITEM ( )  RATIONAL_B_SPLINE_CURVE ( ( 0.9999999999999820144, 0.8660254037844566932, 1.000000000000000000, 0.8660254037844387076, 1.000000000000000000, 0.8660254037844327124, 1.000000000000005995 ) ) 
 REPRESENTATION_ITEM ( '' )  );
#26279 = CARTESIAN_POINT ( 'NONE',  ( 10.00000000000102318, -5.773502691895667560, -79.00000000409673362 ) ) ;
#26280 = FACE_OUTER_BOUND ( 'NONE', #8541, .T. ) ;
#26281 = CARTESIAN_POINT ( 'NONE',  ( 5.405949406249992428, -9.363379034771808662, -156.2812500020484094 ) ) ;
#26282 = CARTESIAN_POINT ( 'NONE',  ( 4.999999999999992006, -8.660254037844389075, -4.125000004096768258 ) ) ;
#26283 = CARTESIAN_POINT ( 'NONE',  ( 9.999999999998969713, 5.773502691896851502, -50.25000000409674072 ) ) ;
#26284 = LOCAL_TIME ( 11, 57, 6.000000000000000000, #41158 ) ;
#26285 = EDGE_CURVE ( 'NONE', #23818, #11901, #26992, .T. ) ;
#26286 = CARTESIAN_POINT ( 'NONE',  ( 5.405949406249999534, 9.363379034771803333, -121.0937500020483952 ) ) ;
#26287 = CARTESIAN_POINT ( 'NONE',  ( -2.293366432827344421E-15, -12.48450537969573659, -96.40625000204839523 ) ) ;
#26288 = CARTESIAN_POINT ( 'NONE',  ( -2.293366432827344421E-15, -12.48450537969573659, -111.2187500020483668 ) ) ;
#26289 = CARTESIAN_POINT ( 'NONE',  ( -5.405949406249996869, 9.363379034771805109, -74.34375000204838102 ) ) ;
#26290 = CARTESIAN_POINT ( 'NONE',  ( 5.405949406249999534, 9.363379034771803333, -85.28125000204838102 ) ) ;
#26291 = CARTESIAN_POINT ( 'NONE',  ( 7.070501591499377789E-16, 11.54700538379251284, -164.0000000040967905 ) ) ;
#26292 =( BOUNDED_CURVE ( )  B_SPLINE_CURVE ( 2, ( #63, #16208, #26590, #30050, #16851, #39741, #10385 ),
 .UNSPECIFIED., .F., .F. ) 
 B_SPLINE_CURVE_WITH_KNOTS ( ( 3, 2, 2, 3 ),
 ( 0.1268656716417910224, 0.1281094527363183799, 0.1293532338308457652, 0.1305970149253731227 ),
 .UNSPECIFIED. ) 
 CURVE ( )  GEOMETRIC_REPRESENTATION_ITEM ( )  RATIONAL_B_SPLINE_CURVE ( ( 1.000000000000003109, 0.8660254037844358210, 1.000000000000000000, 0.8660254037844387076, 1.000000000000000000, 0.8660254037844387076, 1.000000000000000000 ) ) 
 REPRESENTATION_ITEM ( '' )  );
#26293 = FACE_OUTER_BOUND ( 'NONE', #6993, .T. ) ;
#26294 = CARTESIAN_POINT ( 'NONE',  ( -10.81189881249999729, 6.242252689847871849, -164.4062500020483810 ) ) ;
#26295 = CARTESIAN_POINT ( 'NONE',  ( -10.81189881249999729, 1.324075727343319199E-15, -182.2812500020483810 ) ) ;
#26296 = CARTESIAN_POINT ( 'NONE',  ( 5.000000000000000000, 8.660254037844385522, -159.6250000040967905 ) ) ;
#26297 = CARTESIAN_POINT ( 'NONE',  ( -2.121150477449813534E-15, -11.54700538379251284, -156.8750000000000000 ) ) ;
#26298 = CARTESIAN_POINT ( 'NONE',  ( -5.405949406250003975, -9.363379034771801557, -6.343750002048370362 ) ) ;
#26299 = CARTESIAN_POINT ( 'NONE',  ( 9.999999999998969713, 5.773502691896851502, -6.374999999999940492 ) ) ;
#26300 = CARTESIAN_POINT ( 'NONE',  ( 10.81189881249999729, 0.000000000000000000, -112.3437500020483810 ) ) ;
#26301 = CARTESIAN_POINT ( 'NONE',  ( 9.999999999999998224, 0.000000000000000000, -79.99999999999998579 ) ) ;
#26302 = CARTESIAN_POINT ( 'NONE',  ( 10.81189881249999551, -6.242252689847874514, -10.65625000204836859 ) ) ;
#26303 = CARTESIAN_POINT ( 'NONE',  ( -4.999999999999996447, 8.660254037844387298, -99.37500000409679046 ) ) ;
#26304 = LINE ( 'NONE', #42049, #380 ) ;
#26305 = CARTESIAN_POINT ( 'NONE',  ( 10.81189881249999729, 0.000000000000000000, -105.0312500020483810 ) ) ;
#26306 = CARTESIAN_POINT ( 'NONE',  ( -5.405949406250003975, -9.363379034771801557, -89.03125000204838102 ) ) ;
#26307 = ORIENTED_EDGE ( 'NONE', *, *, #8561, .T. ) ;
#26308 = CARTESIAN_POINT ( 'NONE',  ( 7.070501591499377789E-16, 11.54700538379251284, -83.00000000409677625 ) ) ;
#26309 = CARTESIAN_POINT ( 'NONE',  ( 5.000000000000000000, 8.660254037844385522, -48.24999999999998579 ) ) ;
#26310 = CARTESIAN_POINT ( 'NONE',  ( -2.293366432827344421E-15, -12.48450537969573659, -40.71875000204835970 ) ) ;
#26311 = VERTEX_POINT ( 'NONE', #36704 ) ;
#26312 = CARTESIAN_POINT ( 'NONE',  ( 9.999999999999998224, 0.000000000000000000, -7.999999999999952038 ) ) ;
#26313 = CARTESIAN_POINT ( 'NONE',  ( -9.999999999999998224, 1.224646799147353059E-15, -146.7500000000000000 ) ) ;
#26314 = CARTESIAN_POINT ( 'NONE',  ( -10.00000000000000000, -5.773502691896251982, -10.50000000409675849 ) ) ;
#26315 = ORGANIZATION ( 'NAUO-ORG2', 'UNSPECIFIED', 'UNSPECIFIED' ) ;
#26316 = CARTESIAN_POINT ( 'NONE',  ( 9.999999999999998224, 0.000000000000000000, -191.0000000000000000 ) ) ;
#26318 = ORIENTED_EDGE ( 'NONE', *, *, #12588, .F. ) ;
#26317 = CARTESIAN_POINT ( 'NONE',  ( 10.81189881249999551, -6.242252689847874514, -118.6562500020483952 ) ) ;
#26319 = DIRECTION ( 'NONE',  ( 1.000000000000000000, 0.000000000000000000, 0.000000000000000000 ) ) ;
#26320 = ORIENTED_EDGE ( 'NONE', *, *, #15086, .T. ) ;
#26321 = CARTESIAN_POINT ( 'NONE',  ( -5.405949406249996869, 9.363379034771805109, -44.53125000204838102 ) ) ;
#26322 = APPLICATION_PROTOCOL_DEFINITION ( 'international standard', 'config_control_design', 1994, #7703 ) ;
#26323 = CARTESIAN_POINT ( 'NONE',  ( -10.81189881249999907, -6.242252689847864744, -106.9687500020483668 ) ) ;
#26324 = CARTESIAN_POINT ( 'NONE',  ( -10.81189881249999729, 1.324075727343319199E-15, -125.2812500020483668 ) ) ;
#26325 = ORIENTED_EDGE ( 'NONE', *, *, #25109, .F. ) ;
#26326 = CARTESIAN_POINT ( 'NONE',  ( -2.121150477449813534E-15, -11.54700538379251284, -85.25000000409676204 ) ) ;
#26327 = CARTESIAN_POINT ( 'NONE',  ( 9.999999999999998224, 0.000000000000000000, -125.3750000040967905 ) ) ;
#26328 = CARTESIAN_POINT ( 'NONE',  ( -10.81189881249999907, -6.242252689847864744, -182.1562500020483810 ) ) ;
#26329 = CARTESIAN_POINT ( 'NONE',  ( -2.121150477449813534E-15, -11.54700538379251284, -26.37499999999998224 ) ) ;
#26330 = CARTESIAN_POINT ( 'NONE',  ( 9.999999999999998224, 0.000000000000000000, -0.8750000040967653714 ) ) ;
#26331 = CARTESIAN_POINT ( 'NONE',  ( 10.81189881249999551, -6.242252689847874514, -130.4687500020483810 ) ) ;
#26332 = CARTESIAN_POINT ( 'NONE',  ( 7.644554776091147741E-16, 12.48450537969573659, -101.4687500020483668 ) ) ;
#26333 = CARTESIAN_POINT ( 'NONE',  ( 10.81189881249999551, -6.242252689847874514, -108.1562500020483810 ) ) ;
#26334 = CARTESIAN_POINT ( 'NONE',  ( 7.070501591499377789E-16, 11.54700538379251284, -197.0000000040968189 ) ) ;
#26335 = CARTESIAN_POINT ( 'NONE',  ( 10.81189881249999729, 0.000000000000000000, -118.3437500020483810 ) ) ;
#26336 = CARTESIAN_POINT ( 'NONE',  ( 7.644554776091147741E-16, 12.48450537969573659, -187.1562500020484094 ) ) ;
#26337 = CARTESIAN_POINT ( 'NONE',  ( 100.0000000000000284, -20.00000000000001066, -170.0000000000000000 ) ) ;
#26338 = FACE_OUTER_BOUND ( 'NONE', #32895, .T. ) ;
#26339 = CARTESIAN_POINT ( 'NONE',  ( -9.999999999999998224, 1.224646799147353059E-15, -139.2499999999999716 ) ) ;
#26340 = CARTESIAN_POINT ( 'NONE',  ( 4.999999999999992006, -8.660254037844389075, -5.249999999999976907 ) ) ;
#26341 = CARTESIAN_POINT ( 'NONE',  ( 5.405949406249999534, 9.363379034771803333, -61.09375000204836681 ) ) ;
#26342 = CARTESIAN_POINT ( 'NONE',  ( -10.81189881249999729, 1.324075727343319199E-15, -48.59375000204838102 ) ) ;
#26343 = CARTESIAN_POINT ( 'NONE',  ( -5.000000000000003553, -8.660254037844383745, -181.3750000040967905 ) ) ;
#26344 = CARTESIAN_POINT ( 'NONE',  ( -10.81189881249999907, -6.242252689847864744, -21.65625000204837036 ) ) ;
#26345 = CARTESIAN_POINT ( 'NONE',  ( -2.293366432827344421E-15, -12.48450537969573659, -28.71875000204834905 ) ) ;
#26346 = CARTESIAN_POINT ( 'NONE',  ( -2.293366432827344421E-15, -12.48450537969573659, -139.7187500020483810 ) ) ;
#26347 = CARTESIAN_POINT ( 'NONE',  ( 9.999999999999996447, -5.773502691896262640, -102.6249999999999858 ) ) ;
#26348 = CARTESIAN_POINT ( 'NONE',  ( 10.81189881249999907, 6.242252689847868297, -34.40625000204835970 ) ) ;
#26349 = CARTESIAN_POINT ( 'NONE',  ( 10.00000000000102318, -5.773502691895667560, -27.62499999999995737 ) ) ;
#26350 = CARTESIAN_POINT ( 'NONE',  ( 9.999999999999996447, -5.773502691896262640, -71.12499999999998579 ) ) ;
#26351 = CARTESIAN_POINT ( 'NONE',  ( 10.81189881249999729, 0.000000000000000000, -132.0312500020484094 ) ) ;
#26352 = CARTESIAN_POINT ( 'NONE',  ( 5.405949406249999534, 9.363379034771803333, -113.7812500020483952 ) ) ;
#26353 = EDGE_CURVE ( 'NONE', #38098, #27593, #16403, .T. ) ;
#26354 = ORIENTED_EDGE ( 'NONE', *, *, #40947, .T. ) ;
#26355 = CARTESIAN_POINT ( 'NONE',  ( 9.999999999999998224, 0.000000000000000000, -128.0000000000000000 ) ) ;
#26356 = CARTESIAN_POINT ( 'NONE',  ( 4.999999999999992006, -8.660254037844389075, -110.6250000040967763 ) ) ;
#26357 = CARTESIAN_POINT ( 'NONE',  ( -9.999999999999998224, 1.224646799147353059E-15, -103.6250000040967763 ) ) ;
#26358 = CARTESIAN_POINT ( 'NONE',  ( -5.405949406250003975, -9.363379034771801557, -64.84375000204836681 ) ) ;
#26359 = VERTEX_POINT ( 'NONE', #30248 ) ;
#26360 = CARTESIAN_POINT ( 'NONE',  ( -9.999999999999998224, 1.224646799147353059E-15, -29.74999999999997158 ) ) ;
#26361 = CIRCLE ( 'NONE', #27026, 42.00000000000004974 ) ;
#26362 = CARTESIAN_POINT ( 'NONE',  ( 9.999999999999998224, 0.000000000000000000, -21.87500000409675494 ) ) ;
#26363 = CARTESIAN_POINT ( 'NONE',  ( 5.405949406249999534, 9.363379034771803333, -43.28125000204838102 ) ) ;
#26364 = CARTESIAN_POINT ( 'NONE',  ( 4.999999999999992006, -8.660254037844389075, -90.74999999999998579 ) ) ;
#26365 = CARTESIAN_POINT ( 'NONE',  ( 7.070501591499377789E-16, 11.54700538379251284, -35.00000000409675494 ) ) ;
#26366 = CARTESIAN_POINT ( 'NONE',  ( -79.99999999999992895, 19.99999999999998934, -160.0000000000000000 ) ) ;
#26367 = CARTESIAN_POINT ( 'NONE',  ( 5.405949406249999534, 9.363379034771803333, -140.7812500020483810 ) ) ;
#26368 = CARTESIAN_POINT ( 'NONE',  ( 7.644554776091147741E-16, 12.48450537969573659, -140.6562500020484094 ) ) ;
#26369 = DIRECTION ( 'NONE',  ( -0.000000000000000000, -0.000000000000000000, 1.000000000000000000 ) ) ;
#26370 = ORIENTED_EDGE ( 'NONE', *, *, #30711, .T. ) ;
#26371 = ORIENTED_EDGE ( 'NONE', *, *, #18927, .T. ) ;
#26372 = EDGE_CURVE ( 'NONE', #39976, #28849, #29822, .T. ) ;
#26373 = ORIENTED_EDGE ( 'NONE', *, *, #25637, .F. ) ;
#26374 = CARTESIAN_POINT ( 'NONE',  ( 10.00000000000025402, -5.773502691896113426, -121.0000000040967763 ) ) ;
#26375 = CARTESIAN_POINT ( 'NONE',  ( -5.405949406249996869, 9.363379034771805109, -171.8437500020484094 ) ) ;
#26376 = VECTOR ( 'NONE', #22743, 1000.000000000000000 ) ;
#26377 = CARTESIAN_POINT ( 'NONE',  ( 10.81189881249999551, -6.242252689847874514, -22.46875000204837391 ) ) ;
#26378 = DIRECTION ( 'NONE',  ( -0.000000000000000000, -0.000000000000000000, 1.000000000000000000 ) ) ;
#26379 = CARTESIAN_POINT ( 'NONE',  ( 10.81189881249999551, -6.242252689847874514, -158.9687500020484094 ) ) ;
#26380 = CARTESIAN_POINT ( 'NONE',  ( -10.81189881249999907, -6.242252689847864744, -144.4687500020484094 ) ) ;
#26381 = CYLINDRICAL_SURFACE ( 'NONE', #16210, 9.999999999999998224 ) ;
#26382 = CARTESIAN_POINT ( 'NONE',  ( 10.81189881249999729, 0.000000000000000000, -128.8437500020484094 ) ) ;
#26383 = CARTESIAN_POINT ( 'NONE',  ( 10.81189881249999729, 0.000000000000000000, -133.5312500020484094 ) ) ;
#26384 = CARTESIAN_POINT ( 'NONE',  ( 10.81189881249999551, -6.242252689847874514, -16.46875000204836326 ) ) ;
#26385 = CARTESIAN_POINT ( 'NONE',  ( -10.81189881249999729, 6.242252689847871849, -141.7187500020483810 ) ) ;
#26386 = CYLINDRICAL_SURFACE ( 'NONE', #27443, 9.999999999999998224 ) ;
#26387 = CYLINDRICAL_SURFACE ( 'NONE', #31667, 9.999999999999998224 ) ;
#26388 = CARTESIAN_POINT ( 'NONE',  ( 9.999999999999998224, 0.000000000000000000, -161.0000000000000000 ) ) ;
#26389 = CARTESIAN_POINT ( 'NONE',  ( -2.121150477449813534E-15, -11.54700538379251284, -167.7500000040968189 ) ) ;
#26390 = CARTESIAN_POINT ( 'NONE',  ( 5.405949406249999534, 9.363379034771803333, -70.09375000204836681 ) ) ;
#26391 = CARTESIAN_POINT ( 'NONE',  ( 5.405949406249999534, 9.363379034771803333, -43.28125000204838102 ) ) ;
#26392 = CARTESIAN_POINT ( 'NONE',  ( -5.405949406250003975, -9.363379034771801557, -54.34375000204835970 ) ) ;
#26393 = CARTESIAN_POINT ( 'NONE',  ( -10.00000000000012790, -5.773502691896178263, -175.1250000000000284 ) ) ;
#26394 = CARTESIAN_POINT ( 'NONE',  ( -10.81189881249999729, 1.324075727343319199E-15, -164.0937500020484094 ) ) ;
#26395 = CARTESIAN_POINT ( 'NONE',  ( 10.00000000000000000, 5.773502691896255534, -130.8750000000000000 ) ) ;
#26396 = CARTESIAN_POINT ( 'NONE',  ( 10.81189881249999729, 6.242252689847867408, -142.4062500020484094 ) ) ;
#26397 = LINE ( 'NONE', #23378, #25504 ) ;
#26398 = CARTESIAN_POINT ( 'NONE',  ( 10.00000000000000000, 5.773502691896255534, -111.7500000040967763 ) ) ;
#26399 = CARTESIAN_POINT ( 'NONE',  ( -9.999999999999998224, 5.773502691896259087, -91.37499999999998579 ) ) ;
#26400 =( BOUNDED_CURVE ( )  B_SPLINE_CURVE ( 2, ( #8334, #24744, #30573, #40253, #1004, #34020, #17583 ),
 .UNSPECIFIED., .F., .F. ) 
 B_SPLINE_CURVE_WITH_KNOTS ( ( 3, 2, 2, 3 ),
 ( 0.5895522388059702967, 0.5907960199004975710, 0.5920398009950249563, 0.5932835820895523415 ),
 .UNSPECIFIED. ) 
 CURVE ( )  GEOMETRIC_REPRESENTATION_ITEM ( )  RATIONAL_B_SPLINE_CURVE ( ( 0.9999999999999880096, 0.8660254037844506980, 1.000000000000000000, 0.8660254037844387076, 1.000000000000000000, 0.8660254037844267172, 1.000000000000011990 ) ) 
 REPRESENTATION_ITEM ( '' )  );
#26401 = ORIENTED_EDGE ( 'NONE', *, *, #27778, .F. ) ;
#26402 = CARTESIAN_POINT ( 'NONE',  ( 10.81189881249999729, 6.242252689847867408, -113.9062500020483952 ) ) ;
#26403 = CARTESIAN_POINT ( 'NONE',  ( 9.999999999999996447, -5.773502691896262640, -130.0000000040967905 ) ) ;
#26404 = CARTESIAN_POINT ( 'NONE',  ( 10.00000000000076916, -5.773502691895816774, -111.6249999999999716 ) ) ;
#26405 = CARTESIAN_POINT ( 'NONE',  ( -10.81189881249999729, 1.324075727343319199E-15, -165.7812500020484094 ) ) ;
#26406 = CARTESIAN_POINT ( 'NONE',  ( 7.070501591499377789E-16, 11.54700538379251284, -39.50000000409675494 ) ) ;
#26407 = EDGE_CURVE ( 'NONE', #2222, #17679, #35617, .T. ) ;
#26408 = CARTESIAN_POINT ( 'NONE',  ( 7.070501591499376803E-16, 11.54700538379251284, -48.50000000409676915 ) ) ;
#26409 = CARTESIAN_POINT ( 'NONE',  ( 7.644554776091147741E-16, 12.48450537969573659, -56.65625000204838813 ) ) ;
#26410 = CARTESIAN_POINT ( 'NONE',  ( -9.999999999999998224, 1.224646799147353059E-15, -175.2500000000000284 ) ) ;
#26411 = CARTESIAN_POINT ( 'NONE',  ( -10.81189881249999907, -6.242252689847864744, -162.6562500020483810 ) ) ;
#26412 = CARTESIAN_POINT ( 'NONE',  ( -5.405949406249996869, 9.363379034771805109, -138.8437500020484094 ) ) ;
#26413 = CARTESIAN_POINT ( 'NONE',  ( 9.999999999999998224, 0.000000000000000000, -93.87500000409677625 ) ) ;
#26414 = ORIENTED_EDGE ( 'NONE', *, *, #25918, .T. ) ;
#26416 = ORIENTED_EDGE ( 'NONE', *, *, #10897, .F. ) ;
#26415 = CARTESIAN_POINT ( 'NONE',  ( 10.81189881249999907, 6.242252689847868297, -68.90625000204839523 ) ) ;
#26417 = MECHANICAL_CONTEXT ( 'NONE', #15686, 'mechanical' ) ;
#26419 = EDGE_LOOP ( 'NONE', ( #11487, #37297, #26627, #31483 ) ) ;
#26418 = CARTESIAN_POINT ( 'NONE',  ( -10.81189881249999729, 6.242252689847871849, -120.7187500020483952 ) ) ;
#26420 = ORIENTED_EDGE ( 'NONE', *, *, #7371, .F. ) ;
#26421 = CARTESIAN_POINT ( 'NONE',  ( 7.644554776091147741E-16, 12.48450537969573659, -20.46875000204836326 ) ) ;
#26422 = CARTESIAN_POINT ( 'NONE',  ( 5.405949406249999534, 9.363379034771803333, -197.5937500020484094 ) ) ;
#26423 = CARTESIAN_POINT ( 'NONE',  ( 7.644554776091147741E-16, 12.48450537969573659, -44.46875000204836681 ) ) ;
#26424 = LINE ( 'NONE', #20153, #8910 ) ;
#26425 = CARTESIAN_POINT ( 'NONE',  ( -9.999999999999998224, 5.773502691896259087, -25.37499999999998224 ) ) ;
#26426 = CARTESIAN_POINT ( 'NONE',  ( -10.81189881249999729, 1.324075727343319199E-15, -180.5937500020484094 ) ) ;
#26427 = CARTESIAN_POINT ( 'NONE',  ( 7.644554776091147741E-16, 12.48450537969573659, -168.9687500020483810 ) ) ;
#26428 = CARTESIAN_POINT ( 'NONE',  ( 10.81189881249999907, 6.242252689847868297, -152.7187500020483810 ) ) ;
#26429 = CARTESIAN_POINT ( 'NONE',  ( -5.405949406250003975, -9.363379034771801557, -165.3437500020484094 ) ) ;
#26430 = CARTESIAN_POINT ( 'NONE',  ( 7.070501591499376803E-16, 11.54700538379251284, -107.0000000040967763 ) ) ;
#26431 = CARTESIAN_POINT ( 'NONE',  ( 0.000000000000000000, 0.000000000000000000, -99.99999999999998579 ) ) ;
#26432 = CARTESIAN_POINT ( 'NONE',  ( 7.070501591499377789E-16, 11.54700538379251284, -190.6250000000000000 ) ) ;
#26433 = CARTESIAN_POINT ( 'NONE',  ( 5.405949406249992428, -9.363379034771808662, -100.5937500020483810 ) ) ;
#26434 = CARTESIAN_POINT ( 'NONE',  ( 4.999999999999992006, -8.660254037844389075, -101.2499999999999858 ) ) ;
#26435 = CARTESIAN_POINT ( 'NONE',  ( -10.81189881249999729, 1.324075727343319199E-15, -68.28125000204838102 ) ) ;
#26436 = CYLINDRICAL_SURFACE ( 'NONE', #29547, 9.999999999999998224 ) ;
#26437 = CARTESIAN_POINT ( 'NONE',  ( -10.81189881249999907, -6.242252689847864744, -187.9687500020484094 ) ) ;
#26438 = CARTESIAN_POINT ( 'NONE',  ( -5.405949406250003975, -9.363379034771801557, -123.5312500020483952 ) ) ;
#26439 = CARTESIAN_POINT ( 'NONE',  ( 10.81189881249999729, 6.242252689847867408, -161.9062500020483810 ) ) ;
#26440 = CARTESIAN_POINT ( 'NONE',  ( -2.293366432827344421E-15, -12.48450537969573659, -49.90625000204838102 ) ) ;
#26441 = CARTESIAN_POINT ( 'NONE',  ( 7.070501591499377789E-16, 11.54700538379251284, -137.0000000040967905 ) ) ;
#26442 = CARTESIAN_POINT ( 'NONE',  ( 9.999999999999996447, -5.773502691896262640, -116.1250000000000000 ) ) ;
#26443 = ORIENTED_EDGE ( 'NONE', *, *, #24570, .F. ) ;
#26444 = CARTESIAN_POINT ( 'NONE',  ( 5.405949406249999534, 9.363379034771803333, -137.7812500020483810 ) ) ;
#26445 = CARTESIAN_POINT ( 'NONE',  ( 10.81189881249999907, 6.242252689847868297, -158.9062500020483810 ) ) ;
#26446 = CARTESIAN_POINT ( 'NONE',  ( 10.81189881249999907, 6.242252689847868297, -196.4062500020484379 ) ) ;
#26447 = CARTESIAN_POINT ( 'NONE',  ( 7.070501591499376803E-16, 11.54700538379251284, -131.0000000040967905 ) ) ;
#26448 = CARTESIAN_POINT ( 'NONE',  ( -10.81189881249999907, -6.242252689847864744, -78.46875000204838102 ) ) ;
#26449 = ORIENTED_EDGE ( 'NONE', *, *, #11181, .F. ) ;
#26450 = CARTESIAN_POINT ( 'NONE',  ( -9.999999999999998224, 1.224646799147353059E-15, -55.24999999999996447 ) ) ;
#26451 = CARTESIAN_POINT ( 'NONE',  ( 7.644554776091147741E-16, 12.48450537969573659, -185.4687500020483810 ) ) ;
#26452 = CARTESIAN_POINT ( 'NONE',  ( 9.999999999999998224, 0.000000000000000000, -63.87500000409676915 ) ) ;
#26453 = EDGE_CURVE ( 'NONE', #31054, #22217, #23125, .T. ) ;
#26454 = CARTESIAN_POINT ( 'NONE',  ( 9.999999999999872102, 5.773502691896329253, -165.3750000000000000 ) ) ;
#26455 = CARTESIAN_POINT ( 'NONE',  ( 9.999999999999479527, 5.773502691896553074, -140.2500000040967620 ) ) ;
#26456 = EDGE_CURVE ( 'NONE', #21319, #23753, #19335, .T. ) ;
#26457 = CARTESIAN_POINT ( 'NONE',  ( -10.81189881249999729, 6.242252689847871849, -81.90625000204838102 ) ) ;
#26458 = CARTESIAN_POINT ( 'NONE',  ( -5.405949406250003975, -9.363379034771801557, -57.53125000204836681 ) ) ;
#26459 = EDGE_CURVE ( 'NONE', #10615, #30730, #32343, .T. ) ;
#26460 = CARTESIAN_POINT ( 'NONE',  ( -9.999999999999998224, 5.773502691896259087, -61.75000000409678336 ) ) ;
#26461 = CARTESIAN_POINT ( 'NONE',  ( 10.81189881249999729, 0.000000000000000000, -16.34375000204835260 ) ) ;
#26462 = CARTESIAN_POINT ( 'NONE',  ( 9.999999999999998224, 0.000000000000000000, -150.8750000040967905 ) ) ;
#26463 = CARTESIAN_POINT ( 'NONE',  ( 5.405949406249992428, -9.363379034771808662, -183.2812500020484094 ) ) ;
#26464 = CARTESIAN_POINT ( 'NONE',  ( -10.81189881249999729, 6.242252689847871849, -12.90625000204836859 ) ) ;
#26465 = CARTESIAN_POINT ( 'NONE',  ( -9.999999999999998224, 1.224646799147353059E-15, -116.7499999999999858 ) ) ;
#26466 = LINE ( 'NONE', #23447, #6205 ) ;
#26467 = LINE ( 'NONE', #10053, #38727 ) ;
#26468 = DIRECTION ( 'NONE',  ( -0.000000000000000000, -0.000000000000000000, 1.000000000000000000 ) ) ;
#26469 = CARTESIAN_POINT ( 'NONE',  ( -2.121150477449813534E-15, -11.54700538379251284, -170.3750000000000284 ) ) ;
#26470 = CARTESIAN_POINT ( 'NONE',  ( 9.999999999999998224, 0.000000000000000000, -137.3750000040967905 ) ) ;
#26472 = ORIENTED_EDGE ( 'NONE', *, *, #29207, .F. ) ;
#26471 = CARTESIAN_POINT ( 'NONE',  ( 10.81189881249999729, 0.000000000000000000, -91.53125000204838102 ) ) ;
#26473 = CARTESIAN_POINT ( 'NONE',  ( -9.999999999999998224, 1.224646799147353059E-15, -200.0000000000000000 ) ) ;
#26474 = ADVANCED_FACE ( 'NONE', ( #6720 ), #33487, .F. ) ;
#26476 = ORIENTED_EDGE ( 'NONE', *, *, #10106, .T. ) ;
#26475 = CARTESIAN_POINT ( 'NONE',  ( 5.000000000000000000, 8.660254037844385522, -162.2500000000000000 ) ) ;
#26477 = ORIENTED_EDGE ( 'NONE', *, *, #34924, .T. ) ;
#26478 = CARTESIAN_POINT ( 'NONE',  ( -2.293366432827344421E-15, -12.48450537969573659, -36.21875000204835970 ) ) ;
#26479 = CARTESIAN_POINT ( 'NONE',  ( -2.293366432827344421E-15, -12.48450537969573659, -19.90625000204837747 ) ) ;
#26480 = APPROVAL_DATE_TIME ( #39426, #2230 ) ;
#26481 = EDGE_CURVE ( 'NONE', #24722, #270, #17047, .T. ) ;
#26482 = CARTESIAN_POINT ( 'NONE',  ( -10.81189881249999907, -6.242252689847864744, -72.46875000204835260 ) ) ;
#26483 = EDGE_CURVE ( 'NONE', #35357, #30453, #23510, .T. ) ;
#26484 = CARTESIAN_POINT ( 'NONE',  ( -2.293366432827344421E-15, -12.48450537969573659, -196.7187500020484094 ) ) ;
#26485 = CARTESIAN_POINT ( 'NONE',  ( -10.81189881249999729, 6.242252689847871849, -153.7187500020483526 ) ) ;
#26486 =( BOUNDED_CURVE ( )  B_SPLINE_CURVE ( 2, ( #17437, #10967, #24163, #37309, #1280, #14408, #27602 ),
 .UNSPECIFIED., .F., .F. ) 
 B_SPLINE_CURVE_WITH_KNOTS ( ( 3, 2, 2, 3 ),
 ( 0.7014925373134330844, 0.7027363184079604697, 0.7039800995024877439, 0.7052238805970151292 ),
 .UNSPECIFIED. ) 
 CURVE ( )  GEOMETRIC_REPRESENTATION_ITEM ( )  RATIONAL_B_SPLINE_CURVE ( ( 0.9999999999999761302, 0.8660254037844625774, 1.000000000000000000, 0.8660254037844387076, 1.000000000000000000, 0.8660254037844148378, 1.000000000000023981 ) ) 
 REPRESENTATION_ITEM ( '' )  );
#26487 = CARTESIAN_POINT ( 'NONE',  ( 5.000000000000000000, 8.660254037844385522, -72.62500000409677625 ) ) ;
#26488 = DIRECTION ( 'NONE',  ( -0.000000000000000000, -0.000000000000000000, 1.000000000000000000 ) ) ;
#26489 = CARTESIAN_POINT ( 'NONE',  ( 10.81189881249999729, 0.000000000000000000, -147.0312500020483810 ) ) ;
#26490 = CARTESIAN_POINT ( 'NONE',  ( 9.999999999999996447, -5.773502691896262640, 0.4999999959032586094 ) ) ;
#26491 = CARTESIAN_POINT ( 'NONE',  ( 0.000000000000000000, 0.000000000000000000, -200.0000000000000000 ) ) ;
#26492 = CARTESIAN_POINT ( 'NONE',  ( 10.81189881249999907, 6.242252689847868297, -121.2187500020483952 ) ) ;
#26493 = CARTESIAN_POINT ( 'NONE',  ( 9.999999999999998224, 0.000000000000000000, -66.49999999999997158 ) ) ;
#26494 = CARTESIAN_POINT ( 'NONE',  ( -10.81189881249999729, 6.242252689847871849, -87.90625000204838102 ) ) ;
#26495 = CARTESIAN_POINT ( 'NONE',  ( -10.81189881249999729, -6.242252689847864744, -109.9687500020483810 ) ) ;
#26496 = ADVANCED_FACE ( 'NONE', ( #40778 ), #11219, .F. ) ;
#26497 = CARTESIAN_POINT ( 'NONE',  ( -10.81189881249999729, 6.242252689847871849, -74.21875000204836681 ) ) ;
#26498 = CARTESIAN_POINT ( 'NONE',  ( 10.81189881249999729, 0.000000000000000000, -85.53125000204838102 ) ) ;
#26499 = CARTESIAN_POINT ( 'NONE',  ( 9.999999999999998224, 0.000000000000000000, -164.3750000040967905 ) ) ;
#26500 = CARTESIAN_POINT ( 'NONE',  ( -5.405949406250003975, -9.363379034771801557, -162.5312500020484094 ) ) ;
#26501 = CARTESIAN_POINT ( 'NONE',  ( -2.293366432827344421E-15, -12.48450537969573659, -183.4062500020483810 ) ) ;
#26502 = CARTESIAN_POINT ( 'NONE',  ( -10.00000000000000000, -5.773502691896251982, -157.5000000040968189 ) ) ;
#26503 = CARTESIAN_POINT ( 'NONE',  ( 9.999999999999998224, 0.000000000000000000, -156.5000000000000000 ) ) ;
#26504 = CARTESIAN_POINT ( 'NONE',  ( -2.293366432827344421E-15, -12.48450537969573659, -6.218750002048356151 ) ) ;
#26505 = CYLINDRICAL_SURFACE ( 'NONE', #40577, 9.999999999999998224 ) ;
#26506 = CARTESIAN_POINT ( 'NONE',  ( 5.405949406249992428, -9.363379034771808662, -115.5937500020483810 ) ) ;
#26507 = CARTESIAN_POINT ( 'NONE',  ( -5.000000000000003553, -8.660254037844383745, -80.49999999999998579 ) ) ;
#26508 = CARTESIAN_POINT ( 'NONE',  ( -10.81189881249999729, 1.324075727343319199E-15, -15.78125000204835793 ) ) ;
#26509 = CARTESIAN_POINT ( 'NONE',  ( 9.999999999999996447, -5.773502691896262640, -88.00000000409677625 ) ) ;
#26510 = FACE_OUTER_BOUND ( 'NONE', #7364, .T. ) ;
#26511 = CARTESIAN_POINT ( 'NONE',  ( 5.405949406249992428, -9.363379034771808662, -109.7812500020483810 ) ) ;
#26512 = CARTESIAN_POINT ( 'NONE',  ( -10.81189881249999729, -6.242252689847864744, -80.15625000204836681 ) ) ;
#26513 = VERTEX_POINT ( 'NONE', #34767 ) ;
#26514 = EDGE_CURVE ( 'NONE', #37214, #35978, #13013, .T. ) ;
#26515 = CARTESIAN_POINT ( 'NONE',  ( 5.000000000000000000, 8.660254037844385522, -86.12500000409677625 ) ) ;
#26516 = CARTESIAN_POINT ( 'NONE',  ( 7.070501591499376803E-16, 11.54700538379251284, -146.0000000040967905 ) ) ;
#26517 = CARTESIAN_POINT ( 'NONE',  ( -10.81189881249999729, 6.242252689847871849, -39.71875000204835970 ) ) ;
#26518 = ORIENTED_EDGE ( 'NONE', *, *, #32270, .T. ) ;
#26519 = CARTESIAN_POINT ( 'NONE',  ( 10.00000000000000000, 5.773502691896255534, -6.374999999999966249 ) ) ;
#26520 = CARTESIAN_POINT ( 'NONE',  ( 4.999999999999992006, -8.660254037844389075, -141.7500000000000000 ) ) ;
#26521 = CARTESIAN_POINT ( 'NONE',  ( 5.000000000000000000, 8.660254037844385522, -45.62500000409677625 ) ) ;
#26522 = CARTESIAN_POINT ( 'NONE',  ( 10.00000000000000000, 5.773502691896255534, -8.250000004096758488 ) ) ;
#26523 = CARTESIAN_POINT ( 'NONE',  ( 4.999999999999992006, -8.660254037844389075, -189.7500000000000000 ) ) ;
#26524 = CARTESIAN_POINT ( 'NONE',  ( -2.121150477449813534E-15, -11.54700538379251284, -184.2500000040967905 ) ) ;
#26526 = ORIENTED_EDGE ( 'NONE', *, *, #32055, .F. ) ;
#26525 = CARTESIAN_POINT ( 'NONE',  ( 10.81189881249999551, -6.242252689847874514, -115.6562500020483810 ) ) ;
#26527 = DIRECTION ( 'NONE',  ( -0.000000000000000000, -0.000000000000000000, 1.000000000000000000 ) ) ;
#26528 = VERTEX_POINT ( 'NONE', #17473 ) ;
#26529 = EDGE_CURVE ( 'NONE', #22060, #25538, #7492, .T. ) ;
#26530 =( BOUNDED_CURVE ( )  B_SPLINE_CURVE ( 2, ( #9023, #2560, #2766, #5360, #35150, #18517, #15270 ),
 .UNSPECIFIED., .F., .F. ) 
 B_SPLINE_CURVE_WITH_KNOTS ( ( 3, 2, 2, 3 ),
 ( 0.9664179104477613746, 0.9676616915422887599, 0.9689054726368161452, 0.9701492537313435305 ),
 .UNSPECIFIED. ) 
 CURVE ( )  GEOMETRIC_REPRESENTATION_ITEM ( )  RATIONAL_B_SPLINE_CURVE ( ( 0.9999999999999761302, 0.8660254037844625774, 1.000000000000000000, 0.8660254037844387076, 1.000000000000000000, 0.8660254037844148378, 1.000000000000023981 ) ) 
 REPRESENTATION_ITEM ( '' )  );
#26531 = CARTESIAN_POINT ( 'NONE',  ( -10.81189881249999729, 1.324075727343319199E-15, -45.78125000204838813 ) ) ;
#26532 = APPROVAL_STATUS ( 'not_yet_approved' ) ;
#26533 = CARTESIAN_POINT ( 'NONE',  ( 10.81189881249999729, 0.000000000000000000, -91.34375000204838102 ) ) ;
#26534 = CARTESIAN_POINT ( 'NONE',  ( -2.293366432827344421E-15, -12.48450537969573659, -126.4062500020483810 ) ) ;
#26535 = ORIENTED_EDGE ( 'NONE', *, *, #31434, .F. ) ;
#26536 = CARTESIAN_POINT ( 'NONE',  ( 9.999999999999998224, 0.000000000000000000, -82.99999999999997158 ) ) ;
#26537 = CARTESIAN_POINT ( 'NONE',  ( 9.999999999999998224, 0.000000000000000000, -115.9999999999999858 ) ) ;
#26538 =( BOUNDED_CURVE ( )  B_SPLINE_CURVE ( 2, ( #5947, #26007, #3921, #39733, #36504, #10583, #19095 ),
 .UNSPECIFIED., .F., .F. ) 
 B_SPLINE_CURVE_WITH_KNOTS ( ( 3, 2, 2, 3 ),
 ( 0.2014925373134328901, 0.2027363184079602476, 0.2039800995024875774, 0.2052238805970149627 ),
 .UNSPECIFIED. ) 
 CURVE ( )  GEOMETRIC_REPRESENTATION_ITEM ( )  RATIONAL_B_SPLINE_CURVE ( ( 0.9999999999999940048, 0.8660254037844447028, 1.000000000000000000, 0.8660254037844387076, 1.000000000000000000, 0.8660254037844357100, 1.000000000000002887 ) ) 
 REPRESENTATION_ITEM ( '' )  );
#26539 = CARTESIAN_POINT ( 'NONE',  ( -10.81189881249999729, 1.324075727343319199E-15, -183.7812500020484094 ) ) ;
#26540 = FACE_OUTER_BOUND ( 'NONE', #32275, .T. ) ;
#26541 = CARTESIAN_POINT ( 'NONE',  ( -5.405949406249996869, 9.363379034771805109, -128.3437500020484094 ) ) ;
#26542 = CARTESIAN_POINT ( 'NONE',  ( 10.81189881249999907, 6.242252689847868297, -98.71875000204838102 ) ) ;
#26543 = DIRECTION ( 'NONE',  ( -0.000000000000000000, -0.000000000000000000, 1.000000000000000000 ) ) ;
#26544 = CARTESIAN_POINT ( 'NONE',  ( 5.405949406249992428, -9.363379034771808662, -106.7812500020483810 ) ) ;
#26545 = CARTESIAN_POINT ( 'NONE',  ( -9.999999999999998224, 5.773502691896259087, -189.2500000040967905 ) ) ;
#26546 = CARTESIAN_POINT ( 'NONE',  ( -2.293366432827344421E-15, -12.48450537969573659, -111.2187500020483668 ) ) ;
#26547 = CARTESIAN_POINT ( 'NONE',  ( 10.81189881249999729, 0.000000000000000000, -184.5312500020484094 ) ) ;
#26548 = VECTOR ( 'NONE', #13267, 1000.000000000000000 ) ;
#26549 = CARTESIAN_POINT ( 'NONE',  ( -9.999999999999479527, -5.773502691896549521, -95.62499999999995737 ) ) ;
#26550 = CARTESIAN_POINT ( 'NONE',  ( 0.6423023231492728247, 10.81644720607814314, -99.99999999999997158 ) ) ;
#26551 = CARTESIAN_POINT ( 'NONE',  ( -2.121150477449813534E-15, -11.54700538379251284, -128.3750000000000000 ) ) ;
#26552 = CARTESIAN_POINT ( 'NONE',  ( -4.999999999999996447, 8.660254037844387298, -5.999999999999977796 ) ) ;
#26553 = CARTESIAN_POINT ( 'NONE',  ( -10.81189881249999729, 1.324075727343319199E-15, -63.59375000204836681 ) ) ;
#26554 = CARTESIAN_POINT ( 'NONE',  ( -10.81189881249999729, 6.242252689847871849, -48.71875000204835970 ) ) ;
#26555 = CARTESIAN_POINT ( 'NONE',  ( -9.999999999999998224, 1.224646799147353059E-15, -181.6250000040967905 ) ) ;
#26556 = CARTESIAN_POINT ( 'NONE',  ( -5.405949406250003975, -9.363379034771801557, -18.53125000204835970 ) ) ;
#26557 = CARTESIAN_POINT ( 'NONE',  ( 10.81189881249999729, 0.000000000000000000, -32.84375000204836681 ) ) ;
#26558 = CARTESIAN_POINT ( 'NONE',  ( 9.999999999999998224, 1.224646799147353059E-15, -99.99999999999998579 ) ) ;
#26559 = CARTESIAN_POINT ( 'NONE',  ( 10.81189881249999729, 0.000000000000000000, -137.8437500020484094 ) ) ;
#26560 = CARTESIAN_POINT ( 'NONE',  ( -9.999999999999998224, 5.773502691896259087, -104.8749999999999858 ) ) ;
#26561 = CARTESIAN_POINT ( 'NONE',  ( 5.405949406249999534, 9.363379034771803333, -32.78125000204837391 ) ) ;
#26562 = CARTESIAN_POINT ( 'NONE',  ( 4.999999999999992006, -8.660254037844389075, -27.74999999999996803 ) ) ;
#26563 = CARTESIAN_POINT ( 'NONE',  ( 5.000000000000000000, 8.660254037844385522, -60.24999999999997158 ) ) ;
#26564 = CARTESIAN_POINT ( 'NONE',  ( 10.81189881249999907, 6.242252689847868297, -133.4062500020483810 ) ) ;
#26565 = CARTESIAN_POINT ( 'NONE',  ( -5.405949406249996869, 9.363379034771805109, -112.0312500020483810 ) ) ;
#26566 = ORIENTED_EDGE ( 'NONE', *, *, #18720, .T. ) ;
#26567 = FACE_OUTER_BOUND ( 'NONE', #40649, .T. ) ;
#26568 = CARTESIAN_POINT ( 'NONE',  ( 7.070501591499377789E-16, 11.54700538379251284, -111.5000000040967763 ) ) ;
#26569 = CARTESIAN_POINT ( 'NONE',  ( 9.999999999999998224, 0.000000000000000000, -146.0000000000000000 ) ) ;
#26570 = CARTESIAN_POINT ( 'NONE',  ( -10.81189881249999729, 6.242252689847871849, -65.21875000204838102 ) ) ;
#26571 = ORIENTED_EDGE ( 'NONE', *, *, #8956, .F. ) ;
#26572 = CARTESIAN_POINT ( 'NONE',  ( -2.121150477449813534E-15, -11.54700538379251284, -35.37499999999996447 ) ) ;
#26573 = CARTESIAN_POINT ( 'NONE',  ( 10.00000000000000000, 5.773502691896255534, -20.25000000409677625 ) ) ;
#26574 = CARTESIAN_POINT ( 'NONE',  ( -5.405949406250003975, -9.363379034771801557, -41.03125000204838102 ) ) ;
#26575 = CARTESIAN_POINT ( 'NONE',  ( 7.070501591499376803E-16, 11.54700538379251284, -35.00000000409674783 ) ) ;
#26576 = CARTESIAN_POINT ( 'NONE',  ( 9.999999999999996447, -5.773502691896262640, -34.00000000409675494 ) ) ;
#26577 = ADVANCED_FACE ( 'NONE', ( #40988 ), #8435, .T. ) ;
#26578 = CARTESIAN_POINT ( 'NONE',  ( 5.405949406249999534, 9.363379034771803333, -143.7812500020483810 ) ) ;
#26579 = CARTESIAN_POINT ( 'NONE',  ( -4.999999999999996447, 8.660254037844387298, -121.8750000040967905 ) ) ;
#26580 = VERTEX_POINT ( 'NONE', #34550 ) ;
#26581 = ORIENTED_EDGE ( 'NONE', *, *, #7526, .T. ) ;
#26582 = ORIENTED_EDGE ( 'NONE', *, *, #21759, .T. ) ;
#26583 = EDGE_CURVE ( 'NONE', #4760, #6102, #4541, .T. ) ;
#26584 = LINE ( 'NONE', #29402, #6332 ) ;
#26585 = CARTESIAN_POINT ( 'NONE',  ( -5.405949406249996869, 9.363379034771805109, -170.3437500020484094 ) ) ;
#26586 = CARTESIAN_POINT ( 'NONE',  ( -5.405949406249996869, 9.363379034771805109, -21.84375000204835615 ) ) ;
#26587 = LINE ( 'NONE', #32860, #22610 ) ;
#26588 = CARTESIAN_POINT ( 'NONE',  ( 10.81189881249999729, 6.242252689847867408, -157.2187500020483810 ) ) ;
#26589 = CARTESIAN_POINT ( 'NONE',  ( 5.405949406249992428, -9.363379034771808662, -145.5937500020483810 ) ) ;
#26590 = CARTESIAN_POINT ( 'NONE',  ( 5.000000000000000000, 8.660254037844385522, -173.1250000040968189 ) ) ;
#26591 = CARTESIAN_POINT ( 'NONE',  ( 7.644554776091147741E-16, 12.48450537969573659, -122.4687500020483952 ) ) ;
#26592 = AXIS2_PLACEMENT_3D ( 'NONE', #8756, #37894, #18667 ) ;
#26593 = CARTESIAN_POINT ( 'NONE',  ( 10.81189881249999729, 0.000000000000000000, -136.5312500020484094 ) ) ;
#26594 = CARTESIAN_POINT ( 'NONE',  ( -2.293366432827344421E-15, -12.48450537969573659, -7.718750002048352599 ) ) ;
#26595 = CARTESIAN_POINT ( 'NONE',  ( -5.405949406249996869, 9.363379034771805109, -140.3437500020484094 ) ) ;
#26596 = CARTESIAN_POINT ( 'NONE',  ( -9.999999999999998224, 1.224646799147353059E-15, -172.2500000000000000 ) ) ;
#26597 = VECTOR ( 'NONE', #11324, 1000.000000000000000 ) ;
#26598 = DIRECTION ( 'NONE',  ( -0.000000000000000000, -0.000000000000000000, 1.000000000000000000 ) ) ;
#26599 = CARTESIAN_POINT ( 'NONE',  ( -2.121150477449813534E-15, -11.54700538379251284, -153.8750000000000000 ) ) ;
#26600 = CARTESIAN_POINT ( 'NONE',  ( 5.000000000000000000, 8.660254037844385522, -56.12500000409676204 ) ) ;
#26601 = CARTESIAN_POINT ( 'NONE',  ( 7.644554776091147741E-16, 12.48450537969573659, -74.46875000204838102 ) ) ;
#26602 = CARTESIAN_POINT ( 'NONE',  ( -2.293366432827344421E-15, -12.48450537969573659, -43.90625000204838102 ) ) ;
#26603 = CARTESIAN_POINT ( 'NONE',  ( -10.81189881249999729, 1.324075727343319199E-15, -51.59375000204835260 ) ) ;
#26604 = DIRECTION ( 'NONE',  ( -0.000000000000000000, 1.000000000000000000, -0.000000000000000000 ) ) ;
#26605 = CARTESIAN_POINT ( 'NONE',  ( -2.293366432827344421E-15, -12.48450537969573659, -163.7187500020483810 ) ) ;
#26606 = CARTESIAN_POINT ( 'NONE',  ( 5.000000000000000000, 8.660254037844385522, -126.2499999999999716 ) ) ;
#26607 = AXIS2_PLACEMENT_3D ( 'NONE', #21217, #27704, #28735 ) ;
#26608 = CARTESIAN_POINT ( 'NONE',  ( -10.81189881249999729, 6.242252689847871849, -135.9062500020484094 ) ) ;
#26609 =( BOUNDED_CURVE ( )  B_SPLINE_CURVE ( 2, ( #10671, #6814, #14324, #36381, #39818, #33155, #4212 ),
 .UNSPECIFIED., .F., .F. ) 
 B_SPLINE_CURVE_WITH_KNOTS ( ( 3, 2, 2, 3 ),
 ( 0.8805970149253734558, 0.8818407960199008411, 0.8830845771144281153, 0.8843283582089555006 ),
 .UNSPECIFIED. ) 
 CURVE ( )  GEOMETRIC_REPRESENTATION_ITEM ( )  RATIONAL_B_SPLINE_CURVE ( ( 0.9999999999999641398, 0.8660254037844745678, 1.000000000000000000, 0.8660254037844387076, 1.000000000000000000, 0.8660254037844148378, 1.000000000000023981 ) ) 
 REPRESENTATION_ITEM ( '' )  );
#26610 = CARTESIAN_POINT ( 'NONE',  ( -9.999999999999998224, 0.000000000000000000, -99.99999999999998579 ) ) ;
#26611 = CARTESIAN_POINT ( 'NONE',  ( 10.00000000000000000, 5.773502691896255534, -114.7500000040967763 ) ) ;
#26612 = CARTESIAN_POINT ( 'NONE',  ( 5.000000000000000000, 8.660254037844385522, -90.24999999999998579 ) ) ;
#26613 = ORIENTED_EDGE ( 'NONE', *, *, #17490, .T. ) ;
#26614 = CARTESIAN_POINT ( 'NONE',  ( -5.405949406250003975, -9.363379034771801557, -110.0312500020483810 ) ) ;
#26615 = CARTESIAN_POINT ( 'NONE',  ( -4.999999999999996447, 8.660254037844387298, -132.3750000040967905 ) ) ;
#26616 = CARTESIAN_POINT ( 'NONE',  ( 9.999999999999998224, 0.000000000000000000, -134.0000000000000000 ) ) ;
#26617 = CARTESIAN_POINT ( 'NONE',  ( -5.405949406250003975, -9.363379034771801557, -165.5312500020484094 ) ) ;
#26618 = CARTESIAN_POINT ( 'NONE',  ( 4.999999999999992006, -8.660254037844389075, -43.12500000409677625 ) ) ;
#26619 = CARTESIAN_POINT ( 'NONE',  ( 7.070501591499376803E-16, 11.54700538379251284, -155.0000000040968189 ) ) ;
#26620 = CARTESIAN_POINT ( 'NONE',  ( -10.81189881249999729, 1.324075727343319199E-15, -50.28125000204835970 ) ) ;
#26621 = EDGE_CURVE ( 'NONE', #39524, #20204, #34337, .T. ) ;
#26622 = CARTESIAN_POINT ( 'NONE',  ( 7.070501591499376803E-16, 11.54700538379251284, -45.12499999999997158 ) ) ;
#26623 = CARTESIAN_POINT ( 'NONE',  ( 7.644554776091147741E-16, 12.48450537969573659, -164.6562500020484094 ) ) ;
#26624 = CARTESIAN_POINT ( 'NONE',  ( -10.81189881249999907, -6.242252689847864744, -135.4687500020483810 ) ) ;
#26625 = FACE_OUTER_BOUND ( 'NONE', #1215, .T. ) ;
#26626 = CARTESIAN_POINT ( 'NONE',  ( 9.999999999999998224, 0.000000000000000000, -179.0000000000000000 ) ) ;
#26627 = ORIENTED_EDGE ( 'NONE', *, *, #6321, .T. ) ;
#26629 = VERTEX_POINT ( 'NONE', #7998 ) ;
#26628 = CARTESIAN_POINT ( 'NONE',  ( -10.81189881249999729, 6.242252689847871849, -69.90625000204839523 ) ) ;
#26630 = PERSON_AND_ORGANIZATION_ROLE ( 'design_owner' ) ;
#26632 = VERTEX_POINT ( 'NONE', #1314 ) ;
#26631 = CARTESIAN_POINT ( 'NONE',  ( 10.81189881249999551, -6.242252689847874514, -121.4687500020484094 ) ) ;
#26633 = ORIENTED_EDGE ( 'NONE', *, *, #31857, .T. ) ;
#26634 = CARTESIAN_POINT ( 'NONE',  ( 10.81189881249999729, 6.242252689847867408, -17.71875000204836681 ) ) ;
#26635 = CARTESIAN_POINT ( 'NONE',  ( -10.81189881249999729, 6.242252689847871849, -195.7187500020484379 ) ) ;
#26636 = CARTESIAN_POINT ( 'NONE',  ( 5.405949406249992428, -9.363379034771808662, -43.59375000204837391 ) ) ;
#26637 = DIRECTION ( 'NONE',  ( 1.000000000000000000, 0.000000000000000000, 0.000000000000000000 ) ) ;
#26638 = ADVANCED_FACE ( 'NONE', ( #27854 ), #17683, .F. ) ;
#26639 = CARTESIAN_POINT ( 'NONE',  ( -4.999999999999996447, 8.660254037844387298, -151.8750000040967905 ) ) ;
#26640 = CARTESIAN_POINT ( 'NONE',  ( 5.405949406249999534, 9.363379034771803333, -178.0937500020484094 ) ) ;
#26641 = CARTESIAN_POINT ( 'NONE',  ( -5.405949406250003975, -9.363379034771801557, -166.8437500020484094 ) ) ;
#26642 = CARTESIAN_POINT ( 'NONE',  ( -10.81189881249999907, -6.242252689847864744, -145.9687500020484094 ) ) ;
#26643 =( BOUNDED_CURVE ( )  B_SPLINE_CURVE ( 2, ( #8057, #33747, #40612, #21204, #4808, #4168, #17313 ),
 .UNSPECIFIED., .F., .F. ) 
 B_SPLINE_CURVE_WITH_KNOTS ( ( 3, 2, 2, 3 ),
 ( 0.4477611940298508730, 0.4490049751243782028, 0.4502487562189055881, 0.4514925373134329734 ),
 .UNSPECIFIED. ) 
 CURVE ( )  GEOMETRIC_REPRESENTATION_ITEM ( )  RATIONAL_B_SPLINE_CURVE ( ( 0.9999999999999880096, 0.8660254037844506980, 1.000000000000000000, 0.8660254037844387076, 1.000000000000000000, 0.8660254037844267172, 1.000000000000011990 ) ) 
 REPRESENTATION_ITEM ( '' )  );
#26644 = CARTESIAN_POINT ( 'NONE',  ( 10.81189881249999729, 6.242252689847867408, -163.2187500020483810 ) ) ;
#26645 = CARTESIAN_POINT ( 'NONE',  ( -9.999999999999998224, 1.224646799147353059E-15, -118.6250000040967905 ) ) ;
#26646 = CARTESIAN_POINT ( 'NONE',  ( -9.999999999999998224, 1.224646799147353059E-15, -184.2500000000000000 ) ) ;
#26647 = CARTESIAN_POINT ( 'NONE',  ( 5.405949406249992428, -9.363379034771808662, -96.09375000204838102 ) ) ;
#26648 = CARTESIAN_POINT ( 'NONE',  ( -9.999999999999998224, 1.224646799147353059E-15, -34.24999999999997158 ) ) ;
#26649 = CARTESIAN_POINT ( 'NONE',  ( 10.81189881249999907, 6.242252689847868297, -70.40625000204839523 ) ) ;
#26650 = FACE_OUTER_BOUND ( 'NONE', #12368, .T. ) ;
#26651 = CARTESIAN_POINT ( 'NONE',  ( 10.81189881249999907, 6.242252689847868297, -187.2187500020484094 ) ) ;
#26652 = CARTESIAN_POINT ( 'NONE',  ( 10.81189881249999551, -6.242252689847874514, -126.1562500020483810 ) ) ;
#26653 = CARTESIAN_POINT ( 'NONE',  ( 10.81189881249999551, -6.242252689847874514, -160.6562500020484094 ) ) ;
#26654 = CARTESIAN_POINT ( 'NONE',  ( 10.81189881249999729, 0.000000000000000000, -54.03125000204836681 ) ) ;
#26655 = CARTESIAN_POINT ( 'NONE',  ( 7.070501591499377789E-16, 11.54700538379251284, -135.5000000040967905 ) ) ;
#26656 = CARTESIAN_POINT ( 'NONE',  ( 10.00000000000000000, 5.773502691896255534, -117.3750000000000000 ) ) ;
#26657 = VERTEX_POINT ( 'NONE', #7795 ) ;
#26658 = CARTESIAN_POINT ( 'NONE',  ( -10.81189881249999729, -6.242252689847864744, -134.1562500020483810 ) ) ;
#26659 = CARTESIAN_POINT ( 'NONE',  ( -5.405949406250003975, -9.363379034771801557, -147.5312500020483810 ) ) ;
#26660 = CARTESIAN_POINT ( 'NONE',  ( 7.644554776091147741E-16, 12.48450537969573659, -188.6562500020484379 ) ) ;
#26661 = CARTESIAN_POINT ( 'NONE',  ( -5.000000000000003553, -8.660254037844383745, -125.5000000000000000 ) ) ;
#26662 = CARTESIAN_POINT ( 'NONE',  ( -10.81189881249999729, 6.242252689847871849, -83.21875000204838102 ) ) ;
#26663 = ORIENTED_EDGE ( 'NONE', *, *, #31803, .F. ) ;
#26664 = CARTESIAN_POINT ( 'NONE',  ( 7.070501591499377789E-16, 11.54700538379251284, -57.12499999999997868 ) ) ;
#26665 = CARTESIAN_POINT ( 'NONE',  ( 10.81189881249999907, 6.242252689847868297, -179.7187500020484094 ) ) ;
#26666 = CARTESIAN_POINT ( 'NONE',  ( 9.999999999999996447, -5.773502691896262640, -64.00000000409679046 ) ) ;
#26667 = CARTESIAN_POINT ( 'NONE',  ( -2.121150477449813534E-15, -11.54700538379251284, -179.3750000000000000 ) ) ;
#26668 = CARTESIAN_POINT ( 'NONE',  ( -5.000000000000003553, -8.660254037844383745, -175.3750000040967905 ) ) ;
#26669 = CARTESIAN_POINT ( 'NONE',  ( 5.405949406249999534, 9.363379034771803333, -79.28125000204838102 ) ) ;
#26670 = CARTESIAN_POINT ( 'NONE',  ( -5.405949406250003975, -9.363379034771801557, -56.03125000204836681 ) ) ;
#26671 = CARTESIAN_POINT ( 'NONE',  ( 7.070501591499377789E-16, 11.54700538379251284, -53.00000000409676915 ) ) ;
#26672 = CARTESIAN_POINT ( 'NONE',  ( 5.405949406249992428, -9.363379034771808662, -12.09375000204834727 ) ) ;
#26673 = CARTESIAN_POINT ( 'NONE',  ( 9.999999999999998224, 0.000000000000000000, -137.3750000040967905 ) ) ;
#26674 = CARTESIAN_POINT ( 'NONE',  ( -5.405949406250003975, -9.363379034771801557, -188.0312500020484094 ) ) ;
#26675 = CARTESIAN_POINT ( 'NONE',  ( -2.293366432827344421E-15, -12.48450537969573659, -9.406250002048365033 ) ) ;
#26676 = CARTESIAN_POINT ( 'NONE',  ( 4.999999999999992006, -8.660254037844389075, -172.1250000040968189 ) ) ;
#26677 = CARTESIAN_POINT ( 'NONE',  ( -2.121150477449813534E-15, -11.54700538379251284, -117.8749999999999858 ) ) ;
#26678 = LINE ( 'NONE', #10262, #41449 ) ;
#26679 = LINE ( 'NONE', #26262, #36918 ) ;
#26680 = CARTESIAN_POINT ( 'NONE',  ( -9.999999999999998224, 5.773502691896259087, -167.8749999999999716 ) ) ;
#26681 = DIRECTION ( 'NONE',  ( -0.000000000000000000, -0.000000000000000000, 1.000000000000000000 ) ) ;
#26683 = ORIENTED_EDGE ( 'NONE', *, *, #11564, .T. ) ;
#26682 = CARTESIAN_POINT ( 'NONE',  ( -10.81189881249999729, 1.324075727343319199E-15, -93.78125000204838102 ) ) ;
#26684 = CARTESIAN_POINT ( 'NONE',  ( -4.999999999999996447, 8.660254037844387298, -106.8750000040967763 ) ) ;
#26686 = ORIENTED_EDGE ( 'NONE', *, *, #4445, .T. ) ;
#26685 = CARTESIAN_POINT ( 'NONE',  ( -2.121150477449813534E-15, -11.54700538379251284, -153.8749999999999716 ) ) ;
#26687 = ORIENTED_EDGE ( 'NONE', *, *, #2237, .T. ) ;
#26688 = CARTESIAN_POINT ( 'NONE',  ( 7.644554776091147741E-16, 12.48450537969573659, -33.96875000204834549 ) ) ;
#26689 = CARTESIAN_POINT ( 'NONE',  ( -2.293366432827344421E-15, -12.48450537969573659, -22.90625000204837747 ) ) ;
#26690 = CARTESIAN_POINT ( 'NONE',  ( 10.81189881249999907, 6.242252689847868297, -68.71875000204838102 ) ) ;
#26691 = DIRECTION ( 'NONE',  ( -0.000000000000000000, -0.000000000000000000, 1.000000000000000000 ) ) ;
#26692 = EDGE_CURVE ( 'NONE', #37209, #3867, #28073, .T. ) ;
#26693 = CARTESIAN_POINT ( 'NONE',  ( -10.81189881249999729, 6.242252689847871849, -195.7187500020484379 ) ) ;
#26694 = CARTESIAN_POINT ( 'NONE',  ( -5.405949406249996869, 9.363379034771805109, -150.8437500020483810 ) ) ;
#26695 = ADVANCED_FACE ( 'NONE', ( #8218 ), #1749, .T. ) ;
#26696 = CARTESIAN_POINT ( 'NONE',  ( 9.999999999999479527, 5.773502691896553074, -99.37499999999995737 ) ) ;
#26697 = CARTESIAN_POINT ( 'NONE',  ( -10.00000000000076916, 5.773502691895813221, -112.3749999999999858 ) ) ;
#26698 = CARTESIAN_POINT ( 'NONE',  ( 10.81189881249999551, -6.242252689847874514, -151.6562500020484094 ) ) ;
#26699 = CARTESIAN_POINT ( 'NONE',  ( -2.121150477449813534E-15, -11.54700538379251284, 0.2499999959032573882 ) ) ;
#26700 = CARTESIAN_POINT ( 'NONE',  ( 7.644554776091147741E-16, 12.48450537969573659, -123.9687500020483952 ) ) ;
#26701 = CARTESIAN_POINT ( 'NONE',  ( 0.000000000000000000, 0.000000000000000000, -99.99999999999998579 ) ) ;
#26702 = CARTESIAN_POINT ( 'NONE',  ( -5.405949406249996869, 9.363379034771805109, -94.03125000204838102 ) ) ;
#26703 = CARTESIAN_POINT ( 'NONE',  ( -2.293366432827344421E-15, -12.48450537969573659, -106.7187500020483668 ) ) ;
#26704 = CARTESIAN_POINT ( 'NONE',  ( -5.405949406250003975, -9.363379034771801557, -72.34375000204836681 ) ) ;
#26705 = CARTESIAN_POINT ( 'NONE',  ( -10.81189881249999729, 6.242252689847871849, -74.40625000204836681 ) ) ;
#26706 = CARTESIAN_POINT ( 'NONE',  ( -4.999999999999996447, 8.660254037844387298, -159.3750000040967905 ) ) ;
#26707 = CARTESIAN_POINT ( 'NONE',  ( 9.999999999999998224, 0.000000000000000000, -115.9999999999999858 ) ) ;
#26708 = CARTESIAN_POINT ( 'NONE',  ( -10.81189881249999729, -6.242252689847864744, -159.6562500020484094 ) ) ;
#26709 = CARTESIAN_POINT ( 'NONE',  ( -5.405949406249996869, 9.363379034771805109, -173.5312500020484094 ) ) ;
#26710 = CARTESIAN_POINT ( 'NONE',  ( 4.999999999999992006, -8.660254037844389075, -189.7500000000000000 ) ) ;
#26711 = CARTESIAN_POINT ( 'NONE',  ( 10.81189881249999551, -6.242252689847874514, -1.468750002048352377 ) ) ;
#26712 = DIRECTION ( 'NONE',  ( -0.000000000000000000, -0.000000000000000000, 1.000000000000000000 ) ) ;
#26713 = CARTESIAN_POINT ( 'NONE',  ( 10.81189881249999729, 0.000000000000000000, -103.3437500020483668 ) ) ;
#26714 = CARTESIAN_POINT ( 'NONE',  ( -9.999999999999998224, 1.224646799147353059E-15, -82.24999999999998579 ) ) ;
#26715 = CARTESIAN_POINT ( 'NONE',  ( 7.644554776091147741E-16, 12.48450537969573659, -5.656250002048362369 ) ) ;
#26716 = CARTESIAN_POINT ( 'NONE',  ( 9.999999999999996447, -5.773502691896262640, -89.50000000409676204 ) ) ;
#26717 = CARTESIAN_POINT ( 'NONE',  ( -9.999999999999996447, 5.773502691896259975, -168.2500000040968189 ) ) ;
#26718 = CARTESIAN_POINT ( 'NONE',  ( -2.293366432827344421E-15, -12.48450537969573659, -108.4062500020483810 ) ) ;
#26719 = CARTESIAN_POINT ( 'NONE',  ( 5.405949406249992428, -9.363379034771808662, -87.28125000204838102 ) ) ;
#26720 = VERTEX_POINT ( 'NONE', #14876 ) ;
#26721 = CARTESIAN_POINT ( 'NONE',  ( 9.999999999999998224, 0.000000000000000000, -84.87500000409677625 ) ) ;
#26722 = CYLINDRICAL_SURFACE ( 'NONE', #11216, 9.999999999999998224 ) ;
#26723 = CARTESIAN_POINT ( 'NONE',  ( -2.293366432827344421E-15, -12.48450537969573659, -45.21875000204835970 ) ) ;
#26724 = VERTEX_POINT ( 'NONE', #14899 ) ;
#26725 = CARTESIAN_POINT ( 'NONE',  ( -9.999999999999998224, 5.773502691896259087, -5.874999999999963585 ) ) ;
#26726 = CARTESIAN_POINT ( 'NONE',  ( 9.999999999999996447, -5.773502691896262640, -141.6250000000000000 ) ) ;
#26727 = LINE ( 'NONE', #211, #1390 ) ;
#26728 = EDGE_CURVE ( 'NONE', #11948, #14436, #28098, .T. ) ;
#26729 = CARTESIAN_POINT ( 'NONE',  ( -2.121150477449813534E-15, -11.54700538379251284, -10.25000000409676026 ) ) ;
#26730 = CARTESIAN_POINT ( 'NONE',  ( -9.999999999999998224, 1.224646799147353059E-15, -193.2500000000000000 ) ) ;
#26731 = CARTESIAN_POINT ( 'NONE',  ( 9.999999999999479527, 5.773502691896553074, -96.37499999999997158 ) ) ;
#26733 = ORIENTED_EDGE ( 'NONE', *, *, #538, .F. ) ;
#26732 = CARTESIAN_POINT ( 'NONE',  ( 5.405949406249992428, -9.363379034771808662, -118.7812500020483952 ) ) ;
#26734 = VECTOR ( 'NONE', #28037, 1000.000000000000000 ) ;
#26735 = CARTESIAN_POINT ( 'NONE',  ( -10.00000000000102496, 5.773502691895664007, -22.75000000409674072 ) ) ;
#26736 = AXIS2_PLACEMENT_3D ( 'NONE', #33187, #10074, #10280 ) ;
#26737 =( BOUNDED_CURVE ( )  B_SPLINE_CURVE ( 2, ( #2331, #22589, #35766, #41362, #8587, #35344, #15460 ),
 .UNSPECIFIED., .F., .F. ) 
 B_SPLINE_CURVE_WITH_KNOTS ( ( 3, 2, 2, 3 ),
 ( 0.4925373134328359104, 0.4937810945273632957, 0.4950248756218906809, 0.4962686567164180107 ),
 .UNSPECIFIED. ) 
 CURVE ( )  GEOMETRIC_REPRESENTATION_ITEM ( )  RATIONAL_B_SPLINE_CURVE ( ( 0.9999999999999880096, 0.8660254037844506980, 1.000000000000000000, 0.8660254037844387076, 1.000000000000000000, 0.8660254037844267172, 1.000000000000011990 ) ) 
 REPRESENTATION_ITEM ( '' )  );
#26738 = ORIENTED_EDGE ( 'NONE', *, *, #40405, .F. ) ;
#26739 = CARTESIAN_POINT ( 'NONE',  ( 5.405949406249992428, -9.363379034771808662, -45.28125000204838102 ) ) ;
#26740 = APPROVAL_DATE_TIME ( #13553, #15389 ) ;
#26741 = CARTESIAN_POINT ( 'NONE',  ( 10.81189881249999907, 6.242252689847868297, -95.71875000204838102 ) ) ;
#26742 = CARTESIAN_POINT ( 'NONE',  ( 7.644554776091147741E-16, 12.48450537969573659, -127.1562500020483810 ) ) ;
#26744 = VERTEX_POINT ( 'NONE', #31979 ) ;
#26743 = ADVANCED_FACE ( 'NONE', ( #24652 ), #41864, .T. ) ;
#26745 = CARTESIAN_POINT ( 'NONE',  ( 9.999999999999998224, 0.000000000000000000, -132.5000000000000000 ) ) ;
#26746 = CARTESIAN_POINT ( 'NONE',  ( 5.000000000000000000, 8.660254037844385522, -78.24999999999998579 ) ) ;
#26747 = EDGE_CURVE ( 'NONE', #17891, #18350, #3087, .T. ) ;
#26748 = CARTESIAN_POINT ( 'NONE',  ( 10.81189881249999907, 6.242252689847868297, -172.4062500020484094 ) ) ;
#26749 = CARTESIAN_POINT ( 'NONE',  ( 7.070501591499376803E-16, 11.54700538379251284, -14.00000000409676382 ) ) ;
#26750 = EDGE_CURVE ( 'NONE', #32882, #25640, #2843, .T. ) ;
#26751 = CARTESIAN_POINT ( 'NONE',  ( 7.644554776091147741E-16, 12.48450537969573659, -134.4687500020483810 ) ) ;
#26752 = CARTESIAN_POINT ( 'NONE',  ( -10.81189881249999907, -6.242252689847864744, -90.46875000204836681 ) ) ;
#26753 = CARTESIAN_POINT ( 'NONE',  ( -2.121150477449813534E-15, -11.54700538379251284, -44.37499999999997158 ) ) ;
#26754 = CARTESIAN_POINT ( 'NONE',  ( -2.293366432827344421E-15, -12.48450537969573659, -99.40625000204839523 ) ) ;
#26755 = CARTESIAN_POINT ( 'NONE',  ( -9.999999999999998224, 5.773502691896259087, -183.2500000040968189 ) ) ;
#26756 = CARTESIAN_POINT ( 'NONE',  ( 10.81189881249999729, 6.242252689847867408, -116.7187500020483810 ) ) ;
#26757 = CARTESIAN_POINT ( 'NONE',  ( 10.81189881249999729, 0.000000000000000000, -181.5312500020483810 ) ) ;
#26758 = CARTESIAN_POINT ( 'NONE',  ( -9.999999999999998224, 1.224646799147353059E-15, -2.749999999999974687 ) ) ;
#26759 = LINE ( 'NONE', #37100, #3837 ) ;
#26760 = CARTESIAN_POINT ( 'NONE',  ( 10.81189881249999907, 6.242252689847868297, -197.9062500020484379 ) ) ;
#26761 = CARTESIAN_POINT ( 'NONE',  ( 10.81189881249999551, -6.242252689847874514, -58.46875000204836681 ) ) ;
#26762 = CARTESIAN_POINT ( 'NONE',  ( 10.81189881249999907, 6.242252689847868297, -43.21875000204835970 ) ) ;
#26763 = CARTESIAN_POINT ( 'NONE',  ( 7.070501591499377789E-16, 11.54700538379251284, -179.0000000040967905 ) ) ;
#26764 = CARTESIAN_POINT ( 'NONE',  ( -10.81189881249999907, -6.242252689847864744, -17.15625000204838102 ) ) ;
#26765 = CARTESIAN_POINT ( 'NONE',  ( 5.405949406249992428, -9.363379034771808662, -33.09375000204836681 ) ) ;
#26766 = LINE ( 'NONE', #39919, #30255 ) ;
#26767 = CARTESIAN_POINT ( 'NONE',  ( -5.405949406249996869, 9.363379034771805109, -126.8437500020483952 ) ) ;
#26768 = CARTESIAN_POINT ( 'NONE',  ( -9.999999999999998224, 1.224646799147353059E-15, -107.7499999999999858 ) ) ;
#26769 = CARTESIAN_POINT ( 'NONE',  ( -5.405949406249996869, 9.363379034771805109, -40.03125000204838102 ) ) ;
#26770 = CIRCLE ( 'NONE', #33680, 20.00000000000000355 ) ;
#26771 = CARTESIAN_POINT ( 'NONE',  ( 9.999999999999998224, 0.000000000000000000, -48.87500000409678336 ) ) ;
#26772 = CARTESIAN_POINT ( 'NONE',  ( -4.999999999999996447, 8.660254037844387298, -56.99999999999996447 ) ) ;
#26773 = CARTESIAN_POINT ( 'NONE',  ( -5.405949406250003975, -9.363379034771801557, -131.0312500020484094 ) ) ;
#26774 = CARTESIAN_POINT ( 'NONE',  ( 10.81189881249999551, -6.242252689847874514, -108.1562500020483810 ) ) ;
#26775 = ADVANCED_FACE ( 'NONE', ( #28738 ), #4242, .T. ) ;
#26776 = EDGE_LOOP ( 'NONE', ( #35328, #15735, #27961, #36324 ) ) ;
#26777 = CARTESIAN_POINT ( 'NONE',  ( 0.000000000000000000, 0.000000000000000000, -200.0000000000000000 ) ) ;
#26778 = CARTESIAN_POINT ( 'NONE',  ( 9.999999999999998224, 0.000000000000000000, -105.8750000040967763 ) ) ;
#26779 = CARTESIAN_POINT ( 'NONE',  ( -9.999999999999998224, 1.224646799147353059E-15, -146.7500000000000000 ) ) ;
#26780 = CARTESIAN_POINT ( 'NONE',  ( -5.405949406249996869, 9.363379034771805109, -63.84375000204836681 ) ) ;
#26781 = ORIENTED_EDGE ( 'NONE', *, *, #40656, .F. ) ;
#26782 = CARTESIAN_POINT ( 'NONE',  ( 4.999999999999992006, -8.660254037844389075, -30.74999999999997158 ) ) ;
#26783 = CARTESIAN_POINT ( 'NONE',  ( -2.293366432827344421E-15, -12.48450537969573659, -31.90625000204835970 ) ) ;
#26784 = CARTESIAN_POINT ( 'NONE',  ( -9.999999999999998224, 1.224646799147353059E-15, -124.6250000040967763 ) ) ;
#26785 = CARTESIAN_POINT ( 'NONE',  ( 5.000000000000000000, 8.660254037844385522, -36.62500000409676915 ) ) ;
#26786 =( BOUNDED_CURVE ( )  B_SPLINE_CURVE ( 2, ( #5926, #32052, #2481, #32258, #12586, #15609, #32474 ),
 .UNSPECIFIED., .F., .F. ) 
 B_SPLINE_CURVE_WITH_KNOTS ( ( 3, 2, 2, 3 ),
 ( 0.5037313432835821558, 0.5049751243781095411, 0.5062189054726369264, 0.5074626865671643117 ),
 .UNSPECIFIED. ) 
 CURVE ( )  GEOMETRIC_REPRESENTATION_ITEM ( )  RATIONAL_B_SPLINE_CURVE ( ( 0.9999999999999880096, 0.8660254037844506980, 1.000000000000000000, 0.8660254037844387076, 1.000000000000000000, 0.8660254037844267172, 1.000000000000011990 ) ) 
 REPRESENTATION_ITEM ( '' )  );
#26787 = LINE ( 'NONE', #21534, #10715 ) ;
#26788 = CARTESIAN_POINT ( 'NONE',  ( -5.405949406250003975, -9.363379034771801557, -144.5312500020483810 ) ) ;
#26789 = CARTESIAN_POINT ( 'NONE',  ( -9.999999999999479527, -5.773502691896549521, -124.1249999999999858 ) ) ;
#26790 = ORIENTED_EDGE ( 'NONE', *, *, #20159, .T. ) ;
#26791 =( BOUNDED_CURVE ( )  B_SPLINE_CURVE ( 2, ( #4545, #31749, #23610, #31102, #1534, #27857, #1752 ),
 .UNSPECIFIED., .F., .F. ) 
 B_SPLINE_CURVE_WITH_KNOTS ( ( 3, 2, 2, 3 ),
 ( 0.8246268656716420065, 0.8258706467661693917, 0.8271144278606967770, 0.8283582089552240513 ),
 .UNSPECIFIED. ) 
 CURVE ( )  GEOMETRIC_REPRESENTATION_ITEM ( )  RATIONAL_B_SPLINE_CURVE ( ( 0.9999999999999761302, 0.8660254037844625774, 1.000000000000000000, 0.8660254037844387076, 1.000000000000000000, 0.8660254037844148378, 1.000000000000023981 ) ) 
 REPRESENTATION_ITEM ( '' )  );
#26792 = VERTEX_POINT ( 'NONE', #15536 ) ;
#26793 = VECTOR ( 'NONE', #3306, 1000.000000000000000 ) ;
#26794 = CARTESIAN_POINT ( 'NONE',  ( 9.999999999999998224, 1.224646799147353059E-15, -99.99999999999998579 ) ) ;
#26795 = CARTESIAN_POINT ( 'NONE',  ( -2.121150477449813534E-15, -11.54700538379251284, -104.3749999999999858 ) ) ;
#26796 = CARTESIAN_POINT ( 'NONE',  ( -10.81189881249999729, 1.324075727343319199E-15, -164.0937500020484094 ) ) ;
#26797 = CARTESIAN_POINT ( 'NONE',  ( -5.405949406250003975, -9.363379034771801557, -194.0312500020484094 ) ) ;
#26798 = CARTESIAN_POINT ( 'NONE',  ( 7.644554776091147741E-16, 12.48450537969573659, -20.46875000204836326 ) ) ;
#26799 = CARTESIAN_POINT ( 'NONE',  ( -9.999999999999998224, 1.224646799147353059E-15, -122.7500000000000000 ) ) ;
#26800 = CARTESIAN_POINT ( 'NONE',  ( 10.00000000000000000, 5.773502691896255534, -171.3750000000000000 ) ) ;
#26801 = CARTESIAN_POINT ( 'NONE',  ( 10.81189881249999551, -6.242252689847874514, -157.4687500020484379 ) ) ;
#26802 = CARTESIAN_POINT ( 'NONE',  ( 5.405949406249992428, -9.363379034771808662, -135.0937500020483810 ) ) ;
#26803 = CARTESIAN_POINT ( 'NONE',  ( -9.999999999999479527, -5.773502691896549521, -116.6249999999999574 ) ) ;
#26804 = CARTESIAN_POINT ( 'NONE',  ( -5.405949406250003975, -9.363379034771801557, -121.8437500020483952 ) ) ;
#26805 = CARTESIAN_POINT ( 'NONE',  ( 5.405949406249999534, 9.363379034771803333, 0.4062499979516354109 ) ) ;
#26806 = CARTESIAN_POINT ( 'NONE',  ( -5.405949406249996869, 9.363379034771805109, -131.5312500020484094 ) ) ;
#26807 = CARTESIAN_POINT ( 'NONE',  ( -10.81189881249999729, 1.324075727343319199E-15, -9.593750002048345493 ) ) ;
#26808 = CARTESIAN_POINT ( 'NONE',  ( -5.405949406249996869, 9.363379034771805109, -138.8437500020484094 ) ) ;
#26809 = CARTESIAN_POINT ( 'NONE',  ( 9.999999999999998224, 0.000000000000000000, -165.8750000040967905 ) ) ;
#26810 = CARTESIAN_POINT ( 'NONE',  ( 9.999999999999998224, 0.000000000000000000, -195.8750000040967905 ) ) ;
#26811 = CARTESIAN_POINT ( 'NONE',  ( -4.999999999999996447, 8.660254037844387298, -159.0000000000000000 ) ) ;
#26812 = ADVANCED_FACE ( 'NONE', ( #34787 ), #9083, .T. ) ;
#26813 = CARTESIAN_POINT ( 'NONE',  ( -2.293366432827344421E-15, -12.48450537969573659, -81.21875000204838102 ) ) ;
#26814 = CARTESIAN_POINT ( 'NONE',  ( -10.81189881249999907, -6.242252689847864744, -76.96875000204836681 ) ) ;
#26815 = CARTESIAN_POINT ( 'NONE',  ( 10.81189881249999729, 0.000000000000000000, -43.53125000204838102 ) ) ;
#26816 = CARTESIAN_POINT ( 'NONE',  ( -5.405949406250003975, -9.363379034771801557, -52.84375000204835970 ) ) ;
#26817 = CARTESIAN_POINT ( 'NONE',  ( 4.999999999999992006, -8.660254037844389075, -113.6250000040967763 ) ) ;
#26818 = CARTESIAN_POINT ( 'NONE',  ( -10.81189881249999729, 1.324075727343319199E-15, -161.0937500020484094 ) ) ;
#26819 = CARTESIAN_POINT ( 'NONE',  ( 9.999999999999996447, -5.773502691896262640, -129.6250000000000000 ) ) ;
#26820 = CARTESIAN_POINT ( 'NONE',  ( 5.405949406249992428, -9.363379034771808662, -135.2812500020483810 ) ) ;
#26821 = CARTESIAN_POINT ( 'NONE',  ( -2.121150477449813534E-15, -11.54700538379251284, -86.37499999999997158 ) ) ;
#26822 = CARTESIAN_POINT ( 'NONE',  ( 10.81189881249999729, 6.242252689847867408, -16.40625000204838102 ) ) ;
#26823 = VERTEX_POINT ( 'NONE', #18143 ) ;
#26824 = CARTESIAN_POINT ( 'NONE',  ( -10.81189881249999729, 1.324075727343319199E-15, -113.2812500020483952 ) ) ;
#26825 = CARTESIAN_POINT ( 'NONE',  ( 9.999999999999998224, 0.000000000000000000, -131.3750000040967905 ) ) ;
#26826 = CARTESIAN_POINT ( 'NONE',  ( -9.999999999999998224, 1.224646799147353059E-15, -112.2499999999999858 ) ) ;
#26827 = CARTESIAN_POINT ( 'NONE',  ( 5.000000000000000000, 8.660254037844385522, -41.12500000409677625 ) ) ;
#26828 = DIRECTION ( 'NONE',  ( -1.000000000000000000, 0.000000000000000000, 0.000000000000000000 ) ) ;
#26829 = CARTESIAN_POINT ( 'NONE',  ( -10.81189881249999729, 6.242252689847871849, -48.90625000204836681 ) ) ;
#26830 = CARTESIAN_POINT ( 'NONE',  ( 9.999999999999998224, 0.000000000000000000, -135.5000000000000000 ) ) ;
#26831 = CARTESIAN_POINT ( 'NONE',  ( -5.405949406250003975, -9.363379034771801557, -164.0312500020484094 ) ) ;
#26832 = VECTOR ( 'NONE', #20425, 1000.000000000000000 ) ;
#26833 = CARTESIAN_POINT ( 'NONE',  ( -10.81189881249999907, -6.242252689847864744, -133.9687500020483810 ) ) ;
#26834 = CARTESIAN_POINT ( 'NONE',  ( -2.121150477449813534E-15, -11.54700538379251284, -80.75000000409677625 ) ) ;
#26835 = CARTESIAN_POINT ( 'NONE',  ( 5.000000000000000000, 8.660254037844385522, -151.7500000000000000 ) ) ;
#26836 = ORIENTED_EDGE ( 'NONE', *, *, #10650, .T. ) ;
#26837 = CARTESIAN_POINT ( 'NONE',  ( 5.000000000000000000, 8.660254037844385522, -114.6250000040967763 ) ) ;
#26838 = VECTOR ( 'NONE', #21235, 1000.000000000000000 ) ;
#26840 = ORIENTED_EDGE ( 'NONE', *, *, #41781, .F. ) ;
#26839 = CARTESIAN_POINT ( 'NONE',  ( 10.81189881249999907, 6.242252689847868297, -65.90625000204839523 ) ) ;
#26841 = DATE_AND_TIME ( #32899, #38675 ) ;
#26843 = ORIENTED_EDGE ( 'NONE', *, *, #25344, .T. ) ;
#26842 = CARTESIAN_POINT ( 'NONE',  ( 7.644554776091147741E-16, 12.48450537969573659, -120.9687500020483952 ) ) ;
#26844 = CARTESIAN_POINT ( 'NONE',  ( 5.405949406249999534, 9.363379034771803333, -23.59375000204835970 ) ) ;
#26845 = CARTESIAN_POINT ( 'NONE',  ( 10.81189881249999907, 6.242252689847868297, -197.7187500020484094 ) ) ;
#26846 = CARTESIAN_POINT ( 'NONE',  ( -10.81189881249999729, 6.242252689847871849, -48.71875000204835970 ) ) ;
#26847 = DIRECTION ( 'NONE',  ( 1.000000000000000000, 0.000000000000000000, 0.000000000000000000 ) ) ;
#26848 = CARTESIAN_POINT ( 'NONE',  ( -9.999999999999998224, 1.224646799147353059E-15, -31.62500000409676559 ) ) ;
#26849 = CARTESIAN_POINT ( 'NONE',  ( -5.405949406249996869, 9.363379034771805109, -176.3437500020483810 ) ) ;
#26850 = CARTESIAN_POINT ( 'NONE',  ( 7.644554776091147741E-16, 12.48450537969573659, -159.9687500020483810 ) ) ;
#26851 =( BOUNDED_CURVE ( )  B_SPLINE_CURVE ( 2, ( #24185, #10990, #4527, #13793, #30864, #33897, #21136 ),
 .UNSPECIFIED., .F., .F. ) 
 B_SPLINE_CURVE_WITH_KNOTS ( ( 3, 2, 2, 3 ),
 ( 0.1529850746268656692, 0.1542288557213930267, 0.1554726368159203842, 0.1567164179104477695 ),
 .UNSPECIFIED. ) 
 CURVE ( )  GEOMETRIC_REPRESENTATION_ITEM ( )  RATIONAL_B_SPLINE_CURVE ( ( 1.000000000000000000, 0.8660254037844387076, 1.000000000000000000, 0.8660254037844387076, 1.000000000000000000, 0.8660254037844387076, 1.000000000000000000 ) ) 
 REPRESENTATION_ITEM ( '' )  );
#26852 = CARTESIAN_POINT ( 'NONE',  ( -10.81189881249999729, 1.324075727343319199E-15, -152.0937500020483810 ) ) ;
#26853 = CARTESIAN_POINT ( 'NONE',  ( 10.81189881249999551, -6.242252689847874514, -160.4687500020484094 ) ) ;
#26854 = CARTESIAN_POINT ( 'NONE',  ( -9.999999999999998224, 1.224646799147353059E-15, -106.6250000040967763 ) ) ;
#26855 = DIRECTION ( 'NONE',  ( 1.000000000000000000, 0.000000000000000000, 0.000000000000000000 ) ) ;
#26856 = CARTESIAN_POINT ( 'NONE',  ( 9.999999999999996447, -5.773502691896262640, -177.6250000000000000 ) ) ;
#26857 = AXIS2_PLACEMENT_3D ( 'NONE', #10627, #7844, #27905 ) ;
#26858 = CARTESIAN_POINT ( 'NONE',  ( 10.81189881249999551, -6.242252689847874514, -98.96875000204838102 ) ) ;
#26859 = CARTESIAN_POINT ( 'NONE',  ( -8.675003188131697129, -4.974413003141672895, -0.0003472602639886801512 ) ) ;
#26860 = CARTESIAN_POINT ( 'NONE',  ( -10.81189881249999729, 6.242252689847871849, -68.40625000204840944 ) ) ;
#26861 = CARTESIAN_POINT ( 'NONE',  ( 5.000000000000000000, 8.660254037844385522, -168.6250000040967905 ) ) ;
#26862 = CARTESIAN_POINT ( 'NONE',  ( 10.81189881249999729, 0.000000000000000000, -182.8437500020483810 ) ) ;
#26863 = CARTESIAN_POINT ( 'NONE',  ( -2.293366432827344421E-15, -12.48450537969573659, -118.9062500020483952 ) ) ;
#26864 = CARTESIAN_POINT ( 'NONE',  ( 10.81189881249999551, -6.242252689847874514, -159.1562500020484094 ) ) ;
#26865 = CARTESIAN_POINT ( 'NONE',  ( -10.81189881249999729, 6.242252689847871849, -50.40625000204837391 ) ) ;
#26866 = CARTESIAN_POINT ( 'NONE',  ( 7.070501591499377789E-16, 11.54700538379251284, -138.5000000040967905 ) ) ;
#26867 = CARTESIAN_POINT ( 'NONE',  ( -9.999999999999998224, 1.224646799147353059E-15, -104.7499999999999858 ) ) ;
#26868 = ORIENTED_EDGE ( 'NONE', *, *, #14669, .F. ) ;
#26869 = CARTESIAN_POINT ( 'NONE',  ( -10.81189881249999729, 6.242252689847871849, -135.9062500020484094 ) ) ;
#26870 = CARTESIAN_POINT ( 'NONE',  ( -2.293366432827344421E-15, -12.48450537969573659, -144.4062500020484094 ) ) ;
#26871 = CARTESIAN_POINT ( 'NONE',  ( -10.81189881249999907, -6.242252689847864744, -188.1562500020484094 ) ) ;
#26872 = CARTESIAN_POINT ( 'NONE',  ( 10.81189881249999729, 0.000000000000000000, -79.34375000204838102 ) ) ;
#26873 = EDGE_LOOP ( 'NONE', ( #6672, #40881, #30732, #3123 ) ) ;
#26874 = CARTESIAN_POINT ( 'NONE',  ( -2.121150477449813534E-15, -11.54700538379251284, -60.87499999999998579 ) ) ;
#26875 = CARTESIAN_POINT ( 'NONE',  ( 7.644554776091147741E-16, 12.48450537969573659, -177.9687500020483810 ) ) ;
#26876 = CARTESIAN_POINT ( 'NONE',  ( 9.999999999999996447, -5.773502691896262640, -67.00000000409676204 ) ) ;
#26877 = CARTESIAN_POINT ( 'NONE',  ( -9.999999999999998224, 1.224646799147353059E-15, -110.7499999999999858 ) ) ;
#26878 = CARTESIAN_POINT ( 'NONE',  ( -2.121150477449813534E-15, -11.54700538379251284, -175.2500000040968189 ) ) ;
#26879 = CARTESIAN_POINT ( 'NONE',  ( 10.81189881249999907, 6.242252689847868297, -74.90625000204839523 ) ) ;
#26880 = CARTESIAN_POINT ( 'NONE',  ( -10.81189881249999729, 6.242252689847871849, -57.90625000204837391 ) ) ;
#26881 = CARTESIAN_POINT ( 'NONE',  ( -4.999999999999996447, 8.660254037844387298, -55.87500000409676204 ) ) ;
#26882 = CARTESIAN_POINT ( 'NONE',  ( 10.81189881249999551, -6.242252689847874514, -11.96875000204836326 ) ) ;
#26883 = FACE_OUTER_BOUND ( 'NONE', #32226, .T. ) ;
#26884 = CARTESIAN_POINT ( 'NONE',  ( -10.81189881249999729, 6.242252689847871849, -186.9062500020484094 ) ) ;
#26885 = CARTESIAN_POINT ( 'NONE',  ( -10.81189881249999907, -6.242252689847864744, -8.156250002048365033 ) ) ;
#26886 = CARTESIAN_POINT ( 'NONE',  ( 0.000000000000000000, 0.000000000000000000, -99.99999999999998579 ) ) ;
#26887 = CARTESIAN_POINT ( 'NONE',  ( 9.999999999999998224, 0.000000000000000000, -200.0000000000000000 ) ) ;
#26888 = CARTESIAN_POINT ( 'NONE',  ( 9.999999999999479527, 5.773502691896553074, -177.7500000040967620 ) ) ;
#26889 = CARTESIAN_POINT ( 'NONE',  ( 9.999999999999998224, 0.000000000000000000, -200.0000000000000000 ) ) ;
#26890 = AXIS2_PLACEMENT_3D ( 'NONE', #15040, #12025, #24577 ) ;
#26892 = VERTEX_POINT ( 'NONE', #31768 ) ;
#26891 = CARTESIAN_POINT ( 'NONE',  ( 10.81189881249999551, -6.242252689847874514, -94.65625000204838102 ) ) ;
#26894 = VERTEX_POINT ( 'NONE', #11452 ) ;
#26893 = CARTESIAN_POINT ( 'NONE',  ( 1.351487262974977233, 10.72709830801206543, -100.0000000000000000 ) ) ;
#26895 = ORIENTED_EDGE ( 'NONE', *, *, #4394, .T. ) ;
#26896 =( BOUNDED_CURVE ( )  B_SPLINE_CURVE ( 2, ( #8934, #27933, #24923, #12151, #11725, #2465, #15171 ),
 .UNSPECIFIED., .F., .F. ) 
 B_SPLINE_CURVE_WITH_KNOTS ( ( 3, 2, 2, 3 ),
 ( 0.2500000000000001110, 0.2512437810945274963, 0.2524875621890548261, 0.2537313432835822113 ),
 .UNSPECIFIED. ) 
 CURVE ( )  GEOMETRIC_REPRESENTATION_ITEM ( )  RATIONAL_B_SPLINE_CURVE ( ( 0.9999999999999880096, 0.8660254037844506980, 1.000000000000000000, 0.8660254037844387076, 1.000000000000000000, 0.8660254037844267172, 1.000000000000011990 ) ) 
 REPRESENTATION_ITEM ( '' )  );
#26897 = CARTESIAN_POINT ( 'NONE',  ( 5.405949406249992428, -9.363379034771808662, -22.59375000204835615 ) ) ;
#26898 = CARTESIAN_POINT ( 'NONE',  ( -10.81189881249999729, 1.324075727343319199E-15, -20.28125000204836326 ) ) ;
#26899 = CARTESIAN_POINT ( 'NONE',  ( -2.293366432827344421E-15, -12.48450537969573659, -73.71875000204835260 ) ) ;
#26900 = CARTESIAN_POINT ( 'NONE',  ( -9.999999999999998224, 1.224646799147353059E-15, -115.6250000040967905 ) ) ;
#26901 = CARTESIAN_POINT ( 'NONE',  ( -10.00000000000000000, -5.773502691896251982, -46.12499999999997158 ) ) ;
#26902 = CARTESIAN_POINT ( 'NONE',  ( -2.293366432827344421E-15, -12.48450537969573659, -192.2187500020484379 ) ) ;
#26903 = CARTESIAN_POINT ( 'NONE',  ( 5.405949406249999534, 9.363379034771803333, -152.5937500020483810 ) ) ;
#26904 = DIRECTION ( 'NONE',  ( -0.000000000000000000, -0.000000000000000000, -1.000000000000000000 ) ) ;
#26905 = CARTESIAN_POINT ( 'NONE',  ( -9.999999999999996447, 5.773502691896259975, -172.3750000000000568 ) ) ;
#26906 = CARTESIAN_POINT ( 'NONE',  ( 5.405949406249992428, -9.363379034771808662, -147.2812500020483810 ) ) ;
#26907 = CARTESIAN_POINT ( 'NONE',  ( -2.121150477449813534E-15, -11.54700538379251284, -4.250000004096763817 ) ) ;
#26908 = DIRECTION ( 'NONE',  ( -0.000000000000000000, -0.000000000000000000, -1.000000000000000000 ) ) ;
#26909 = CARTESIAN_POINT ( 'NONE',  ( -10.81189881249999729, 6.242252689847871849, -123.7187500020483952 ) ) ;
#26910 = DIRECTION ( 'NONE',  ( -0.000000000000000000, -0.000000000000000000, 1.000000000000000000 ) ) ;
#26911 = CARTESIAN_POINT ( 'NONE',  ( -10.81189881249999729, 1.324075727343319199E-15, -90.78125000204838102 ) ) ;
#26912 = CARTESIAN_POINT ( 'NONE',  ( 5.405949406249999534, 9.363379034771803333, -97.09375000204838102 ) ) ;
#26913 = CARTESIAN_POINT ( 'NONE',  ( 10.81189881249999907, 6.242252689847868297, -71.71875000204836681 ) ) ;
#26914 = CARTESIAN_POINT ( 'NONE',  ( -5.405949406249996869, 9.363379034771805109, -74.53125000204838102 ) ) ;
#26915 = CARTESIAN_POINT ( 'NONE',  ( 4.999999999999992006, -8.660254037844389075, -163.1250000040967905 ) ) ;
#26916 = CARTESIAN_POINT ( 'NONE',  ( 7.644554776091147741E-16, 12.48450537969573659, -158.6562500020484094 ) ) ;
#26917 = CARTESIAN_POINT ( 'NONE',  ( -5.405949406249996869, 9.363379034771805109, -170.5312500020484094 ) ) ;
#26918 = CARTESIAN_POINT ( 'NONE',  ( -10.00000000000015987, 5.773502691896167605, -192.2500000040968473 ) ) ;
#26919 = CARTESIAN_POINT ( 'NONE',  ( -9.999999999999998224, 1.224646799147353059E-15, -146.7500000000000000 ) ) ;
#26920 = CARTESIAN_POINT ( 'NONE',  ( 9.999999999999998224, 0.000000000000000000, -108.4999999999999858 ) ) ;
#26921 = CARTESIAN_POINT ( 'NONE',  ( 5.405949406249999534, 9.363379034771803333, -103.0937500020483810 ) ) ;
#26922 = CARTESIAN_POINT ( 'NONE',  ( -5.000000000000003553, -8.660254037844383745, -81.99999999999998579 ) ) ;
#26923 = CARTESIAN_POINT ( 'NONE',  ( 5.405949406249992428, -9.363379034771808662, -3.281250002048374803 ) ) ;
#26924 = CARTESIAN_POINT ( 'NONE',  ( 10.00000000000000000, 5.773502691896255534, -87.75000000409677625 ) ) ;
#26925 = VECTOR ( 'NONE', #4432, 1000.000000000000000 ) ;
#26926 = CARTESIAN_POINT ( 'NONE',  ( 7.070501591499376803E-16, 11.54700538379251284, -168.5000000040967620 ) ) ;
#26927 = CARTESIAN_POINT ( 'NONE',  ( 10.81189881249999907, 6.242252689847868297, -103.4062500020483952 ) ) ;
#26928 = CARTESIAN_POINT ( 'NONE',  ( -10.81189881249999729, 1.324075727343319199E-15, -81.78125000204839523 ) ) ;
#26929 = CARTESIAN_POINT ( 'NONE',  ( -9.999999999999998224, 5.773502691896259087, -73.75000000409676204 ) ) ;
#26930 = CARTESIAN_POINT ( 'NONE',  ( -9.999999999999998224, 1.224646799147353059E-15, -133.6250000040967620 ) ) ;
#26931 = CARTESIAN_POINT ( 'NONE',  ( -5.405949406250003975, -9.363379034771801557, -37.84375000204837391 ) ) ;
#26932 = ORIENTED_EDGE ( 'NONE', *, *, #10920, .F. ) ;
#26933 = CARTESIAN_POINT ( 'NONE',  ( -5.000000000000003553, -8.660254037844383745, -12.99999999999995559 ) ) ;
#26934 = CARTESIAN_POINT ( 'NONE',  ( 5.405949406249992428, -9.363379034771808662, -27.28125000204836681 ) ) ;
#26935 = EDGE_CURVE ( 'NONE', #22340, #26513, #20724, .T. ) ;
#26936 = CARTESIAN_POINT ( 'NONE',  ( -10.00000000000000000, -5.773502691896251982, -148.1249999999999716 ) ) ;
#26937 = DIRECTION ( 'NONE',  ( 1.000000000000000000, 0.000000000000000000, 0.000000000000000000 ) ) ;
#26938 = CARTESIAN_POINT ( 'NONE',  ( 4.999999999999992006, -8.660254037844389075, -16.12500000409675138 ) ) ;
#26939 = EDGE_CURVE ( 'NONE', #20834, #28118, #39747, .T. ) ;
#26940 = CARTESIAN_POINT ( 'NONE',  ( 10.00000000000000000, 5.773502691896255534, -192.3750000000000000 ) ) ;
#26941 = CARTESIAN_POINT ( 'NONE',  ( 5.000000000000000000, 8.660254037844385522, -123.2500000000000000 ) ) ;
#26943 = ORIENTED_EDGE ( 'NONE', *, *, #6913, .T. ) ;
#26942 = CARTESIAN_POINT ( 'NONE',  ( 10.81189881249999907, 6.242252689847868297, -115.4062500020484094 ) ) ;
#26944 = CARTESIAN_POINT ( 'NONE',  ( -10.00000000000154188, 5.773502691895366468, -13.37499999999992717 ) ) ;
#26945 = ORIENTED_EDGE ( 'NONE', *, *, #27596, .F. ) ;
#26946 = VERTEX_POINT ( 'NONE', #1985 ) ;
#26947 = CARTESIAN_POINT ( 'NONE',  ( -10.81189881249999729, 6.242252689847871849, -42.90625000204838102 ) ) ;
#26948 = DATE_TIME_ROLE ( 'creation_date' ) ;
#26949 = AXIS2_PLACEMENT_3D ( 'NONE', #22337, #41319, #34875 ) ;
#26950 = CARTESIAN_POINT ( 'NONE',  ( 10.81189881249999907, 6.242252689847868297, -92.71875000204836681 ) ) ;
#26951 = CARTESIAN_POINT ( 'NONE',  ( 10.81189881249999729, 6.242252689847867408, -119.9062500020483810 ) ) ;
#26952 = ORIENTED_EDGE ( 'NONE', *, *, #19280, .T. ) ;
#26953 = CARTESIAN_POINT ( 'NONE',  ( 9.999999999999998224, 0.000000000000000000, -51.87500000409675494 ) ) ;
#26954 = CARTESIAN_POINT ( 'NONE',  ( -2.293366432827344421E-15, -12.48450537969573659, -198.2187500020484094 ) ) ;
#26955 = CARTESIAN_POINT ( 'NONE',  ( 7.644554776091147741E-16, 12.48450537969573659, -172.1562500020484094 ) ) ;
#26956 = DIRECTION ( 'NONE',  ( 0.000000000000000000, 1.000000000000000000, 0.000000000000000000 ) ) ;
#26957 = CARTESIAN_POINT ( 'NONE',  ( -2.293366432827344421E-15, -12.48450537969573659, -133.7187500020483810 ) ) ;
#26958 = CARTESIAN_POINT ( 'NONE',  ( 7.644554776091147741E-16, 12.48450537969573659, -95.46875000204839523 ) ) ;
#26959 = CARTESIAN_POINT ( 'NONE',  ( 10.81189881249999729, 0.000000000000000000, -99.03125000204839523 ) ) ;
#26960 = CARTESIAN_POINT ( 'NONE',  ( -9.999999999999998224, 1.224646799147353059E-15, -183.1250000040967905 ) ) ;
#26961 = CARTESIAN_POINT ( 'NONE',  ( -10.81189881249999729, 1.324075727343319199E-15, -105.5937500020483810 ) ) ;
#26962 = CARTESIAN_POINT ( 'NONE',  ( -5.405949406250003975, -9.363379034771801557, -176.0312500020483810 ) ) ;
#26963 = DIRECTION ( 'NONE',  ( 0.000000000000000000, 0.000000000000000000, 1.000000000000000000 ) ) ;
#26964 = CARTESIAN_POINT ( 'NONE',  ( -10.81189881249999729, -6.242252689847864744, -179.1562500020484094 ) ) ;
#26965 = CARTESIAN_POINT ( 'NONE',  ( 10.81189881249999907, 6.242252689847868297, -194.9062500020484379 ) ) ;
#26966 = CARTESIAN_POINT ( 'NONE',  ( 10.81189881249999551, -6.242252689847874514, -61.46875000204838813 ) ) ;
#26967 = CARTESIAN_POINT ( 'NONE',  ( -10.81189881249999729, 6.242252689847871849, -41.21875000204834549 ) ) ;
#26968 = CARTESIAN_POINT ( 'NONE',  ( -2.121150477449813534E-15, -11.54700538379251284, -175.2500000040968189 ) ) ;
#26969 = CARTESIAN_POINT ( 'NONE',  ( 5.405949406249999534, 9.363379034771803333, -16.28125000204835970 ) ) ;
#26970 = CARTESIAN_POINT ( 'NONE',  ( -10.81189881249999729, 6.242252689847871849, -21.71875000204837036 ) ) ;
#26971 = LINE ( 'NONE', #40129, #6797 ) ;
#26972 = CARTESIAN_POINT ( 'NONE',  ( 10.81189881249999551, -6.242252689847874514, -127.4687500020483810 ) ) ;
#26973 = CARTESIAN_POINT ( 'NONE',  ( -4.999999999999996447, 8.660254037844387298, -107.9999999999999858 ) ) ;
#26974 = CARTESIAN_POINT ( 'NONE',  ( 10.81189881249999729, 0.000000000000000000, -30.03125000204837036 ) ) ;
#26975 = DIRECTION ( 'NONE',  ( -0.000000000000000000, -0.000000000000000000, 1.000000000000000000 ) ) ;
#26976 = CARTESIAN_POINT ( 'NONE',  ( 7.070501591499377789E-16, 11.54700538379251284, -61.62499999999998579 ) ) ;
#26977 = CARTESIAN_POINT ( 'NONE',  ( -5.405949406249996869, 9.363379034771805109, -124.0312500020483952 ) ) ;
#26978 = CARTESIAN_POINT ( 'NONE',  ( 5.405949406249992428, -9.363379034771808662, -109.7812500020483810 ) ) ;
#26979 = ORIENTED_EDGE ( 'NONE', *, *, #42434, .F. ) ;
#26980 = VECTOR ( 'NONE', #18391, 1000.000000000000000 ) ;
#26981 = CARTESIAN_POINT ( 'NONE',  ( 0.000000000000000000, 0.000000000000000000, -200.0000000000000000 ) ) ;
#26982 = CARTESIAN_POINT ( 'NONE',  ( 5.000000000000000000, 8.660254037844385522, -98.12500000409677625 ) ) ;
#26983 = DIRECTION ( 'NONE',  ( 0.000000000000000000, 1.000000000000000000, 0.000000000000000000 ) ) ;
#26984 = CARTESIAN_POINT ( 'NONE',  ( -10.81189881249999729, 1.324075727343319199E-15, -62.09375000204836681 ) ) ;
#26985 = ORIENTED_EDGE ( 'NONE', *, *, #9191, .T. ) ;
#26986 = CARTESIAN_POINT ( 'NONE',  ( 7.070501591499377789E-16, 11.54700538379251284, -36.12499999999996447 ) ) ;
#26987 = PRODUCT_DEFINITION_FORMATION_WITH_SPECIFIED_SOURCE ( 'ANY', '', #18390, .NOT_KNOWN. ) ;
#26988 = EDGE_CURVE ( 'NONE', #18833, #13430, #33718, .T. ) ;
#26989 = EDGE_CURVE ( 'NONE', #30038, #39101, #36728, .T. ) ;
#26990 = CARTESIAN_POINT ( 'NONE',  ( 10.81189881249999729, 6.242252689847867408, -35.90625000204835260 ) ) ;
#26991 = ADVANCED_FACE ( 'NONE', ( #29569 ), #21498, .T. ) ;
#26992 = LINE ( 'NONE', #33913, #13160 ) ;
#26993 =( BOUNDED_CURVE ( )  B_SPLINE_CURVE ( 2, ( #15673, #15465, #25838, #28666, #2962, #18932, #21748 ),
 .UNSPECIFIED., .F., .F. ) 
 B_SPLINE_CURVE_WITH_KNOTS ( ( 3, 2, 2, 3 ),
 ( 0.4291044776119404269, 0.4303482587064677567, 0.4315920398009951975, 0.4328358208955225273 ),
 .UNSPECIFIED. ) 
 CURVE ( )  GEOMETRIC_REPRESENTATION_ITEM ( )  RATIONAL_B_SPLINE_CURVE ( ( 0.9999999999999880096, 0.8660254037844506980, 1.000000000000000000, 0.8660254037844387076, 1.000000000000000000, 0.8660254037844207220, 1.000000000000017986 ) ) 
 REPRESENTATION_ITEM ( '' )  );
#26994 = CARTESIAN_POINT ( 'NONE',  ( 9.999999999999998224, 0.000000000000000000, -36.87500000409676915 ) ) ;
#26995 = EDGE_CURVE ( 'NONE', #36343, #2376, #1710, .T. ) ;
#26996 = EDGE_CURVE ( 'NONE', #41377, #17005, #16369, .T. ) ;
#26997 = CARTESIAN_POINT ( 'NONE',  ( 24.99999999999999645, 3.061616997868382648E-15, -99.99999999999998579 ) ) ;
#26998 = AXIS2_PLACEMENT_3D ( 'NONE', #10169, #17059, #20095 ) ;
#26999 = CARTESIAN_POINT ( 'NONE',  ( 10.81189881249999907, 6.242252689847868297, -143.9062500020484094 ) ) ;
#27000 = PRODUCT_RELATED_PRODUCT_CATEGORY ( 'detail', '', ( #31497 ) ) ;
#27001 = CARTESIAN_POINT ( 'NONE',  ( -9.999999999999998224, 1.224646799147353059E-15, -105.1250000040967763 ) ) ;
#27002 = EDGE_LOOP ( 'NONE', ( #16130, #2602, #15858, #1141 ) ) ;
#27003 = VERTEX_POINT ( 'NONE', #22669 ) ;
#27004 = EDGE_CURVE ( 'NONE', #18939, #26093, #12924, .T. ) ;
#27005 = CARTESIAN_POINT ( 'NONE',  ( -10.00000000000051337, 5.773502691895962435, -113.8749999999999858 ) ) ;
#27006 = AXIS2_PLACEMENT_3D ( 'NONE', #13978, #33456, #30847 ) ;
#27007 = CARTESIAN_POINT ( 'NONE',  ( -9.999999999999998224, 1.224646799147353059E-15, -147.1250000040967905 ) ) ;
#27008 = CARTESIAN_POINT ( 'NONE',  ( 10.81189881249999729, 0.000000000000000000, -163.3437500020484094 ) ) ;
#27009 = EDGE_CURVE ( 'NONE', #19531, #1650, #6686, .T. ) ;
#27010 = CARTESIAN_POINT ( 'NONE',  ( -5.405949406249996869, 9.363379034771805109, -197.5312500020484094 ) ) ;
#27011 = CARTESIAN_POINT ( 'NONE',  ( 7.644554776091147741E-16, 12.48450537969573659, -18.96875000204837391 ) ) ;
#27012 = CARTESIAN_POINT ( 'NONE',  ( -4.999999999999996447, 8.660254037844387298, -171.0000000000000000 ) ) ;
#27013 = CARTESIAN_POINT ( 'NONE',  ( -5.405949406250003975, -9.363379034771801557, -154.8437500020483810 ) ) ;
#27014 = CARTESIAN_POINT ( 'NONE',  ( -10.81189881249999729, 6.242252689847871849, -137.2187500020483810 ) ) ;
#27015 = CARTESIAN_POINT ( 'NONE',  ( -9.999999999999998224, 1.224646799147353059E-15, -116.7499999999999858 ) ) ;
#27016 = CARTESIAN_POINT ( 'NONE',  ( -5.405949406250003975, -9.363379034771801557, -118.8437500020483810 ) ) ;
#27017 = CARTESIAN_POINT ( 'NONE',  ( 5.000000000000000000, 8.660254037844385522, -197.1250000040967905 ) ) ;
#27018 = CARTESIAN_POINT ( 'NONE',  ( -2.293366432827344421E-15, -12.48450537969573659, -124.9062500020483810 ) ) ;
#27020 = CARTESIAN_POINT ( 'NONE',  ( -5.405949406250003975, -9.363379034771801557, -7.843750002048343717 ) ) ;
#27019 =( BOUNDED_CURVE ( )  B_SPLINE_CURVE ( 2, ( #2968, #28462, #8599, #16095, #41595, #38367, #18937 ),
 .UNSPECIFIED., .F., .F. ) 
 B_SPLINE_CURVE_WITH_KNOTS ( ( 3, 2, 2, 3 ),
 ( 0.1753731343283582433, 0.1766169154228856009, 0.1778606965174129861, 0.1791044776119403437 ),
 .UNSPECIFIED. ) 
 CURVE ( )  GEOMETRIC_REPRESENTATION_ITEM ( )  RATIONAL_B_SPLINE_CURVE ( ( 0.9999999999999970024, 0.8660254037844417052, 1.000000000000000000, 0.8660254037844387076, 1.000000000000000000, 0.8660254037844327124, 1.000000000000005995 ) ) 
 REPRESENTATION_ITEM ( '' )  );
#27021 = CARTESIAN_POINT ( 'NONE',  ( 10.81189881249999729, 0.000000000000000000, -137.8437500020484094 ) ) ;
#27022 = CARTESIAN_POINT ( 'NONE',  ( 10.81189881249999729, 6.242252689847867408, -199.4062500020484379 ) ) ;
#27023 = CARTESIAN_POINT ( 'NONE',  ( 9.999999999999227285, 5.773502691896701400, -110.2500000040967478 ) ) ;
#27024 = CARTESIAN_POINT ( 'NONE',  ( 9.999999999999996447, -5.773502691896262640, -156.6250000000000000 ) ) ;
#27025 = CARTESIAN_POINT ( 'NONE',  ( -9.999999999999998224, 1.224646799147353059E-15, -23.74999999999996447 ) ) ;
#27026 = AXIS2_PLACEMENT_3D ( 'NONE', #6444, #3843, #16977 ) ;
#27027 = CARTESIAN_POINT ( 'NONE',  ( -10.81189881249999729, -6.242252689847864744, -85.96875000204836681 ) ) ;
#27028 = CARTESIAN_POINT ( 'NONE',  ( 5.405949406249992428, -9.363379034771808662, -67.59375000204836681 ) ) ;
#27029 = DIRECTION ( 'NONE',  ( -1.000000000000000000, 0.000000000000000000, -0.000000000000000000 ) ) ;
#27030 = CARTESIAN_POINT ( 'NONE',  ( 10.81189881249999729, 0.000000000000000000, -42.03125000204838102 ) ) ;
#27031 = CARTESIAN_POINT ( 'NONE',  ( 10.81189881249999729, 0.000000000000000000, -47.84375000204838102 ) ) ;
#27032 = CARTESIAN_POINT ( 'NONE',  ( 10.81189881249999729, 0.000000000000000000, -199.3437500020484094 ) ) ;
#27033 = CARTESIAN_POINT ( 'NONE',  ( 10.81189881249999729, 0.000000000000000000, -151.3437500020483810 ) ) ;
#27034 = CARTESIAN_POINT ( 'NONE',  ( 5.000000000000000000, 8.660254037844385522, -130.7499999999999716 ) ) ;
#27035 = CARTESIAN_POINT ( 'NONE',  ( -5.405949406250003975, -9.363379034771801557, -128.0312500020484094 ) ) ;
#27036 = EDGE_CURVE ( 'NONE', #39976, #22389, #14919, .T. ) ;
#27037 = CARTESIAN_POINT ( 'NONE',  ( 9.999999999999998224, 0.000000000000000000, -94.99999999999998579 ) ) ;
#27038 = CARTESIAN_POINT ( 'NONE',  ( -10.00000000000000000, -5.773502691896251982, -83.62499999999998579 ) ) ;
#27039 = CARTESIAN_POINT ( 'NONE',  ( 10.81189881249999729, 6.242252689847867408, -19.40625000204837747 ) ) ;
#27040 = VERTEX_POINT ( 'NONE', #2822 ) ;
#27041 =( BOUNDED_CURVE ( )  B_SPLINE_CURVE ( 2, ( #11957, #35074, #18436, #25147, #21894, #8949, #21679 ),
 .UNSPECIFIED., .F., .F. ) 
 B_SPLINE_CURVE_WITH_KNOTS ( ( 3, 2, 2, 3 ),
 ( 0.2201492537313433639, 0.2213930348258707215, 0.2226368159203980790, 0.2238805970149254365 ),
 .UNSPECIFIED. ) 
 CURVE ( )  GEOMETRIC_REPRESENTATION_ITEM ( )  RATIONAL_B_SPLINE_CURVE ( ( 0.9999999999999910072, 0.8660254037844477004, 1.000000000000000000, 0.8660254037844387076, 1.000000000000000000, 0.8660254037844327124, 1.000000000000005995 ) ) 
 REPRESENTATION_ITEM ( '' )  );
#27042 = CARTESIAN_POINT ( 'NONE',  ( -2.293366432827344421E-15, -12.48450537969573659, -111.4062500020483952 ) ) ;
#27043 = CARTESIAN_POINT ( 'NONE',  ( 7.070501591499377789E-16, 11.54700538379251284, -129.5000000040967620 ) ) ;
#27044 = CARTESIAN_POINT ( 'NONE',  ( -9.999999999999998224, 1.224646799147353059E-15, -178.2500000000000284 ) ) ;
#27045 = CARTESIAN_POINT ( 'NONE',  ( 4.999999999999992006, -8.660254037844389075, -44.62500000409677625 ) ) ;
#27046 = CARTESIAN_POINT ( 'NONE',  ( 10.00000000000102318, -5.773502691895667560, -58.00000000409673362 ) ) ;
#27047 = CARTESIAN_POINT ( 'NONE',  ( -5.405949406250003975, -9.363379034771801557, -48.53125000204838813 ) ) ;
#27048 = AXIS2_PLACEMENT_3D ( 'NONE', #32547, #22189, #12448 ) ;
#27049 =( BOUNDED_CURVE ( )  B_SPLINE_CURVE ( 2, ( #20767, #33956, #4378, #30716, #11048, #41682, #9107 ),
 .UNSPECIFIED., .F., .F. ) 
 B_SPLINE_CURVE_WITH_KNOTS ( ( 3, 2, 2, 3 ),
 ( 0.9477611940298510396, 0.9490049751243784248, 0.9502487562189058101, 0.9514925373134331954 ),
 .UNSPECIFIED. ) 
 CURVE ( )  GEOMETRIC_REPRESENTATION_ITEM ( )  RATIONAL_B_SPLINE_CURVE ( ( 0.9999999999999641398, 0.8660254037844745678, 1.000000000000000000, 0.8660254037844387076, 1.000000000000000000, 0.8660254037844028474, 1.000000000000035971 ) ) 
 REPRESENTATION_ITEM ( '' )  );
#27050 = CARTESIAN_POINT ( 'NONE',  ( 10.00000000000102318, -5.773502691895667560, -40.00000000409673362 ) ) ;
#27051 = CARTESIAN_POINT ( 'NONE',  ( -5.405949406250003975, -9.363379034771801557, -153.5312500020484094 ) ) ;
#27052 = CARTESIAN_POINT ( 'NONE',  ( -5.405949406250003975, -9.363379034771801557, -138.3437500020484094 ) ) ;
#27053 = CARTESIAN_POINT ( 'NONE',  ( -2.121150477449813534E-15, -11.54700538379251284, -195.8750000000000284 ) ) ;
#27054 = ORIENTED_EDGE ( 'NONE', *, *, #9872, .F. ) ;
#27055 = CIRCLE ( 'NONE', #5010, 5.000000000000002665 ) ;
#27056 = EDGE_CURVE ( 'NONE', #36297, #22119, #33022, .T. ) ;
#27058 = ORIENTED_EDGE ( 'NONE', *, *, #9872, .T. ) ;
#27057 = CARTESIAN_POINT ( 'NONE',  ( -5.405949406249996869, 9.363379034771805109, -61.03125000204837391 ) ) ;
#27059 = SHAPE_DEFINITION_REPRESENTATION ( #24960, #12816 ) ;
#27061 = ORIENTED_EDGE ( 'NONE', *, *, #37295, .F. ) ;
#27060 = CARTESIAN_POINT ( 'NONE',  ( 10.81189881249999551, -6.242252689847874514, -113.9687500020483810 ) ) ;
#27062 = CARTESIAN_POINT ( 'NONE',  ( -10.81189881249999729, 6.242252689847871849, -18.71875000204837036 ) ) ;
#27063 = CARTESIAN_POINT ( 'NONE',  ( 10.81189881249999551, -6.242252689847874514, -193.4687500020484094 ) ) ;
#27064 = CARTESIAN_POINT ( 'NONE',  ( 5.405949406249999534, 9.363379034771803333, -50.59375000204835260 ) ) ;
#27065 = CARTESIAN_POINT ( 'NONE',  ( -10.00000000000102496, 5.773502691895664007, -61.75000000409674783 ) ) ;
#27066 = CARTESIAN_POINT ( 'NONE',  ( 10.00000000000102318, -5.773502691895667560, -31.00000000409671586 ) ) ;
#27067 = CARTESIAN_POINT ( 'NONE',  ( -5.405949406249996869, 9.363379034771805109, -179.3437500020483810 ) ) ;
#27068 = CARTESIAN_POINT ( 'NONE',  ( 10.81189881249999907, 6.242252689847868297, -161.7187500020483810 ) ) ;
#27069 = CARTESIAN_POINT ( 'NONE',  ( 10.81189881249999907, 6.242252689847868297, -139.2187500020484094 ) ) ;
#27070 = CARTESIAN_POINT ( 'NONE',  ( -5.405949406249996869, 9.363379034771805109, -165.8437500020484094 ) ) ;
#27071 = CARTESIAN_POINT ( 'NONE',  ( -9.999999999999998224, 1.224646799147353059E-15, -86.74999999999998579 ) ) ;
#27072 = CARTESIAN_POINT ( 'NONE',  ( -5.000000000000003553, -8.660254037844383745, -139.3750000040968189 ) ) ;
#27073 = CARTESIAN_POINT ( 'NONE',  ( -2.121150477449813534E-15, -11.54700538379251284, -179.3750000000000284 ) ) ;
#27074 = CARTESIAN_POINT ( 'NONE',  ( 10.81189881249999907, 6.242252689847868297, -89.71875000204836681 ) ) ;
#27075 = CARTESIAN_POINT ( 'NONE',  ( -2.121150477449813534E-15, -11.54700538379251284, -72.87499999999997158 ) ) ;
#27076 = CARTESIAN_POINT ( 'NONE',  ( 10.81189881249999729, 0.000000000000000000, -66.03125000204838102 ) ) ;
#27077 = CARTESIAN_POINT ( 'NONE',  ( 0.000000000000000000, 0.000000000000000000, -99.99999999999998579 ) ) ;
#27078 = CARTESIAN_POINT ( 'NONE',  ( 5.405949406249992428, -9.363379034771808662, -175.5937500020484094 ) ) ;
#27079 = CARTESIAN_POINT ( 'NONE',  ( -5.405949406249996869, 9.363379034771805109, -125.5312500020483952 ) ) ;
#27080 = CARTESIAN_POINT ( 'NONE',  ( 5.405949406249992428, -9.363379034771808662, -162.2812500020484094 ) ) ;
#27081 = CARTESIAN_POINT ( 'NONE',  ( -10.81189881249999907, -6.242252689847864744, -48.65625000204836681 ) ) ;
#27082 = CARTESIAN_POINT ( 'NONE',  ( -2.121150477449813534E-15, -11.54700538379251284, -136.2500000040967620 ) ) ;
#27083 = CARTESIAN_POINT ( 'NONE',  ( 4.999999999999992006, -8.660254037844389075, -104.2499999999999858 ) ) ;
#27084 = ORIENTED_EDGE ( 'NONE', *, *, #20111, .T. ) ;
#27085 = CARTESIAN_POINT ( 'NONE',  ( 10.81189881249999729, 6.242252689847867408, -136.4062500020484094 ) ) ;
#27086 = CARTESIAN_POINT ( 'NONE',  ( -5.405949406250003975, -9.363379034771801557, -150.5312500020483810 ) ) ;
#27087 = CARTESIAN_POINT ( 'NONE',  ( -2.293366432827344421E-15, -12.48450537969573659, -186.4062500020484094 ) ) ;
#27088 = CARTESIAN_POINT ( 'NONE',  ( -10.81189881249999729, 1.324075727343319199E-15, -83.09375000204836681 ) ) ;
#27089 = ORIENTED_EDGE ( 'NONE', *, *, #7198, .F. ) ;
#27090 = CARTESIAN_POINT ( 'NONE',  ( 10.00000000000000000, 5.773502691896255534, -51.37499999999999289 ) ) ;
#27091 = CARTESIAN_POINT ( 'NONE',  ( 10.81189881249999907, 6.242252689847868297, -178.2187500020483810 ) ) ;
#27092 = CARTESIAN_POINT ( 'NONE',  ( -9.999999999999998224, 1.224646799147353059E-15, -63.12500000409676204 ) ) ;
#27093 = CARTESIAN_POINT ( 'NONE',  ( -9.999999999999227285, -5.773502691896698735, -110.6249999999999574 ) ) ;
#27094 = CARTESIAN_POINT ( 'NONE',  ( 4.999999999999992006, -8.660254037844389075, -165.7500000000000000 ) ) ;
#27095 = CARTESIAN_POINT ( 'NONE',  ( 7.644554776091147741E-16, 12.48450537969573659, -79.15625000204838102 ) ) ;
#27096 = CARTESIAN_POINT ( 'NONE',  ( 10.81189881249999551, -6.242252689847874514, -63.15625000204837391 ) ) ;
#27097 = CARTESIAN_POINT ( 'NONE',  ( 9.999999999999998224, 0.000000000000000000, -51.87500000409675494 ) ) ;
#27098 = CARTESIAN_POINT ( 'NONE',  ( 7.644554776091147741E-16, 12.48450537969573659, -6.968750002048357040 ) ) ;
#27099 = CARTESIAN_POINT ( 'NONE',  ( -10.00000000000102496, 5.773502691895664007, -88.37499999999997158 ) ) ;
#27100 = CARTESIAN_POINT ( 'NONE',  ( -10.81189881249999729, 6.242252689847871849, -176.4062500020484094 ) ) ;
#27101 = CARTESIAN_POINT ( 'NONE',  ( 10.81189881249999551, -6.242252689847874514, -3.156250002048361036 ) ) ;
#27102 = CARTESIAN_POINT ( 'NONE',  ( 4.999999999999992006, -8.660254037844389075, -73.12500000409677625 ) ) ;
#27103 = CARTESIAN_POINT ( 'NONE',  ( 9.999999999999998224, 0.000000000000000000, -48.87500000409678336 ) ) ;
#27104 = CARTESIAN_POINT ( 'NONE',  ( 10.00000000000102318, -5.773502691895667560, -103.0000000040967194 ) ) ;
#27105 = CARTESIAN_POINT ( 'NONE',  ( 5.000000000000000000, 8.660254037844385522, -177.6250000040968189 ) ) ;
#27106 = CARTESIAN_POINT ( 'NONE',  ( 9.999999999999998224, 0.000000000000000000, -122.0000000000000000 ) ) ;
#27107 = ADVANCED_FACE ( 'NONE', ( #32399, #42291 ), #19628, .F. ) ;
#27109 = ORIENTED_EDGE ( 'NONE', *, *, #10646, .F. ) ;
#27108 = CARTESIAN_POINT ( 'NONE',  ( 7.644554776091147741E-16, 12.48450537969573659, -85.15625000204838102 ) ) ;
#27111 = VERTEX_POINT ( 'NONE', #2615 ) ;
#27110 = CARTESIAN_POINT ( 'NONE',  ( -9.999999999999612754, -5.773502691896474914, -154.1249999999999716 ) ) ;
#27112 =( BOUNDED_CURVE ( )  B_SPLINE_CURVE ( 2, ( #10814, #30694, #15116, #12307, #8462, #11457, #41231 ),
 .UNSPECIFIED., .F., .F. ) 
 B_SPLINE_CURVE_WITH_KNOTS ( ( 3, 2, 2, 3 ),
 ( 0.09701492537313441411, 0.09825870646766173000, 0.09950248756218905977, 0.1007462686567163757 ),
 .UNSPECIFIED. ) 
 CURVE ( )  GEOMETRIC_REPRESENTATION_ITEM ( )  RATIONAL_B_SPLINE_CURVE ( ( 0.9999999999999910072, 0.8660254037844477004, 1.000000000000000000, 0.8660254037844387076, 1.000000000000000000, 0.8660254037844431485, 0.9999999999999955591 ) ) 
 REPRESENTATION_ITEM ( '' )  );
#27113 = ORIENTED_EDGE ( 'NONE', *, *, #3754, .T. ) ;
#27114 = CARTESIAN_POINT ( 'NONE',  ( 7.644554776091147741E-16, 12.48450537969573659, -26.46875000204837747 ) ) ;
#27115 = CARTESIAN_POINT ( 'NONE',  ( 10.81189881249999907, 6.242252689847868297, -13.40625000204836326 ) ) ;
#27116 = CONTEXT_DEPENDENT_SHAPE_REPRESENTATION ( #26253, #27325 ) ;
#27117 = CARTESIAN_POINT ( 'NONE',  ( 5.405949406249999534, 9.363379034771803333, -70.09375000204836681 ) ) ;
#27118 = FACE_OUTER_BOUND ( 'NONE', #35922, .T. ) ;
#27119 = B_SPLINE_CURVE_WITH_KNOTS ( 'NONE', 3,
 ( #30707, #24453, #17085, #23799, #33950, #37599, #8043, #36954, #20544, #4583, #40181, #30503, #24669, #1353, #30918, #17512, #34377, #930, #14483, #1138, #33732, #27892, #14261, #27678, #37814, #20330, #14046, #7607, #10612 ),
 .UNSPECIFIED., .F., .F.,
 ( 4, 2, 2, 2, 2, 2, 2, 2, 2, 2, 2, 2, 1, 2, 4 ),
 ( 0.000000000000000000, 0.001276655870610494525, 0.002553311741220990350, 0.005106623482441982435, 0.006383279353052479128, 0.007659935223662975821, 0.008936591094273473382, 0.01021324696488396834, 0.01148990283549446330, 0.01276655870610495652, 0.01531987044732594644, 0.01659652631793644140, 0.01787318218854693636, 0.01914983805915743131, 0.02042649392976792627 ),
 .UNSPECIFIED. ) ;
#27120 = CARTESIAN_POINT ( 'NONE',  ( -2.121150477449813534E-15, -11.54700538379251284, -45.87499999999997158 ) ) ;
#27121 = CARTESIAN_POINT ( 'NONE',  ( -5.405949406250003975, -9.363379034771801557, -181.8437500020483810 ) ) ;
#27122 = ADVANCED_FACE ( 'NONE', ( #39273 ), #25910, .T. ) ;
#27123 = CYLINDRICAL_SURFACE ( 'NONE', #26736, 9.999999999999998224 ) ;
#27124 = CARTESIAN_POINT ( 'NONE',  ( -4.999999999999996447, 8.660254037844387298, -141.0000000000000000 ) ) ;
#27125 = CARTESIAN_POINT ( 'NONE',  ( 9.999999999999998224, 0.000000000000000000, -144.5000000000000000 ) ) ;
#27126 = CARTESIAN_POINT ( 'NONE',  ( 5.405949406249992428, -9.363379034771808662, -109.5937500020483810 ) ) ;
#27127 = CARTESIAN_POINT ( 'NONE',  ( 9.999999999999998224, 0.000000000000000000, -194.0000000000000000 ) ) ;
#27128 = CARTESIAN_POINT ( 'NONE',  ( -5.405949406250003975, -9.363379034771801557, -90.53125000204838102 ) ) ;
#27129 = CARTESIAN_POINT ( 'NONE',  ( 5.405949406249999534, 9.363379034771803333, -98.59375000204838102 ) ) ;
#27130 = CARTESIAN_POINT ( 'NONE',  ( -5.405949406249996869, 9.363379034771805109, -66.84375000204836681 ) ) ;
#27131 = CARTESIAN_POINT ( 'NONE',  ( -10.81189881249999729, 6.242252689847871849, -75.90625000204838102 ) ) ;
#27132 = CARTESIAN_POINT ( 'NONE',  ( -10.00000000000000000, -5.773502691896251982, -163.5000000040967620 ) ) ;
#27133 = CARTESIAN_POINT ( 'NONE',  ( 10.81189881249999729, 0.000000000000000000, -156.0312500020484094 ) ) ;
#27134 = CARTESIAN_POINT ( 'NONE',  ( 7.644554776091147741E-16, 12.48450537969573659, -175.1562500020484094 ) ) ;
#27135 = CARTESIAN_POINT ( 'NONE',  ( 5.405949406249992428, -9.363379034771808662, -1.593750002048366365 ) ) ;
#27136 = CARTESIAN_POINT ( 'NONE',  ( -9.999999999999479527, -5.773502691896549521, -149.6249999999999716 ) ) ;
#27137 = CARTESIAN_POINT ( 'NONE',  ( -5.405949406250003975, -9.363379034771801557, -109.8437500020483810 ) ) ;
#27138 = CARTESIAN_POINT ( 'NONE',  ( 9.999999999999998224, 0.000000000000000000, -156.5000000000000000 ) ) ;
#27139 = CARTESIAN_POINT ( 'NONE',  ( -9.999999999999998224, 1.224646799147353059E-15, -74.74999999999998579 ) ) ;
#27140 = CARTESIAN_POINT ( 'NONE',  ( -10.81189881249999907, -6.242252689847864744, -3.656250002048361036 ) ) ;
#27141 = CARTESIAN_POINT ( 'NONE',  ( -9.999999999999998224, 5.773502691896259087, -93.25000000409677625 ) ) ;
#27142 = CARTESIAN_POINT ( 'NONE',  ( -2.121150477449813534E-15, -11.54700538379251284, -95.75000000409677625 ) ) ;
#27143 = CARTESIAN_POINT ( 'NONE',  ( -5.405949406250003975, -9.363379034771801557, -99.53125000204839523 ) ) ;
#27144 = CARTESIAN_POINT ( 'NONE',  ( -5.405949406249996869, 9.363379034771805109, -82.03125000204839523 ) ) ;
#27145 = CARTESIAN_POINT ( 'NONE',  ( -9.999999999999998224, 1.224646799147353059E-15, -78.12500000409677625 ) ) ;
#27146 = CARTESIAN_POINT ( 'NONE',  ( -4.999999999999996447, 8.660254037844387298, -118.5000000000000000 ) ) ;
#27147 = CARTESIAN_POINT ( 'NONE',  ( 10.81189881249999907, 6.242252689847868297, -34.21875000204835260 ) ) ;
#27148 = ORIENTED_EDGE ( 'NONE', *, *, #17095, .T. ) ;
#27149 = CARTESIAN_POINT ( 'NONE',  ( 5.000000000000000000, 8.660254037844385522, -10.74999999999995381 ) ) ;
#27150 = EDGE_CURVE ( 'NONE', #25371, #16036, #7241, .T. ) ;
#27151 = CARTESIAN_POINT ( 'NONE',  ( -10.81189881249999729, 6.242252689847871849, -26.40625000204838102 ) ) ;
#27152 = CARTESIAN_POINT ( 'NONE',  ( -10.81189881249999729, 1.324075727343319199E-15, -9.593750002048345493 ) ) ;
#27153 = CARTESIAN_POINT ( 'NONE',  ( -9.999999999999998224, 5.773502691896259087, -4.750000004096754935 ) ) ;
#27154 = CARTESIAN_POINT ( 'NONE',  ( -5.405949406250003975, -9.363379034771801557, -135.5312500020484094 ) ) ;
#27155 =( BOUNDED_CURVE ( )  B_SPLINE_CURVE ( 2, ( #21080, #5116, #40703, #17613, #30808, #21723, #34906 ),
 .UNSPECIFIED., .F., .F. ) 
 B_SPLINE_CURVE_WITH_KNOTS ( ( 3, 2, 2, 3 ),
 ( 0.01119402985074628015, 0.01243781094527364461, 0.01368159203980100908, 0.01492537313432837180 ),
 .UNSPECIFIED. ) 
 CURVE ( )  GEOMETRIC_REPRESENTATION_ITEM ( )  RATIONAL_B_SPLINE_CURVE ( ( 0.9999999999999986677, 0.8660254037844400399, 1.000000000000000000, 0.8660254037844387076, 1.000000000000000000, 0.8660254037844372643, 1.000000000000001554 ) ) 
 REPRESENTATION_ITEM ( '' )  );
#27156 = ADVANCED_FACE ( 'NONE', ( #29789 ), #230, .T. ) ;
#27157 = CARTESIAN_POINT ( 'NONE',  ( 9.999999999999998224, 0.000000000000000000, -188.0000000000000000 ) ) ;
#27158 = CARTESIAN_POINT ( 'NONE',  ( 5.000000000000000000, 8.660254037844385522, -96.24999999999998579 ) ) ;
#27160 = ORIENTED_EDGE ( 'NONE', *, *, #20133, .T. ) ;
#27159 = CARTESIAN_POINT ( 'NONE',  ( -2.293366432827344421E-15, -12.48450537969573659, -106.9062500020483952 ) ) ;
#27161 = CARTESIAN_POINT ( 'NONE',  ( 9.999999999999998224, 0.000000000000000000, -36.87500000409676915 ) ) ;
#27162 = EDGE_LOOP ( 'NONE', ( #37619, #35507, #23279, #22391 ) ) ;
#27163 = ORIENTED_EDGE ( 'NONE', *, *, #713, .T. ) ;
#27164 = CARTESIAN_POINT ( 'NONE',  ( 10.81189881249999729, 0.000000000000000000, -45.03125000204838102 ) ) ;
#27165 = APPROVAL_ROLE ( '' ) ;
#27166 = CARTESIAN_POINT ( 'NONE',  ( 5.405949406249992428, -9.363379034771808662, -99.09375000204838102 ) ) ;
#27167 = CARTESIAN_POINT ( 'NONE',  ( -2.293366432827344421E-15, -12.48450537969573659, -124.9062500020483810 ) ) ;
#27168 = DIRECTION ( 'NONE',  ( -1.000000000000000000, 0.000000000000000000, 0.000000000000000000 ) ) ;
#27169 = CARTESIAN_POINT ( 'NONE',  ( 5.405949406249999534, 9.363379034771803333, -199.0937500020484094 ) ) ;
#27170 = CARTESIAN_POINT ( 'NONE',  ( 10.81189881249999907, 6.242252689847868297, -175.4062500020484094 ) ) ;
#27171 = CARTESIAN_POINT ( 'NONE',  ( 4.999999999999992006, -8.660254037844389075, -138.7499999999999716 ) ) ;
#27172 = EDGE_CURVE ( 'NONE', #38211, #31374, #38376, .T. ) ;
#27173 = CARTESIAN_POINT ( 'NONE',  ( 10.81189881249999729, 6.242252689847867408, -127.2187500020483810 ) ) ;
#27174 = CARTESIAN_POINT ( 'NONE',  ( -2.293366432827344421E-15, -12.48450537969573659, -91.71875000204838102 ) ) ;
#27175 = CARTESIAN_POINT ( 'NONE',  ( -4.999999999999996447, 8.660254037844387298, -106.4999999999999858 ) ) ;
#27176 = CARTESIAN_POINT ( 'NONE',  ( -2.293366432827344421E-15, -12.48450537969573659, -103.9062500020483810 ) ) ;
#27177 = CARTESIAN_POINT ( 'NONE',  ( -4.999999999999996447, 8.660254037844387298, -189.3750000040967905 ) ) ;
#27178 = CARTESIAN_POINT ( 'NONE',  ( -5.405949406249996869, 9.363379034771805109, -110.3437500020483810 ) ) ;
#27179 = CARTESIAN_POINT ( 'NONE',  ( -10.81189881249999729, -6.242252689847864744, -180.6562500020484094 ) ) ;
#27180 = CARTESIAN_POINT ( 'NONE',  ( -4.999999999999996447, 8.660254037844387298, -107.9999999999999858 ) ) ;
#27181 = CARTESIAN_POINT ( 'NONE',  ( 9.999999999999998224, 0.000000000000000000, -152.3750000040967905 ) ) ;
#27182 = CARTESIAN_POINT ( 'NONE',  ( -2.293366432827344421E-15, -12.48450537969573659, -192.4062500020484094 ) ) ;
#27183 = CARTESIAN_POINT ( 'NONE',  ( 7.644554776091147741E-16, 12.48450537969573659, -54.96875000204836681 ) ) ;
#27184 = CARTESIAN_POINT ( 'NONE',  ( 10.81189881249999729, 0.000000000000000000, -38.84375000204837391 ) ) ;
#27185 = CARTESIAN_POINT ( 'NONE',  ( -4.999999999999996447, 8.660254037844387298, -169.8750000040967905 ) ) ;
#27186 = CARTESIAN_POINT ( 'NONE',  ( 7.644554776091147741E-16, 12.48450537969573659, -10.15625000204837924 ) ) ;
#27187 = CARTESIAN_POINT ( 'NONE',  ( 10.81189881249999729, 0.000000000000000000, -25.34375000204835970 ) ) ;
#27188 = FACE_OUTER_BOUND ( 'NONE', #41189, .T. ) ;
#27189 = CARTESIAN_POINT ( 'NONE',  ( 7.644554776091147741E-16, 12.48450537969573659, -131.4687500020483810 ) ) ;
#27190 = CARTESIAN_POINT ( 'NONE',  ( 7.070501591499377789E-16, 11.54700538379251284, -97.62499999999997158 ) ) ;
#27191 = CARTESIAN_POINT ( 'NONE',  ( -10.81189881249999729, 1.324075727343319199E-15, -30.78125000204837036 ) ) ;
#27192 = DIRECTION ( 'NONE',  ( 1.000000000000000000, 0.000000000000000000, 0.000000000000000000 ) ) ;
#27193 = CARTESIAN_POINT ( 'NONE',  ( 10.00000000000000000, 5.773502691896255534, -55.87499999999997158 ) ) ;
#27194 = CARTESIAN_POINT ( 'NONE',  ( 10.81189881249999907, 6.242252689847868297, -121.4062500020483810 ) ) ;
#27195 = CARTESIAN_POINT ( 'NONE',  ( -2.293366432827344421E-15, -12.48450537969573659, -105.4062500020483810 ) ) ;
#27196 = ORIENTED_EDGE ( 'NONE', *, *, #39410, .T. ) ;
#27197 = DIRECTION ( 'NONE',  ( -0.000000000000000000, -0.000000000000000000, 1.000000000000000000 ) ) ;
#27198 = CARTESIAN_POINT ( 'NONE',  ( -5.000000000000003553, -8.660254037844383745, -101.8750000040967905 ) ) ;
#27199 = FACE_OUTER_BOUND ( 'NONE', #25797, .T. ) ;
#27200 = CARTESIAN_POINT ( 'NONE',  ( -10.81189881249999907, -6.242252689847864744, -60.46875000204838102 ) ) ;
#27201 = ORIENTED_EDGE ( 'NONE', *, *, #4394, .F. ) ;
#27202 = CARTESIAN_POINT ( 'NONE',  ( -10.00000000000000000, -5.773502691896251982, -37.12499999999995026 ) ) ;
#27203 = CARTESIAN_POINT ( 'NONE',  ( -10.81189881249999729, 6.242252689847871849, -35.40625000204836681 ) ) ;
#27204 = CARTESIAN_POINT ( 'NONE',  ( -9.999999999999998224, 1.224646799147353059E-15, -111.1250000040967763 ) ) ;
#27205 = CARTESIAN_POINT ( 'NONE',  ( 7.070501591499377789E-16, 11.54700538379251284, -26.00000000409677270 ) ) ;
#27206 = CARTESIAN_POINT ( 'NONE',  ( 9.999999999999994671, -5.773502691896262640, -138.6250000000000000 ) ) ;
#27207 = CARTESIAN_POINT ( 'NONE',  ( -10.81189881249999729, 1.324075727343319199E-15, -138.7812500020483810 ) ) ;
#27208 = CARTESIAN_POINT ( 'NONE',  ( 9.999999999999998224, 0.000000000000000000, -119.3750000040967905 ) ) ;
#27209 = VERTEX_POINT ( 'NONE', #20268 ) ;
#27210 = ORIENTED_EDGE ( 'NONE', *, *, #1586, .F. ) ;
#27211 = CARTESIAN_POINT ( 'NONE',  ( -57.00000000000002132, 7.164183775012018789E-15, -240.0000000000000000 ) ) ;
#27212 = CARTESIAN_POINT ( 'NONE',  ( -5.405949406250003975, -9.363379034771801557, -163.8437500020484094 ) ) ;
#27213 = AXIS2_PLACEMENT_3D ( 'NONE', #6654, #19804, #36431 ) ;
#27214 = CARTESIAN_POINT ( 'NONE',  ( 5.405949406249992428, -9.363379034771808662, -195.2812500020484094 ) ) ;
#27215 = ADVANCED_FACE ( 'NONE', ( #40318 ), #20051, .T. ) ;
#27216 = CARTESIAN_POINT ( 'NONE',  ( -2.293366432827344421E-15, -12.48450537969573659, -13.71875000204836503 ) ) ;
#27217 = CARTESIAN_POINT ( 'NONE',  ( -9.999999999999998224, 1.224646799147353059E-15, -200.0000000000000000 ) ) ;
#27218 = EDGE_CURVE ( 'NONE', #27040, #27517, #32595, .T. ) ;
#27219 = CARTESIAN_POINT ( 'NONE',  ( -2.293366432827344421E-15, -12.48450537969573659, -144.2187500020484094 ) ) ;
#27220 = CARTESIAN_POINT ( 'NONE',  ( 10.81189881249999729, 0.000000000000000000, -140.8437500020483810 ) ) ;
#27221 = EDGE_CURVE ( 'NONE', #38243, #6565, #39905, .T. ) ;
#27222 = CARTESIAN_POINT ( 'NONE',  ( 10.81189881249999907, 6.242252689847868297, -106.4062500020483952 ) ) ;
#27223 = CARTESIAN_POINT ( 'NONE',  ( -10.81189881249999729, 1.324075727343319199E-15, -119.0937500020483810 ) ) ;
#27224 = CARTESIAN_POINT ( 'NONE',  ( 7.070501591499377789E-16, 11.54700538379251284, -192.5000000040968189 ) ) ;
#27225 = CARTESIAN_POINT ( 'NONE',  ( 10.81189881249999551, -6.242252689847874514, -127.6562500020483952 ) ) ;
#27226 = CARTESIAN_POINT ( 'NONE',  ( -5.405949406249996869, 9.363379034771805109, -9.843750002048345493 ) ) ;
#27227 = CARTESIAN_POINT ( 'NONE',  ( -10.81189881249999729, -6.242252689847864744, -127.9687500020483810 ) ) ;
#27228 = CARTESIAN_POINT ( 'NONE',  ( 9.999999999999742428, 5.773502691896404748, -163.8750000000000284 ) ) ;
#27229 = CARTESIAN_POINT ( 'NONE',  ( 9.999999999999998224, 0.000000000000000000, -11.37500000409674783 ) ) ;
#27230 = CARTESIAN_POINT ( 'NONE',  ( -10.00000000000000000, -5.773502691896251982, -155.6249999999999716 ) ) ;
#27231 = CARTESIAN_POINT ( 'NONE',  ( 4.999999999999992006, -8.660254037844389075, -23.24999999999996447 ) ) ;
#27232 = CARTESIAN_POINT ( 'NONE',  ( 5.405949406249999534, 9.363379034771803333, -80.59375000204838102 ) ) ;
#27233 = CARTESIAN_POINT ( 'NONE',  ( 10.81189881249999729, 0.000000000000000000, -62.84375000204836681 ) ) ;
#27234 = LINE ( 'NONE', #30496, #11166 ) ;
#27235 = CARTESIAN_POINT ( 'NONE',  ( 10.81189881249999729, 0.000000000000000000, -34.53125000204837391 ) ) ;
#27236 = CARTESIAN_POINT ( 'NONE',  ( 10.81189881249999551, -6.242252689847874514, -43.46875000204836681 ) ) ;
#27237 = CARTESIAN_POINT ( 'NONE',  ( -10.00000000000031797, 5.773502691896072569, -185.8750000000000000 ) ) ;
#27238 = CARTESIAN_POINT ( 'NONE',  ( -5.405949406250003975, -9.363379034771801557, -153.3437500020483810 ) ) ;
#27239 = CARTESIAN_POINT ( 'NONE',  ( 10.00000000000000000, 5.773502691896255534, -132.3750000000000000 ) ) ;
#27240 = CARTESIAN_POINT ( 'NONE',  ( 7.644554776091147741E-16, 12.48450537969573659, -133.1562500020483810 ) ) ;
#27241 = CARTESIAN_POINT ( 'NONE',  ( 0.000000000000000000, 0.000000000000000000, -220.0000000000000000 ) ) ;
#27242 = VECTOR ( 'NONE', #2426, 1000.000000000000000 ) ;
#27243 = CARTESIAN_POINT ( 'NONE',  ( 7.070501591499377789E-16, 11.54700538379251284, -81.12499999999997158 ) ) ;
#27244 = CARTESIAN_POINT ( 'NONE',  ( -10.81189881249999729, -6.242252689847864744, -20.15625000204838102 ) ) ;
#27245 = ORIENTED_EDGE ( 'NONE', *, *, #1751, .F. ) ;
#27246 = CARTESIAN_POINT ( 'NONE',  ( -10.81189881249999729, -6.242252689847864744, -107.1562500020483952 ) ) ;
#27247 = CARTESIAN_POINT ( 'NONE',  ( 4.999999999999992006, -8.660254037844389075, -127.1250000040967620 ) ) ;
#27248 = CARTESIAN_POINT ( 'NONE',  ( 5.000000000000000000, 8.660254037844385522, -32.12500000409676204 ) ) ;
#27249 = EDGE_CURVE ( 'NONE', #30972, #17641, #11642, .T. ) ;
#27250 = FACE_OUTER_BOUND ( 'NONE', #29663, .T. ) ;
#27251 = CARTESIAN_POINT ( 'NONE',  ( -10.81189881249999907, -6.242252689847864744, -56.15625000204838102 ) ) ;
#27252 = DIRECTION ( 'NONE',  ( -0.000000000000000000, -0.000000000000000000, 1.000000000000000000 ) ) ;
#27253 = CARTESIAN_POINT ( 'NONE',  ( -5.405949406249996869, 9.363379034771805109, -151.0312500020483810 ) ) ;
#27254 = CARTESIAN_POINT ( 'NONE',  ( 7.644554776091147741E-16, 12.48450537969573659, -132.9687500020483810 ) ) ;
#27255 = CARTESIAN_POINT ( 'NONE',  ( 9.999999999999998224, 0.000000000000000000, -3.875000004096768258 ) ) ;
#27256 = EDGE_CURVE ( 'NONE', #2239, #684, #38126, .T. ) ;
#27257 = ORIENTED_EDGE ( 'NONE', *, *, #36970, .T. ) ;
#27258 = CARTESIAN_POINT ( 'NONE',  ( 5.000000000000000000, 8.660254037844385522, -164.1250000040967905 ) ) ;
#27259 = ORIENTED_EDGE ( 'NONE', *, *, #14202, .T. ) ;
#27260 = ORIENTED_EDGE ( 'NONE', *, *, #29565, .T. ) ;
#27261 = PERSON_AND_ORGANIZATION ( #11915, #17965 ) ;
#27263 = ORIENTED_EDGE ( 'NONE', *, *, #9831, .F. ) ;
#27262 = CARTESIAN_POINT ( 'NONE',  ( 7.644554776091147741E-16, 12.48450537969573659, -108.9687500020483952 ) ) ;
#27264 = AXIS2_PLACEMENT_3D ( 'NONE', #8713, #25546, #28785 ) ;
#27265 =( BOUNDED_CURVE ( )  B_SPLINE_CURVE ( 2, ( #3603, #32952, #23235, #33171, #33593, #6826, #26470 ),
 .UNSPECIFIED., .F., .F. ) 
 B_SPLINE_CURVE_WITH_KNOTS ( ( 3, 2, 2, 3 ),
 ( 0.3022388059701494045, 0.3034825870646767343, 0.3047263681592040085, 0.3059701492537313383 ),
 .UNSPECIFIED. ) 
 CURVE ( )  GEOMETRIC_REPRESENTATION_ITEM ( )  RATIONAL_B_SPLINE_CURVE ( ( 0.9999999999999820144, 0.8660254037844566932, 1.000000000000000000, 0.8660254037844387076, 1.000000000000000000, 0.8660254037844387076, 1.000000000000000000 ) ) 
 REPRESENTATION_ITEM ( '' )  );
#27266 = CARTESIAN_POINT ( 'NONE',  ( 7.070501591499376803E-16, 11.54700538379251284, -189.1250000000000000 ) ) ;
#27267 = CARTESIAN_POINT ( 'NONE',  ( 10.81189881249999729, 0.000000000000000000, -190.3437500020484094 ) ) ;
#27268 = AXIS2_PLACEMENT_3D ( 'NONE', #20197, #579, #4013 ) ;
#27269 = CARTESIAN_POINT ( 'NONE',  ( -5.405949406250003975, -9.363379034771801557, -42.34375000204837391 ) ) ;
#27270 = CARTESIAN_POINT ( 'NONE',  ( 2.525711100651609531, -10.23860432883650162, 1.566949817559350803E-14 ) ) ;
#27271 = FACE_OUTER_BOUND ( 'NONE', #691, .T. ) ;
#27272 = ADVANCED_FACE ( 'NONE', ( #13774 ), #862, .T. ) ;
#27273 = CARTESIAN_POINT ( 'NONE',  ( 7.644554776091147741E-16, 12.48450537969573659, -174.9687500020484094 ) ) ;
#27274 = AXIS2_PLACEMENT_3D ( 'NONE', #15410, #11965, #42163 ) ;
#27275 = CARTESIAN_POINT ( 'NONE',  ( 5.405949406249999534, 9.363379034771803333, -160.0937500020484094 ) ) ;
#27276 = CARTESIAN_POINT ( 'NONE',  ( -9.999999999999998224, 1.224646799147353059E-15, -178.2500000000000284 ) ) ;
#27277 = CARTESIAN_POINT ( 'NONE',  ( 10.81189881249999907, 6.242252689847868297, -145.2187500020484094 ) ) ;
#27279 = EDGE_CURVE ( 'NONE', #41954, #31616, #27694, .T. ) ;
#27278 = CARTESIAN_POINT ( 'NONE',  ( -10.81189881249999729, -6.242252689847864744, -150.4687500020484094 ) ) ;
#27280 = CARTESIAN_POINT ( 'NONE',  ( -9.999999999999998224, 1.224646799147353059E-15, -126.1250000040967620 ) ) ;
#27281 =( BOUNDED_CURVE ( )  B_SPLINE_CURVE ( 2, ( #32421, #25521, #15350, #28548, #25935, #38879, #39084 ),
 .UNSPECIFIED., .F., .F. ) 
 B_SPLINE_CURVE_WITH_KNOTS ( ( 3, 2, 2, 3 ),
 ( 0.3880597014925373789, 0.3893034825870647087, 0.3905472636815920939, 0.3917910447761194792 ),
 .UNSPECIFIED. ) 
 CURVE ( )  GEOMETRIC_REPRESENTATION_ITEM ( )  RATIONAL_B_SPLINE_CURVE ( ( 0.9999999999999940048, 0.8660254037844447028, 1.000000000000000000, 0.8660254037844387076, 1.000000000000000000, 0.8660254037844327124, 1.000000000000005995 ) ) 
 REPRESENTATION_ITEM ( '' )  );
#27282 = CARTESIAN_POINT ( 'NONE',  ( 10.00000000000000000, 5.773502691896255534, -175.8750000000000000 ) ) ;
#27283 = ADVANCED_FACE ( 'NONE', ( #7760 ), #8896, .T. ) ;
#27284 = CARTESIAN_POINT ( 'NONE',  ( -10.81189881249999907, -6.242252689847864744, -87.46875000204838102 ) ) ;
#27285 = CARTESIAN_POINT ( 'NONE',  ( -9.999999999999998224, 1.224646799147353059E-15, -110.7499999999999858 ) ) ;
#27286 = CARTESIAN_POINT ( 'NONE',  ( -10.81189881249999729, 6.242252689847871849, -65.40625000204838102 ) ) ;
#27287 = CARTESIAN_POINT ( 'NONE',  ( 5.000000000000000000, 8.660254037844385522, -146.1250000040967905 ) ) ;
#27288 = CARTESIAN_POINT ( 'NONE',  ( -10.81189881249999729, 6.242252689847871849, -180.7187500020483810 ) ) ;
#27289 = CARTESIAN_POINT ( 'NONE',  ( -10.81189881249999729, 6.242252689847871849, -122.4062500020483952 ) ) ;
#27290 = CARTESIAN_POINT ( 'NONE',  ( -10.81189881249999729, 6.242252689847871849, -155.4062500020483810 ) ) ;
#27291 = CC_DESIGN_PERSON_AND_ORGANIZATION_ASSIGNMENT ( #19505, #36341, ( #31497 ) ) ;
#27292 = CARTESIAN_POINT ( 'NONE',  ( 10.81189881249999729, 0.000000000000000000, -55.53125000204836681 ) ) ;
#27293 = CARTESIAN_POINT ( 'NONE',  ( 7.070501591499377789E-16, 11.54700538379251284, -131.0000000040967905 ) ) ;
#27294 = CARTESIAN_POINT ( 'NONE',  ( -9.999999999999998224, 5.773502691896259087, -104.8749999999999858 ) ) ;
#27295 = ORIENTED_EDGE ( 'NONE', *, *, #37696, .T. ) ;
#27296 =( BOUNDED_CURVE ( )  B_SPLINE_CURVE ( 2, ( #27044, #519, #39979, #6975, #36327, #10410, #13634 ),
 .UNSPECIFIED., .F., .F. ) 
 B_SPLINE_CURVE_WITH_KNOTS ( ( 3, 2, 2, 3 ),
 ( 0.1082089552238805485, 0.1094527363184079616, 0.1106965174129353746, 0.1119402985074627876 ),
 .UNSPECIFIED. ) 
 CURVE ( )  GEOMETRIC_REPRESENTATION_ITEM ( )  RATIONAL_B_SPLINE_CURVE ( ( 1.000000000000004441, 0.8660254037844343777, 1.000000000000000000, 0.8660254037844387076, 1.000000000000000000, 0.8660254037844282715, 1.000000000000010436 ) ) 
 REPRESENTATION_ITEM ( '' )  );
#27297 = CARTESIAN_POINT ( 'NONE',  ( 5.405949406249999534, 9.363379034771803333, -134.7812500020483810 ) ) ;
#27298 = CARTESIAN_POINT ( 'NONE',  ( -10.00000000000000000, -5.773502691896251982, -150.0000000040967905 ) ) ;
#27299 = CARTESIAN_POINT ( 'NONE',  ( -5.405949406249996869, 9.363379034771805109, -146.5312500020483810 ) ) ;
#27300 = CARTESIAN_POINT ( 'NONE',  ( 5.405949406249999534, 9.363379034771803333, -191.7812500020484094 ) ) ;
#27301 = ORIENTED_EDGE ( 'NONE', *, *, #35719, .T. ) ;
#27302 = CARTESIAN_POINT ( 'NONE',  ( 9.999999999999998224, 0.000000000000000000, -46.99999999999998579 ) ) ;
#27303 = CARTESIAN_POINT ( 'NONE',  ( 5.405949406249992428, -9.363379034771808662, -183.0937500020483810 ) ) ;
#27304 = CARTESIAN_POINT ( 'NONE',  ( -9.999999999999998224, 5.773502691896259087, -55.75000000409678336 ) ) ;
#27305 = CARTESIAN_POINT ( 'NONE',  ( 4.999999999999992006, -8.660254037844389075, -179.2500000000000284 ) ) ;
#27306 = LINE ( 'NONE', #11096, #17376 ) ;
#27307 = CARTESIAN_POINT ( 'NONE',  ( -10.81189881249999729, 6.242252689847871849, -74.40625000204836681 ) ) ;
#27308 = AXIS2_PLACEMENT_3D ( 'NONE', #31014, #31233, #14789 ) ;
#27309 = CARTESIAN_POINT ( 'NONE',  ( -10.81189881249999729, 6.242252689847871849, -62.40625000204838813 ) ) ;
#27310 = EDGE_CURVE ( 'NONE', #33916, #5939, #36980, .T. ) ;
#27311 = CARTESIAN_POINT ( 'NONE',  ( 7.070501591499377789E-16, 11.54700538379251284, -54.50000000409676915 ) ) ;
#27312 = CARTESIAN_POINT ( 'NONE',  ( 7.644554776091147741E-16, 12.48450537969573659, -9.968750002048359704 ) ) ;
#27313 = CARTESIAN_POINT ( 'NONE',  ( 9.999999999999998224, 0.000000000000000000, -105.4999999999999858 ) ) ;
#27314 = CARTESIAN_POINT ( 'NONE',  ( -5.405949406250003975, -9.363379034771801557, -176.0312500020483810 ) ) ;
#27315 = CARTESIAN_POINT ( 'NONE',  ( 10.81189881249999907, 6.242252689847868297, -5.906250002048363257 ) ) ;
#27316 = CARTESIAN_POINT ( 'NONE',  ( 0.000000000000000000, 20.00000000000000000, -235.0000000000000000 ) ) ;
#27317 = CARTESIAN_POINT ( 'NONE',  ( -9.999999999999998224, 1.224646799147353059E-15, -197.7500000000000000 ) ) ;
#27318 = CARTESIAN_POINT ( 'NONE',  ( 0.000000000000000000, 0.000000000000000000, -160.0000000000000000 ) ) ;
#27319 = CARTESIAN_POINT ( 'NONE',  ( -4.999999999999996447, 8.660254037844387298, -105.3750000040967763 ) ) ;
#27320 = CYLINDRICAL_SURFACE ( 'NONE', #9642, 9.999999999999998224 ) ;
#27322 = VERTEX_POINT ( 'NONE', #2124 ) ;
#27321 = CARTESIAN_POINT ( 'NONE',  ( -5.405949406250003975, -9.363379034771801557, -84.53125000204838102 ) ) ;
#27324 = ORIENTED_EDGE ( 'NONE', *, *, #23769, .T. ) ;
#27323 = CARTESIAN_POINT ( 'NONE',  ( 0.000000000000000000, 0.000000000000000000, -160.0000000000000000 ) ) ;
#27325 = PRODUCT_DEFINITION_SHAPE ( 'NONE', 'NONE',  #42696 ) ;
#27326 = ORIENTED_EDGE ( 'NONE', *, *, #38108, .F. ) ;
#27327 = CARTESIAN_POINT ( 'NONE',  ( 10.81189881249999729, 0.000000000000000000, -34.34375000204836681 ) ) ;
#27328 = CARTESIAN_POINT ( 'NONE',  ( -5.405949406249996869, 9.363379034771805109, -27.84375000204836326 ) ) ;
#27329 = CARTESIAN_POINT ( 'NONE',  ( 7.644554776091147741E-16, 12.48450537969573659, -13.15625000204836148 ) ) ;
#27330 = CARTESIAN_POINT ( 'NONE',  ( -10.81189881249999907, -6.242252689847864744, -63.46875000204838102 ) ) ;
#27331 = FACE_OUTER_BOUND ( 'NONE', #22787, .T. ) ;
#27332 = CARTESIAN_POINT ( 'NONE',  ( -9.999999999999998224, 1.224646799147353059E-15, -41.74999999999997868 ) ) ;
#27333 = CARTESIAN_POINT ( 'NONE',  ( -10.81189881249999907, -6.242252689847864744, -181.9687500020484094 ) ) ;
#27334 = CARTESIAN_POINT ( 'NONE',  ( 10.81189881249999907, 6.242252689847868297, -163.2187500020483810 ) ) ;
#27335 = CARTESIAN_POINT ( 'NONE',  ( -5.405949406250003975, -9.363379034771801557, -1.843750002048366587 ) ) ;
#27336 = CARTESIAN_POINT ( 'NONE',  ( -5.000000000000003553, -8.660254037844383745, -182.8750000040967905 ) ) ;
#27337 = CARTESIAN_POINT ( 'NONE',  ( 9.999999999999479527, 5.773502691896553074, -147.3750000000000000 ) ) ;
#27338 = FACE_OUTER_BOUND ( 'NONE', #12183, .T. ) ;
#27339 = CARTESIAN_POINT ( 'NONE',  ( 5.000000000000000000, 8.660254037844385522, -199.7500000000000000 ) ) ;
#27340 = CARTESIAN_POINT ( 'NONE',  ( 10.81189881249999551, -6.242252689847874514, -116.9687500020483952 ) ) ;
#27341 = CARTESIAN_POINT ( 'NONE',  ( 9.999999999998456346, 5.773502691897149042, -15.37499999999994138 ) ) ;
#27342 = CARTESIAN_POINT ( 'NONE',  ( -10.81189881249999729, 1.324075727343319199E-15, -87.78125000204838102 ) ) ;
#27343 = CARTESIAN_POINT ( 'NONE',  ( -2.293366432827344421E-15, -12.48450537969573659, -99.21875000204836681 ) ) ;
#27344 = CARTESIAN_POINT ( 'NONE',  ( 10.81189881249999551, -6.242252689847874514, -68.96875000204839523 ) ) ;
#27345 = CARTESIAN_POINT ( 'NONE',  ( -10.81189881249999729, 6.242252689847871849, -78.90625000204838102 ) ) ;
#27346 = CARTESIAN_POINT ( 'NONE',  ( 10.00000000000000000, 5.773502691896255534, -156.7500000040967905 ) ) ;
#27347 = CARTESIAN_POINT ( 'NONE',  ( -4.999999999999996447, 8.660254037844387298, -132.0000000000000000 ) ) ;
#27348 = CARTESIAN_POINT ( 'NONE',  ( -10.81189881249999729, 6.242252689847871849, -156.9062500020483526 ) ) ;
#27349 = CARTESIAN_POINT ( 'NONE',  ( -10.81189881249999729, 1.324075727343319199E-15, -171.7812500020484094 ) ) ;
#27350 = EDGE_CURVE ( 'NONE', #23935, #21158, #41384, .T. ) ;
#27351 = CARTESIAN_POINT ( 'NONE',  ( 0.000000000000000000, 0.000000000000000000, -180.0000000000000000 ) ) ;
#27352 = DIRECTION ( 'NONE',  ( -0.000000000000000000, -0.000000000000000000, 1.000000000000000000 ) ) ;
#27353 = CARTESIAN_POINT ( 'NONE',  ( 10.81189881249999551, -6.242252689847874514, -109.4687500020483810 ) ) ;
#27354 = CARTESIAN_POINT ( 'NONE',  ( 7.070501591499376803E-16, 11.54700538379251284, -63.12499999999997158 ) ) ;
#27355 = CARTESIAN_POINT ( 'NONE',  ( 7.070501591499377789E-16, 11.54700538379251284, -73.62499999999995737 ) ) ;
#27356 = CARTESIAN_POINT ( 'NONE',  ( 10.81189881249999907, 6.242252689847868297, -5.906250002048363257 ) ) ;
#27357 = CARTESIAN_POINT ( 'NONE',  ( -5.000000000000003553, -8.660254037844383745, -89.87500000409677625 ) ) ;
#27358 = CARTESIAN_POINT ( 'NONE',  ( -9.999999999999998224, 1.224646799147353059E-15, -172.2500000000000000 ) ) ;
#27359 = CARTESIAN_POINT ( 'NONE',  ( -2.293366432827344421E-15, -12.48450537969573659, -103.9062500020483810 ) ) ;
#27360 = CARTESIAN_POINT ( 'NONE',  ( 10.81189881249999551, -6.242252689847874514, -85.65625000204839523 ) ) ;
#27361 = CARTESIAN_POINT ( 'NONE',  ( 9.999999999999998224, 0.000000000000000000, -77.37500000409677625 ) ) ;
#27362 = CARTESIAN_POINT ( 'NONE',  ( -4.999999999999996447, 8.660254037844387298, -19.49999999999996092 ) ) ;
#27363 = CARTESIAN_POINT ( 'NONE',  ( -10.81189881249999729, 6.242252689847871849, -30.71875000204834905 ) ) ;
#27364 = ORIENTED_EDGE ( 'NONE', *, *, #1968, .F. ) ;
#27365 = CARTESIAN_POINT ( 'NONE',  ( -10.00000000000000000, -5.773502691896251982, -2.624999999999948486 ) ) ;
#27366 = CARTESIAN_POINT ( 'NONE',  ( 10.81189881249999907, 6.242252689847868297, -29.90625000204835970 ) ) ;
#27367 = CARTESIAN_POINT ( 'NONE',  ( -5.405949406250003975, -9.363379034771801557, -12.34375000204834905 ) ) ;
#27368 = DIRECTION ( 'NONE',  ( -0.000000000000000000, -0.000000000000000000, 1.000000000000000000 ) ) ;
#27369 =( BOUNDED_CURVE ( )  B_SPLINE_CURVE ( 2, ( #34151, #39962, #3936, #14033, #4569, #17711, #17074 ),
 .UNSPECIFIED., .F., .F. ) 
 B_SPLINE_CURVE_WITH_KNOTS ( ( 3, 2, 2, 3 ),
 ( 0.9626865671641793298, 0.9639303482587067151, 0.9651741293532341004, 0.9664179104477613746 ),
 .UNSPECIFIED. ) 
 CURVE ( )  GEOMETRIC_REPRESENTATION_ITEM ( )  RATIONAL_B_SPLINE_CURVE ( ( 0.9999999999999761302, 0.8660254037844625774, 1.000000000000000000, 0.8660254037844387076, 1.000000000000000000, 0.8660254037844148378, 1.000000000000023981 ) ) 
 REPRESENTATION_ITEM ( '' )  );
#27370 = CARTESIAN_POINT ( 'NONE',  ( 5.000000000000000000, 8.660254037844385522, -2.125000004096766482 ) ) ;
#27371 = CARTESIAN_POINT ( 'NONE',  ( -5.405949406249996869, 9.363379034771805109, -127.0312500020483952 ) ) ;
#27372 = EDGE_CURVE ( 'NONE', #30360, #29087, #24903, .T. ) ;
#27373 = CARTESIAN_POINT ( 'NONE',  ( 7.070501591499377789E-16, 11.54700538379251284, -180.1250000000000000 ) ) ;
#27374 = CARTESIAN_POINT ( 'NONE',  ( 9.999999999999998224, 0.000000000000000000, -144.8750000040967905 ) ) ;
#27376 = VERTEX_POINT ( 'NONE', #38150 ) ;
#27375 = CARTESIAN_POINT ( 'NONE',  ( -10.81189881249999729, 6.242252689847871849, -113.4062500020483810 ) ) ;
#27377 = DIRECTION ( 'NONE',  ( -0.000000000000000000, -0.000000000000000000, 1.000000000000000000 ) ) ;
#27378 = ORIENTED_EDGE ( 'NONE', *, *, #24260, .T. ) ;
#27379 = ORIENTED_EDGE ( 'NONE', *, *, #39059, .F. ) ;
#27380 = CARTESIAN_POINT ( 'NONE',  ( -2.293366432827344421E-15, -12.48450537969573659, -34.90625000204836681 ) ) ;
#27381 = PERSON_AND_ORGANIZATION ( #11915, #17965 ) ;
#27382 = CARTESIAN_POINT ( 'NONE',  ( 5.405949406249992428, -9.363379034771808662, -91.59375000204838102 ) ) ;
#27383 = CYLINDRICAL_SURFACE ( 'NONE', #32581, 9.999999999999998224 ) ;
#27384 = CARTESIAN_POINT ( 'NONE',  ( 9.999999999999998224, 0.000000000000000000, -108.4999999999999858 ) ) ;
#27385 = CARTESIAN_POINT ( 'NONE',  ( 10.81189881249999729, 0.000000000000000000, -199.3437500020484094 ) ) ;
#27386 = CARTESIAN_POINT ( 'NONE',  ( 10.81189881249999729, 0.000000000000000000, -175.5312500020483810 ) ) ;
#27387 = CARTESIAN_POINT ( 'NONE',  ( 5.000000000000000000, 8.660254037844385522, -138.2499999999999716 ) ) ;
#27388 = CARTESIAN_POINT ( 'NONE',  ( 10.81189881249999729, 6.242252689847867408, -124.2187500020483952 ) ) ;
#27389 = CARTESIAN_POINT ( 'NONE',  ( 10.81189881249999551, -6.242252689847874514, -92.96875000204838102 ) ) ;
#27390 = CARTESIAN_POINT ( 'NONE',  ( 7.644554776091147741E-16, 12.48450537969573659, -5.656250002048358816 ) ) ;
#27391 = CARTESIAN_POINT ( 'NONE',  ( -10.00000000000038547, 5.773502691896036154, -154.3749999999999716 ) ) ;
#27392 = CARTESIAN_POINT ( 'NONE',  ( -10.81189881249999729, 1.324075727343319199E-15, -99.78125000204839523 ) ) ;
#27393 = CARTESIAN_POINT ( 'NONE',  ( 5.000000000000000000, 8.660254037844385522, -180.6250000040967905 ) ) ;
#27394 = CARTESIAN_POINT ( 'NONE',  ( -10.81189881249999729, -6.242252689847864744, -106.9687500020483810 ) ) ;
#27395 = CARTESIAN_POINT ( 'NONE',  ( -10.81189881249999729, 1.324075727343319199E-15, -177.7812500020484094 ) ) ;
#27396 = ADVANCED_FACE ( 'NONE', ( #38789 ), #29089, .T. ) ;
#27397 = CARTESIAN_POINT ( 'NONE',  ( 9.999999999999998224, 0.000000000000000000, -108.4999999999999858 ) ) ;
#27398 = CARTESIAN_POINT ( 'NONE',  ( 7.070501591499376803E-16, 11.54700538379251284, -132.5000000040967905 ) ) ;
#27399 = CARTESIAN_POINT ( 'NONE',  ( 5.405949406249992428, -9.363379034771808662, -198.2812500020484094 ) ) ;
#27400 = CARTESIAN_POINT ( 'NONE',  ( -5.405949406249996869, 9.363379034771805109, -53.34375000204835970 ) ) ;
#27401 = CARTESIAN_POINT ( 'NONE',  ( -10.81189881249999729, 6.242252689847871849, -42.71875000204835970 ) ) ;
#27402 = CARTESIAN_POINT ( 'NONE',  ( -9.999999999999998224, 5.773502691896259087, -174.2500000040967905 ) ) ;
#27403 = CARTESIAN_POINT ( 'NONE',  ( 10.81189881249999907, 6.242252689847868297, -7.406250002048366810 ) ) ;
#27404 = CARTESIAN_POINT ( 'NONE',  ( 10.81189881249999551, -6.242252689847874514, -17.96875000204836681 ) ) ;
#27405 = CARTESIAN_POINT ( 'NONE',  ( -9.999999999999479527, -5.773502691896549521, -124.5000000040967620 ) ) ;
#27406 = CARTESIAN_POINT ( 'NONE',  ( -10.81189881249999729, 1.324075727343319199E-15, -129.5937500020483810 ) ) ;
#27407 = CARTESIAN_POINT ( 'NONE',  ( 9.999999999999998224, 0.000000000000000000, -99.49999999999998579 ) ) ;
#27408 = CARTESIAN_POINT ( 'NONE',  ( -10.81189881249999729, 6.242252689847871849, -27.90625000204838102 ) ) ;
#27409 = CARTESIAN_POINT ( 'NONE',  ( -5.000000000000003553, -8.660254037844383745, -116.8750000040967905 ) ) ;
#27410 = CYLINDRICAL_SURFACE ( 'NONE', #9327, 9.999999999999998224 ) ;
#27411 = CARTESIAN_POINT ( 'NONE',  ( -5.000000000000003553, -8.660254037844383745, -60.99999999999997158 ) ) ;
#27412 = CARTESIAN_POINT ( 'NONE',  ( 7.644554776091147741E-16, 12.48450537969573659, -124.1562500020483952 ) ) ;
#27413 = CARTESIAN_POINT ( 'NONE',  ( 5.405949406249999534, 9.363379034771803333, -104.7812500020483810 ) ) ;
#27414 = VERTEX_POINT ( 'NONE', #25631 ) ;
#27415 =( BOUNDED_CURVE ( )  B_SPLINE_CURVE ( 2, ( #13876, #40630, #7642, #10861, #14518, #10647, #17975 ),
 .UNSPECIFIED., .F., .F. ) 
 B_SPLINE_CURVE_WITH_KNOTS ( ( 3, 2, 2, 3 ),
 ( 0.5261194029850747578, 0.5273631840796021431, 0.5286069651741294173, 0.5298507462686568026 ),
 .UNSPECIFIED. ) 
 CURVE ( )  GEOMETRIC_REPRESENTATION_ITEM ( )  RATIONAL_B_SPLINE_CURVE ( ( 0.9999999999999880096, 0.8660254037844506980, 1.000000000000000000, 0.8660254037844387076, 1.000000000000000000, 0.8660254037844267172, 1.000000000000011990 ) ) 
 REPRESENTATION_ITEM ( '' )  );
#27416 = CARTESIAN_POINT ( 'NONE',  ( -9.999999999999742428, -5.773502691896402084, -118.1249999999999858 ) ) ;
#27417 = CARTESIAN_POINT ( 'NONE',  ( -4.999999999999996447, 8.660254037844387298, -103.8750000040967763 ) ) ;
#27418 = CARTESIAN_POINT ( 'NONE',  ( 7.070501591499376803E-16, 11.54700538379251284, -141.5000000040967905 ) ) ;
#27419 = CARTESIAN_POINT ( 'NONE',  ( -5.405949406249996869, 9.363379034771805109, -166.0312500020484094 ) ) ;
#27420 = CARTESIAN_POINT ( 'NONE',  ( 10.81189881249999551, -6.242252689847874514, -58.46875000204837391 ) ) ;
#27421 = VERTEX_POINT ( 'NONE', #18285 ) ;
#27422 = CARTESIAN_POINT ( 'NONE',  ( 4.999999999999992006, -8.660254037844389075, -29.24999999999997158 ) ) ;
#27423 = AXIS2_PLACEMENT_3D ( 'NONE', #24213, #13819, #4349 ) ;
#27424 = CARTESIAN_POINT ( 'NONE',  ( 10.81189881249999551, -6.242252689847874514, -37.65625000204836681 ) ) ;
#27425 = CARTESIAN_POINT ( 'NONE',  ( 9.999999999999996447, -5.773502691896262640, -164.1249999999999716 ) ) ;
#27426 = VECTOR ( 'NONE', #28249, 1000.000000000000000 ) ;
#27427 = EDGE_CURVE ( 'NONE', #36710, #12497, #29298, .T. ) ;
#27428 = CARTESIAN_POINT ( 'NONE',  ( 10.00000000000000000, 5.773502691896255534, -29.25000000409675494 ) ) ;
#27429 = CARTESIAN_POINT ( 'NONE',  ( 5.405949406249999534, 9.363379034771803333, -131.7812500020483810 ) ) ;
#27430 = CARTESIAN_POINT ( 'NONE',  ( -1.034724182395691638, 10.15477877528964257, -4.586030929915079049E-15 ) ) ;
#27431 = CARTESIAN_POINT ( 'NONE',  ( 9.999999999999742428, 5.773502691896404748, -162.7500000040968189 ) ) ;
#27432 = ORIENTED_EDGE ( 'NONE', *, *, #22293, .T. ) ;
#27434 = ORIENTED_EDGE ( 'NONE', *, *, #34023, .F. ) ;
#27433 = VERTEX_POINT ( 'NONE', #41147 ) ;
#27435 = CARTESIAN_POINT ( 'NONE',  ( 0.000000000000000000, 0.000000000000000000, -99.99999999999998579 ) ) ;
#27436 = CARTESIAN_POINT ( 'NONE',  ( 0.000000000000000000, 0.000000000000000000, -200.0000000000000000 ) ) ;
#27437 = CARTESIAN_POINT ( 'NONE',  ( -5.405949406250003975, -9.363379034771801557, -166.8437500020484094 ) ) ;
#27438 = CARTESIAN_POINT ( 'NONE',  ( 10.81189881249999729, 0.000000000000000000, -193.5312500020484094 ) ) ;
#27439 = CARTESIAN_POINT ( 'NONE',  ( -10.81189881249999729, 6.242252689847871849, -15.71875000204835793 ) ) ;
#27440 = CARTESIAN_POINT ( 'NONE',  ( 9.999999999999998224, 0.000000000000000000, -75.49999999999998579 ) ) ;
#27441 = AXIS2_PLACEMENT_3D ( 'NONE', #3828, #33402, #3191 ) ;
#27442 = CARTESIAN_POINT ( 'NONE',  ( 5.405949406249992428, -9.363379034771808662, -150.0937500020483810 ) ) ;
#27443 = AXIS2_PLACEMENT_3D ( 'NONE', #23147, #36310, #6742 ) ;
#27444 = CARTESIAN_POINT ( 'NONE',  ( 7.644554776091147741E-16, 12.48450537969573659, -138.9687500020484094 ) ) ;
#27445 = CARTESIAN_POINT ( 'NONE',  ( 10.81189881249999551, -6.242252689847874514, -108.1562500020483810 ) ) ;
#27446 = CARTESIAN_POINT ( 'NONE',  ( -5.405949406250003975, -9.363379034771801557, -117.3437500020483810 ) ) ;
#27447 = CARTESIAN_POINT ( 'NONE',  ( 7.070501591499377789E-16, 11.54700538379251284, -195.5000000040968189 ) ) ;
#27448 = CARTESIAN_POINT ( 'NONE',  ( -2.293366432827344421E-15, -12.48450537969573659, -127.9062500020483952 ) ) ;
#27449 = CARTESIAN_POINT ( 'NONE',  ( 7.644554776091147741E-16, 12.48450537969573659, -12.96875000204836148 ) ) ;
#27450 = CARTESIAN_POINT ( 'NONE',  ( 7.644554776091147741E-16, 12.48450537969573659, -126.9687500020483952 ) ) ;
#27451 = CYLINDRICAL_SURFACE ( 'NONE', #30234, 9.999999999999998224 ) ;
#27452 = DIRECTION ( 'NONE',  ( -0.08715574274765837404, 0.000000000000000000, -0.9961946980917455452 ) ) ;
#27453 = CARTESIAN_POINT ( 'NONE',  ( -5.000000000000003553, -8.660254037844383745, -157.0000000000000000 ) ) ;
#27454 = CARTESIAN_POINT ( 'NONE',  ( -9.999999999999998224, 1.224646799147353059E-15, -22.24999999999996447 ) ) ;
#27455 = CARTESIAN_POINT ( 'NONE',  ( 10.81189881249999729, 6.242252689847867408, -76.21875000204838102 ) ) ;
#27456 = CARTESIAN_POINT ( 'NONE',  ( 10.81189881249999551, -6.242252689847874514, -61.46875000204838102 ) ) ;
#27457 = CARTESIAN_POINT ( 'NONE',  ( 4.999999999999992006, -8.660254037844389075, -158.6250000040967905 ) ) ;
#27458 = CARTESIAN_POINT ( 'NONE',  ( -10.81189881249999729, 6.242252689847871849, -36.90625000204835970 ) ) ;
#27459 = CARTESIAN_POINT ( 'NONE',  ( 7.644554776091147741E-16, 12.48450537969573659, -45.96875000204836681 ) ) ;
#27460 = CARTESIAN_POINT ( 'NONE',  ( 9.999999999999998224, 0.000000000000000000, -200.0000000000000000 ) ) ;
#27461 = CARTESIAN_POINT ( 'NONE',  ( -5.405949406250003975, -9.363379034771801557, -157.8437500020483810 ) ) ;
#27462 = CARTESIAN_POINT ( 'NONE',  ( -5.000000000000003553, -8.660254037844383745, -119.5000000000000000 ) ) ;
#27463 = CARTESIAN_POINT ( 'NONE',  ( 10.81189881249999729, 0.000000000000000000, -132.0312500020484094 ) ) ;
#27464 = CARTESIAN_POINT ( 'NONE',  ( -9.999999999999998224, 1.224646799147353059E-15, -187.6250000040967905 ) ) ;
#27465 = CARTESIAN_POINT ( 'NONE',  ( 10.00000000000000000, 5.773502691896255534, -82.87499999999997158 ) ) ;
#27466 = CARTESIAN_POINT ( 'NONE',  ( 5.405949406249992428, -9.363379034771808662, -16.78125000204835970 ) ) ;
#27467 = EDGE_LOOP ( 'NONE', ( #35308, #33806, #9691, #30254 ) ) ;
#27468 = CARTESIAN_POINT ( 'NONE',  ( 5.405949406249992428, -9.363379034771808662, -103.7812500020483810 ) ) ;
#27469 = CARTESIAN_POINT ( 'NONE',  ( 5.000000000000000000, 8.660254037844385522, -120.6250000040967905 ) ) ;
#27470 = CARTESIAN_POINT ( 'NONE',  ( 9.999999999999998224, 0.000000000000000000, -33.87500000409676915 ) ) ;
#27471 = CARTESIAN_POINT ( 'NONE',  ( -9.214310226692173294E-15, 125.0000000000000000, 32.24999999999999289 ) ) ;
#27472 = CARTESIAN_POINT ( 'NONE',  ( -10.81189881249999729, 1.324075727343319199E-15, -53.28125000204836681 ) ) ;
#27473 = CARTESIAN_POINT ( 'NONE',  ( -2.121150477449813534E-15, -11.54700538379251284, -135.8750000000000000 ) ) ;
#27474 = CARTESIAN_POINT ( 'NONE',  ( -5.405949406250003975, -9.363379034771801557, -156.5312500020484094 ) ) ;
#27475 = CARTESIAN_POINT ( 'NONE',  ( 10.81189881249999551, -6.242252689847874514, -128.9687500020483810 ) ) ;
#27477 = EDGE_CURVE ( 'NONE', #4157, #22331, #1454, .T. ) ;
#27476 = CARTESIAN_POINT ( 'NONE',  ( -4.999999999999996447, 8.660254037844387298, -144.0000000000000000 ) ) ;
#27478 = CIRCLE ( 'NONE', #21276, 5.500000000000003553 ) ;
#27479 = ORIENTED_EDGE ( 'NONE', *, *, #41809, .F. ) ;
#27480 = EDGE_CURVE ( 'NONE', #27322, #6831, #8646, .T. ) ;
#27481 = CARTESIAN_POINT ( 'NONE',  ( -4.999999999999996447, 8.660254037844387298, -31.49999999999997158 ) ) ;
#27482 = ORIENTED_EDGE ( 'NONE', *, *, #26747, .F. ) ;
#27483 = ORIENTED_EDGE ( 'NONE', *, *, #16415, .T. ) ;
#27485 = ORIENTED_EDGE ( 'NONE', *, *, #23349, .T. ) ;
#27484 = CARTESIAN_POINT ( 'NONE',  ( -10.81189881249999729, 6.242252689847871849, -113.2187500020483952 ) ) ;
#27486 = CARTESIAN_POINT ( 'NONE',  ( -9.999999999998969713, -5.773502691896847949, -42.00000000409673362 ) ) ;
#27487 = CARTESIAN_POINT ( 'NONE',  ( -10.81189881249999729, 1.324075727343319199E-15, -186.5937500020483810 ) ) ;
#27488 = CARTESIAN_POINT ( 'NONE',  ( 5.405949406249992428, -9.363379034771808662, -42.09375000204837391 ) ) ;
#27489 = CARTESIAN_POINT ( 'NONE',  ( -4.999999999999996447, 8.660254037844387298, -61.87500000409676204 ) ) ;
#27490 = CARTESIAN_POINT ( 'NONE',  ( -9.999999999999998224, 1.224646799147353059E-15, -10.62500000409674605 ) ) ;
#27491 = CARTESIAN_POINT ( 'NONE',  ( -10.81189881249999729, 1.324075727343319199E-15, -176.0937500020484094 ) ) ;
#27492 = CARTESIAN_POINT ( 'NONE',  ( 10.81189881249999907, 6.242252689847868297, -157.2187500020483810 ) ) ;
#27493 = CARTESIAN_POINT ( 'NONE',  ( 9.999999999999998224, 0.000000000000000000, -65.37500000409676204 ) ) ;
#27494 = CARTESIAN_POINT ( 'NONE',  ( 10.81189881249999551, -6.242252689847874514, -137.9687500020483810 ) ) ;
#27495 = CARTESIAN_POINT ( 'NONE',  ( 5.405949406249992428, -9.363379034771808662, -154.5937500020483810 ) ) ;
#27496 = CARTESIAN_POINT ( 'NONE',  ( -10.00000000000076916, 5.773502691895813221, -126.2500000040967763 ) ) ;
#27497 = FACE_OUTER_BOUND ( 'NONE', #34546, .T. ) ;
#27498 = CARTESIAN_POINT ( 'NONE',  ( 9.999999999999998224, 0.000000000000000000, -180.5000000000000000 ) ) ;
#27499 = CARTESIAN_POINT ( 'NONE',  ( 7.644554776091147741E-16, 12.48450537969573659, -86.46875000204838102 ) ) ;
#27500 = CARTESIAN_POINT ( 'NONE',  ( 10.00000000000076916, -5.773502691895816774, -113.1249999999999716 ) ) ;
#27501 = CARTESIAN_POINT ( 'NONE',  ( -10.81189881249999907, -6.242252689847864744, -62.15625000204838102 ) ) ;
#27502 = CARTESIAN_POINT ( 'NONE',  ( -9.999999999999998224, 1.224646799147353059E-15, -87.12500000409677625 ) ) ;
#27503 = CARTESIAN_POINT ( 'NONE',  ( -10.81189881249999907, -6.242252689847864744, -178.9687500020484094 ) ) ;
#27504 = CARTESIAN_POINT ( 'NONE',  ( 10.81189881249999551, -6.242252689847874514, -112.6562500020483810 ) ) ;
#27505 = AXIS2_PLACEMENT_3D ( 'NONE', #8552, #31868, #31433 ) ;
#27506 = CARTESIAN_POINT ( 'NONE',  ( -10.81189881249999729, 1.324075727343319199E-15, -155.2812500020484094 ) ) ;
#27507 = FACE_OUTER_BOUND ( 'NONE', #25352, .T. ) ;
#27508 = CARTESIAN_POINT ( 'NONE',  ( -5.405949406250003975, -9.363379034771801557, -44.03125000204838102 ) ) ;
#27509 = CARTESIAN_POINT ( 'NONE',  ( 7.070501591499377789E-16, 11.54700538379251284, -129.5000000040967620 ) ) ;
#27510 = CARTESIAN_POINT ( 'NONE',  ( -4.999999999999996447, 8.660254037844387298, -103.5000000000000000 ) ) ;
#27511 = ORIENTED_EDGE ( 'NONE', *, *, #18294, .T. ) ;
#27512 = CARTESIAN_POINT ( 'NONE',  ( -2.293366432827344421E-15, -12.48450537969573659, -129.4062500020483810 ) ) ;
#27513 = CARTESIAN_POINT ( 'NONE',  ( 4.999999999999992006, -8.660254037844389075, -148.1250000040967905 ) ) ;
#27514 = CARTESIAN_POINT ( 'NONE',  ( 10.81189881249999729, 0.000000000000000000, -141.0312500020483810 ) ) ;
#27515 = VECTOR ( 'NONE', #41570, 1000.000000000000000 ) ;
#27516 = CARTESIAN_POINT ( 'NONE',  ( -2.293366432827344421E-15, -12.48450537969573659, -189.4062500020484094 ) ) ;
#27517 = VERTEX_POINT ( 'NONE', #9429 ) ;
#27518 = CARTESIAN_POINT ( 'NONE',  ( -2.121150477449813534E-15, -11.54700538379251284, -45.87499999999996447 ) ) ;
#27519 = CARTESIAN_POINT ( 'NONE',  ( -5.405949406249996869, 9.363379034771805109, -177.8437500020483810 ) ) ;
#27520 = CARTESIAN_POINT ( 'NONE',  ( 10.00000000000000000, 5.773502691896255534, -60.75000000409676915 ) ) ;
#27521 = CARTESIAN_POINT ( 'NONE',  ( -9.999999999999998224, 1.224646799147353059E-15, -158.7500000000000000 ) ) ;
#27522 = CARTESIAN_POINT ( 'NONE',  ( -10.81189881249999729, 1.324075727343319199E-15, -72.78125000204838102 ) ) ;
#27523 = CARTESIAN_POINT ( 'NONE',  ( 5.405949406249992428, -9.363379034771808662, -48.28125000204838813 ) ) ;
#27524 = CARTESIAN_POINT ( 'NONE',  ( 5.000000000000000000, 8.660254037844385522, -48.62500000409678336 ) ) ;
#27525 = AXIS2_PLACEMENT_3D ( 'NONE', #27928, #36777, #34623 ) ;
#27526 = CARTESIAN_POINT ( 'NONE',  ( 10.81189881249999729, 0.000000000000000000, -11.84375000204834727 ) ) ;
#27527 = CARTESIAN_POINT ( 'NONE',  ( -10.81189881249999729, 1.324075727343319199E-15, -173.2812500020484094 ) ) ;
#27528 = CARTESIAN_POINT ( 'NONE',  ( -10.81189881249999907, -6.242252689847864744, -5.156250002048362369 ) ) ;
#27529 = DIRECTION ( 'NONE',  ( 1.000000000000000000, 0.000000000000000000, 0.000000000000000000 ) ) ;
#27531 = ADVANCED_FACE ( 'NONE', ( #6200 ), #33385, .T. ) ;
#27530 = CARTESIAN_POINT ( 'NONE',  ( 10.00000000000051159, -5.773502691895965988, -81.62499999999995737 ) ) ;
#27532 = FACE_OUTER_BOUND ( 'NONE', #37603, .T. ) ;
#27533 = CARTESIAN_POINT ( 'NONE',  ( -5.000000000000003553, -8.660254037844383745, -60.99999999999997158 ) ) ;
#27534 =( BOUNDED_CURVE ( )  B_SPLINE_CURVE ( 2, ( #33387, #19769, #3382, #23451, #10266, #29717, #36600 ),
 .UNSPECIFIED., .F., .F. ) 
 B_SPLINE_CURVE_WITH_KNOTS ( ( 3, 2, 2, 3 ),
 ( 0.6828358208955226383, 0.6840796019900500236, 0.6853233830845772978, 0.6865671641791046831 ),
 .UNSPECIFIED. ) 
 CURVE ( )  GEOMETRIC_REPRESENTATION_ITEM ( )  RATIONAL_B_SPLINE_CURVE ( ( 0.9999999999999761302, 0.8660254037844625774, 1.000000000000000000, 0.8660254037844387076, 1.000000000000000000, 0.8660254037844148378, 1.000000000000023981 ) ) 
 REPRESENTATION_ITEM ( '' )  );
#27535 = EDGE_CURVE ( 'NONE', #1789, #15268, #36392, .T. ) ;
#27536 = CARTESIAN_POINT ( 'NONE',  ( 10.00000000000102318, -5.773502691895667560, -20.12499999999993960 ) ) ;
#27538 = VERTEX_POINT ( 'NONE', #42428 ) ;
#27537 = CARTESIAN_POINT ( 'NONE',  ( 5.405949406249999534, 9.363379034771803333, -85.28125000204838102 ) ) ;
#27540 = EDGE_LOOP ( 'NONE', ( #24093, #28832, #36743, #8737 ) ) ;
#27539 = FACE_OUTER_BOUND ( 'NONE', #4484, .T. ) ;
#27541 = CC_DESIGN_DATE_AND_TIME_ASSIGNMENT ( #36873, #26948, ( #24384 ) ) ;
#27542 = ORIENTED_EDGE ( 'NONE', *, *, #15090, .T. ) ;
#27543 = CARTESIAN_POINT ( 'NONE',  ( -10.81189881249999729, 6.242252689847871849, -39.71875000204835970 ) ) ;
#27544 = CARTESIAN_POINT ( 'NONE',  ( -10.81189881249999729, 6.242252689847871849, -24.71875000204837036 ) ) ;
#27545 = CARTESIAN_POINT ( 'NONE',  ( -5.405949406250003975, -9.363379034771801557, -14.03125000204835615 ) ) ;
#27546 = AXIS2_PLACEMENT_3D ( 'NONE', #29983, #20884, #1049 ) ;
#27547 = CARTESIAN_POINT ( 'NONE',  ( 10.81189881249999907, 6.242252689847868297, -61.21875000204838102 ) ) ;
#27548 = DIRECTION ( 'NONE',  ( 1.000000000000000000, 0.000000000000000000, 0.000000000000000000 ) ) ;
#27549 = CARTESIAN_POINT ( 'NONE',  ( -2.121150477449813534E-15, -11.54700538379251284, -41.37499999999996447 ) ) ;
#27550 = CARTESIAN_POINT ( 'NONE',  ( -10.81189881249999729, 1.324075727343319199E-15, -185.0937500020483810 ) ) ;
#27551 = CARTESIAN_POINT ( 'NONE',  ( -5.405949406250003975, -9.363379034771801557, -162.3437500020484094 ) ) ;
#27552 = CARTESIAN_POINT ( 'NONE',  ( -10.81189881249999729, 6.242252689847871849, -177.7187500020484379 ) ) ;
#27553 = CYLINDRICAL_SURFACE ( 'NONE', #28133, 9.999999999999998224 ) ;
#27554 = DIRECTION ( 'NONE',  ( -1.000000000000000000, 0.000000000000000000, 0.000000000000000000 ) ) ;
#27555 = EDGE_CURVE ( 'NONE', #23028, #13495, #15953, .T. ) ;
#27556 = DIRECTION ( 'NONE',  ( -0.000000000000000000, -0.000000000000000000, -1.000000000000000000 ) ) ;
#27557 = CARTESIAN_POINT ( 'NONE',  ( -5.405949406250003975, -9.363379034771801557, -111.3437500020483810 ) ) ;
#27558 = LINE ( 'NONE', #8564, #12833 ) ;
#27559 = CARTESIAN_POINT ( 'NONE',  ( -10.81189881249999729, 6.242252689847871849, -78.90625000204838102 ) ) ;
#27560 = CARTESIAN_POINT ( 'NONE',  ( -5.405949406250003975, -9.363379034771801557, -97.84375000204838102 ) ) ;
#27561 = CARTESIAN_POINT ( 'NONE',  ( -2.293366432827344421E-15, -12.48450537969573659, -72.21875000204835260 ) ) ;
#27562 = CARTESIAN_POINT ( 'NONE',  ( 10.81189881249999729, 0.000000000000000000, -75.03125000204838102 ) ) ;
#27563 = CARTESIAN_POINT ( 'NONE',  ( -2.121150477449813534E-15, -11.54700538379251284, -151.2500000040967620 ) ) ;
#27564 = CARTESIAN_POINT ( 'NONE',  ( 10.00000000000000000, 5.773502691896255534, -133.8750000000000000 ) ) ;
#27565 = CARTESIAN_POINT ( 'NONE',  ( -10.81189881249999729, 1.324075727343319199E-15, -158.2812500020484094 ) ) ;
#27566 = CARTESIAN_POINT ( 'NONE',  ( 5.405949406249992428, -9.363379034771808662, -169.7812500020484094 ) ) ;
#27567 = CARTESIAN_POINT ( 'NONE',  ( -9.999999999999998224, 1.224646799147353059E-15, -108.1250000040967763 ) ) ;
#27568 = FACE_OUTER_BOUND ( 'NONE', #7053, .T. ) ;
#27569 = CARTESIAN_POINT ( 'NONE',  ( 10.81189881249999907, 6.242252689847868297, -106.2187500020483668 ) ) ;
#27570 = DIRECTION ( 'NONE',  ( -1.000000000000000000, 0.000000000000000000, 0.000000000000000000 ) ) ;
#27571 = CARTESIAN_POINT ( 'NONE',  ( 9.999999999999996447, -5.773502691896262640, -74.12499999999997158 ) ) ;
#27572 = CARTESIAN_POINT ( 'NONE',  ( -5.405949406250003975, -9.363379034771801557, -2.031250002048373915 ) ) ;
#27573 = CARTESIAN_POINT ( 'NONE',  ( -2.121150477449813534E-15, -11.54700538379251284, -80.75000000409677625 ) ) ;
#27574 = CARTESIAN_POINT ( 'NONE',  ( 4.999999999999992006, -8.660254037844389075, -171.7500000000000000 ) ) ;
#27575 = CARTESIAN_POINT ( 'NONE',  ( -5.405949406249996869, 9.363379034771805109, -103.0312500020483952 ) ) ;
#27576 = CARTESIAN_POINT ( 'NONE',  ( 10.81189881249999551, -6.242252689847874514, -72.15625000204836681 ) ) ;
#27577 = CARTESIAN_POINT ( 'NONE',  ( 10.00000000000000000, 5.773502691896255534, -78.75000000409679046 ) ) ;
#27578 = CARTESIAN_POINT ( 'NONE',  ( 9.999999999999998224, 0.000000000000000000, -113.3750000040967763 ) ) ;
#27579 = CARTESIAN_POINT ( 'NONE',  ( -5.405949406249996869, 9.363379034771805109, -30.84375000204836326 ) ) ;
#27580 = ORIENTED_EDGE ( 'NONE', *, *, #4173, .T. ) ;
#27581 = CARTESIAN_POINT ( 'NONE',  ( 5.405949406249999534, 9.363379034771803333, -199.2812500020484094 ) ) ;
#27582 = CARTESIAN_POINT ( 'NONE',  ( 5.405949406249992428, -9.363379034771808662, -25.78125000204836681 ) ) ;
#27583 = CARTESIAN_POINT ( 'NONE',  ( 7.644554776091147741E-16, 12.48450537969573659, -15.96875000204835615 ) ) ;
#27584 = FACE_OUTER_BOUND ( 'NONE', #14070, .T. ) ;
#27585 = CARTESIAN_POINT ( 'NONE',  ( 9.999999999999998224, 0.000000000000000000, -6.875000004096742501 ) ) ;
#27586 = CARTESIAN_POINT ( 'NONE',  ( -2.293366432827344421E-15, -12.48450537969573659, -129.4062500020483810 ) ) ;
#27587 = CARTESIAN_POINT ( 'NONE',  ( 7.070501591499377789E-16, 11.54700538379251284, -184.6250000000000000 ) ) ;
#27588 = CARTESIAN_POINT ( 'NONE',  ( 5.000000000000000000, 8.660254037844385522, -106.7499999999999858 ) ) ;
#27590 = ORIENTED_EDGE ( 'NONE', *, *, #18991, .T. ) ;
#27589 = CARTESIAN_POINT ( 'NONE',  ( 10.81189881249999729, 0.000000000000000000, -112.5312500020483952 ) ) ;
#27591 = CARTESIAN_POINT ( 'NONE',  ( -5.000000000000002665, 20.00000000000000000, -235.0000000000000000 ) ) ;
#27592 = VERTEX_POINT ( 'NONE', #12857 ) ;
#27593 = VERTEX_POINT ( 'NONE', #13278 ) ;
#27594 = CARTESIAN_POINT ( 'NONE',  ( -2.293366432827344421E-15, -12.48450537969573659, -39.40625000204835260 ) ) ;
#27595 = APPLICATION_PROTOCOL_DEFINITION ( 'international standard', 'config_control_design', 1994, #844 ) ;
#27596 = EDGE_CURVE ( 'NONE', #8492, #9326, #26467, .T. ) ;
#27597 = CARTESIAN_POINT ( 'NONE',  ( 5.405949406249992428, -9.363379034771808662, -88.59375000204838102 ) ) ;
#27598 = LINE ( 'NONE', #31058, #14614 ) ;
#27599 = CARTESIAN_POINT ( 'NONE',  ( 1.351487262974977233, 10.72709830801206543, -100.0000000000000000 ) ) ;
#27600 = CARTESIAN_POINT ( 'NONE',  ( 9.999999999999998224, 0.000000000000000000, -156.8750000040967905 ) ) ;
#27601 = CARTESIAN_POINT ( 'NONE',  ( 10.81189881249999729, 0.000000000000000000, -171.0312500020484094 ) ) ;
#27602 = CARTESIAN_POINT ( 'NONE',  ( -9.999999999999998224, 1.224646799147353059E-15, -58.24999999999997158 ) ) ;
#27603 = VECTOR ( 'NONE', #20887, 1000.000000000000000 ) ;
#27604 = CARTESIAN_POINT ( 'NONE',  ( 5.405949406249999534, 9.363379034771803333, -125.5937500020483668 ) ) ;
#27605 = CARTESIAN_POINT ( 'NONE',  ( -5.405949406249996869, 9.363379034771805109, -92.34375000204838102 ) ) ;
#27606 = DIRECTION ( 'NONE',  ( -0.000000000000000000, -0.000000000000000000, 1.000000000000000000 ) ) ;
#27607 = CARTESIAN_POINT ( 'NONE',  ( -5.405949406249996869, 9.363379034771805109, -198.8437500020484094 ) ) ;
#27608 = CARTESIAN_POINT ( 'NONE',  ( -10.81189881249999729, 6.242252689847871849, -98.40625000204838102 ) ) ;
#27609 = CARTESIAN_POINT ( 'NONE',  ( -9.999999999999998224, 5.773502691896259087, -181.7500000040967905 ) ) ;
#27610 = CARTESIAN_POINT ( 'NONE',  ( 10.81189881249999729, 6.242252689847867408, -106.2187500020483810 ) ) ;
#27611 = CARTESIAN_POINT ( 'NONE',  ( 10.81189881249999729, 0.000000000000000000, -175.5312500020483810 ) ) ;
#27612 = CARTESIAN_POINT ( 'NONE',  ( -10.00000000000102496, 5.773502691895664007, -2.874999999999923617 ) ) ;
#27613 = CARTESIAN_POINT ( 'NONE',  ( 10.70731569305653252, 1.500182182591227154, -180.0000000000000284 ) ) ;
#27614 = CARTESIAN_POINT ( 'NONE',  ( -5.405949406249996869, 9.363379034771805109, -196.0312500020484094 ) ) ;
#27615 = CARTESIAN_POINT ( 'NONE',  ( 10.81189881249999729, 0.000000000000000000, -52.34375000204835260 ) ) ;
#27616 = CARTESIAN_POINT ( 'NONE',  ( 9.999999999999998224, 0.000000000000000000, -171.8750000040968189 ) ) ;
#27617 = CARTESIAN_POINT ( 'NONE',  ( -10.81189881249999907, -6.242252689847864744, -8.156250002048370362 ) ) ;
#27618 = CARTESIAN_POINT ( 'NONE',  ( 5.405949406249992428, -9.363379034771808662, -22.59375000204835615 ) ) ;
#27619 = CARTESIAN_POINT ( 'NONE',  ( 8.614196012144985204, -6.533971456632194474, -180.0000000000000000 ) ) ;
#27620 = CARTESIAN_POINT ( 'NONE',  ( 7.644554776091147741E-16, 12.48450537969573659, -126.9687500020483668 ) ) ;
#27621 = CARTESIAN_POINT ( 'NONE',  ( 7.070501591499377789E-16, 11.54700538379251284, -100.6250000000000000 ) ) ;
#27622 = CARTESIAN_POINT ( 'NONE',  ( -10.81189881249999729, 1.324075727343319199E-15, -26.28125000204836681 ) ) ;
#27623 = CARTESIAN_POINT ( 'NONE',  ( 10.00000000000000000, 5.773502691896255534, -104.2500000040967763 ) ) ;
#27624 =( BOUNDED_CURVE ( )  B_SPLINE_CURVE ( 2, ( #41130, #18053, #11361, #24556, #1676, #28000, #11570 ),
 .UNSPECIFIED., .F., .F. ) 
 B_SPLINE_CURVE_WITH_KNOTS ( ( 3, 2, 2, 3 ),
 ( 0.7761194029850747578, 0.7773631840796021431, 0.7786069651741295283, 0.7798507462686569136 ),
 .UNSPECIFIED. ) 
 CURVE ( )  GEOMETRIC_REPRESENTATION_ITEM ( )  RATIONAL_B_SPLINE_CURVE ( ( 0.9999999999999880096, 0.8660254037844506980, 1.000000000000000000, 0.8660254037844387076, 1.000000000000000000, 0.8660254037844148378, 1.000000000000023981 ) ) 
 REPRESENTATION_ITEM ( '' )  );
#27625 = DIRECTION ( 'NONE',  ( -0.000000000000000000, -0.000000000000000000, 1.000000000000000000 ) ) ;
#27626 = CARTESIAN_POINT ( 'NONE',  ( 7.070501591499377789E-16, 11.54700538379251284, -54.12499999999997868 ) ) ;
#27627 = CARTESIAN_POINT ( 'NONE',  ( -10.81189881249999729, 1.324075727343319199E-15, -125.2812500020483668 ) ) ;
#27628 = CARTESIAN_POINT ( 'NONE',  ( -10.81189881249999729, -6.242252689847864744, -108.6562500020483952 ) ) ;
#27629 = EDGE_LOOP ( 'NONE', ( #39470, #1836, #27726, #16837 ) ) ;
#27630 = CARTESIAN_POINT ( 'NONE',  ( -9.999999999999998224, 1.224646799147353059E-15, -103.6250000040967763 ) ) ;
#27631 = CARTESIAN_POINT ( 'NONE',  ( 9.999999999999998224, 0.000000000000000000, -88.99999999999998579 ) ) ;
#27632 = CARTESIAN_POINT ( 'NONE',  ( 10.81189881249999729, 0.000000000000000000, -165.0312500020484094 ) ) ;
#27633 = CARTESIAN_POINT ( 'NONE',  ( 10.81189881249999729, 0.000000000000000000, -56.84375000204835970 ) ) ;
#27634 = ORIENTED_EDGE ( 'NONE', *, *, #11435, .F. ) ;
#27635 = CARTESIAN_POINT ( 'NONE',  ( -2.121150477449813534E-15, -11.54700538379251284, -24.87499999999998934 ) ) ;
#27636 = CARTESIAN_POINT ( 'NONE',  ( 7.644554776091147741E-16, 12.48450537969573659, -37.15625000204836681 ) ) ;
#27637 = CARTESIAN_POINT ( 'NONE',  ( -10.00000000000000000, -5.773502691896251982, -160.1250000000000284 ) ) ;
#27638 = DIRECTION ( 'NONE',  ( -0.000000000000000000, -0.000000000000000000, 1.000000000000000000 ) ) ;
#27639 = CARTESIAN_POINT ( 'NONE',  ( 9.999999999999996447, -5.773502691896262640, -26.50000000409677270 ) ) ;
#27640 = FACE_OUTER_BOUND ( 'NONE', #25194, .T. ) ;
#27641 = CARTESIAN_POINT ( 'NONE',  ( -10.81189881249999907, -6.242252689847864744, -135.6562500020484094 ) ) ;
#27642 = CARTESIAN_POINT ( 'NONE',  ( -4.999999999999996447, 8.660254037844387298, -46.49999999999998579 ) ) ;
#27643 = CARTESIAN_POINT ( 'NONE',  ( 9.999999999999998224, 0.000000000000000000, -174.8750000040967905 ) ) ;
#27644 = EDGE_LOOP ( 'NONE', ( #20731, #1089, #17584, #9329 ) ) ;
#27646 = ORIENTED_EDGE ( 'NONE', *, *, #14315, .F. ) ;
#27645 = ORIENTED_EDGE ( 'NONE', *, *, #12168, .F. ) ;
#27647 = CARTESIAN_POINT ( 'NONE',  ( -5.000000000000003553, -8.660254037844383745, -46.37500000409677625 ) ) ;
#27648 = CARTESIAN_POINT ( 'NONE',  ( 9.999999999999479527, 5.773502691896553074, -174.7500000040967905 ) ) ;
#27649 = CARTESIAN_POINT ( 'NONE',  ( 10.81189881249999551, -6.242252689847874514, -161.9687500020484094 ) ) ;
#27650 = CARTESIAN_POINT ( 'NONE',  ( 5.405949406249992428, -9.363379034771808662, -193.7812500020484094 ) ) ;
#27651 = CARTESIAN_POINT ( 'NONE',  ( -10.81189881249999907, -6.242252689847864744, -18.46875000204837036 ) ) ;
#27652 = CARTESIAN_POINT ( 'NONE',  ( -9.999999999999998224, 1.224646799147353059E-15, -58.62500000409676204 ) ) ;
#27653 = CARTESIAN_POINT ( 'NONE',  ( 10.81189881249999729, 0.000000000000000000, -149.8437500020483810 ) ) ;
#27654 = CARTESIAN_POINT ( 'NONE',  ( 5.405949406249999534, 9.363379034771803333, -139.0937500020483810 ) ) ;
#27655 = CARTESIAN_POINT ( 'NONE',  ( 5.405949406249992428, -9.363379034771808662, -108.2812500020483810 ) ) ;
#27656 = CARTESIAN_POINT ( 'NONE',  ( 10.81189881249999729, 0.000000000000000000, -115.3437500020483810 ) ) ;
#27657 = CARTESIAN_POINT ( 'NONE',  ( -9.999999999999998224, 1.224646799147353059E-15, -196.6250000040967905 ) ) ;
#27658 = CARTESIAN_POINT ( 'NONE',  ( -5.405949406250003975, -9.363379034771801557, -122.0312500020483952 ) ) ;
#27659 = CARTESIAN_POINT ( 'NONE',  ( 10.81189881249999551, -6.242252689847874514, -5.968750002048344605 ) ) ;
#27661 = EDGE_CURVE ( 'NONE', #35515, #7848, #39615, .T. ) ;
#27660 = CARTESIAN_POINT ( 'NONE',  ( 10.81189881249999729, 6.242252689847867408, -133.2187500020483810 ) ) ;
#27662 = AXIS2_PLACEMENT_3D ( 'NONE', #33958, #20552, #16664 ) ;
#27663 = CARTESIAN_POINT ( 'NONE',  ( 4.999999999999992006, -8.660254037844389075, -166.1250000040967905 ) ) ;
#27664 =( BOUNDED_CURVE ( )  B_SPLINE_CURVE ( 2, ( #37039, #800, #17380, #40681, #17168, #30580, #27977 ),
 .UNSPECIFIED., .F., .F. ) 
 B_SPLINE_CURVE_WITH_KNOTS ( ( 3, 2, 2, 3 ),
 ( 0.3843283582089552786, 0.3855721393034826638, 0.3868159203980099936, 0.3880597014925373789 ),
 .UNSPECIFIED. ) 
 CURVE ( )  GEOMETRIC_REPRESENTATION_ITEM ( )  RATIONAL_B_SPLINE_CURVE ( ( 0.9999999999999940048, 0.8660254037844447028, 1.000000000000000000, 0.8660254037844387076, 1.000000000000000000, 0.8660254037844327124, 1.000000000000005995 ) ) 
 REPRESENTATION_ITEM ( '' )  );
#27665 = CARTESIAN_POINT ( 'NONE',  ( -9.999999999999998224, 1.224646799147353059E-15, -109.6250000040967763 ) ) ;
#27666 = CARTESIAN_POINT ( 'NONE',  ( -9.999999999999998224, 1.224646799147353059E-15, -145.2500000000000000 ) ) ;
#27667 = CARTESIAN_POINT ( 'NONE',  ( -9.999999999999998224, 5.773502691896259087, -23.87499999999998224 ) ) ;
#27668 = SECURITY_CLASSIFICATION ( '', '', #22656 ) ;
#27669 = CARTESIAN_POINT ( 'NONE',  ( 10.81189881249999551, -6.242252689847874514, -77.96875000204838102 ) ) ;
#27670 = CARTESIAN_POINT ( 'NONE',  ( -5.405949406250003975, -9.363379034771801557, -67.84375000204836681 ) ) ;
#27671 = CARTESIAN_POINT ( 'NONE',  ( 10.00000000000102318, -5.773502691895667560, -19.00000000409674428 ) ) ;
#27672 = CARTESIAN_POINT ( 'NONE',  ( -5.405949406249996869, 9.363379034771805109, -31.03125000204837036 ) ) ;
#27673 = CARTESIAN_POINT ( 'NONE',  ( -5.405949406249996869, 9.363379034771805109, -47.34375000204838102 ) ) ;
#27674 = CARTESIAN_POINT ( 'NONE',  ( -9.999999999999872102, -5.773502691896326589, -163.5000000040967620 ) ) ;
#27675 = CARTESIAN_POINT ( 'NONE',  ( -5.405949406249996869, 9.363379034771805109, -152.3437500020483810 ) ) ;
#27676 = CARTESIAN_POINT ( 'NONE',  ( -10.00000000000000000, -5.773502691896251982, -118.1250000000000142 ) ) ;
#27677 = CARTESIAN_POINT ( 'NONE',  ( -10.81189881249999729, 1.324075727343319199E-15, -131.2812500020483810 ) ) ;
#27678 = CARTESIAN_POINT ( 'NONE',  ( 9.602216827598432758, 4.693292424609470714, -179.9999999999999432 ) ) ;
#27679 = CARTESIAN_POINT ( 'NONE',  ( -5.000000000000003553, -8.660254037844383745, -84.99999999999997158 ) ) ;
#27680 = CARTESIAN_POINT ( 'NONE',  ( -5.405949406249996869, 9.363379034771805109, -19.03125000204835970 ) ) ;
#27681 = ORIENTED_EDGE ( 'NONE', *, *, #23603, .T. ) ;
#27682 = CARTESIAN_POINT ( 'NONE',  ( -10.81189881249999729, -6.242252689847864744, -105.6562500020483952 ) ) ;
#27683 = CARTESIAN_POINT ( 'NONE',  ( -10.00000000000000000, -5.773502691896251982, -124.5000000040967620 ) ) ;
#27684 = CARTESIAN_POINT ( 'NONE',  ( 10.00000000000025402, -5.773502691896113426, -154.0000000040967905 ) ) ;
#27685 = CARTESIAN_POINT ( 'NONE',  ( -4.999999999999996447, 8.660254037844387298, -33.37500000409676915 ) ) ;
#27686 = CARTESIAN_POINT ( 'NONE',  ( 5.000000000000000000, 8.660254037844385522, -75.24999999999998579 ) ) ;
#27687 = CARTESIAN_POINT ( 'NONE',  ( -5.405949406249996869, 9.363379034771805109, -47.53125000204838813 ) ) ;
#27688 = CARTESIAN_POINT ( 'NONE',  ( 10.81189881249999551, -6.242252689847874514, -154.6562500020484379 ) ) ;
#27689 = EDGE_CURVE ( 'NONE', #26744, #41802, #39830, .T. ) ;
#27690 = CARTESIAN_POINT ( 'NONE',  ( -5.405949406249996869, 9.363379034771805109, -128.3437500020484094 ) ) ;
#27691 = ORIENTED_EDGE ( 'NONE', *, *, #15619, .F. ) ;
#27692 = CARTESIAN_POINT ( 'NONE',  ( -9.999999999999998224, 1.224646799147353059E-15, -176.7500000000000284 ) ) ;
#27693 = ORIENTED_EDGE ( 'NONE', *, *, #1146, .T. ) ;
#27694 = CIRCLE ( 'NONE', #7021, 24.99999999999999645 ) ;
#27695 = SECURITY_CLASSIFICATION ( '', '', #12032 ) ;
#27696 = EDGE_LOOP ( 'NONE', ( #8845, #11866, #10957, #42016 ) ) ;
#27698 = VERTEX_POINT ( 'NONE', #3379 ) ;
#27697 = CARTESIAN_POINT ( 'NONE',  ( -2.293366432827344421E-15, -12.48450537969573659, -108.2187500020483668 ) ) ;
#27699 = CARTESIAN_POINT ( 'NONE',  ( 10.00000000000051159, -5.773502691895965988, -41.50000000409674072 ) ) ;
#27700 = CARTESIAN_POINT ( 'NONE',  ( -10.81189881249999729, 1.324075727343319199E-15, -191.0937500020484094 ) ) ;
#27701 = VECTOR ( 'NONE', #20140, 1000.000000000000000 ) ;
#27702 = CARTESIAN_POINT ( 'NONE',  ( -10.81189881249999907, -6.242252689847864744, -37.96875000204837391 ) ) ;
#27703 = CARTESIAN_POINT ( 'NONE',  ( 7.446394548109336320, -7.792472342551713282, 3.494387113477268989E-15 ) ) ;
#27704 = DIRECTION ( 'NONE',  ( -0.000000000000000000, -0.000000000000000000, 1.000000000000000000 ) ) ;
#27705 = CARTESIAN_POINT ( 'NONE',  ( -2.293366432827344421E-15, -12.48450537969573659, -168.2187500020483810 ) ) ;
#27706 = CARTESIAN_POINT ( 'NONE',  ( -2.293366432827344421E-15, -12.48450537969573659, -162.2187500020483810 ) ) ;
#27707 = CARTESIAN_POINT ( 'NONE',  ( -9.999999999998456346, -5.773502691897145489, -66.00000000409674783 ) ) ;
#27708 = CARTESIAN_POINT ( 'NONE',  ( -5.405949406250003975, -9.363379034771801557, -142.8437500020483810 ) ) ;
#27709 = CARTESIAN_POINT ( 'NONE',  ( -10.81189881249999729, 6.242252689847871849, -149.4062500020484094 ) ) ;
#27710 = CARTESIAN_POINT ( 'NONE',  ( 10.81189881249999729, 6.242252689847867408, -157.2187500020483810 ) ) ;
#27711 = CARTESIAN_POINT ( 'NONE',  ( -9.999999999999998224, 1.224646799147353059E-15, -155.7500000000000000 ) ) ;
#27712 = CARTESIAN_POINT ( 'NONE',  ( 9.999999999999998224, 0.000000000000000000, -138.8750000040968189 ) ) ;
#27713 = CARTESIAN_POINT ( 'NONE',  ( -4.999999999999996447, 8.660254037844387298, -180.0000000000000000 ) ) ;
#27714 = CARTESIAN_POINT ( 'NONE',  ( -10.81189881249999729, 1.324075727343319199E-15, -89.09375000204838102 ) ) ;
#27715 = CARTESIAN_POINT ( 'NONE',  ( -9.999999999999998224, 1.224646799147353059E-15, -180.1250000040968189 ) ) ;
#27716 = CARTESIAN_POINT ( 'NONE',  ( -5.405949406249996869, 9.363379034771805109, -56.53125000204836681 ) ) ;
#27717 = DIRECTION ( 'NONE',  ( -0.000000000000000000, -0.000000000000000000, 1.000000000000000000 ) ) ;
#27718 = EDGE_CURVE ( 'NONE', #23938, #16772, #25161, .T. ) ;
#27719 = CARTESIAN_POINT ( 'NONE',  ( -5.405949406249996869, 9.363379034771805109, -179.3437500020483810 ) ) ;
#27720 = CARTESIAN_POINT ( 'NONE',  ( 7.644554776091147741E-16, 12.48450537969573659, -118.1562500020483952 ) ) ;
#27721 = CARTESIAN_POINT ( 'NONE',  ( -10.81189881249999729, -6.242252689847864744, -152.1562500020484094 ) ) ;
#27722 = DIRECTION ( 'NONE',  ( 1.000000000000000000, 0.000000000000000000, 0.000000000000000000 ) ) ;
#27723 = CARTESIAN_POINT ( 'NONE',  ( -5.405949406250003975, -9.363379034771801557, -47.03125000204838813 ) ) ;
#27724 = CARTESIAN_POINT ( 'NONE',  ( 4.999999999999992006, -8.660254037844389075, -130.1250000040967620 ) ) ;
#27725 = CARTESIAN_POINT ( 'NONE',  ( -5.000000000000003553, -8.660254037844383745, -105.9999999999999858 ) ) ;
#27726 = ORIENTED_EDGE ( 'NONE', *, *, #37811, .F. ) ;
#27727 = CARTESIAN_POINT ( 'NONE',  ( 5.405949406249999534, 9.363379034771803333, -127.2812500020483810 ) ) ;
#27728 = CARTESIAN_POINT ( 'NONE',  ( -9.999999999999998224, 5.773502691896259087, -147.2500000040967905 ) ) ;
#27729 = DIRECTION ( 'NONE',  ( 1.000000000000000000, 0.000000000000000000, 0.000000000000000000 ) ) ;
#27730 = CARTESIAN_POINT ( 'NONE',  ( -2.293366432827344421E-15, -12.48450537969573659, -180.4062500020484379 ) ) ;
#27731 = EDGE_LOOP ( 'NONE', ( #6926, #39046, #18113, #41543 ) ) ;
#27732 = CARTESIAN_POINT ( 'NONE',  ( 9.999999999999996447, -5.773502691896262640, -51.62499999999999289 ) ) ;
#27733 = CARTESIAN_POINT ( 'NONE',  ( 10.81189881249999729, 0.000000000000000000, -172.3437500020484094 ) ) ;
#27734 = CARTESIAN_POINT ( 'NONE',  ( 9.999999999999996447, -5.773502691896262640, -55.00000000409678336 ) ) ;
#27735 = CARTESIAN_POINT ( 'NONE',  ( -9.999999999999998224, 1.224646799147353059E-15, -163.6250000040967905 ) ) ;
#27736 = CARTESIAN_POINT ( 'NONE',  ( 9.999999999999998224, 0.000000000000000000, -131.0000000000000000 ) ) ;
#27737 = CARTESIAN_POINT ( 'NONE',  ( -5.405949406250003975, -9.363379034771801557, -68.03125000204838102 ) ) ;
#27738 = CARTESIAN_POINT ( 'NONE',  ( -5.405949406250003975, -9.363379034771801557, -54.53125000204836681 ) ) ;
#27739 = CARTESIAN_POINT ( 'NONE',  ( 5.000000000000000000, 8.660254037844385522, -45.62500000409677625 ) ) ;
#27740 = CARTESIAN_POINT ( 'NONE',  ( 7.644554776091147741E-16, 12.48450537969573659, -2.468750002048353043 ) ) ;
#27741 = CARTESIAN_POINT ( 'NONE',  ( -9.999999999999998224, 1.224646799147353059E-15, -30.12500000409676204 ) ) ;
#27742 = CARTESIAN_POINT ( 'NONE',  ( -10.81189881249999729, 6.242252689847871849, -177.9062500020484094 ) ) ;
#27743 = AXIS2_PLACEMENT_3D ( 'NONE', #19702, #18868, #9569 ) ;
#27744 = CARTESIAN_POINT ( 'NONE',  ( -4.999999999999996447, 8.660254037844387298, -147.3750000040967905 ) ) ;
#27745 = CARTESIAN_POINT ( 'NONE',  ( 9.999999999999998224, 0.000000000000000000, -45.87500000409677625 ) ) ;
#27746 = CARTESIAN_POINT ( 'NONE',  ( 9.999999999999998224, 0.000000000000000000, -200.0000000000000000 ) ) ;
#27747 = DIRECTION ( 'NONE',  ( -0.08682659386424779191, 0.08682659386424779191, 0.9924325091389669673 ) ) ;
#27748 = CARTESIAN_POINT ( 'NONE',  ( 0.000000000000000000, 0.000000000000000000, -200.0000000000000000 ) ) ;
#27750 = ORIENTED_EDGE ( 'NONE', *, *, #1370, .T. ) ;
#27749 = CARTESIAN_POINT ( 'NONE',  ( 5.405949406249999534, 9.363379034771803333, -88.28125000204838102 ) ) ;
#27752 = VERTEX_POINT ( 'NONE', #19345 ) ;
#27751 = DIRECTION ( 'NONE',  ( -0.3779644730092256433, -0.6546536707079758655, -0.6546536707079793072 ) ) ;
#27753 = ORIENTED_EDGE ( 'NONE', *, *, #3590, .F. ) ;
#27754 = CARTESIAN_POINT ( 'NONE',  ( 10.81189881249999551, -6.242252689847874514, -40.46875000204835260 ) ) ;
#27755 = CARTESIAN_POINT ( 'NONE',  ( -5.405949406250003975, -9.363379034771801557, -25.84375000204835970 ) ) ;
#27756 = CARTESIAN_POINT ( 'NONE',  ( -10.81189881249999907, -6.242252689847864744, -12.65625000204835970 ) ) ;
#27758 = VERTEX_POINT ( 'NONE', #13490 ) ;
#27757 = CARTESIAN_POINT ( 'NONE',  ( -10.81189881249999729, 1.324075727343319199E-15, -66.59375000204836681 ) ) ;
#27759 = DIRECTION ( 'NONE',  ( -0.000000000000000000, -0.000000000000000000, 1.000000000000000000 ) ) ;
#27760 = CARTESIAN_POINT ( 'NONE',  ( 9.999999999999996447, -5.773502691896262640, -47.12499999999997868 ) ) ;
#27761 = CARTESIAN_POINT ( 'NONE',  ( 10.81189881249999729, 0.000000000000000000, -188.8437500020483810 ) ) ;
#27762 = CARTESIAN_POINT ( 'NONE',  ( -5.405949406249996869, 9.363379034771805109, -162.8437500020484094 ) ) ;
#27763 = CARTESIAN_POINT ( 'NONE',  ( 5.405949406249992428, -9.363379034771808662, -178.5937500020484094 ) ) ;
#27764 = CARTESIAN_POINT ( 'NONE',  ( -9.999999999999676703, -5.773502691896437611, -183.0000000040967905 ) ) ;
#27765 = CARTESIAN_POINT ( 'NONE',  ( -9.999999999999998224, 1.224646799147353059E-15, -200.0000000000000000 ) ) ;
#27766 = DIRECTION ( 'NONE',  ( 1.000000000000000000, 0.000000000000000000, 0.000000000000000000 ) ) ;
#27767 = CARTESIAN_POINT ( 'NONE',  ( -9.999999999999998224, 1.224646799147353059E-15, -188.7500000000000000 ) ) ;
#27768 = CARTESIAN_POINT ( 'NONE',  ( -10.81189881249999729, 1.324075727343319199E-15, -113.0937500020483810 ) ) ;
#27769 = LINE ( 'NONE', #40692, #7347 ) ;
#27770 = CARTESIAN_POINT ( 'NONE',  ( -10.81189881249999729, 1.324075727343319199E-15, -81.78125000204839523 ) ) ;
#27771 = ADVANCED_FACE ( 'NONE', ( #39411 ), #9637, .T. ) ;
#27772 = CARTESIAN_POINT ( 'NONE',  ( 5.405949406249999534, 9.363379034771803333, -100.0937500020483810 ) ) ;
#27773 = CARTESIAN_POINT ( 'NONE',  ( 5.405949406249999534, 9.363379034771803333, -59.59375000204835970 ) ) ;
#27774 = EDGE_CURVE ( 'NONE', #15995, #41544, #4467, .T. ) ;
#27775 = CARTESIAN_POINT ( 'NONE',  ( 10.81189881249999729, 0.000000000000000000, -69.03125000204838102 ) ) ;
#27776 = CARTESIAN_POINT ( 'NONE',  ( 4.999999999999992006, -8.660254037844389075, -152.6250000040967905 ) ) ;
#27777 = CARTESIAN_POINT ( 'NONE',  ( -10.00000000000000000, -5.773502691896251982, -134.6250000000000000 ) ) ;
#27778 = EDGE_CURVE ( 'NONE', #25691, #24966, #26678, .T. ) ;
#27779 = CARTESIAN_POINT ( 'NONE',  ( -10.81189881249999729, 6.242252689847871849, -153.9062500020483810 ) ) ;
#27780 = CARTESIAN_POINT ( 'NONE',  ( 5.405949406249992428, -9.363379034771808662, -168.2812500020484094 ) ) ;
#27781 = CARTESIAN_POINT ( 'NONE',  ( 5.000000000000000000, 8.660254037844385522, -98.12500000409677625 ) ) ;
#27782 = CARTESIAN_POINT ( 'NONE',  ( -9.999999999999998224, 1.224646799147353059E-15, -32.74999999999997158 ) ) ;
#27783 = CARTESIAN_POINT ( 'NONE',  ( -10.81189881249999729, 6.242252689847871849, -98.21875000204838102 ) ) ;
#27784 = LINE ( 'NONE', #14373, #3172 ) ;
#27785 = CARTESIAN_POINT ( 'NONE',  ( -9.999999999999998224, 1.224646799147353059E-15, -76.24999999999998579 ) ) ;
#27786 = CARTESIAN_POINT ( 'NONE',  ( -5.405949406249996869, 9.363379034771805109, 0.4687499979516285276 ) ) ;
#27787 = CARTESIAN_POINT ( 'NONE',  ( 9.999999999999996447, -5.773502691896262640, -80.50000000409676204 ) ) ;
#27788 = CARTESIAN_POINT ( 'NONE',  ( 9.999999999999998224, 0.000000000000000000, -132.8750000040967905 ) ) ;
#27789 = CC_DESIGN_DATE_AND_TIME_ASSIGNMENT ( #22186, #39005, ( #40065 ) ) ;
#27790 = CARTESIAN_POINT ( 'NONE',  ( -10.81189881249999729, 6.242252689847871849, -101.4062500020483952 ) ) ;
#27791 = CARTESIAN_POINT ( 'NONE',  ( 5.405949406249992428, -9.363379034771808662, -76.78125000204838102 ) ) ;
#27792 =( BOUNDED_CURVE ( )  B_SPLINE_CURVE ( 2, ( #38519, #6151, #25790, #15416, #41542, #38946, #9379 ),
 .UNSPECIFIED., .F., .F. ) 
 B_SPLINE_CURVE_WITH_KNOTS ( ( 3, 2, 2, 3 ),
 ( 0.2798507462686568026, 0.2810945273631841879, 0.2823383084577115731, 0.2835820895522389029 ),
 .UNSPECIFIED. ) 
 CURVE ( )  GEOMETRIC_REPRESENTATION_ITEM ( )  RATIONAL_B_SPLINE_CURVE ( ( 0.9999999999999880096, 0.8660254037844506980, 1.000000000000000000, 0.8660254037844387076, 1.000000000000000000, 0.8660254037844267172, 1.000000000000011990 ) ) 
 REPRESENTATION_ITEM ( '' )  );
#27793 = CARTESIAN_POINT ( 'NONE',  ( -9.999999999999998224, 5.773502691896259087, -75.25000000409677625 ) ) ;
#27794 = CARTESIAN_POINT ( 'NONE',  ( -9.999999999999998224, 1.224646799147353059E-15, -133.2499999999999716 ) ) ;
#27795 = CARTESIAN_POINT ( 'NONE',  ( 10.81189881249999729, 0.000000000000000000, -22.34375000204835615 ) ) ;
#27796 = ORIENTED_EDGE ( 'NONE', *, *, #22756, .F. ) ;
#27797 = CARTESIAN_POINT ( 'NONE',  ( 7.644554776091147741E-16, 12.48450537969573659, -197.6562500020484379 ) ) ;
#27798 = CARTESIAN_POINT ( 'NONE',  ( -2.293366432827344421E-15, -12.48450537969573659, -31.90625000204835970 ) ) ;
#27799 = CARTESIAN_POINT ( 'NONE',  ( -10.81189881249999729, 1.324075727343319199E-15, -11.09375000204834727 ) ) ;
#27800 = EDGE_CURVE ( 'NONE', #4342, #32995, #22594, .T. ) ;
#27801 = CARTESIAN_POINT ( 'NONE',  ( 10.00000000000000000, 5.773502691896255534, -2.250000004096752715 ) ) ;
#27802 = CARTESIAN_POINT ( 'NONE',  ( -5.405949406250003975, -9.363379034771801557, -126.5312500020483952 ) ) ;
#27803 = ADVANCED_FACE ( 'NONE', ( #35771 ), #2961, .T. ) ;
#27804 = CARTESIAN_POINT ( 'NONE',  ( 7.070501591499377789E-16, 11.54700538379251284, -183.1250000000000000 ) ) ;
#27805 = FACE_OUTER_BOUND ( 'NONE', #31001, .T. ) ;
#27807 = EDGE_LOOP ( 'NONE', ( #10407, #32438 ) ) ;
#27806 = CARTESIAN_POINT ( 'NONE',  ( -5.405949406250003975, -9.363379034771801557, -113.0312500020483952 ) ) ;
#27808 = FACE_OUTER_BOUND ( 'NONE', #22319, .T. ) ;
#27809 = EDGE_CURVE ( 'NONE', #10098, #18914, #29554, .T. ) ;
#27810 = VERTEX_POINT ( 'NONE', #30140 ) ;
#27811 = ORIENTED_EDGE ( 'NONE', *, *, #38726, .F. ) ;
#27812 = CARTESIAN_POINT ( 'NONE',  ( 5.405949406249992428, -9.363379034771808662, -34.78125000204837391 ) ) ;
#27813 = PERSON_AND_ORGANIZATION_ROLE ( 'design_supplier' ) ;
#27814 = CARTESIAN_POINT ( 'NONE',  ( -10.81189881249999907, -6.242252689847864744, -88.96875000204836681 ) ) ;
#27815 = CARTESIAN_POINT ( 'NONE',  ( -2.121150477449813534E-15, -11.54700538379251284, -167.3750000000000000 ) ) ;
#27816 = CARTESIAN_POINT ( 'NONE',  ( -9.999999999999479527, -5.773502691896549521, -109.1249999999999716 ) ) ;
#27817 = DIRECTION ( 'NONE',  ( 1.000000000000000000, 0.000000000000000000, 0.000000000000000000 ) ) ;
#27818 = CARTESIAN_POINT ( 'NONE',  ( 10.81189881249999551, -6.242252689847874514, -166.6562500020484094 ) ) ;
#27819 = CARTESIAN_POINT ( 'NONE',  ( 1.351487262974977233, 10.72709830801206543, -100.0000000000000000 ) ) ;
#27820 = CARTESIAN_POINT ( 'NONE',  ( 10.81189881249999551, -6.242252689847874514, -127.4687500020483810 ) ) ;
#27821 = CARTESIAN_POINT ( 'NONE',  ( -10.81189881249999907, -6.242252689847864744, -87.46875000204838102 ) ) ;
#27822 = CARTESIAN_POINT ( 'NONE',  ( -10.81189881249999729, 6.242252689847871849, -0.9062500020483681418 ) ) ;
#27823 = CARTESIAN_POINT ( 'NONE',  ( 10.81189881249999551, -6.242252689847874514, -193.4687500020484094 ) ) ;
#27824 = CARTESIAN_POINT ( 'NONE',  ( 10.81189881249999551, -6.242252689847874514, -88.65625000204838102 ) ) ;
#27825 = CARTESIAN_POINT ( 'NONE',  ( -5.000000000000003553, -8.660254037844383745, -179.8750000040967905 ) ) ;
#27826 = CARTESIAN_POINT ( 'NONE',  ( -5.405949406250003975, -9.363379034771801557, -105.3437500020483810 ) ) ;
#27827 = CARTESIAN_POINT ( 'NONE',  ( -2.293366432827344421E-15, -12.48450537969573659, -166.9062500020484379 ) ) ;
#27828 = EDGE_CURVE ( 'NONE', #18233, #36337, #41124, .T. ) ;
#27829 = CARTESIAN_POINT ( 'NONE',  ( 9.999999999998969713, 5.773502691896851502, -69.37499999999997158 ) ) ;
#27830 = CARTESIAN_POINT ( 'NONE',  ( 10.81189881249999729, 6.242252689847867408, -170.9062500020484094 ) ) ;
#27831 = CARTESIAN_POINT ( 'NONE',  ( 10.81189881249999551, -6.242252689847874514, -184.6562500020484094 ) ) ;
#27832 = CARTESIAN_POINT ( 'NONE',  ( 10.81189881249999729, 0.000000000000000000, -55.34375000204835970 ) ) ;
#27833 = CARTESIAN_POINT ( 'NONE',  ( 7.070501591499377789E-16, 11.54700538379251284, -173.0000000040967905 ) ) ;
#27834 = CARTESIAN_POINT ( 'NONE',  ( -10.81189881249999729, 1.324075727343319199E-15, -14.28125000204835615 ) ) ;
#27835 = CARTESIAN_POINT ( 'NONE',  ( 5.405949406249992428, -9.363379034771808662, -19.59375000204835615 ) ) ;
#27836 = CARTESIAN_POINT ( 'NONE',  ( 10.00000000000012257, -5.773502691896187144, -193.0000000040968189 ) ) ;
#27837 = CARTESIAN_POINT ( 'NONE',  ( 5.405949406249999534, 9.363379034771803333, -124.0937500020483952 ) ) ;
#27838 = CARTESIAN_POINT ( 'NONE',  ( 7.070501591499377789E-16, 11.54700538379251284, -96.12500000000000000 ) ) ;
#27839 = CARTESIAN_POINT ( 'NONE',  ( 7.644554776091147741E-16, 12.48450537969573659, -25.15625000204837747 ) ) ;
#27840 = CARTESIAN_POINT ( 'NONE',  ( 9.999999999999996447, -5.773502691896262640, -107.5000000040967763 ) ) ;
#27841 = CARTESIAN_POINT ( 'NONE',  ( -2.121150477449813534E-15, -11.54700538379251284, -190.2500000040967905 ) ) ;
#27842 = CARTESIAN_POINT ( 'NONE',  ( 4.999999999999992006, -8.660254037844389075, -48.74999999999998579 ) ) ;
#27843 = CARTESIAN_POINT ( 'NONE',  ( 5.405949406249999534, 9.363379034771803333, -122.7812500020483952 ) ) ;
#27844 = CARTESIAN_POINT ( 'NONE',  ( -2.293366432827344421E-15, -12.48450537969573659, -99.40625000204839523 ) ) ;
#27845 = VERTEX_POINT ( 'NONE', #11323 ) ;
#27846 = CARTESIAN_POINT ( 'NONE',  ( 5.000000000000000000, 8.660254037844385522, -102.6250000040967905 ) ) ;
#27847 = CARTESIAN_POINT ( 'NONE',  ( -9.999999999999479527, -5.773502691896549521, -113.6249999999999716 ) ) ;
#27848 = CARTESIAN_POINT ( 'NONE',  ( -2.293366432827344421E-15, -12.48450537969573659, -163.9062500020483810 ) ) ;
#27849 = CARTESIAN_POINT ( 'NONE',  ( -10.81189881249999729, 1.324075727343319199E-15, -57.59375000204835970 ) ) ;
#27850 = ORIENTED_EDGE ( 'NONE', *, *, #23823, .F. ) ;
#27851 = CARTESIAN_POINT ( 'NONE',  ( -9.999999999999998224, 5.773502691896259087, -22.37499999999997868 ) ) ;
#27852 = CARTESIAN_POINT ( 'NONE',  ( 10.81189881249999729, 0.000000000000000000, -31.53125000204837391 ) ) ;
#27853 = CARTESIAN_POINT ( 'NONE',  ( -9.999999999999998224, 1.224646799147353059E-15, -158.7500000000000000 ) ) ;
#27854 = FACE_OUTER_BOUND ( 'NONE', #28724, .T. ) ;
#27855 = CARTESIAN_POINT ( 'NONE',  ( 4.999999999999992006, -8.660254037844389075, -29.62500000409676204 ) ) ;
#27856 = EDGE_CURVE ( 'NONE', #41318, #41327, #24516, .T. ) ;
#27857 = CARTESIAN_POINT ( 'NONE',  ( 10.00000000000102318, -5.773502691895667560, -33.62499999999993605 ) ) ;
#27858 = CARTESIAN_POINT ( 'NONE',  ( -10.81189881249999729, 1.324075727343319199E-15, -134.2812500020483810 ) ) ;
#27859 = CARTESIAN_POINT ( 'NONE',  ( 9.999999999999479527, 5.773502691896553074, -75.75000000409676204 ) ) ;
#27860 = CARTESIAN_POINT ( 'NONE',  ( -9.999999999999868550, 5.773502691896333694, -174.2500000040967905 ) ) ;
#27861 = ORIENTED_EDGE ( 'NONE', *, *, #8554, .T. ) ;
#27862 = CARTESIAN_POINT ( 'NONE',  ( -5.405949406249996869, 9.363379034771805109, -65.53125000204838102 ) ) ;
#27864 = ORIENTED_EDGE ( 'NONE', *, *, #2377, .F. ) ;
#27863 = ORIENTED_EDGE ( 'NONE', *, *, #36779, .F. ) ;
#27865 = CYLINDRICAL_SURFACE ( 'NONE', #32530, 9.999999999999998224 ) ;
#27866 = CARTESIAN_POINT ( 'NONE',  ( 10.81189881249999729, 0.000000000000000000, -155.8437500020483810 ) ) ;
#27867 = CARTESIAN_POINT ( 'NONE',  ( -5.405949406250003975, -9.363379034771801557, -191.0312500020484094 ) ) ;
#27868 = CARTESIAN_POINT ( 'NONE',  ( 7.644554776091147741E-16, 12.48450537969573659, -11.46875000204836859 ) ) ;
#27869 = CARTESIAN_POINT ( 'NONE',  ( 0.000000000000000000, 0.000000000000000000, -200.0000000000000000 ) ) ;
#27870 = CARTESIAN_POINT ( 'NONE',  ( 10.81189881249999729, 6.242252689847867408, -151.2187500020484094 ) ) ;
#27871 = CARTESIAN_POINT ( 'NONE',  ( -10.81189881249999729, 1.324075727343319199E-15, -131.0937500020483810 ) ) ;
#27872 =( BOUNDED_CURVE ( )  B_SPLINE_CURVE ( 2, ( #31323, #1755, #5193, #14884, #28079, #41208, #11647 ),
 .UNSPECIFIED., .F., .F. ) 
 B_SPLINE_CURVE_WITH_KNOTS ( ( 3, 2, 2, 3 ),
 ( 0.6455223880597016350, 0.6467661691542290203, 0.6480099502487564056, 0.6492537313432837909 ),
 .UNSPECIFIED. ) 
 CURVE ( )  GEOMETRIC_REPRESENTATION_ITEM ( )  RATIONAL_B_SPLINE_CURVE ( ( 0.9999999999999880096, 0.8660254037844506980, 1.000000000000000000, 0.8660254037844387076, 1.000000000000000000, 0.8660254037844148378, 1.000000000000023981 ) ) 
 REPRESENTATION_ITEM ( '' )  );
#27873 = CARTESIAN_POINT ( 'NONE',  ( 10.81189881249999907, 6.242252689847868297, -109.4062500020483952 ) ) ;
#27874 = CARTESIAN_POINT ( 'NONE',  ( 5.405949406249992428, -9.363379034771808662, -121.5937500020483952 ) ) ;
#27875 = CARTESIAN_POINT ( 'NONE',  ( -9.999999999999998224, 1.224646799147353059E-15, -190.6250000040967905 ) ) ;
#27876 = CARTESIAN_POINT ( 'NONE',  ( -10.81189881249999729, 6.242252689847871849, -125.4062500020483810 ) ) ;
#27877 = CARTESIAN_POINT ( 'NONE',  ( 5.405949406249992428, -9.363379034771808662, -3.093750002048367698 ) ) ;
#27878 = CARTESIAN_POINT ( 'NONE',  ( 10.81189881249999729, 0.000000000000000000, -133.3437500020484094 ) ) ;
#27879 = CARTESIAN_POINT ( 'NONE',  ( 9.999999999999998224, 0.000000000000000000, -54.49999999999996447 ) ) ;
#27880 = CARTESIAN_POINT ( 'NONE',  ( -9.999999999999996447, 5.773502691896259975, -165.2500000040967905 ) ) ;
#27881 = CARTESIAN_POINT ( 'NONE',  ( -5.000000000000003553, -8.660254037844383745, -148.0000000000000000 ) ) ;
#27882 = CARTESIAN_POINT ( 'NONE',  ( 4.999999999999992006, -8.660254037844389075, -20.24999999999996092 ) ) ;
#27883 = CARTESIAN_POINT ( 'NONE',  ( -10.81189881249999729, -6.242252689847864744, -72.46875000204836681 ) ) ;
#27884 = CARTESIAN_POINT ( 'NONE',  ( 7.644554776091147741E-16, 12.48450537969573659, -57.96875000204836681 ) ) ;
#27885 = CARTESIAN_POINT ( 'NONE',  ( -9.999999999999998224, 1.224646799147353059E-15, -117.1250000040967905 ) ) ;
#27886 = CARTESIAN_POINT ( 'NONE',  ( -2.293366432827344421E-15, -12.48450537969573659, -37.90625000204836681 ) ) ;
#27887 = CARTESIAN_POINT ( 'NONE',  ( 10.81189881249999551, -6.242252689847874514, -41.96875000204836681 ) ) ;
#27888 = FACE_OUTER_BOUND ( 'NONE', #35183, .T. ) ;
#27889 = CARTESIAN_POINT ( 'NONE',  ( -2.293366432827344421E-15, -12.48450537969573659, -156.2187500020483810 ) ) ;
#27890 = CARTESIAN_POINT ( 'NONE',  ( 5.000000000000000000, 8.660254037844385522, -121.7500000000000000 ) ) ;
#27891 = CARTESIAN_POINT ( 'NONE',  ( -10.81189881249999729, -6.242252689847864744, -129.6562500020483810 ) ) ;
#27892 = CARTESIAN_POINT ( 'NONE',  ( 8.928897960546947843, 5.779144828205879492, -179.9999999999999716 ) ) ;
#27893 = CARTESIAN_POINT ( 'NONE',  ( 5.000000000000000000, 8.660254037844385522, -73.74999999999998579 ) ) ;
#27894 = CARTESIAN_POINT ( 'NONE',  ( -10.81189881249999729, 1.324075727343319199E-15, -12.78125000204835615 ) ) ;
#27895 = ORIENTED_EDGE ( 'NONE', *, *, #11969, .T. ) ;
#27896 = CARTESIAN_POINT ( 'NONE',  ( -5.405949406250003975, -9.363379034771801557, -101.0312500020483952 ) ) ;
#27897 = CARTESIAN_POINT ( 'NONE',  ( 9.999999999999998224, 0.000000000000000000, -126.8750000040967905 ) ) ;
#27898 = CARTESIAN_POINT ( 'NONE',  ( 4.999999999999992006, -8.660254037844389075, -143.6250000040967905 ) ) ;
#27899 = CARTESIAN_POINT ( 'NONE',  ( 5.405949406249999534, 9.363379034771803333, -83.59375000204836681 ) ) ;
#27900 = EDGE_CURVE ( 'NONE', #5939, #23120, #17576, .T. ) ;
#27901 = CARTESIAN_POINT ( 'NONE',  ( 5.000000000000000000, 8.660254037844385522, -35.12500000409676915 ) ) ;
#27902 = CARTESIAN_POINT ( 'NONE',  ( 5.405949406249992428, -9.363379034771808662, -43.78125000204838102 ) ) ;
#27903 = CARTESIAN_POINT ( 'NONE',  ( 10.81189881249999907, 6.242252689847868297, -154.4062500020484094 ) ) ;
#27904 = CARTESIAN_POINT ( 'NONE',  ( -2.293366432827344421E-15, -12.48450537969573659, -124.7187500020483668 ) ) ;
#27905 = DIRECTION ( 'NONE',  ( -1.000000000000000000, 0.000000000000000000, 0.000000000000000000 ) ) ;
#27906 = ORIENTED_EDGE ( 'NONE', *, *, #41442, .F. ) ;
#27907 = ADVANCED_BREP_SHAPE_REPRESENTATION ( '', ( #28380, #39998 ), #29026 ) ;
#27908 = CARTESIAN_POINT ( 'NONE',  ( -9.999999999999998224, 1.224646799147353059E-15, -22.24999999999996447 ) ) ;
#27910 = EDGE_CURVE ( 'NONE', #29986, #18454, #42521, .T. ) ;
#27909 = ORIENTED_EDGE ( 'NONE', *, *, #34660, .T. ) ;
#27911 = ORIENTED_EDGE ( 'NONE', *, *, #1065, .T. ) ;
#27912 = ORIENTED_EDGE ( 'NONE', *, *, #2743, .F. ) ;
#27913 = CARTESIAN_POINT ( 'NONE',  ( 9.999999999999998224, 0.000000000000000000, -165.5000000000000000 ) ) ;
#27914 =( BOUNDED_CURVE ( )  B_SPLINE_CURVE ( 2, ( #5237, #21198, #11477, #38040, #24891, #24678, #15356 ),
 .UNSPECIFIED., .F., .F. ) 
 B_SPLINE_CURVE_WITH_KNOTS ( ( 3, 2, 2, 3 ),
 ( 0.9216417910447763928, 0.9228855721393036671, 0.9241293532338311634, 0.9253731343283585487 ),
 .UNSPECIFIED. ) 
 CURVE ( )  GEOMETRIC_REPRESENTATION_ITEM ( )  RATIONAL_B_SPLINE_CURVE ( ( 0.9999999999999761302, 0.8660254037844625774, 1.000000000000000000, 0.8660254037844387076, 1.000000000000000000, 0.8660254037844028474, 1.000000000000035971 ) ) 
 REPRESENTATION_ITEM ( '' )  );
#27915 = CARTESIAN_POINT ( 'NONE',  ( -10.81189881249999729, 1.324075727343319199E-15, -189.5937500020483810 ) ) ;
#27916 = CARTESIAN_POINT ( 'NONE',  ( -5.405949406250003975, -9.363379034771801557, -39.34375000204837391 ) ) ;
#27917 = CARTESIAN_POINT ( 'NONE',  ( -7.750360283152410545, -6.449078031086257212, -1.202135122527668287E-14 ) ) ;
#27918 = CYLINDRICAL_SURFACE ( 'NONE', #2498, 9.999999999999998224 ) ;
#27919 = CARTESIAN_POINT ( 'NONE',  ( -2.293366432827344421E-15, -12.48450537969573659, -172.7187500020483810 ) ) ;
#27920 = CARTESIAN_POINT ( 'NONE',  ( -10.81189881249999907, -6.242252689847864744, -150.4687500020484094 ) ) ;
#27921 = CARTESIAN_POINT ( 'NONE',  ( 9.999999999999998224, 0.000000000000000000, -122.3750000040967905 ) ) ;
#27922 = CARTESIAN_POINT ( 'NONE',  ( 7.644554776091147741E-16, 12.48450537969573659, -140.4687500020483810 ) ) ;
#27923 = AXIS2_PLACEMENT_3D ( 'NONE', #26777, #17040, #30240 ) ;
#27924 = CARTESIAN_POINT ( 'NONE',  ( -2.293366432827344421E-15, -12.48450537969573659, -148.9062500020483810 ) ) ;
#27925 = CARTESIAN_POINT ( 'NONE',  ( 10.81189881249999729, 6.242252689847867408, -152.7187500020483810 ) ) ;
#27926 = CARTESIAN_POINT ( 'NONE',  ( -42.00000000000001421, 0.000000000000000000, -200.0000000000000000 ) ) ;
#27927 =( BOUNDED_CURVE ( )  B_SPLINE_CURVE ( 2, ( #624, #20024, #12900, #26516, #19809, #13110, #40088 ),
 .UNSPECIFIED., .F., .F. ) 
 B_SPLINE_CURVE_WITH_KNOTS ( ( 3, 2, 2, 3 ),
 ( 0.2611940298507463565, 0.2624378109452737418, 0.2636815920398011270, 0.2649253731343284568 ),
 .UNSPECIFIED. ) 
 CURVE ( )  GEOMETRIC_REPRESENTATION_ITEM ( )  RATIONAL_B_SPLINE_CURVE ( ( 0.9999999999999880096, 0.8660254037844506980, 1.000000000000000000, 0.8660254037844387076, 1.000000000000000000, 0.8660254037844267172, 1.000000000000011990 ) ) 
 REPRESENTATION_ITEM ( '' )  );
#27928 = CARTESIAN_POINT ( 'NONE',  ( 0.000000000000000000, 0.000000000000000000, -200.0000000000000000 ) ) ;
#27929 = CARTESIAN_POINT ( 'NONE',  ( 9.999999999999996447, -5.773502691896262640, -168.6250000000000000 ) ) ;
#27930 = CARTESIAN_POINT ( 'NONE',  ( 7.644554776091147741E-16, 12.48450537969573659, -90.96875000204838102 ) ) ;
#27931 = CARTESIAN_POINT ( 'NONE',  ( -5.000000000000003553, -8.660254037844383745, -113.4999999999999858 ) ) ;
#27932 = CARTESIAN_POINT ( 'NONE',  ( 5.405949406249992428, -9.363379034771808662, -57.28125000204836681 ) ) ;
#27933 = CARTESIAN_POINT ( 'NONE',  ( -9.999999999999479527, -5.773502691896549521, -149.6249999999999716 ) ) ;
#27934 = CARTESIAN_POINT ( 'NONE',  ( -10.81189881249999907, -6.242252689847864744, -180.4687500020484094 ) ) ;
#27935 = CARTESIAN_POINT ( 'NONE',  ( 5.405949406249992428, -9.363379034771808662, -111.2812500020483810 ) ) ;
#27936 = CARTESIAN_POINT ( 'NONE',  ( -10.81189881249999729, 1.324075727343319199E-15, -156.7812500020484094 ) ) ;
#27937 = CARTESIAN_POINT ( 'NONE',  ( 0.000000000000000000, 0.000000000000000000, -99.99999999999998579 ) ) ;
#27938 = CARTESIAN_POINT ( 'NONE',  ( 5.405949406249992428, -9.363379034771808662, -42.28125000204838102 ) ) ;
#27939 = CARTESIAN_POINT ( 'NONE',  ( -2.121150477449813534E-15, -11.54700538379251284, -131.7500000040967905 ) ) ;
#27940 = CARTESIAN_POINT ( 'NONE',  ( -9.999999999999998224, 1.224646799147353059E-15, -95.74999999999998579 ) ) ;
#27941 = EDGE_CURVE ( 'NONE', #28436, #41419, #33801, .T. ) ;
#27942 = ORIENTED_EDGE ( 'NONE', *, *, #18445, .T. ) ;
#27943 = AXIS2_PLACEMENT_3D ( 'NONE', #9774, #6969, #6340 ) ;
#27944 = CARTESIAN_POINT ( 'NONE',  ( 7.644554776091147741E-16, 12.48450537969573659, -124.1562500020483810 ) ) ;
#27945 = CARTESIAN_POINT ( 'NONE',  ( 5.000000000000000000, 8.660254037844385522, -149.1250000040967905 ) ) ;
#27946 = CARTESIAN_POINT ( 'NONE',  ( 9.999999999999998224, 0.000000000000000000, -185.0000000000000000 ) ) ;
#27947 = CARTESIAN_POINT ( 'NONE',  ( -5.405949406249996869, 9.363379034771805109, -181.0312500020483810 ) ) ;
#27948 = VERTEX_POINT ( 'NONE', #20830 ) ;
#27949 = CARTESIAN_POINT ( 'NONE',  ( -5.405949406250003975, -9.363379034771801557, -174.3437500020484094 ) ) ;
#27950 = CARTESIAN_POINT ( 'NONE',  ( -9.999999999999998224, 1.224646799147353059E-15, -54.12500000409675494 ) ) ;
#27951 = DIRECTION ( 'NONE',  ( -0.000000000000000000, -0.000000000000000000, -1.000000000000000000 ) ) ;
#27952 = DIRECTION ( 'NONE',  ( 1.000000000000000000, 0.000000000000000000, 0.000000000000000000 ) ) ;
#27953 = CARTESIAN_POINT ( 'NONE',  ( -5.405949406250003975, -9.363379034771801557, -71.03125000204838102 ) ) ;
#27954 = CARTESIAN_POINT ( 'NONE',  ( 10.81189881249999729, 0.000000000000000000, -51.03125000204835970 ) ) ;
#27955 = CARTESIAN_POINT ( 'NONE',  ( 9.999999999999998224, 0.000000000000000000, -45.87500000409677625 ) ) ;
#27956 = CARTESIAN_POINT ( 'NONE',  ( 5.405949406249999534, 9.363379034771803333, -1.093750002048365921 ) ) ;
#27957 = CARTESIAN_POINT ( 'NONE',  ( 9.999999999998969713, 5.773502691896851502, -88.87499999999998579 ) ) ;
#27958 = CARTESIAN_POINT ( 'NONE',  ( -10.81189881249999729, 6.242252689847871849, -174.9062500020483810 ) ) ;
#27959 = CARTESIAN_POINT ( 'NONE',  ( -2.121150477449813534E-15, -11.54700538379251284, -87.87500000000000000 ) ) ;
#27960 = CARTESIAN_POINT ( 'NONE',  ( 9.999999999999998224, 0.000000000000000000, -198.5000000000000000 ) ) ;
#27961 = ORIENTED_EDGE ( 'NONE', *, *, #13792, .T. ) ;
#27962 = CARTESIAN_POINT ( 'NONE',  ( -9.999999999999998224, 1.224646799147353059E-15, -16.62500000409675138 ) ) ;
#27963 = CARTESIAN_POINT ( 'NONE',  ( 9.999999999999998224, 0.000000000000000000, -60.49999999999997158 ) ) ;
#27964 = CARTESIAN_POINT ( 'NONE',  ( 5.000000000000000000, 8.660254037844385522, -39.62500000409676915 ) ) ;
#27966 = ORIENTED_EDGE ( 'NONE', *, *, #24327, .F. ) ;
#27965 = CARTESIAN_POINT ( 'NONE',  ( 5.405949406249992428, -9.363379034771808662, -82.78125000204838102 ) ) ;
#27967 = CARTESIAN_POINT ( 'NONE',  ( -10.00000000000154188, 5.773502691895366468, -24.25000000409672296 ) ) ;
#27968 = EDGE_CURVE ( 'NONE', #35088, #26744, #33902, .T. ) ;
#27970 = ORIENTED_EDGE ( 'NONE', *, *, #33871, .T. ) ;
#27969 = DIRECTION ( 'NONE',  ( -0.000000000000000000, -0.000000000000000000, -1.000000000000000000 ) ) ;
#27971 = ORIENTED_EDGE ( 'NONE', *, *, #3823, .T. ) ;
#27972 = CARTESIAN_POINT ( 'NONE',  ( -10.81189881249999729, -6.242252689847864744, -39.46875000204835970 ) ) ;
#27973 = CARTESIAN_POINT ( 'NONE',  ( -5.000000000000002665, 20.00000000000000000, -219.9999999999999716 ) ) ;
#27974 = CARTESIAN_POINT ( 'NONE',  ( 10.81189881249999551, -6.242252689847874514, -13.65625000204836503 ) ) ;
#27976 = ORIENTED_EDGE ( 'NONE', *, *, #37433, .T. ) ;
#27975 = CARTESIAN_POINT ( 'NONE',  ( -10.81189881249999729, 1.324075727343319199E-15, -60.59375000204836681 ) ) ;
#27977 = CARTESIAN_POINT ( 'NONE',  ( 9.999999999999998224, 0.000000000000000000, -122.0000000000000000 ) ) ;
#27978 = CARTESIAN_POINT ( 'NONE',  ( 7.070501591499377789E-16, 11.54700538379251284, -36.12499999999996447 ) ) ;
#27979 = CARTESIAN_POINT ( 'NONE',  ( -10.81189881249999907, -6.242252689847864744, -183.4687500020484379 ) ) ;
#27980 = CARTESIAN_POINT ( 'NONE',  ( 5.405949406249992428, -9.363379034771808662, -166.5937500020484094 ) ) ;
#27981 = CARTESIAN_POINT ( 'NONE',  ( 10.81189881249999551, -3.636584649182867057, -179.9165719629227169 ) ) ;
#27982 = CARTESIAN_POINT ( 'NONE',  ( 4.999999999999992006, -8.660254037844389075, -182.6250000040967905 ) ) ;
#27983 = CARTESIAN_POINT ( 'NONE',  ( 9.999999999999479527, 5.773502691896553074, -141.3750000000000000 ) ) ;
#27984 = CARTESIAN_POINT ( 'NONE',  ( -9.999999999999998224, 1.224646799147353059E-15, -21.12500000409675494 ) ) ;
#27985 = CARTESIAN_POINT ( 'NONE',  ( -2.121150477449813534E-15, -11.54700538379251284, -197.3750000000000284 ) ) ;
#27986 = CARTESIAN_POINT ( 'NONE',  ( 10.81189881249999551, -6.242252689847874514, -110.9687500020483810 ) ) ;
#27987 = DIRECTION ( 'NONE',  ( 0.000000000000000000, 0.000000000000000000, -1.000000000000000000 ) ) ;
#27988 = CARTESIAN_POINT ( 'NONE',  ( 10.81189881249999551, -6.242252689847874514, -79.65625000204838102 ) ) ;
#27989 = CARTESIAN_POINT ( 'NONE',  ( -10.81189881249999729, 1.324075727343319199E-15, -95.09375000204838102 ) ) ;
#27990 = CARTESIAN_POINT ( 'NONE',  ( -10.81189881249999729, 1.324075727343319199E-15, -62.09375000204836681 ) ) ;
#27991 = AXIS2_PLACEMENT_3D ( 'NONE', #20950, #24641, #21599 ) ;
#27992 = CARTESIAN_POINT ( 'NONE',  ( -10.81189881249999729, 6.242252689847871849, -68.40625000204839523 ) ) ;
#27993 = CARTESIAN_POINT ( 'NONE',  ( 4.999999999999992006, -8.660254037844389075, -154.1250000040967905 ) ) ;
#27994 = CARTESIAN_POINT ( 'NONE',  ( -2.121150477449813534E-15, -11.54700538379251284, -134.3750000000000000 ) ) ;
#27995 = CARTESIAN_POINT ( 'NONE',  ( -2.293366432827344421E-15, -12.48450537969573659, -150.4062500020484379 ) ) ;
#27996 = CARTESIAN_POINT ( 'NONE',  ( 5.405949406249992428, -9.363379034771808662, -166.7812500020484094 ) ) ;
#27997 = LINE ( 'NONE', #24553, #37866 ) ;
#27998 = FACE_OUTER_BOUND ( 'NONE', #39624, .T. ) ;
#27999 = CARTESIAN_POINT ( 'NONE',  ( 7.644554776091147741E-16, 12.48450537969573659, -96.96875000204838102 ) ) ;
#28000 = CARTESIAN_POINT ( 'NONE',  ( -10.00000000000102496, 5.773502691895664007, -42.25000000409672651 ) ) ;
#28001 = CARTESIAN_POINT ( 'NONE',  ( -5.000000000000003553, -8.660254037844383745, -71.49999999999998579 ) ) ;
#28002 = CARTESIAN_POINT ( 'NONE',  ( -2.293366432827344421E-15, -12.48450537969573659, -0.4062500020483583718 ) ) ;
#28003 = CARTESIAN_POINT ( 'NONE',  ( -4.999999999999996447, 8.660254037844387298, -78.37500000409677625 ) ) ;
#28004 =( BOUNDED_CURVE ( )  B_SPLINE_CURVE ( 2, ( #22954, #19483, #36108, #32670, #3098, #6542, #9979 ),
 .UNSPECIFIED., .F., .F. ) 
 B_SPLINE_CURVE_WITH_KNOTS ( ( 3, 2, 2, 3 ),
 ( 0.4962686567164180107, 0.4975124378109453960, 0.4987562189054727257, 0.5000000000000001110 ),
 .UNSPECIFIED. ) 
 CURVE ( )  GEOMETRIC_REPRESENTATION_ITEM ( )  RATIONAL_B_SPLINE_CURVE ( ( 0.9999999999999880096, 0.8660254037844506980, 1.000000000000000000, 0.8660254037844387076, 1.000000000000000000, 0.8660254037844267172, 1.000000000000011990 ) ) 
 REPRESENTATION_ITEM ( '' )  );
#28005 = CARTESIAN_POINT ( 'NONE',  ( 5.000000000000000000, 8.660254037844385522, -26.12500000409675849 ) ) ;
#28006 = CARTESIAN_POINT ( 'NONE',  ( 10.81189881249999729, 0.000000000000000000, -90.03125000204838102 ) ) ;
#28007 = CARTESIAN_POINT ( 'NONE',  ( 5.405949406249992428, -9.363379034771808662, -73.78125000204838102 ) ) ;
#28008 = B_SPLINE_CURVE_WITH_KNOTS ( 'NONE', 3,
 ( #9847, #16300, #3806, #6824, #16730, #7251, #16516, #23233, #32737, #19767 ),
 .UNSPECIFIED., .F., .F.,
 ( 4, 2, 2, 2, 4 ),
 ( 0.000000000000000000, 0.04166666664189333513, 0.08333333328378667026, 0.1249999999256800054, 0.1666666665675733405 ),
 .UNSPECIFIED. ) ;
#28009 = CARTESIAN_POINT ( 'NONE',  ( 4.999999999999992006, -8.660254037844389075, -71.62500000409677625 ) ) ;
#28010 = CARTESIAN_POINT ( 'NONE',  ( 7.070501591499376803E-16, 11.54700538379251284, -113.0000000040967763 ) ) ;
#28011 = CARTESIAN_POINT ( 'NONE',  ( -10.81189881249999729, 6.242252689847871849, -26.21875000204837391 ) ) ;
#28012 = ORIENTED_EDGE ( 'NONE', *, *, #10900, .F. ) ;
#28013 = CARTESIAN_POINT ( 'NONE',  ( -5.000000000000003553, -8.660254037844383745, -5.499999999999976907 ) ) ;
#28014 = CARTESIAN_POINT ( 'NONE',  ( -5.405949406250003975, -9.363379034771801557, -18.53125000204835970 ) ) ;
#28015 = CARTESIAN_POINT ( 'NONE',  ( -10.81189881249999729, 6.242252689847871849, -15.71875000204835793 ) ) ;
#28016 = CARTESIAN_POINT ( 'NONE',  ( 9.999999999999998224, 0.000000000000000000, -63.87500000409676915 ) ) ;
#28017 = CARTESIAN_POINT ( 'NONE',  ( -2.121150477449813534E-15, -11.54700538379251284, 0.2499999959032495056 ) ) ;
#28018 = CARTESIAN_POINT ( 'NONE',  ( -10.00000000000025580, 5.773502691896109873, -160.7500000040967620 ) ) ;
#28019 = CARTESIAN_POINT ( 'NONE',  ( -5.405949406249996869, 9.363379034771805109, -133.0312500020484094 ) ) ;
#28020 = CARTESIAN_POINT ( 'NONE',  ( -5.000000000000003553, -8.660254037844383745, -184.0000000000000000 ) ) ;
#28021 = CARTESIAN_POINT ( 'NONE',  ( -2.121150477449813534E-15, -11.54700538379251284, -35.75000000409675494 ) ) ;
#28023 = ORIENTED_EDGE ( 'NONE', *, *, #11053, .F. ) ;
#28022 = CARTESIAN_POINT ( 'NONE',  ( 5.405949406249992428, -9.363379034771808662, -111.2812500020483810 ) ) ;
#28024 = CARTESIAN_POINT ( 'NONE',  ( -9.999999999999612754, -5.773502691896474914, -154.5000000040967905 ) ) ;
#28025 = EDGE_CURVE ( 'NONE', #40993, #41044, #7897, .T. ) ;
#28026 = ORIENTED_EDGE ( 'NONE', *, *, #8053, .F. ) ;
#28027 = ADVANCED_FACE ( 'NONE', ( #24310 ), #20401, .F. ) ;
#28028 = VECTOR ( 'NONE', #16581, 1000.000000000000000 ) ;
#28029 = VERTEX_POINT ( 'NONE', #30568 ) ;
#28030 = CARTESIAN_POINT ( 'NONE',  ( -2.293366432827344421E-15, -12.48450537969573659, -40.90625000204836681 ) ) ;
#28031 = PERSON_AND_ORGANIZATION ( #11915, #17965 ) ;
#28032 = CARTESIAN_POINT ( 'NONE',  ( 5.405949406249999534, 9.363379034771803333, -85.09375000204836681 ) ) ;
#28033 = DIRECTION ( 'NONE',  ( 1.000000000000000000, 0.000000000000000000, 0.000000000000000000 ) ) ;
#28034 = CARTESIAN_POINT ( 'NONE',  ( -2.121150477449813534E-15, -11.54700538379251284, -108.8749999999999858 ) ) ;
#28035 = CYLINDRICAL_SURFACE ( 'NONE', #34336, 9.999999999999998224 ) ;
#28036 = CARTESIAN_POINT ( 'NONE',  ( -10.81189881249999729, 6.242252689847871849, -167.4062500020483810 ) ) ;
#28037 = DIRECTION ( 'NONE',  ( -0.000000000000000000, -0.000000000000000000, -1.000000000000000000 ) ) ;
#28038 = CARTESIAN_POINT ( 'NONE',  ( -2.293366432827344421E-15, -12.48450537969573659, -112.7187500020483668 ) ) ;
#28039 = PRODUCT_DEFINITION_SHAPE ( 'NONE', 'NONE',  #19626 ) ;
#28040 = CARTESIAN_POINT ( 'NONE',  ( -5.405949406250003975, -9.363379034771801557, -87.34375000204836681 ) ) ;
#28041 = CARTESIAN_POINT ( 'NONE',  ( 10.81189881249999729, 6.242252689847867408, -5.906250002048359704 ) ) ;
#28042 = CARTESIAN_POINT ( 'NONE',  ( 5.405949406249999534, 9.363379034771803333, -191.5937500020484094 ) ) ;
#28043 = CARTESIAN_POINT ( 'NONE',  ( 7.644554776091147741E-16, 12.48450537969573659, -94.15625000204839523 ) ) ;
#28044 = CARTESIAN_POINT ( 'NONE',  ( 10.00000000000000000, 5.773502691896255534, -180.7500000040968189 ) ) ;
#28045 = CARTESIAN_POINT ( 'NONE',  ( -10.81189881249999729, 1.324075727343319199E-15, -171.7812500020484094 ) ) ;
#28046 =( BOUNDED_CURVE ( )  B_SPLINE_CURVE ( 2, ( #2648, #5679, #15147, #9117, #35247, #31805, #38683 ),
 .UNSPECIFIED., .F., .F. ) 
 B_SPLINE_CURVE_WITH_KNOTS ( ( 3, 2, 2, 3 ),
 ( 0.5970149253731344974, 0.5982587064676618827, 0.5995024875621891569, 0.6007462686567165422 ),
 .UNSPECIFIED. ) 
 CURVE ( )  GEOMETRIC_REPRESENTATION_ITEM ( )  RATIONAL_B_SPLINE_CURVE ( ( 0.9999999999999761302, 0.8660254037844625774, 1.000000000000000000, 0.8660254037844387076, 1.000000000000000000, 0.8660254037844267172, 1.000000000000011990 ) ) 
 REPRESENTATION_ITEM ( '' )  );
#28047 = CARTESIAN_POINT ( 'NONE',  ( 7.070501591499376803E-16, 11.54700538379251284, -103.6249999999999858 ) ) ;
#28048 = CARTESIAN_POINT ( 'NONE',  ( 5.405949406249999534, 9.363379034771803333, -173.7812500020484094 ) ) ;
#28049 = CARTESIAN_POINT ( 'NONE',  ( 10.81189881249999729, 0.000000000000000000, -192.0312500020484094 ) ) ;
#28050 = CARTESIAN_POINT ( 'NONE',  ( 5.405949406249999534, 9.363379034771803333, -50.59375000204835260 ) ) ;
#28051 = CARTESIAN_POINT ( 'NONE',  ( 10.00000000000000000, 5.773502691896255534, -164.2500000040967905 ) ) ;
#28052 = CARTESIAN_POINT ( 'NONE',  ( -5.405949406249996869, 9.363379034771805109, -8.531250002048352599 ) ) ;
#28053 = CARTESIAN_POINT ( 'NONE',  ( -5.405949406249996869, 9.363379034771805109, -15.84375000204835082 ) ) ;
#28054 = FACE_OUTER_BOUND ( 'NONE', #41434, .T. ) ;
#28055 = CARTESIAN_POINT ( 'NONE',  ( 7.644554776091147741E-16, 12.48450537969573659, -125.4687500020483952 ) ) ;
#28056 = CARTESIAN_POINT ( 'NONE',  ( -2.121150477449813534E-15, -11.54700538379251284, -95.37500000000000000 ) ) ;
#28057 = CARTESIAN_POINT ( 'NONE',  ( -10.81189881249999729, 6.242252689847871849, -18.90625000204837391 ) ) ;
#28058 = CARTESIAN_POINT ( 'NONE',  ( -10.00000000000000000, -5.773502691896251982, -103.5000000040967763 ) ) ;
#28059 = DIRECTION ( 'NONE',  ( -0.000000000000000000, -0.000000000000000000, 1.000000000000000000 ) ) ;
#28060 = CARTESIAN_POINT ( 'NONE',  ( -9.999999999999998224, 1.224646799147353059E-15, -53.74999999999996447 ) ) ;
#28061 = CARTESIAN_POINT ( 'NONE',  ( 7.644554776091147741E-16, 12.48450537969573659, -113.6562500020483952 ) ) ;
#28062 = CARTESIAN_POINT ( 'NONE',  ( 5.405949406249992428, -9.363379034771808662, -102.2812500020483952 ) ) ;
#28063 = ORIENTED_EDGE ( 'NONE', *, *, #4849, .F. ) ;
#28064 = CARTESIAN_POINT ( 'NONE',  ( 10.00000000000000000, 5.773502691896255534, -90.75000000409677625 ) ) ;
#28065 = LINE ( 'NONE', #31092, #12556 ) ;
#28066 = CARTESIAN_POINT ( 'NONE',  ( -5.405949406249996869, 9.363379034771805109, -157.0312500020484094 ) ) ;
#28067 = CARTESIAN_POINT ( 'NONE',  ( -2.293366432827344421E-15, -12.48450537969573659, -49.71875000204836681 ) ) ;
#28068 = ORIENTED_EDGE ( 'NONE', *, *, #21446, .T. ) ;
#28069 = CARTESIAN_POINT ( 'NONE',  ( 9.999999999999998224, 0.000000000000000000, -27.49999999999996803 ) ) ;
#28070 = CLOSED_SHELL ( 'NONE', ( #32298, #23591, #16275, #39638, #18619, #11383, #3002, #28357, #5527, #26775, #41929, #22812, #29648, #13284 ) ) ;
#28071 = CARTESIAN_POINT ( 'NONE',  ( 5.405949406249999534, 9.363379034771803333, -23.78125000204836681 ) ) ;
#28072 = CARTESIAN_POINT ( 'NONE',  ( 5.000000000000000000, 8.660254037844385522, -162.2500000000000000 ) ) ;
#28073 = LINE ( 'NONE', #30880, #35288 ) ;
#28074 = CARTESIAN_POINT ( 'NONE',  ( -5.000000000000003553, -8.660254037844383745, -28.37500000409676204 ) ) ;
#28075 = DIRECTION ( 'NONE',  ( -0.000000000000000000, -0.000000000000000000, -1.000000000000000000 ) ) ;
#28076 = CARTESIAN_POINT ( 'NONE',  ( 10.81189881249999907, 6.242252689847868297, -134.9062500020483810 ) ) ;
#28077 = CARTESIAN_POINT ( 'NONE',  ( 7.070501591499376803E-16, 11.54700538379251284, -111.1249999999999858 ) ) ;
#28078 = ADVANCED_FACE ( 'NONE', ( #27532 ), #14116, .F. ) ;
#28079 = CARTESIAN_POINT ( 'NONE',  ( 4.999999999999992006, -8.660254037844389075, -68.62500000409677625 ) ) ;
#28080 = ORIENTED_EDGE ( 'NONE', *, *, #30729, .T. ) ;
#28081 = EDGE_CURVE ( 'NONE', #25114, #15207, #6115, .T. ) ;
#28082 = CARTESIAN_POINT ( 'NONE',  ( -5.405949406250003975, -9.363379034771801557, -59.03125000204836681 ) ) ;
#28083 = APPROVAL_ROLE ( '' ) ;
#28084 = EDGE_CURVE ( 'NONE', #37499, #7028, #4715, .T. ) ;
#28086 = ORIENTED_EDGE ( 'NONE', *, *, #37948, .F. ) ;
#28085 = ORIENTED_EDGE ( 'NONE', *, *, #24858, .F. ) ;
#28087 = CARTESIAN_POINT ( 'NONE',  ( -9.999999999999998224, 1.224646799147353059E-15, -161.7500000000000000 ) ) ;
#28088 = APPROVAL ( #25276, 'UNSPECIFIED' ) ;
#28089 = CYLINDRICAL_SURFACE ( 'NONE', #11823, 9.999999999999998224 ) ;
#28090 = CARTESIAN_POINT ( 'NONE',  ( 5.405949406249999534, 9.363379034771803333, -155.5937500020483810 ) ) ;
#28091 = CARTESIAN_POINT ( 'NONE',  ( 10.81189881249999729, 0.000000000000000000, -187.5312500020484094 ) ) ;
#28092 = CARTESIAN_POINT ( 'NONE',  ( 10.81189881249999907, 6.242252689847868297, -10.21875000204836326 ) ) ;
#28093 = LINE ( 'NONE', #21165, #4672 ) ;
#28094 = EDGE_CURVE ( 'NONE', #28405, #1054, #21474, .T. ) ;
#28095 = CARTESIAN_POINT ( 'NONE',  ( -5.405949406249996869, 9.363379034771805109, -146.3437500020483810 ) ) ;
#28096 = CARTESIAN_POINT ( 'NONE',  ( -10.81189881249999729, 1.324075727343319199E-15, -104.2812500020483810 ) ) ;
#28097 = CARTESIAN_POINT ( 'NONE',  ( -10.81189881249999729, 1.324075727343319199E-15, -108.5937500020483810 ) ) ;
#28098 = LINE ( 'NONE', #22251, #15959 ) ;
#28099 = CARTESIAN_POINT ( 'NONE',  ( -10.81189881249999729, 1.324075727343319199E-15, -119.2812500020483952 ) ) ;
#28100 = CARTESIAN_POINT ( 'NONE',  ( -5.405949406249996869, 9.363379034771805109, -3.843750002048368586 ) ) ;
#28102 = EDGE_CURVE ( 'NONE', #17690, #18615, #14982, .T. ) ;
#28101 = CARTESIAN_POINT ( 'NONE',  ( -5.405949406249996869, 9.363379034771805109, -129.8437500020484094 ) ) ;
#28103 = CARTESIAN_POINT ( 'NONE',  ( -5.405949406250003975, -9.363379034771801557, -194.0312500020484094 ) ) ;
#28104 = CARTESIAN_POINT ( 'NONE',  ( 9.999999999999996447, -5.773502691896262640, -150.6250000000000000 ) ) ;
#28105 = CARTESIAN_POINT ( 'NONE',  ( -4.999999999999996447, 8.660254037844387298, -10.49999999999995381 ) ) ;
#28106 = CARTESIAN_POINT ( 'NONE',  ( 5.405949406249999534, 9.363379034771803333, -74.59375000204838102 ) ) ;
#28107 = CARTESIAN_POINT ( 'NONE',  ( -10.81189881249999729, 1.324075727343319199E-15, -60.59375000204836681 ) ) ;
#28108 = CARTESIAN_POINT ( 'NONE',  ( -9.999999999999998224, 1.224646799147353059E-15, -187.6250000040967905 ) ) ;
#28109 = CARTESIAN_POINT ( 'NONE',  ( -2.293366432827344421E-15, -12.48450537969573659, -31.90625000204835970 ) ) ;
#28110 = AXIS2_PLACEMENT_3D ( 'NONE', #14188, #1713, #11396 ) ;
#28111 = CARTESIAN_POINT ( 'NONE',  ( 10.81189881249999551, -6.242252689847874514, -34.46875000204835260 ) ) ;
#28112 = DIRECTION ( 'NONE',  ( -0.000000000000000000, -0.000000000000000000, 1.000000000000000000 ) ) ;
#28113 = CARTESIAN_POINT ( 'NONE',  ( 10.81189881249999907, 6.242252689847868297, -143.7187500020483810 ) ) ;
#28114 = CARTESIAN_POINT ( 'NONE',  ( -2.121150477449813534E-15, -11.54700538379251284, -119.3749999999999858 ) ) ;
#28115 = CARTESIAN_POINT ( 'NONE',  ( 7.070501591499376803E-16, 11.54700538379251284, -42.12499999999997158 ) ) ;
#28116 = CARTESIAN_POINT ( 'NONE',  ( -10.00000000000000000, -5.773502691896251982, -79.12499999999998579 ) ) ;
#28117 = CARTESIAN_POINT ( 'NONE',  ( 5.405949406249992428, -9.363379034771808662, -13.78125000204835615 ) ) ;
#28118 = VERTEX_POINT ( 'NONE', #25156 ) ;
#28119 = CARTESIAN_POINT ( 'NONE',  ( -5.405949406249996869, 9.363379034771805109, -100.0312500020483952 ) ) ;
#28120 = CARTESIAN_POINT ( 'NONE',  ( -2.121150477449813534E-15, -11.54700538379251284, -125.7500000040967763 ) ) ;
#28121 = LINE ( 'NONE', #1579, #38768 ) ;
#28122 = CARTESIAN_POINT ( 'NONE',  ( -10.81189881249999729, 1.324075727343319199E-15, -74.09375000204838102 ) ) ;
#28123 = CARTESIAN_POINT ( 'NONE',  ( -9.999999999999998224, 1.224646799147353059E-15, -34.62500000409676915 ) ) ;
#28124 = CARTESIAN_POINT ( 'NONE',  ( -5.000000000000003553, -8.660254037844383745, -2.875000004096767370 ) ) ;
#28125 = CARTESIAN_POINT ( 'NONE',  ( -5.405949406249996869, 9.363379034771805109, -41.53125000204838102 ) ) ;
#28126 = CARTESIAN_POINT ( 'NONE',  ( 9.999999999999998224, 0.000000000000000000, -150.5000000000000000 ) ) ;
#28127 = CARTESIAN_POINT ( 'NONE',  ( -5.405949406250003975, -9.363379034771801557, -146.0312500020483810 ) ) ;
#28128 = CARTESIAN_POINT ( 'NONE',  ( 10.81189881249999551, -6.242252689847874514, -124.4687500020483952 ) ) ;
#28129 = CARTESIAN_POINT ( 'NONE',  ( 5.000000000000000000, 8.660254037844385522, -165.6250000040967905 ) ) ;
#28130 = CARTESIAN_POINT ( 'NONE',  ( 9.999999999999998224, 0.000000000000000000, -120.5000000000000000 ) ) ;
#28131 = ORIENTED_EDGE ( 'NONE', *, *, #12241, .T. ) ;
#28132 = VERTEX_POINT ( 'NONE', #1638 ) ;
#28133 = AXIS2_PLACEMENT_3D ( 'NONE', #37472, #21501, #7699 ) ;
#28134 = ORIENTED_EDGE ( 'NONE', *, *, #39278, .T. ) ;
#28135 = AXIS2_PLACEMENT_3D ( 'NONE', #24907, #2657, #41700 ) ;
#28136 =( BOUNDED_CURVE ( )  B_SPLINE_CURVE ( 2, ( #16031, #32681, #22966, #42580, #29439, #32890, #13003 ),
 .UNSPECIFIED., .F., .F. ) 
 B_SPLINE_CURVE_WITH_KNOTS ( ( 3, 2, 2, 3 ),
 ( 0.2164179104477612636, 0.2176616915422886489, 0.2189054726368160064, 0.2201492537313433639 ),
 .UNSPECIFIED. ) 
 CURVE ( )  GEOMETRIC_REPRESENTATION_ITEM ( )  RATIONAL_B_SPLINE_CURVE ( ( 0.9999999999999910072, 0.8660254037844477004, 1.000000000000000000, 0.8660254037844387076, 1.000000000000000000, 0.8660254037844297148, 1.000000000000008882 ) ) 
 REPRESENTATION_ITEM ( '' )  );
#28137 = CARTESIAN_POINT ( 'NONE',  ( -4.999999999999996447, 8.660254037844387298, -189.0000000000000000 ) ) ;
#28138 = CARTESIAN_POINT ( 'NONE',  ( -10.81189881249999729, 1.324075727343319199E-15, -182.0937500020483810 ) ) ;
#28140 = ADVANCED_FACE ( 'NONE', ( #18656 ), #24951, .F. ) ;
#28139 = CARTESIAN_POINT ( 'NONE',  ( 5.405949406249999534, 9.363379034771803333, -43.09375000204837391 ) ) ;
#28141 = CARTESIAN_POINT ( 'NONE',  ( -5.405949406249996869, 9.363379034771805109, -173.3437500020484094 ) ) ;
#28142 = CARTESIAN_POINT ( 'NONE',  ( 7.644554776091147741E-16, 12.48450537969573659, -153.9687500020484094 ) ) ;
#28143 = CARTESIAN_POINT ( 'NONE',  ( 4.999999999999992006, -8.660254037844389075, -25.12500000409675849 ) ) ;
#28144 = CARTESIAN_POINT ( 'NONE',  ( 5.405949406249992428, -9.363379034771808662, -135.0937500020483810 ) ) ;
#28145 = CARTESIAN_POINT ( 'NONE',  ( -2.293366432827344421E-15, -12.48450537969573659, -138.4062500020483810 ) ) ;
#28146 = CARTESIAN_POINT ( 'NONE',  ( 5.405949406249999534, 9.363379034771803333, -152.5937500020483810 ) ) ;
#28147 = CARTESIAN_POINT ( 'NONE',  ( -10.00000000000076916, 5.773502691895813221, -127.3749999999999858 ) ) ;
#28148 = CARTESIAN_POINT ( 'NONE',  ( 9.999999999999998224, 0.000000000000000000, -170.0000000000000000 ) ) ;
#28149 = CARTESIAN_POINT ( 'NONE',  ( -10.81189881249999907, -6.242252689847864744, -79.96875000204836681 ) ) ;
#28150 = CARTESIAN_POINT ( 'NONE',  ( -9.999999999999227285, -5.773502691896698735, -136.1249999999999716 ) ) ;
#28151 = CARTESIAN_POINT ( 'NONE',  ( 10.81189881249999907, 6.242252689847868297, -61.40625000204838102 ) ) ;
#28152 = CARTESIAN_POINT ( 'NONE',  ( -10.43766569794794208, -0.1000697250298307195, -99.99999999999998579 ) ) ;
#28153 = CARTESIAN_POINT ( 'NONE',  ( 5.405949406249999534, 9.363379034771803333, -172.0937500020484094 ) ) ;
#28154 = CARTESIAN_POINT ( 'NONE',  ( -10.81189881249999907, -6.242252689847864744, -117.6562500020483952 ) ) ;
#28155 = CARTESIAN_POINT ( 'NONE',  ( 7.644554776091147741E-16, 12.48450537969573659, -154.1562500020484094 ) ) ;
#28156 = CARTESIAN_POINT ( 'NONE',  ( -2.121150477449813534E-15, -11.54700538379251284, -23.75000000409677270 ) ) ;
#28157 = CARTESIAN_POINT ( 'NONE',  ( 10.81189881249999907, 6.242252689847868297, -47.90625000204837391 ) ) ;
#28158 = CARTESIAN_POINT ( 'NONE',  ( -9.999999999999998224, 5.773502691896259087, -118.7500000040967905 ) ) ;
#28159 = CARTESIAN_POINT ( 'NONE',  ( -2.121150477449813534E-15, -11.54700538379251284, -98.37500000000000000 ) ) ;
#28160 = ORIENTED_EDGE ( 'NONE', *, *, #24079, .F. ) ;
#28161 = CARTESIAN_POINT ( 'NONE',  ( -5.405949406249996869, 9.363379034771805109, -125.5312500020483952 ) ) ;
#28162 = CARTESIAN_POINT ( 'NONE',  ( -9.999999999999998224, 1.224646799147353059E-15, -151.6250000040967905 ) ) ;
#28163 = DIRECTION ( 'NONE',  ( -0.000000000000000000, 1.000000000000000000, -0.000000000000000000 ) ) ;
#28164 = CARTESIAN_POINT ( 'NONE',  ( -2.293366432827344421E-15, -12.48450537969573659, -177.4062500020483810 ) ) ;
#28165 = ORIENTED_EDGE ( 'NONE', *, *, #31256, .F. ) ;
#28166 = CARTESIAN_POINT ( 'NONE',  ( -5.405949406249996869, 9.363379034771805109, -176.3437500020483810 ) ) ;
#28167 = CARTESIAN_POINT ( 'NONE',  ( -5.000000000000003553, -8.660254037844383745, -59.87500000409676204 ) ) ;
#28168 = VECTOR ( 'NONE', #15589, 1000.000000000000000 ) ;
#28169 = CARTESIAN_POINT ( 'NONE',  ( -2.121150477449813534E-15, -11.54700538379251284, -165.8750000000000000 ) ) ;
#28170 = CARTESIAN_POINT ( 'NONE',  ( 9.999999999999998224, 0.000000000000000000, -57.87500000409676204 ) ) ;
#28171 = CARTESIAN_POINT ( 'NONE',  ( -10.81189881249999729, 6.242252689847871849, -68.40625000204839523 ) ) ;
#28172 = CARTESIAN_POINT ( 'NONE',  ( -5.000000000000003553, -8.660254037844383745, -40.37500000409677625 ) ) ;
#28173 = CARTESIAN_POINT ( 'NONE',  ( 5.405949406249992428, -9.363379034771808662, -6.093750002048370362 ) ) ;
#28174 = CARTESIAN_POINT ( 'NONE',  ( -10.00000000000154188, 5.773502691895366468, -9.250000004096717632 ) ) ;
#28175 = CARTESIAN_POINT ( 'NONE',  ( 5.405949406249992428, -9.363379034771808662, -165.2812500020484094 ) ) ;
#28176 = LINE ( 'NONE', #32056, #3595 ) ;
#28177 = LINE ( 'NONE', #34232, #30297 ) ;
#28178 = ORIENTED_EDGE ( 'NONE', *, *, #39889, .F. ) ;
#28179 = DIRECTION ( 'NONE',  ( 1.000000000000000000, 0.000000000000000000, 0.000000000000000000 ) ) ;
#28180 = PLANE ( 'NONE',  #14842 ) ;
#28181 =( BOUNDED_CURVE ( )  B_SPLINE_CURVE ( 2, ( #304, #20340, #33533, #26619, #39768, #23388, #20134 ),
 .UNSPECIFIED., .F., .F. ) 
 B_SPLINE_CURVE_WITH_KNOTS ( ( 3, 2, 2, 3 ),
 ( 0.2164179104477612636, 0.2176616915422886489, 0.2189054726368160064, 0.2201492537313433639 ),
 .UNSPECIFIED. ) 
 CURVE ( )  GEOMETRIC_REPRESENTATION_ITEM ( )  RATIONAL_B_SPLINE_CURVE ( ( 0.9999999999999910072, 0.8660254037844477004, 1.000000000000000000, 0.8660254037844387076, 1.000000000000000000, 0.8660254037844297148, 1.000000000000008882 ) ) 
 REPRESENTATION_ITEM ( '' )  );
#28182 = CYLINDRICAL_SURFACE ( 'NONE', #35167, 9.999999999999998224 ) ;
#28184 = ORIENTED_EDGE ( 'NONE', *, *, #28081, .T. ) ;
#28183 = CARTESIAN_POINT ( 'NONE',  ( -2.293366432827344421E-15, -12.48450537969573659, -78.40625000204838102 ) ) ;
#28185 = DIRECTION ( 'NONE',  ( 0.000000000000000000, 0.000000000000000000, 1.000000000000000000 ) ) ;
#28187 = VERTEX_POINT ( 'NONE', #5083 ) ;
#28186 = CARTESIAN_POINT ( 'NONE',  ( -9.999999999999998224, 1.224646799147353059E-15, -140.7500000000000000 ) ) ;
#28188 = ORIENTED_EDGE ( 'NONE', *, *, #9016, .T. ) ;
#28189 = CARTESIAN_POINT ( 'NONE',  ( -10.81189881249999729, -6.242252689847864744, -36.46875000204835970 ) ) ;
#28190 = CARTESIAN_POINT ( 'NONE',  ( 7.070501591499376803E-16, 11.54700538379251284, -74.00000000409677625 ) ) ;
#28191 = CARTESIAN_POINT ( 'NONE',  ( -5.405949406249996869, 9.363379034771805109, -8.531250002048352599 ) ) ;
#28192 =( BOUNDED_CURVE ( )  B_SPLINE_CURVE ( 2, ( #24355, #31258, #37497, #14813, #21090, #10731, #34278 ),
 .UNSPECIFIED., .F., .F. ) 
 B_SPLINE_CURVE_WITH_KNOTS ( ( 3, 2, 2, 3 ),
 ( 0.3208955223880597396, 0.3221393034825871804, 0.3233830845771145657, 0.3246268656716419510 ),
 .UNSPECIFIED. ) 
 CURVE ( )  GEOMETRIC_REPRESENTATION_ITEM ( )  RATIONAL_B_SPLINE_CURVE ( ( 0.9999999999999940048, 0.8660254037844447028, 1.000000000000000000, 0.8660254037844387076, 1.000000000000000000, 0.8660254037844207220, 1.000000000000017986 ) ) 
 REPRESENTATION_ITEM ( '' )  );
#28194 = EDGE_LOOP ( 'NONE', ( #18496, #24189, #16200, #20241 ) ) ;
#28193 = CARTESIAN_POINT ( 'NONE',  ( -5.405949406249996869, 9.363379034771805109, -66.84375000204836681 ) ) ;
#28195 = CARTESIAN_POINT ( 'NONE',  ( -4.999999999999996447, 8.660254037844387298, -112.4999999999999858 ) ) ;
#28196 = CARTESIAN_POINT ( 'NONE',  ( 4.999999999999992006, -8.660254037844389075, -39.74999999999997868 ) ) ;
#28197 = CARTESIAN_POINT ( 'NONE',  ( 10.81189881249999551, -6.242252689847874514, -197.9687500020484094 ) ) ;
#28198 = CARTESIAN_POINT ( 'NONE',  ( -2.293366432827344421E-15, -12.48450537969573659, -175.7187500020483810 ) ) ;
#28199 = CARTESIAN_POINT ( 'NONE',  ( 10.81189881249999729, 0.000000000000000000, -154.3437500020483810 ) ) ;
#28200 = CARTESIAN_POINT ( 'NONE',  ( 9.999999999999998224, 0.000000000000000000, -43.99999999999998579 ) ) ;
#28201 = CARTESIAN_POINT ( 'NONE',  ( -9.999999999999998224, 1.224646799147353059E-15, -112.2499999999999858 ) ) ;
#28202 = CARTESIAN_POINT ( 'NONE',  ( -9.999999999999998224, 1.224646799147353059E-15, -7.625000004096743389 ) ) ;
#28203 = CARTESIAN_POINT ( 'NONE',  ( 9.999999999999996447, -5.773502691896262640, -197.1250000000000284 ) ) ;
#28204 = CARTESIAN_POINT ( 'NONE',  ( 5.405949406249992428, -9.363379034771808662, -106.5937500020483810 ) ) ;
#28205 = DIRECTION ( 'NONE',  ( -0.000000000000000000, -0.000000000000000000, 1.000000000000000000 ) ) ;
#28206 = CARTESIAN_POINT ( 'NONE',  ( 5.405949406249992428, -9.363379034771808662, -85.78125000204838102 ) ) ;
#28207 = CARTESIAN_POINT ( 'NONE',  ( 10.81189881249999729, 6.242252689847867408, -92.71875000204838102 ) ) ;
#28208 = CARTESIAN_POINT ( 'NONE',  ( -5.405949406250003975, -9.363379034771801557, -65.03125000204838102 ) ) ;
#28209 = CARTESIAN_POINT ( 'NONE',  ( -9.999999999999998224, 5.773502691896259087, -151.7500000040967620 ) ) ;
#28210 = CARTESIAN_POINT ( 'NONE',  ( 10.00000000000000000, 5.773502691896255534, -124.8750000000000000 ) ) ;
#28211 = EDGE_CURVE ( 'NONE', #32901, #35303, #18033, .T. ) ;
#28212 = AXIS2_PLACEMENT_3D ( 'NONE', #1990, #31344, #38653 ) ;
#28213 = CARTESIAN_POINT ( 'NONE',  ( -10.81189881249999729, -6.242252689847864744, -152.1562500020484094 ) ) ;
#28214 = CARTESIAN_POINT ( 'NONE',  ( -10.81189881249999729, 1.324075727343319199E-15, -165.7812500020484094 ) ) ;
#28215 = CARTESIAN_POINT ( 'NONE',  ( 9.999999999999998224, 0.000000000000000000, -200.0000000000000000 ) ) ;
#28216 = CARTESIAN_POINT ( 'NONE',  ( 9.999999999999998224, 0.000000000000000000, -159.8750000040967905 ) ) ;
#28217 = CARTESIAN_POINT ( 'NONE',  ( 7.644554776091147741E-16, 12.48450537969573659, -101.4687500020483668 ) ) ;
#28218 = VERTEX_POINT ( 'NONE', #28397 ) ;
#28219 = CARTESIAN_POINT ( 'NONE',  ( 7.070501591499377789E-16, 11.54700538379251284, -67.62500000000001421 ) ) ;
#28220 = CARTESIAN_POINT ( 'NONE',  ( 10.81189881249999729, 0.000000000000000000, -196.3437500020484094 ) ) ;
#28221 = CARTESIAN_POINT ( 'NONE',  ( -9.999999999999998224, 1.224646799147353059E-15, -84.12500000409677625 ) ) ;
#28222 = DIRECTION ( 'NONE',  ( -1.000000000000000000, 0.000000000000000000, 0.000000000000000000 ) ) ;
#28223 = CARTESIAN_POINT ( 'NONE',  ( 9.999999999999998224, 0.000000000000000000, -120.8750000040967905 ) ) ;
#28224 = CARTESIAN_POINT ( 'NONE',  ( 10.81189881249999729, 0.000000000000000000, -93.03125000204838102 ) ) ;
#28225 = CARTESIAN_POINT ( 'NONE',  ( 10.81189881249999729, 6.242252689847867408, -77.90625000204836681 ) ) ;
#28226 = CARTESIAN_POINT ( 'NONE',  ( -9.999999999999998224, 1.224646799147353059E-15, -64.62500000409676204 ) ) ;
#28227 = CARTESIAN_POINT ( 'NONE',  ( 9.999999999999998224, 0.000000000000000000, -77.37500000409677625 ) ) ;
#28228 = CARTESIAN_POINT ( 'NONE',  ( 10.81189881249999551, -6.242252689847874514, -23.96875000204837391 ) ) ;
#28229 = CARTESIAN_POINT ( 'NONE',  ( 4.999999999999992006, -8.660254037844389075, -0.7499999999999729106 ) ) ;
#28230 = CARTESIAN_POINT ( 'NONE',  ( 5.405949406249992428, -9.363379034771808662, -21.28125000204836326 ) ) ;
#28231 = CARTESIAN_POINT ( 'NONE',  ( -2.293366432827344421E-15, -12.48450537969573659, -1.718750002048356373 ) ) ;
#28232 = CARTESIAN_POINT ( 'NONE',  ( 4.999999999999992006, -8.660254037844389075, -176.6250000040968189 ) ) ;
#28233 = CARTESIAN_POINT ( 'NONE',  ( -10.81189881249999729, 6.242252689847871849, -146.2187500020483810 ) ) ;
#28234 = CARTESIAN_POINT ( 'NONE',  ( -9.999999999999479527, -5.773502691896549521, -108.0000000040967478 ) ) ;
#28235 = CARTESIAN_POINT ( 'NONE',  ( 5.000000000000000000, 8.660254037844385522, -133.7499999999999716 ) ) ;
#28236 = CARTESIAN_POINT ( 'NONE',  ( -2.121150477449813534E-15, -11.54700538379251284, -183.8750000000000284 ) ) ;
#28237 = CARTESIAN_POINT ( 'NONE',  ( 0.000000000000000000, 0.000000000000000000, -200.0000000000000000 ) ) ;
#28239 = ORIENTED_EDGE ( 'NONE', *, *, #34162, .F. ) ;
#28238 = CARTESIAN_POINT ( 'NONE',  ( -10.81189881249999729, 1.324075727343319199E-15, -105.7812500020483810 ) ) ;
#28240 = CARTESIAN_POINT ( 'NONE',  ( 9.999999999999998224, 0.000000000000000000, -138.8750000040968189 ) ) ;
#28241 = VERTEX_POINT ( 'NONE', #21689 ) ;
#28242 = EDGE_LOOP ( 'NONE', ( #11596, #39839 ) ) ;
#28243 = VECTOR ( 'NONE', #14958, 1000.000000000000114 ) ;
#28244 = CARTESIAN_POINT ( 'NONE',  ( -5.405949406250003975, -9.363379034771801557, -35.03125000204837391 ) ) ;
#28245 = SECURITY_CLASSIFICATION_LEVEL ( 'unclassified' ) ;
#28246 = CARTESIAN_POINT ( 'NONE',  ( 7.644554776091147741E-16, 12.48450537969573659, -83.46875000204838102 ) ) ;
#28247 = CARTESIAN_POINT ( 'NONE',  ( -9.999999999999998224, 0.000000000000000000, -99.99999999999998579 ) ) ;
#28248 = CARTESIAN_POINT ( 'NONE',  ( 10.19523493519047719, 1.536126885025608235, -100.0000000000000142 ) ) ;
#28249 = DIRECTION ( 'NONE',  ( -0.000000000000000000, -0.000000000000000000, 1.000000000000000000 ) ) ;
#28250 = CARTESIAN_POINT ( 'NONE',  ( -10.81189881249999729, 6.242252689847871849, -162.9062500020484094 ) ) ;
#28251 = CARTESIAN_POINT ( 'NONE',  ( -9.999999999999982236, -5.773502691896262640, -199.1250000000000284 ) ) ;
#28252 = CARTESIAN_POINT ( 'NONE',  ( -5.405949406250003975, -9.363379034771801557, -117.3437500020483810 ) ) ;
#28253 =( BOUNDED_CURVE ( )  B_SPLINE_CURVE ( 2, ( #33757, #17747, #37183, #7630, #34613, #33971, #7416 ),
 .UNSPECIFIED., .F., .F. ) 
 B_SPLINE_CURVE_WITH_KNOTS ( ( 3, 2, 2, 3 ),
 ( 0.3432835820895522860, 0.3445273631840797268, 0.3457711442786070566, 0.3470149253731344974 ),
 .UNSPECIFIED. ) 
 CURVE ( )  GEOMETRIC_REPRESENTATION_ITEM ( )  RATIONAL_B_SPLINE_CURVE ( ( 0.9999999999999940048, 0.8660254037844447028, 1.000000000000000000, 0.8660254037844387076, 1.000000000000000000, 0.8660254037844207220, 1.000000000000017986 ) ) 
 REPRESENTATION_ITEM ( '' )  );
#28254 = CARTESIAN_POINT ( 'NONE',  ( -10.81189881249999729, 1.324075727343319199E-15, -87.59375000204836681 ) ) ;
#28255 = CARTESIAN_POINT ( 'NONE',  ( 5.405949406249992428, -9.363379034771808662, -3.281250002048374803 ) ) ;
#28256 = CARTESIAN_POINT ( 'NONE',  ( 10.81189881249999729, 0.000000000000000000, -190.3437500020484094 ) ) ;
#28257 = CARTESIAN_POINT ( 'NONE',  ( 7.644554776091147741E-16, 12.48450537969573659, -91.15625000204838102 ) ) ;
#28258 = CARTESIAN_POINT ( 'NONE',  ( 5.000000000000000000, 8.660254037844385522, -174.6250000040968189 ) ) ;
#28259 = CARTESIAN_POINT ( 'NONE',  ( 10.81189881249999729, 0.000000000000000000, -166.5312500020484094 ) ) ;
#28260 = CARTESIAN_POINT ( 'NONE',  ( 4.999999999999992006, -8.660254037844389075, -1.125000004096765593 ) ) ;
#28261 = CARTESIAN_POINT ( 'NONE',  ( -10.81189881249999729, 6.242252689847871849, -177.9062500020484094 ) ) ;
#28262 = CARTESIAN_POINT ( 'NONE',  ( -10.81189881249999907, -6.242252689847864744, -186.6562500020484094 ) ) ;
#28263 = CARTESIAN_POINT ( 'NONE',  ( 10.81189881249999551, -6.242252689847874514, -47.96875000204836681 ) ) ;
#28264 = AXIS2_PLACEMENT_3D ( 'NONE', #31855, #38307, #25580 ) ;
#28265 = CARTESIAN_POINT ( 'NONE',  ( -10.00000000000000000, -5.773502691896251982, -162.0000000040967620 ) ) ;
#28266 = CARTESIAN_POINT ( 'NONE',  ( 5.405949406249992428, -9.363379034771808662, -3.281250002048374803 ) ) ;
#28267 = CARTESIAN_POINT ( 'NONE',  ( -10.81189881249999729, 1.324075727343319199E-15, -15.59375000204835082 ) ) ;
#28268 = CARTESIAN_POINT ( 'NONE',  ( -5.000000000000003553, -8.660254037844383745, -158.8750000040967905 ) ) ;
#28269 = CARTESIAN_POINT ( 'NONE',  ( -10.81189881249999907, -6.242252689847864744, -120.4687500020483810 ) ) ;
#28270 = ADVANCED_FACE ( 'NONE', ( #8958 ), #22120, .T. ) ;
#28271 = CARTESIAN_POINT ( 'NONE',  ( -9.999999999999998224, 1.224646799147353059E-15, -92.74999999999998579 ) ) ;
#28272 = CARTESIAN_POINT ( 'NONE',  ( -5.405949406250003975, -9.363379034771801557, -17.03125000204835970 ) ) ;
#28273 = CARTESIAN_POINT ( 'NONE',  ( -9.999999999999998224, 5.773502691896259087, -106.7500000040967620 ) ) ;
#28274 = CARTESIAN_POINT ( 'NONE',  ( -9.999999999999998224, 1.224646799147353059E-15, -82.24999999999998579 ) ) ;
#28275 = CARTESIAN_POINT ( 'NONE',  ( 5.000000000000000000, 8.660254037844385522, -51.24999999999996447 ) ) ;
#28276 = CARTESIAN_POINT ( 'NONE',  ( 5.405949406249999534, 9.363379034771803333, -118.2812500020483952 ) ) ;
#28277 = CARTESIAN_POINT ( 'NONE',  ( -5.405949406250003975, -9.363379034771801557, -102.5312500020483952 ) ) ;
#28278 = ORIENTED_EDGE ( 'NONE', *, *, #20419, .T. ) ;
#28279 = CARTESIAN_POINT ( 'NONE',  ( 9.999999999999998224, 0.000000000000000000, -93.87500000409677625 ) ) ;
#28280 = CARTESIAN_POINT ( 'NONE',  ( 10.81189881249999551, -6.242252689847874514, -159.1562500020484094 ) ) ;
#28281 = CARTESIAN_POINT ( 'NONE',  ( 5.405949406249992428, -9.363379034771808662, -51.09375000204835260 ) ) ;
#28282 = ORIENTED_EDGE ( 'NONE', *, *, #18180, .T. ) ;
#28283 = CARTESIAN_POINT ( 'NONE',  ( -9.999999999999998224, 5.773502691896259087, -23.87499999999998579 ) ) ;
#28284 = CARTESIAN_POINT ( 'NONE',  ( -2.293366432827344421E-15, -12.48450537969573659, -27.40625000204838102 ) ) ;
#28285 = CARTESIAN_POINT ( 'NONE',  ( 9.999999999999998224, 0.000000000000000000, -164.0000000000000000 ) ) ;
#28286 = CARTESIAN_POINT ( 'NONE',  ( 5.000000000000000000, 8.660254037844385522, -21.62500000409675494 ) ) ;
#28287 = DIRECTION ( 'NONE',  ( 0.000000000000000000, 0.000000000000000000, 1.000000000000000000 ) ) ;
#28288 = CARTESIAN_POINT ( 'NONE',  ( 5.405949406249992428, -9.363379034771808662, -135.2812500020483810 ) ) ;
#28289 = CARTESIAN_POINT ( 'NONE',  ( -10.00000000000102496, 5.773502691895664007, -75.25000000409673362 ) ) ;
#28290 = CARTESIAN_POINT ( 'NONE',  ( 0.000000000000000000, 20.00000000000000000, -220.0000000000000000 ) ) ;
#28291 = ORIENTED_EDGE ( 'NONE', *, *, #39523, .F. ) ;
#28292 = CARTESIAN_POINT ( 'NONE',  ( 7.644554776091147741E-16, 12.48450537969573659, -58.15625000204838102 ) ) ;
#28293 = PERSON_AND_ORGANIZATION ( #11915, #17965 ) ;
#28294 =( GEOMETRIC_REPRESENTATION_CONTEXT ( 3 ) GLOBAL_UNCERTAINTY_ASSIGNED_CONTEXT ( ( #10429 ) ) GLOBAL_UNIT_ASSIGNED_CONTEXT ( ( #23882, #14121, #21048 ) ) REPRESENTATION_CONTEXT ( 'NONE', 'WORKASPACE' ) );
#28296 = ORIENTED_EDGE ( 'NONE', *, *, #37809, .T. ) ;
#28295 = ORIENTED_EDGE ( 'NONE', *, *, #38630, .F. ) ;
#28297 = DIRECTION ( 'NONE',  ( -0.000000000000000000, -0.000000000000000000, 1.000000000000000000 ) ) ;
#28298 = DIRECTION ( 'NONE',  ( 1.000000000000000000, 0.000000000000000000, 0.000000000000000000 ) ) ;
#28299 =( BOUNDED_CURVE ( )  B_SPLINE_CURVE ( 2, ( #14647, #11411, #14857, #25250, #1513, #38395, #24605 ),
 .UNSPECIFIED., .F., .F. ) 
 B_SPLINE_CURVE_WITH_KNOTS ( ( 3, 2, 2, 3 ),
 ( 0.2276119402985075368, 0.2288557213930349221, 0.2300995024875622796, 0.2313432835820896372 ),
 .UNSPECIFIED. ) 
 CURVE ( )  GEOMETRIC_REPRESENTATION_ITEM ( )  RATIONAL_B_SPLINE_CURVE ( ( 0.9999999999999910072, 0.8660254037844477004, 1.000000000000000000, 0.8660254037844387076, 1.000000000000000000, 0.8660254037844297148, 1.000000000000008882 ) ) 
 REPRESENTATION_ITEM ( '' )  );
#28300 = CARTESIAN_POINT ( 'NONE',  ( -2.293366432827344421E-15, -12.48450537969573659, -160.7187500020483810 ) ) ;
#28301 = CARTESIAN_POINT ( 'NONE',  ( 10.81189881249999907, 6.242252689847868297, -185.9062500020484094 ) ) ;
#28302 = CARTESIAN_POINT ( 'NONE',  ( -5.405949406250003975, -9.363379034771801557, -6.343750002048370362 ) ) ;
#28303 = CARTESIAN_POINT ( 'NONE',  ( 10.81189881249999729, 0.000000000000000000, -143.8437500020483810 ) ) ;
#28304 = CARTESIAN_POINT ( 'NONE',  ( 5.405949406249999534, 9.363379034771803333, -95.78125000204838102 ) ) ;
#28305 = CARTESIAN_POINT ( 'NONE',  ( 5.405949406249992428, -9.363379034771808662, -108.0937500020483810 ) ) ;
#28306 = CARTESIAN_POINT ( 'NONE',  ( -5.000000000000003553, -8.660254037844383745, -149.8750000040967905 ) ) ;
#28307 = CARTESIAN_POINT ( 'NONE',  ( 10.81189881249999729, 0.000000000000000000, -120.0312500020483952 ) ) ;
#28308 = CARTESIAN_POINT ( 'NONE',  ( -10.81189881249999907, -6.242252689847864744, -0.4687500020483501006 ) ) ;
#28309 = CARTESIAN_POINT ( 'NONE',  ( 7.644554776091147741E-16, 12.48450537969573659, -122.4687500020483952 ) ) ;
#28310 = CARTESIAN_POINT ( 'NONE',  ( 10.81189881249999551, -6.242252689847874514, -192.1562500020484094 ) ) ;
#28311 = DIRECTION ( 'NONE',  ( -0.000000000000000000, -0.000000000000000000, 1.000000000000000000 ) ) ;
#28312 = CARTESIAN_POINT ( 'NONE',  ( 7.070501591499377789E-16, 11.54700538379251284, -150.1250000000000000 ) ) ;
#28313 = CARTESIAN_POINT ( 'NONE',  ( 4.999999999999992006, -8.660254037844389075, -14.24999999999995737 ) ) ;
#28314 = CARTESIAN_POINT ( 'NONE',  ( -10.81189881249999729, 1.324075727343319199E-15, -80.09375000204838102 ) ) ;
#28315 = CARTESIAN_POINT ( 'NONE',  ( 5.405949406249992428, -9.363379034771808662, -55.59375000204835970 ) ) ;
#28316 = CARTESIAN_POINT ( 'NONE',  ( 5.000000000000000000, 8.660254037844385522, -186.6250000040967905 ) ) ;
#28317 = CARTESIAN_POINT ( 'NONE',  ( 10.81189881249999729, 0.000000000000000000, -22.53125000204836326 ) ) ;
#28318 = CARTESIAN_POINT ( 'NONE',  ( 10.81189881249999907, 6.242252689847868297, -41.71875000204835970 ) ) ;
#28319 = CARTESIAN_POINT ( 'NONE',  ( -9.999999999999998224, 1.224646799147353059E-15, -108.1250000040967763 ) ) ;
#28320 = CARTESIAN_POINT ( 'NONE',  ( -10.81189881249999907, -6.242252689847864744, -145.9687500020484094 ) ) ;
#28321 = ADVANCED_FACE ( 'NONE', ( #8747 ), #41537, .T. ) ;
#28322 = CARTESIAN_POINT ( 'NONE',  ( -4.999999999999996447, 8.660254037844387298, -123.0000000000000000 ) ) ;
#28323 = CARTESIAN_POINT ( 'NONE',  ( -10.00000000000102496, 5.773502691895664007, -41.87499999999994316 ) ) ;
#28324 = EDGE_CURVE ( 'NONE', #40457, #3711, #22122, .T. ) ;
#28325 = CARTESIAN_POINT ( 'NONE',  ( -2.121150477449813534E-15, -11.54700538379251284, -72.87499999999995737 ) ) ;
#28326 = CARTESIAN_POINT ( 'NONE',  ( 10.81189881249999729, 0.000000000000000000, -139.5312500020484094 ) ) ;
#28327 = CARTESIAN_POINT ( 'NONE',  ( -10.81189881249999729, -6.242252689847864744, -6.656250002048365033 ) ) ;
#28328 = EDGE_CURVE ( 'NONE', #17345, #35521, #5870, .T. ) ;
#28329 = ORIENTED_EDGE ( 'NONE', *, *, #13251, .F. ) ;
#28330 = CARTESIAN_POINT ( 'NONE',  ( 7.644554776091147741E-16, 12.48450537969573659, -103.1562500020483952 ) ) ;
#28331 = CARTESIAN_POINT ( 'NONE',  ( 10.00000000000000000, 5.773502691896255534, -113.2500000040967905 ) ) ;
#28332 = CARTESIAN_POINT ( 'NONE',  ( -5.000000000000003553, -8.660254037844383745, -140.5000000000000000 ) ) ;
#28333 = CARTESIAN_POINT ( 'NONE',  ( -10.81189881249999729, 1.324075727343319199E-15, -77.09375000204838102 ) ) ;
#28334 =( GEOMETRIC_REPRESENTATION_CONTEXT ( 3 ) GLOBAL_UNCERTAINTY_ASSIGNED_CONTEXT ( ( #39784 ) ) GLOBAL_UNIT_ASSIGNED_CONTEXT ( ( #40886, #38945, #5298 ) ) REPRESENTATION_CONTEXT ( 'NONE', 'WORKASPACE' ) );
#28335 = CARTESIAN_POINT ( 'NONE',  ( -9.999999999999998224, 5.773502691896259087, -25.75000000409677270 ) ) ;
#28336 = VECTOR ( 'NONE', #42324, 1000.000000000000000 ) ;
#28337 = CARTESIAN_POINT ( 'NONE',  ( -9.999999999999998224, 1.224646799147353059E-15, -74.74999999999998579 ) ) ;
#28338 = CC_DESIGN_PERSON_AND_ORGANIZATION_ASSIGNMENT ( #16101, #26063, ( #40065 ) ) ;
#28339 = CARTESIAN_POINT ( 'NONE',  ( 7.644554776091147741E-16, 12.48450537969573659, -43.15625000204837391 ) ) ;
#28340 = LINE ( 'NONE', #41478, #28336 ) ;
#28341 = CARTESIAN_POINT ( 'NONE',  ( -10.81189881249999729, 1.324075727343319199E-15, -141.7812500020483810 ) ) ;
#28342 = CARTESIAN_POINT ( 'NONE',  ( 5.405949406249992428, -9.363379034771808662, -130.5937500020483810 ) ) ;
#28343 = CARTESIAN_POINT ( 'NONE',  ( -2.121150477449813534E-15, -11.54700538379251284, -164.7500000040968189 ) ) ;
#28344 = EDGE_CURVE ( 'NONE', #32304, #19459, #33972, .T. ) ;
#28345 = CARTESIAN_POINT ( 'NONE',  ( -9.999999999999998224, 1.224646799147353059E-15, -190.2500000000000000 ) ) ;
#28346 = VERTEX_POINT ( 'NONE', #41018 ) ;
#28347 = EDGE_CURVE ( 'NONE', #9909, #5974, #7823, .T. ) ;
#28348 = ORIENTED_EDGE ( 'NONE', *, *, #15327, .T. ) ;
#28349 = ORIENTED_EDGE ( 'NONE', *, *, #1167, .T. ) ;
#28350 = AXIS2_PLACEMENT_3D ( 'NONE', #31626, #8525, #2059 ) ;
#28351 = DIRECTION ( 'NONE',  ( -0.000000000000000000, -0.000000000000000000, 1.000000000000000000 ) ) ;
#28352 = CARTESIAN_POINT ( 'NONE',  ( 10.81189881249999729, 0.000000000000000000, -179.8437500020483810 ) ) ;
#28353 = CARTESIAN_POINT ( 'NONE',  ( -10.81189881249999729, 6.242252689847871849, -30.71875000204834905 ) ) ;
#28354 = CARTESIAN_POINT ( 'NONE',  ( 9.999999999999998224, 0.000000000000000000, -129.8750000040967905 ) ) ;
#28355 = CARTESIAN_POINT ( 'NONE',  ( 10.81189881249999551, -6.242252689847874514, -160.4687500020484094 ) ) ;
#28356 = CARTESIAN_POINT ( 'NONE',  ( 10.81189881249999551, -6.242252689847874514, -155.9687500020484094 ) ) ;
#28357 = ADVANCED_FACE ( 'NONE', ( #23792, #11462, #20970 ), #24229, .F. ) ;
#28358 = CARTESIAN_POINT ( 'NONE',  ( -9.999999999999998224, 1.224646799147353059E-15, -163.2500000000000000 ) ) ;
#28359 = CARTESIAN_POINT ( 'NONE',  ( 10.81189881249999729, 0.000000000000000000, -136.3437500020484094 ) ) ;
#28360 = CARTESIAN_POINT ( 'NONE',  ( -10.81189881249999907, -6.242252689847864744, -143.1562500020484094 ) ) ;
#28361 = CARTESIAN_POINT ( 'NONE',  ( -2.293366432827344421E-15, -12.48450537969573659, -144.2187500020484094 ) ) ;
#28362 = CARTESIAN_POINT ( 'NONE',  ( 7.071067811865477282, -7.071067811865471064, -200.0000000000000000 ) ) ;
#28363 = CARTESIAN_POINT ( 'NONE',  ( 7.070501591499376803E-16, 11.54700538379251284, -183.1250000000000000 ) ) ;
#28364 = CARTESIAN_POINT ( 'NONE',  ( 5.000000000000000000, 8.660254037844385522, -168.2500000000000000 ) ) ;
#28365 = CARTESIAN_POINT ( 'NONE',  ( 10.81189881249999907, 6.242252689847868297, -79.21875000204838102 ) ) ;
#28366 = CARTESIAN_POINT ( 'NONE',  ( -6.089403866005159038, 8.962546680094892082, -99.99999999999998579 ) ) ;
#28367 = CARTESIAN_POINT ( 'NONE',  ( -5.405949406249996869, 9.363379034771805109, -61.03125000204837391 ) ) ;
#28368 = CARTESIAN_POINT ( 'NONE',  ( -9.469335213649141991, 4.843080047529867649, -100.0000000000000142 ) ) ;
#28369 = CARTESIAN_POINT ( 'NONE',  ( 10.81189881249999907, 6.242252689847868297, -167.7187500020483810 ) ) ;
#28370 = CARTESIAN_POINT ( 'NONE',  ( 10.81189881249999907, 6.242252689847868297, -113.9062500020483952 ) ) ;
#28371 = CARTESIAN_POINT ( 'NONE',  ( -5.405949406250003975, -9.363379034771801557, -144.5312500020483810 ) ) ;
#28372 = DIRECTION ( 'NONE',  ( 0.000000000000000000, 0.000000000000000000, 1.000000000000000000 ) ) ;
#28373 = CARTESIAN_POINT ( 'NONE',  ( -5.405949406250003975, -9.363379034771801557, -45.53125000204838102 ) ) ;
#28374 = CARTESIAN_POINT ( 'NONE',  ( 7.070501591499377789E-16, 11.54700538379251284, -122.0000000040967905 ) ) ;
#28375 = CARTESIAN_POINT ( 'NONE',  ( -5.000000000000003553, -8.660254037844383745, -103.0000000000000000 ) ) ;
#28376 = ORIENTED_EDGE ( 'NONE', *, *, #8538, .T. ) ;
#28377 = CARTESIAN_POINT ( 'NONE',  ( -5.405949406250003975, -9.363379034771801557, -126.5312500020483952 ) ) ;
#28378 = CARTESIAN_POINT ( 'NONE',  ( 10.00000000000000000, 5.773502691896255534, -140.2500000040967905 ) ) ;
#28379 = CARTESIAN_POINT ( 'NONE',  ( -9.999999999999998224, 1.224646799147353059E-15, -67.62500000409676204 ) ) ;
#28380 = MANIFOLD_SOLID_BREP ( 'Cavity2', #9445 ) ;
#28381 = CARTESIAN_POINT ( 'NONE',  ( 10.81189881249999729, 0.000000000000000000, -178.5312500020483810 ) ) ;
#28382 = ORIENTED_EDGE ( 'NONE', *, *, #9293, .T. ) ;
#28383 = CARTESIAN_POINT ( 'NONE',  ( 5.405949406249992428, -9.363379034771808662, -174.0937500020484094 ) ) ;
#28384 = CARTESIAN_POINT ( 'NONE',  ( 7.070501591499377789E-16, 11.54700538379251284, -47.00000000409677625 ) ) ;
#28385 = FACE_OUTER_BOUND ( 'NONE', #9586, .T. ) ;
#28386 = CARTESIAN_POINT ( 'NONE',  ( -9.999999999999996447, 5.773502691896259975, -171.2500000040967905 ) ) ;
#28387 = CARTESIAN_POINT ( 'NONE',  ( 5.405949406249999534, 9.363379034771803333, -65.78125000204838102 ) ) ;
#28388 = VECTOR ( 'NONE', #38993, 1000.000000000000000 ) ;
#28389 = CARTESIAN_POINT ( 'NONE',  ( -9.999999999999998224, 1.224646799147353059E-15, -48.12500000409677625 ) ) ;
#28390 = CARTESIAN_POINT ( 'NONE',  ( -4.999999999999996447, 8.660254037844387298, -147.3750000040967905 ) ) ;
#28391 = CARTESIAN_POINT ( 'NONE',  ( -5.405949406249996869, 9.363379034771805109, -170.5312500020484094 ) ) ;
#28392 = PRODUCT_DEFINITION_FORMATION_WITH_SPECIFIED_SOURCE ( 'ANY', '', #10757, .NOT_KNOWN. ) ;
#28393 = EDGE_CURVE ( 'NONE', #32933, #31697, #27234, .T. ) ;
#28394 = DIRECTION ( 'NONE',  ( 1.000000000000000000, 4.506943796211477094E-16, 0.000000000000000000 ) ) ;
#28395 = CARTESIAN_POINT ( 'NONE',  ( -5.000000000000003553, -8.660254037844383745, -34.37500000409676915 ) ) ;
#28396 = ORIENTED_EDGE ( 'NONE', *, *, #37394, .T. ) ;
#28397 = CARTESIAN_POINT ( 'NONE',  ( -9.999999999999998224, 1.224646799147353059E-15, -156.1250000040967905 ) ) ;
#28398 =( BOUNDED_CURVE ( )  B_SPLINE_CURVE ( 2, ( #32950, #10054, #369, #23449, #17156, #19980, #3380 ),
 .UNSPECIFIED., .F., .F. ) 
 B_SPLINE_CURVE_WITH_KNOTS ( ( 3, 2, 2, 3 ),
 ( 0.3171641791044778058, 0.3184079601990050801, 0.3196517412935324653, 0.3208955223880597396 ),
 .UNSPECIFIED. ) 
 CURVE ( )  GEOMETRIC_REPRESENTATION_ITEM ( )  RATIONAL_B_SPLINE_CURVE ( ( 0.9999999999999820144, 0.8660254037844566932, 1.000000000000000000, 0.8660254037844387076, 1.000000000000000000, 0.8660254037844327124, 1.000000000000005995 ) ) 
 REPRESENTATION_ITEM ( '' )  );
#28399 = DIRECTION ( 'NONE',  ( 1.000000000000000000, 0.000000000000000000, 0.000000000000000000 ) ) ;
#28400 = CARTESIAN_POINT ( 'NONE',  ( 9.999999999999932498, 5.773502691896291950, -195.7500000040968189 ) ) ;
#28401 = AXIS2_PLACEMENT_3D ( 'NONE', #35041, #15153, #5467 ) ;
#28403 = ORIENTED_EDGE ( 'NONE', *, *, #39183, .T. ) ;
#28402 = CARTESIAN_POINT ( 'NONE',  ( 5.405949406249999534, 9.363379034771803333, -77.78125000204838102 ) ) ;
#28405 = VERTEX_POINT ( 'NONE', #11249 ) ;
#28404 = CARTESIAN_POINT ( 'NONE',  ( -14.84614977916192302, -1.734723475976807094E-15, 52.14285714285716011 ) ) ;
#28406 = ORIENTED_EDGE ( 'NONE', *, *, #12569, .T. ) ;
#28407 = CARTESIAN_POINT ( 'NONE',  ( 10.81189881249999551, -6.242252689847874514, -25.46875000204837391 ) ) ;
#28408 = CARTESIAN_POINT ( 'NONE',  ( -5.000000000000003553, -8.660254037844383745, -53.49999999999996447 ) ) ;
#28409 = CARTESIAN_POINT ( 'NONE',  ( 10.81189881249999729, 0.000000000000000000, -6.031250002048377468 ) ) ;
#28411 = EDGE_LOOP ( 'NONE', ( #4552, #36818, #18642, #42539 ) ) ;
#28410 = CARTESIAN_POINT ( 'NONE',  ( 5.405949406249999534, 9.363379034771803333, -55.09375000204835970 ) ) ;
#28412 = CARTESIAN_POINT ( 'NONE',  ( 7.070501591499376803E-16, 11.54700538379251284, -28.62499999999997513 ) ) ;
#28413 = CARTESIAN_POINT ( 'NONE',  ( 4.999999999999992006, -8.660254037844389075, -35.24999999999997868 ) ) ;
#28414 = CARTESIAN_POINT ( 'NONE',  ( 10.81189881249999729, 0.000000000000000000, -194.8437500020484094 ) ) ;
#28415 = CARTESIAN_POINT ( 'NONE',  ( -10.81189881249999907, -6.242252689847864744, -180.4687500020484094 ) ) ;
#28416 = CARTESIAN_POINT ( 'NONE',  ( -2.293366432827344421E-15, -12.48450537969573659, -154.7187500020483810 ) ) ;
#28417 = AXIS2_PLACEMENT_3D ( 'NONE', #33183, #26691, #39844 ) ;
#28418 = CARTESIAN_POINT ( 'NONE',  ( -5.405949406250003975, -9.363379034771801557, -178.8437500020483810 ) ) ;
#28419 = CARTESIAN_POINT ( 'NONE',  ( 9.999999999999998224, 0.000000000000000000, -200.0000000000000000 ) ) ;
#28420 = CARTESIAN_POINT ( 'NONE',  ( 4.999999999999992006, -8.660254037844389075, -126.7499999999999716 ) ) ;
#28421 = CARTESIAN_POINT ( 'NONE',  ( -4.999999999999996447, 8.660254037844387298, -196.5000000000000000 ) ) ;
#28422 = CARTESIAN_POINT ( 'NONE',  ( -5.405949406250003975, -9.363379034771801557, -106.8437500020483810 ) ) ;
#28423 = CARTESIAN_POINT ( 'NONE',  ( -9.999999999999998224, 1.224646799147353059E-15, -184.2500000000000000 ) ) ;
#28424 = CARTESIAN_POINT ( 'NONE',  ( -10.81189881249999907, -6.242252689847864744, -84.65625000204836681 ) ) ;
#28425 = CARTESIAN_POINT ( 'NONE',  ( 7.644554776091147741E-16, 12.48450537969573659, -92.46875000204838102 ) ) ;
#28426 = CARTESIAN_POINT ( 'NONE',  ( 5.405949406249999534, 9.363379034771803333, -67.28125000204838102 ) ) ;
#28427 = CARTESIAN_POINT ( 'NONE',  ( -2.121150477449813534E-15, -11.54700538379251284, -149.7500000040968189 ) ) ;
#28428 = CARTESIAN_POINT ( 'NONE',  ( -2.121150477449813534E-15, -11.54700538379251284, -122.3750000000000142 ) ) ;
#28429 = ORIENTED_EDGE ( 'NONE', *, *, #23193, .T. ) ;
#28430 = CARTESIAN_POINT ( 'NONE',  ( 10.81189881249999729, 6.242252689847867408, -151.4062500020484094 ) ) ;
#28431 = CARTESIAN_POINT ( 'NONE',  ( -5.405949406249996869, 9.363379034771805109, -163.0312500020484094 ) ) ;
#28432 = AXIS2_PLACEMENT_3D ( 'NONE', #36631, #7077, #39026 ) ;
#28433 = CARTESIAN_POINT ( 'NONE',  ( 0.000000000000000000, 0.000000000000000000, -99.99999999999998579 ) ) ;
#28434 = CARTESIAN_POINT ( 'NONE',  ( -9.999999999999479527, -5.773502691896549521, -38.62499999999993605 ) ) ;
#28435 = CARTESIAN_POINT ( 'NONE',  ( -10.81189881249999729, 1.324075727343319199E-15, -99.59375000204838102 ) ) ;
#28436 = VERTEX_POINT ( 'NONE', #24447 ) ;
#28437 = CARTESIAN_POINT ( 'NONE',  ( -2.121150477449813534E-15, -11.54700538379251284, -66.87500000000000000 ) ) ;
#28438 = CARTESIAN_POINT ( 'NONE',  ( 5.405949406249992428, -9.363379034771808662, -193.5937500020484094 ) ) ;
#28439 = CARTESIAN_POINT ( 'NONE',  ( -10.00000000000000000, -5.773502691896251982, -84.00000000409677625 ) ) ;
#28440 = CARTESIAN_POINT ( 'NONE',  ( 1.680766644672218924, -10.37565344158061542, -180.0000000000000284 ) ) ;
#28441 = CARTESIAN_POINT ( 'NONE',  ( -9.999999999999998224, 1.224646799147353059E-15, -124.2500000000000000 ) ) ;
#28442 = CARTESIAN_POINT ( 'NONE',  ( -10.81189881249999907, -6.242252689847864744, -90.65625000204836681 ) ) ;
#28443 = CARTESIAN_POINT ( 'NONE',  ( -10.81189881249999729, -6.242252689847864744, -78.65625000204836681 ) ) ;
#28444 =( BOUNDED_CURVE ( )  B_SPLINE_CURVE ( 2, ( #4325, #17463, #14216, #34913, #7784, #34110, #41356 ),
 .UNSPECIFIED., .F., .F. ) 
 B_SPLINE_CURVE_WITH_KNOTS ( ( 3, 2, 2, 3 ),
 ( 0.9477611940298510396, 0.9490049751243784248, 0.9502487562189058101, 0.9514925373134331954 ),
 .UNSPECIFIED. ) 
 CURVE ( )  GEOMETRIC_REPRESENTATION_ITEM ( )  RATIONAL_B_SPLINE_CURVE ( ( 0.9999999999999641398, 0.8660254037844745678, 1.000000000000000000, 0.8660254037844387076, 1.000000000000000000, 0.8660254037844028474, 1.000000000000035971 ) ) 
 REPRESENTATION_ITEM ( '' )  );
#28445 = CARTESIAN_POINT ( 'NONE',  ( -10.00000000000000000, -5.773502691896251982, -69.00000000409677625 ) ) ;
#28446 = DIRECTION ( 'NONE',  ( -0.000000000000000000, -0.000000000000000000, 1.000000000000000000 ) ) ;
#28447 = CARTESIAN_POINT ( 'NONE',  ( -5.405949406249996869, 9.363379034771805109, -29.34375000204836326 ) ) ;
#28448 = ORIENTED_EDGE ( 'NONE', *, *, #11167, .F. ) ;
#28449 = CARTESIAN_POINT ( 'NONE',  ( -10.81189881249999729, 1.324075727343319199E-15, -189.7812500020484094 ) ) ;
#28450 = EDGE_CURVE ( 'NONE', #21857, #22494, #9136, .T. ) ;
#28451 = CARTESIAN_POINT ( 'NONE',  ( 10.81189881249999551, -6.242252689847874514, -22.65625000204837747 ) ) ;
#28452 = CARTESIAN_POINT ( 'NONE',  ( 5.405949406249992428, -9.363379034771808662, -7.593750002048343717 ) ) ;
#28453 = FACE_OUTER_BOUND ( 'NONE', #28708, .T. ) ;
#28454 = CARTESIAN_POINT ( 'NONE',  ( -5.405949406249996869, 9.363379034771805109, -143.3437500020483810 ) ) ;
#28455 = CARTESIAN_POINT ( 'NONE',  ( 4.999999999999992006, -8.660254037844389075, -37.12500000409676915 ) ) ;
#28456 = LINE ( 'NONE', #7046, #32130 ) ;
#28457 =( BOUNDED_CURVE ( )  B_SPLINE_CURVE ( 2, ( #9277, #35203, #35625, #31545, #6052, #19202, #14891 ),
 .UNSPECIFIED., .F., .F. ) 
 B_SPLINE_CURVE_WITH_KNOTS ( ( 3, 2, 2, 3 ),
 ( 0.2686567164179105571, 0.2699004975124379424, 0.2711442786069652722, 0.2723880597014926574 ),
 .UNSPECIFIED. ) 
 CURVE ( )  GEOMETRIC_REPRESENTATION_ITEM ( )  RATIONAL_B_SPLINE_CURVE ( ( 0.9999999999999880096, 0.8660254037844506980, 1.000000000000000000, 0.8660254037844387076, 1.000000000000000000, 0.8660254037844267172, 1.000000000000011990 ) ) 
 REPRESENTATION_ITEM ( '' )  );
#28458 = CARTESIAN_POINT ( 'NONE',  ( -9.999999999999998224, 1.224646799147353059E-15, -173.7500000000000284 ) ) ;
#28459 = CARTESIAN_POINT ( 'NONE',  ( -9.999999999999998224, 1.224646799147353059E-15, -175.6250000040968189 ) ) ;
#28461 = EDGE_LOOP ( 'NONE', ( #12188, #7150, #7525, #41212 ) ) ;
#28460 = CARTESIAN_POINT ( 'NONE',  ( 5.405949406249999534, 9.363379034771803333, -103.2812500020483952 ) ) ;
#28462 = CARTESIAN_POINT ( 'NONE',  ( -9.999999999999872102, -5.773502691896326589, -164.6249999999999716 ) ) ;
#28463 = ORIENTED_EDGE ( 'NONE', *, *, #11687, .F. ) ;
#28464 = ORIENTED_EDGE ( 'NONE', *, *, #42273, .F. ) ;
#28465 = EDGE_CURVE ( 'NONE', #38628, #18833, #17934, .T. ) ;
#28466 = CARTESIAN_POINT ( 'NONE',  ( -2.293366432827344421E-15, -12.48450537969573659, -31.90625000204835970 ) ) ;
#28467 = PERSON_AND_ORGANIZATION_ROLE ( 'classification_officer' ) ;
#28468 = VECTOR ( 'NONE', #1622, 1000.000000000000000 ) ;
#28469 = CARTESIAN_POINT ( 'NONE',  ( -10.81189881249999729, 6.242252689847871849, -87.71875000204838102 ) ) ;
#28470 = CARTESIAN_POINT ( 'NONE',  ( -99.99999999999994316, -40.00000000000000711, -160.0000000000000000 ) ) ;
#28471 = CARTESIAN_POINT ( 'NONE',  ( 9.617269083703753552, -3.087026286776204831, -100.0000000000000142 ) ) ;
#28472 = FACE_OUTER_BOUND ( 'NONE', #15575, .T. ) ;
#28473 = CARTESIAN_POINT ( 'NONE',  ( -5.405949406250003975, -9.363379034771801557, -167.0312500020484094 ) ) ;
#28474 = CARTESIAN_POINT ( 'NONE',  ( 9.999999999999996447, -5.773502691896262640, -11.50000000409676559 ) ) ;
#28475 = CARTESIAN_POINT ( 'NONE',  ( 4.999999999999992006, -8.660254037844389075, -198.7500000000000000 ) ) ;
#28476 = CARTESIAN_POINT ( 'NONE',  ( -5.405949406249996869, 9.363379034771805109, -113.3437500020483810 ) ) ;
#28477 = CARTESIAN_POINT ( 'NONE',  ( 7.644554776091147741E-16, 12.48450537969573659, -86.46875000204838102 ) ) ;
#28478 = CARTESIAN_POINT ( 'NONE',  ( -5.405949406249996869, 9.363379034771805109, -197.3437500020484094 ) ) ;
#28479 = CARTESIAN_POINT ( 'NONE',  ( 10.81189881249999551, -6.242252689847874514, -93.15625000204838102 ) ) ;
#28480 = CARTESIAN_POINT ( 'NONE',  ( -9.999999999999998224, 5.773502691896259087, -169.7500000040967905 ) ) ;
#28481 = CARTESIAN_POINT ( 'NONE',  ( 10.81189881249999551, -6.242252689847874514, -169.6562500020484094 ) ) ;
#28482 = CARTESIAN_POINT ( 'NONE',  ( 10.81189881249999729, 6.242252689847867408, -175.4062500020484094 ) ) ;
#28483 = CARTESIAN_POINT ( 'NONE',  ( 7.644554776091147741E-16, 12.48450537969573659, -191.6562500020484094 ) ) ;
#28484 = CARTESIAN_POINT ( 'NONE',  ( -5.405949406250003975, -9.363379034771801557, -46.84375000204838102 ) ) ;
#28485 = CARTESIAN_POINT ( 'NONE',  ( -5.000000000000003553, -8.660254037844383745, -160.3750000040967905 ) ) ;
#28486 = CARTESIAN_POINT ( 'NONE',  ( -2.293366432827344421E-15, -12.48450537969573659, -1.906250002048373027 ) ) ;
#28487 = CARTESIAN_POINT ( 'NONE',  ( -5.405949406250003975, -9.363379034771801557, -16.84375000204835260 ) ) ;
#28488 = CARTESIAN_POINT ( 'NONE',  ( 9.999999999999998224, 0.000000000000000000, -54.49999999999996447 ) ) ;
#28489 = CARTESIAN_POINT ( 'NONE',  ( -5.405949406249996869, 9.363379034771805109, -120.8437500020483952 ) ) ;
#28490 = CARTESIAN_POINT ( 'NONE',  ( 9.999999999999996447, -5.773502691896262640, -87.62499999999998579 ) ) ;
#28491 = CARTESIAN_POINT ( 'NONE',  ( -5.405949406249996869, 9.363379034771805109, -20.53125000204836326 ) ) ;
#28492 = CARTESIAN_POINT ( 'NONE',  ( -9.999999999999998224, 1.224646799147353059E-15, -106.6250000040967763 ) ) ;
#28493 = CYLINDRICAL_SURFACE ( 'NONE', #23098, 9.999999999999998224 ) ;
#28494 = CARTESIAN_POINT ( 'NONE',  ( -5.000000000000003553, -8.660254037844383745, -54.99999999999996447 ) ) ;
#28495 = CARTESIAN_POINT ( 'NONE',  ( -5.405949406250003975, -9.363379034771801557, -114.5312500020483952 ) ) ;
#28496 = CARTESIAN_POINT ( 'NONE',  ( -2.293366432827344421E-15, -12.48450537969573659, -97.90625000204839523 ) ) ;
#28497 = ORIENTED_EDGE ( 'NONE', *, *, #30302, .T. ) ;
#28498 = ADVANCED_FACE ( 'NONE', ( #11035 ), #10819, .F. ) ;
#28499 = CARTESIAN_POINT ( 'NONE',  ( -9.999999999999998224, 1.224646799147353059E-15, -94.62500000409677625 ) ) ;
#28500 = CARTESIAN_POINT ( 'NONE',  ( 9.999999999999998224, 0.000000000000000000, -100.9999999999999858 ) ) ;
#28501 = CARTESIAN_POINT ( 'NONE',  ( 10.81189881249999729, 0.000000000000000000, -154.5312500020484094 ) ) ;
#28502 = CARTESIAN_POINT ( 'NONE',  ( -10.81189881249999729, 6.242252689847871849, -51.71875000204836681 ) ) ;
#28503 = VERTEX_POINT ( 'NONE', #8036 ) ;
#28504 = CARTESIAN_POINT ( 'NONE',  ( -5.000000000000003553, -8.660254037844383745, -20.49999999999996447 ) ) ;
#28505 = CARTESIAN_POINT ( 'NONE',  ( 10.81189881249999729, 6.242252689847867408, -25.40625000204838813 ) ) ;
#28506 = CARTESIAN_POINT ( 'NONE',  ( -5.000000000000003553, -8.660254037844383745, -152.5000000000000000 ) ) ;
#28507 = CARTESIAN_POINT ( 'NONE',  ( 9.999999999999996447, -5.773502691896262640, -22.00000000409677270 ) ) ;
#28508 = CARTESIAN_POINT ( 'NONE',  ( -9.999999999999998224, 5.773502691896259087, -196.3750000000000568 ) ) ;
#28509 = CARTESIAN_POINT ( 'NONE',  ( -10.81189881249999729, 1.324075727343319199E-15, -128.2812500020483810 ) ) ;
#28510 = CARTESIAN_POINT ( 'NONE',  ( 9.999999999999998224, 0.000000000000000000, -65.37500000409676204 ) ) ;
#28511 = CARTESIAN_POINT ( 'NONE',  ( 10.00000000000051159, -5.773502691895965988, -44.50000000409674783 ) ) ;
#28512 = ORIENTED_EDGE ( 'NONE', *, *, #8183, .F. ) ;
#28513 = CARTESIAN_POINT ( 'NONE',  ( 5.405949406249999534, 9.363379034771803333, -55.28125000204836681 ) ) ;
#28514 = CALENDAR_DATE ( 2026, 28, 9 ) ;
#28515 = CARTESIAN_POINT ( 'NONE',  ( 5.405949406249999534, 9.363379034771803333, -115.0937500020483810 ) ) ;
#28516 = EDGE_CURVE ( 'NONE', #9539, #27414, #69, .T. ) ;
#28518 = VERTEX_POINT ( 'NONE', #14038 ) ;
#28517 = VERTEX_POINT ( 'NONE', #1566 ) ;
#28519 =( BOUNDED_CURVE ( )  B_SPLINE_CURVE ( 2, ( #4950, #31292, #14850, #28047, #41173, #24820, #8410 ),
 .UNSPECIFIED., .F., .F. ) 
 B_SPLINE_CURVE_WITH_KNOTS ( ( 3, 2, 2, 3 ),
 ( 0.4776119402985076756, 0.4788557213930350054, 0.4800995024875623352, 0.4813432835820896649 ),
 .UNSPECIFIED. ) 
 CURVE ( )  GEOMETRIC_REPRESENTATION_ITEM ( )  RATIONAL_B_SPLINE_CURVE ( ( 0.9999999999999761302, 0.8660254037844625774, 1.000000000000000000, 0.8660254037844387076, 1.000000000000000000, 0.8660254037844267172, 1.000000000000011990 ) ) 
 REPRESENTATION_ITEM ( '' )  );
#28520 = LINE ( 'NONE', #35201, #3901 ) ;
#28521 = CARTESIAN_POINT ( 'NONE',  ( 9.999999999999998224, 0.000000000000000000, -183.5000000000000000 ) ) ;
#28522 = CARTESIAN_POINT ( 'NONE',  ( 10.81189881249999551, -6.242252689847874514, -155.9687500020484094 ) ) ;
#28523 = CARTESIAN_POINT ( 'NONE',  ( 10.81189881249999551, -6.242252689847874514, -184.6562500020484094 ) ) ;
#28524 = CARTESIAN_POINT ( 'NONE',  ( -2.293366432827344421E-15, -12.48450537969573659, -7.718750002048352599 ) ) ;
#28525 = CARTESIAN_POINT ( 'NONE',  ( -2.293366432827344421E-15, -12.48450537969573659, -141.2187500020483810 ) ) ;
#28526 = CARTESIAN_POINT ( 'NONE',  ( 7.644554776091147741E-16, 12.48450537969573659, -113.4687500020483952 ) ) ;
#28527 = CARTESIAN_POINT ( 'NONE',  ( -5.000000000000003553, -8.660254037844383745, -161.5000000000000000 ) ) ;
#28528 = CARTESIAN_POINT ( 'NONE',  ( -10.81189881249999729, 1.324075727343319199E-15, -114.7812500020483952 ) ) ;
#28529 = CARTESIAN_POINT ( 'NONE',  ( 10.81189881249999551, -6.242252689847874514, -4.468750002048369474 ) ) ;
#28530 = CARTESIAN_POINT ( 'NONE',  ( 10.81189881249999729, 0.000000000000000000, -121.3437500020483952 ) ) ;
#28531 = CARTESIAN_POINT ( 'NONE',  ( -10.81189881249999729, -6.242252689847864744, -197.1562500020484379 ) ) ;
#28532 = DIRECTION ( 'NONE',  ( 0.000000000000000000, 1.000000000000000000, 0.000000000000000000 ) ) ;
#28533 = CARTESIAN_POINT ( 'NONE',  ( -9.999999999999998224, 1.224646799147353059E-15, -151.2500000000000000 ) ) ;
#28534 = CARTESIAN_POINT ( 'NONE',  ( 5.000000000000000000, 8.660254037844385522, -15.24999999999995737 ) ) ;
#28535 = CARTESIAN_POINT ( 'NONE',  ( 7.644554776091147741E-16, 12.48450537969573659, -69.96875000204838102 ) ) ;
#28536 = CARTESIAN_POINT ( 'NONE',  ( 10.81189881249999551, -6.242252689847874514, -56.96875000204838102 ) ) ;
#28537 = CARTESIAN_POINT ( 'NONE',  ( 4.999999999999992006, -8.660254037844389075, -188.6250000040967905 ) ) ;
#28538 = CARTESIAN_POINT ( 'NONE',  ( 10.81189881249999907, 6.242252689847868297, -29.90625000204836326 ) ) ;
#28539 = CARTESIAN_POINT ( 'NONE',  ( 10.81189881249999729, 0.000000000000000000, -37.34375000204836681 ) ) ;
#28540 = CARTESIAN_POINT ( 'NONE',  ( 9.999999999999998224, 0.000000000000000000, -95.37500000409677625 ) ) ;
#28541 = CARTESIAN_POINT ( 'NONE',  ( 10.81189881249999551, -6.242252689847874514, -142.4687500020483810 ) ) ;
#28542 = CARTESIAN_POINT ( 'NONE',  ( 9.999999999999998224, 0.000000000000000000, -109.9999999999999858 ) ) ;
#28543 = CARTESIAN_POINT ( 'NONE',  ( -9.999999999999998224, 1.224646799147353059E-15, -145.2500000000000000 ) ) ;
#28544 = CARTESIAN_POINT ( 'NONE',  ( 9.999999999999998224, 0.000000000000000000, -78.49999999999998579 ) ) ;
#28545 = CARTESIAN_POINT ( 'NONE',  ( -10.81189881249999907, -6.242252689847864744, -137.1562500020483810 ) ) ;
#28546 = CARTESIAN_POINT ( 'NONE',  ( 5.405949406249999534, 9.363379034771803333, -11.78125000204835438 ) ) ;
#28547 = VERTEX_POINT ( 'NONE', #10605 ) ;
#28548 = CARTESIAN_POINT ( 'NONE',  ( 7.070501591499376803E-16, 11.54700538379251284, -120.5000000040967905 ) ) ;
#28549 = CARTESIAN_POINT ( 'NONE',  ( 5.000000000000000000, 8.660254037844385522, -117.6250000040967905 ) ) ;
#28550 = CARTESIAN_POINT ( 'NONE',  ( 9.999999999999998224, 0.000000000000000000, -57.49999999999996447 ) ) ;
#28551 = CARTESIAN_POINT ( 'NONE',  ( -10.81189881249999729, 6.242252689847871849, -75.71875000204836681 ) ) ;
#28552 = CARTESIAN_POINT ( 'NONE',  ( 5.000000000000000000, 8.660254037844385522, -39.24999999999997868 ) ) ;
#28553 = CARTESIAN_POINT ( 'NONE',  ( 9.999999999999996447, -5.773502691896262640, -26.50000000409677270 ) ) ;
#28554 = CARTESIAN_POINT ( 'NONE',  ( 9.999999999999998224, 0.000000000000000000, -131.3750000040967905 ) ) ;
#28555 = CARTESIAN_POINT ( 'NONE',  ( 10.81189881249999907, 6.242252689847868297, -43.40625000204836681 ) ) ;
#28556 = DIRECTION ( 'NONE',  ( 0.000000000000000000, 0.000000000000000000, 1.000000000000000000 ) ) ;
#28557 = CARTESIAN_POINT ( 'NONE',  ( -10.81189881249999729, 6.242252689847871849, -141.9062500020484094 ) ) ;
#28558 = CARTESIAN_POINT ( 'NONE',  ( 10.81189881249999907, 6.242252689847868297, -151.4062500020484094 ) ) ;
#28559 = CARTESIAN_POINT ( 'NONE',  ( 5.000000000000000000, 8.660254037844385522, -60.24999999999997158 ) ) ;
#28560 = CARTESIAN_POINT ( 'NONE',  ( 4.999999999999992006, -8.660254037844389075, -173.6250000040968189 ) ) ;
#28561 = ORIENTED_EDGE ( 'NONE', *, *, #33231, .T. ) ;
#28562 =( BOUNDED_CURVE ( )  B_SPLINE_CURVE ( 2, ( #30111, #31181, #41286, #41507, #21662, #18634, #8723 ),
 .UNSPECIFIED., .F., .F. ) 
 B_SPLINE_CURVE_WITH_KNOTS ( ( 3, 2, 2, 3 ),
 ( 0.3283582089552238847, 0.3296019900497513255, 0.3308457711442787108, 0.3320895522388061516 ),
 .UNSPECIFIED. ) 
 CURVE ( )  GEOMETRIC_REPRESENTATION_ITEM ( )  RATIONAL_B_SPLINE_CURVE ( ( 1.000000000000000000, 0.8660254037844387076, 1.000000000000000000, 0.8660254037844387076, 1.000000000000000000, 0.8660254037844207220, 1.000000000000017986 ) ) 
 REPRESENTATION_ITEM ( '' )  );
#28563 = VERTEX_POINT ( 'NONE', #14696 ) ;
#28564 = EDGE_CURVE ( 'NONE', #13865, #39976, #13520, .T. ) ;
#28565 = VERTEX_POINT ( 'NONE', #716 ) ;
#28566 = EDGE_CURVE ( 'NONE', #31053, #31108, #17945, .T. ) ;
#28567 = CARTESIAN_POINT ( 'NONE',  ( -9.999999999999998224, 1.224646799147353059E-15, -135.1250000040967620 ) ) ;
#28568 = CARTESIAN_POINT ( 'NONE',  ( 10.81189881249999729, 0.000000000000000000, -178.3437500020483810 ) ) ;
#28569 = CARTESIAN_POINT ( 'NONE',  ( 5.405949406249999534, 9.363379034771803333, -31.09375000204836326 ) ) ;
#28570 = LINE ( 'NONE', #8282, #17746 ) ;
#28571 = CARTESIAN_POINT ( 'NONE',  ( 5.405949406249999534, 9.363379034771803333, -166.0937500020484094 ) ) ;
#28572 = CARTESIAN_POINT ( 'NONE',  ( -10.81189881249999729, 1.324075727343319199E-15, -153.5937500020483810 ) ) ;
#28573 = DIRECTION ( 'NONE',  ( -0.000000000000000000, -0.000000000000000000, 1.000000000000000000 ) ) ;
#28574 = CARTESIAN_POINT ( 'NONE',  ( 10.81189881249999551, -6.242252689847874514, -133.4687500020483810 ) ) ;
#28575 = CARTESIAN_POINT ( 'NONE',  ( -5.405949406250003975, -9.363379034771801557, -141.5312500020483810 ) ) ;
#28576 = CARTESIAN_POINT ( 'NONE',  ( 5.405949406249992428, -9.363379034771808662, -148.5937500020483810 ) ) ;
#28577 = CARTESIAN_POINT ( 'NONE',  ( 9.999999999999998224, 0.000000000000000000, -152.0000000000000000 ) ) ;
#28578 = CARTESIAN_POINT ( 'NONE',  ( -9.999999999999998224, 1.224646799147353059E-15, -177.1250000040968189 ) ) ;
#28579 = CARTESIAN_POINT ( 'NONE',  ( -10.00000000000000000, -5.773502691896251982, -170.6250000000000284 ) ) ;
#28580 = CARTESIAN_POINT ( 'NONE',  ( -10.81189881249999729, 1.324075727343319199E-15, -84.59375000204836681 ) ) ;
#28581 = CARTESIAN_POINT ( 'NONE',  ( -5.000000000000003553, -8.660254037844383745, -114.9999999999999858 ) ) ;
#28582 = CARTESIAN_POINT ( 'NONE',  ( 10.81189881249999729, 0.000000000000000000, -54.03125000204836681 ) ) ;
#28583 = CARTESIAN_POINT ( 'NONE',  ( 9.999999999999998224, 0.000000000000000000, -78.87500000409677625 ) ) ;
#28584 = CARTESIAN_POINT ( 'NONE',  ( -10.81189881249999729, 1.324075727343319199E-15, -168.5937500020484094 ) ) ;
#28585 = EDGE_CURVE ( 'NONE', #36032, #34991, #8178, .T. ) ;
#28586 = CARTESIAN_POINT ( 'NONE',  ( -4.999999999999996447, 8.660254037844387298, -135.0000000000000000 ) ) ;
#28587 = CARTESIAN_POINT ( 'NONE',  ( 7.644554776091147741E-16, 12.48450537969573659, -148.1562500020484094 ) ) ;
#28588 = CARTESIAN_POINT ( 'NONE',  ( 7.644554776091147741E-16, 12.48450537969573659, -35.65625000204835970 ) ) ;
#28589 = CARTESIAN_POINT ( 'NONE',  ( -2.121150477449813534E-15, -11.54700538379251284, -122.7500000040967905 ) ) ;
#28590 = CARTESIAN_POINT ( 'NONE',  ( -4.999999999999996447, 8.660254037844387298, -102.0000000000000000 ) ) ;
#28591 = VERTEX_POINT ( 'NONE', #40945 ) ;
#28592 = CARTESIAN_POINT ( 'NONE',  ( -5.405949406250003975, -9.363379034771801557, -120.5312500020483952 ) ) ;
#28593 = CARTESIAN_POINT ( 'NONE',  ( 10.00000000000000000, 5.773502691896255534, -141.7500000040967905 ) ) ;
#28594 = FACE_OUTER_BOUND ( 'NONE', #23133, .T. ) ;
#28595 = CARTESIAN_POINT ( 'NONE',  ( 5.405949406249992428, -9.363379034771808662, -180.2812500020484094 ) ) ;
#28596 = EDGE_LOOP ( 'NONE', ( #3220, #27301, #5492, #4386 ) ) ;
#28597 = CARTESIAN_POINT ( 'NONE',  ( 10.00000000000000000, 5.773502691896255534, -53.25000000409676915 ) ) ;
#28598 = EDGE_CURVE ( 'NONE', #10904, #37078, #11391, .T. ) ;
#28599 = CARTESIAN_POINT ( 'NONE',  ( 7.070501591499376803E-16, 11.54700538379251284, -130.6250000000000000 ) ) ;
#28600 = CARTESIAN_POINT ( 'NONE',  ( 10.81189881249999729, 0.000000000000000000, -67.53125000204838102 ) ) ;
#28601 = CYLINDRICAL_SURFACE ( 'NONE', #31797, 9.999999999999998224 ) ;
#28602 = CARTESIAN_POINT ( 'NONE',  ( -5.405949406249996869, 9.363379034771805109, -166.0312500020484094 ) ) ;
#28603 = CARTESIAN_POINT ( 'NONE',  ( 12.99038105676667954, -7.500000000000051514, 49.99999999999998579 ) ) ;
#28604 = DIRECTION ( 'NONE',  ( 1.000000000000000000, 0.000000000000000000, 0.000000000000000000 ) ) ;
#28605 = ORIENTED_EDGE ( 'NONE', *, *, #2901, .F. ) ;
#28606 = CARTESIAN_POINT ( 'NONE',  ( 5.000000000000000000, 8.660254037844385522, -17.12500000409675138 ) ) ;
#28607 = CARTESIAN_POINT ( 'NONE',  ( -9.999999999999998224, 1.224646799147353059E-15, -172.6250000040968189 ) ) ;
#28608 = CARTESIAN_POINT ( 'NONE',  ( 5.000000000000000000, 8.660254037844385522, -27.24999999999996803 ) ) ;
#28610 = ORIENTED_EDGE ( 'NONE', *, *, #5677, .F. ) ;
#28609 = CARTESIAN_POINT ( 'NONE',  ( 10.81189881249999907, 6.242252689847868297, -74.90625000204839523 ) ) ;
#28611 = CARTESIAN_POINT ( 'NONE',  ( 0.000000000000000000, 0.000000000000000000, 0.000000000000000000 ) ) ;
#28612 = ADVANCED_FACE ( 'NONE', ( #4293 ), #27383, .T. ) ;
#28614 = ORIENTED_EDGE ( 'NONE', *, *, #37969, .T. ) ;
#28613 = CARTESIAN_POINT ( 'NONE',  ( 9.999999999999998224, 0.000000000000000000, -177.8750000040967905 ) ) ;
#28615 = ORIENTED_EDGE ( 'NONE', *, *, #6781, .T. ) ;
#28616 = ADVANCED_FACE ( 'NONE', ( #30629 ), #31279, .T. ) ;
#28617 = CARTESIAN_POINT ( 'NONE',  ( 10.81189881249999551, -6.242252689847874514, -29.96875000204834549 ) ) ;
#28618 = DIRECTION ( 'NONE',  ( -0.000000000000000000, -0.000000000000000000, -1.000000000000000000 ) ) ;
#28619 = CARTESIAN_POINT ( 'NONE',  ( -10.81189881249999907, -6.242252689847864744, -6.656250002048364145 ) ) ;
#28622 = ADVANCED_FACE ( 'NONE', ( #17645 ), #37734, .F. ) ;
#28621 = ORIENTED_EDGE ( 'NONE', *, *, #18843, .F. ) ;
#28620 = CARTESIAN_POINT ( 'NONE',  ( 10.81189881249999907, 6.242252689847868297, -56.71875000204838813 ) ) ;
#28623 = DIRECTION ( 'NONE',  ( -0.000000000000000000, -0.000000000000000000, -1.000000000000000000 ) ) ;
#28624 = CARTESIAN_POINT ( 'NONE',  ( 10.00000000000000000, 5.773502691896255534, -34.87499999999996447 ) ) ;
#28625 = CARTESIAN_POINT ( 'NONE',  ( -10.81189881249999729, 1.324075727343319199E-15, -191.0937500020484094 ) ) ;
#28626 = CARTESIAN_POINT ( 'NONE',  ( -10.81189881249999729, 1.324075727343319199E-15, -180.5937500020484094 ) ) ;
#28627 = CARTESIAN_POINT ( 'NONE',  ( 7.644554776091147741E-16, 12.48450537969573659, -159.9687500020483810 ) ) ;
#28628 = CARTESIAN_POINT ( 'NONE',  ( -5.405949406249996869, 9.363379034771805109, -168.8437500020484094 ) ) ;
#28629 = CARTESIAN_POINT ( 'NONE',  ( 9.999999999999998224, 0.000000000000000000, -200.0000000000000000 ) ) ;
#28630 = VECTOR ( 'NONE', #6242, 1000.000000000000000 ) ;
#28631 = CARTESIAN_POINT ( 'NONE',  ( -9.999999999999227285, -5.773502691896698735, -127.1249999999999574 ) ) ;
#28632 = CARTESIAN_POINT ( 'NONE',  ( -9.999999999999998224, 5.773502691896259087, -199.3750000000000000 ) ) ;
#28633 = CARTESIAN_POINT ( 'NONE',  ( -10.81189881249999729, 6.242252689847871849, -101.2187500020483810 ) ) ;
#28634 = CARTESIAN_POINT ( 'NONE',  ( -9.999999999999479527, -5.773502691896549521, -73.12499999999995737 ) ) ;
#28635 = CARTESIAN_POINT ( 'NONE',  ( 10.81189881249999729, 0.000000000000000000, -70.53125000204838102 ) ) ;
#28636 = CARTESIAN_POINT ( 'NONE',  ( -5.405949406249996869, 9.363379034771805109, -93.84375000204838102 ) ) ;
#28637 = CARTESIAN_POINT ( 'NONE',  ( 10.81189881249999907, 6.242252689847868297, -68.90625000204839523 ) ) ;
#28638 = CARTESIAN_POINT ( 'NONE',  ( 5.000000000000000000, 8.660254037844385522, -144.6250000040967905 ) ) ;
#28639 = CARTESIAN_POINT ( 'NONE',  ( 5.000000000000000000, 8.660254037844385522, -121.7500000000000000 ) ) ;
#28640 = ADVANCED_FACE ( 'NONE', ( #18085 ), #24807, .F. ) ;
#28641 = ORIENTED_EDGE ( 'NONE', *, *, #5437, .T. ) ;
#28642 = CARTESIAN_POINT ( 'NONE',  ( -10.81189881249999729, 6.242252689847871849, -147.9062500020484094 ) ) ;
#28643 = CARTESIAN_POINT ( 'NONE',  ( -5.405949406249996869, 9.363379034771805109, -164.5312500020484094 ) ) ;
#28644 = FACE_OUTER_BOUND ( 'NONE', #15264, .T. ) ;
#28645 = CARTESIAN_POINT ( 'NONE',  ( -9.999999999999998224, 1.224646799147353059E-15, -119.7500000000000000 ) ) ;
#28646 = CARTESIAN_POINT ( 'NONE',  ( -5.405949406249996869, 9.363379034771805109, -99.84375000204838102 ) ) ;
#28647 = EDGE_LOOP ( 'NONE', ( #11515, #34345, #34986, #20617 ) ) ;
#28648 = CARTESIAN_POINT ( 'NONE',  ( -5.000000000000003553, -8.660254037844383745, -62.49999999999997158 ) ) ;
#28649 = CARTESIAN_POINT ( 'NONE',  ( -10.81189881249999907, -6.242252689847864744, -195.4687500020484094 ) ) ;
#28650 = CARTESIAN_POINT ( 'NONE',  ( 10.00000000000000000, 5.773502691896255534, -74.25000000409677625 ) ) ;
#28651 = CARTESIAN_POINT ( 'NONE',  ( -8.236488666302303585, -5.752346336555091533, -180.0000000000000284 ) ) ;
#28652 = CARTESIAN_POINT ( 'NONE',  ( 4.999999999999992006, -8.660254037844389075, -11.62500000409674783 ) ) ;
#28653 = CARTESIAN_POINT ( 'NONE',  ( -10.81189881249999729, 6.242252689847871849, -92.40625000204838102 ) ) ;
#28654 = AXIS2_PLACEMENT_3D ( 'NONE', #21842, #29174, #12537 ) ;
#28655 = CARTESIAN_POINT ( 'NONE',  ( 10.81189881249999729, 0.000000000000000000, -66.03125000204838102 ) ) ;
#28656 = CARTESIAN_POINT ( 'NONE',  ( 9.999999999999998224, 0.000000000000000000, -71.37500000409677625 ) ) ;
#28657 = LINE ( 'NONE', #41581, #29835 ) ;
#28658 = CARTESIAN_POINT ( 'NONE',  ( -2.293366432827344421E-15, -12.48450537969573659, -25.71875000204837391 ) ) ;
#28659 = CARTESIAN_POINT ( 'NONE',  ( 9.999999999999998224, 0.000000000000000000, -47.37500000409677625 ) ) ;
#28660 = CARTESIAN_POINT ( 'NONE',  ( -10.81189881249999729, 6.242252689847871849, -195.9062500020484094 ) ) ;
#28661 = CARTESIAN_POINT ( 'NONE',  ( 10.81189881249999729, 0.000000000000000000, -19.53125000204835970 ) ) ;
#28662 = CARTESIAN_POINT ( 'NONE',  ( -10.81189881249999729, 6.242252689847871849, -6.718750002048347270 ) ) ;
#28663 = CARTESIAN_POINT ( 'NONE',  ( 9.999999999999998224, 0.000000000000000000, -140.3750000040967905 ) ) ;
#28664 = VECTOR ( 'NONE', #12594, 1000.000000000000000 ) ;
#28665 = CARTESIAN_POINT ( 'NONE',  ( -4.999999999999996447, 8.660254037844387298, 1.124999995903236405 ) ) ;
#28666 = CARTESIAN_POINT ( 'NONE',  ( -2.121150477449813534E-15, -11.54700538379251284, -112.2500000040967763 ) ) ;
#28667 = CARTESIAN_POINT ( 'NONE',  ( 5.000000000000000000, 8.660254037844385522, -174.2500000000000284 ) ) ;
#28668 = CARTESIAN_POINT ( 'NONE',  ( 9.999999999999998224, 0.000000000000000000, -167.0000000000000000 ) ) ;
#28670 = ORIENTED_EDGE ( 'NONE', *, *, #6276, .T. ) ;
#28669 = CARTESIAN_POINT ( 'NONE',  ( -10.81189881249999729, 6.242252689847871849, -101.4062500020483952 ) ) ;
#28671 = CARTESIAN_POINT ( 'NONE',  ( -2.121150477449813534E-15, -11.54700538379251284, -161.7500000040968189 ) ) ;
#28672 = VERTEX_POINT ( 'NONE', #14832 ) ;
#28673 = VERTEX_POINT ( 'NONE', #18300 ) ;
#28674 = CARTESIAN_POINT ( 'NONE',  ( -5.405949406249996869, 9.363379034771805109, -32.53125000204837391 ) ) ;
#28675 = ITEM_DEFINED_TRANSFORMATION ( 'NONE', 'NONE', #13124,  #39998 ) ;
#28676 = CARTESIAN_POINT ( 'NONE',  ( -10.81189881249999729, 1.324075727343319199E-15, -81.59375000204838102 ) ) ;
#28677 = DIRECTION ( 'NONE',  ( 0.000000000000000000, 0.000000000000000000, -1.000000000000000000 ) ) ;
#28678 = LINE ( 'NONE', #32341, #3189 ) ;
#28679 =( BOUNDED_CURVE ( )  B_SPLINE_CURVE ( 2, ( #25483, #19194, #9269, #12910, #31751, #22234, #42483 ),
 .UNSPECIFIED., .F., .F. ) 
 B_SPLINE_CURVE_WITH_KNOTS ( ( 3, 2, 2, 3 ),
 ( 0.4029850746268657802, 0.4042288557213931655, 0.4054726368159204397, 0.4067164179104478250 ),
 .UNSPECIFIED. ) 
 CURVE ( )  GEOMETRIC_REPRESENTATION_ITEM ( )  RATIONAL_B_SPLINE_CURVE ( ( 0.9999999999999880096, 0.8660254037844506980, 1.000000000000000000, 0.8660254037844387076, 1.000000000000000000, 0.8660254037844327124, 1.000000000000005995 ) ) 
 REPRESENTATION_ITEM ( '' )  );
#28680 = VECTOR ( 'NONE', #38151, 1000.000000000000000 ) ;
#28681 = CARTESIAN_POINT ( 'NONE',  ( -9.999999999999998224, 1.224646799147353059E-15, -106.2499999999999858 ) ) ;
#28682 = CARTESIAN_POINT ( 'NONE',  ( -10.81189881249999729, 6.242252689847871849, -153.9062500020483810 ) ) ;
#28683 = CARTESIAN_POINT ( 'NONE',  ( 4.999999999999992006, -8.660254037844389075, -10.12500000409674605 ) ) ;
#28684 = CARTESIAN_POINT ( 'NONE',  ( -9.999999999999998224, 0.000000000000000000, -99.99999999999998579 ) ) ;
#28685 = ADVANCED_FACE ( 'NONE', ( #21326 ), #1492, .T. ) ;
#28686 = CARTESIAN_POINT ( 'NONE',  ( 5.405949406249992428, -9.363379034771808662, -129.0937500020483810 ) ) ;
#28687 = CARTESIAN_POINT ( 'NONE',  ( -5.405949406250003975, -9.363379034771801557, -112.8437500020483810 ) ) ;
#28688 = CIRCLE ( 'NONE', #20400, 35.00000000000000711 ) ;
#28689 = CARTESIAN_POINT ( 'NONE',  ( 10.81189881249999729, 0.000000000000000000, -85.34375000204836681 ) ) ;
#28690 = CARTESIAN_POINT ( 'NONE',  ( 5.405949406249999534, 9.363379034771803333, -91.28125000204838102 ) ) ;
#28691 = CARTESIAN_POINT ( 'NONE',  ( -10.00000000000000000, -5.773502691896251982, -169.5000000040967620 ) ) ;
#28692 = CARTESIAN_POINT ( 'NONE',  ( 7.644554776091147741E-16, 12.48450537969573659, -173.6562500020483810 ) ) ;
#28693 =( BOUNDED_CURVE ( )  B_SPLINE_CURVE ( 2, ( #15436, #28634, #6169, #27075, #23635, #24056, #10230 ),
 .UNSPECIFIED., .F., .F. ) 
 B_SPLINE_CURVE_WITH_KNOTS ( ( 3, 2, 2, 3 ),
 ( 0.6305970149253732338, 0.6318407960199006190, 0.6330845771144280043, 0.6343283582089553896 ),
 .UNSPECIFIED. ) 
 CURVE ( )  GEOMETRIC_REPRESENTATION_ITEM ( )  RATIONAL_B_SPLINE_CURVE ( ( 0.9999999999999880096, 0.8660254037844506980, 1.000000000000000000, 0.8660254037844387076, 1.000000000000000000, 0.8660254037844267172, 1.000000000000011990 ) ) 
 REPRESENTATION_ITEM ( '' )  );
#28694 = CARTESIAN_POINT ( 'NONE',  ( -5.405949406250003975, -9.363379034771801557, -177.5312500020483810 ) ) ;
#28695 = CARTESIAN_POINT ( 'NONE',  ( 10.81189881249999729, 0.000000000000000000, -186.0312500020484094 ) ) ;
#28696 = CARTESIAN_POINT ( 'NONE',  ( 7.644554776091147741E-16, 12.48450537969573659, -42.96875000204835970 ) ) ;
#28697 = CARTESIAN_POINT ( 'NONE',  ( -2.121150477449813534E-15, -11.54700538379251284, -163.2500000040967620 ) ) ;
#28698 = CARTESIAN_POINT ( 'NONE',  ( 7.070501591499376803E-16, 11.54700538379251284, -86.00000000409677625 ) ) ;
#28699 = CARTESIAN_POINT ( 'NONE',  ( -5.405949406249996869, 9.363379034771805109, -12.84375000204834905 ) ) ;
#28700 = CARTESIAN_POINT ( 'NONE',  ( -9.999999999999742428, -5.773502691896402084, -157.1250000000000000 ) ) ;
#28701 = CARTESIAN_POINT ( 'NONE',  ( -10.81189881249999729, 1.324075727343319199E-15, -120.5937500020483952 ) ) ;
#28702 = CARTESIAN_POINT ( 'NONE',  ( 5.000000000000000000, 8.660254037844385522, -85.74999999999998579 ) ) ;
#28703 = CARTESIAN_POINT ( 'NONE',  ( -5.405949406250003975, -9.363379034771801557, -18.53125000204835970 ) ) ;
#28704 = CARTESIAN_POINT ( 'NONE',  ( -10.00000000000000000, -5.773502691896251982, -99.00000000409679046 ) ) ;
#28705 = CARTESIAN_POINT ( 'NONE',  ( -9.999999999999998224, 1.224646799147353059E-15, -136.6250000040967620 ) ) ;
#28706 = CARTESIAN_POINT ( 'NONE',  ( 10.81189881249999551, -6.242252689847874514, -115.6562500020483810 ) ) ;
#28707 = CARTESIAN_POINT ( 'NONE',  ( -10.81189881249999729, 1.324075727343319199E-15, -101.2812500020483952 ) ) ;
#28708 = EDGE_LOOP ( 'NONE', ( #32382, #4421, #9937, #42520 ) ) ;
#28709 =( BOUNDED_CURVE ( )  B_SPLINE_CURVE ( 2, ( #36299, #7153, #12967, #26795, #6314, #25956, #36085 ),
 .UNSPECIFIED., .F., .F. ) 
 B_SPLINE_CURVE_WITH_KNOTS ( ( 3, 2, 2, 3 ),
 ( 0.4738805970149255198, 0.4751243781094529051, 0.4763681592039803459, 0.4776119402985076756 ),
 .UNSPECIFIED. ) 
 CURVE ( )  GEOMETRIC_REPRESENTATION_ITEM ( )  RATIONAL_B_SPLINE_CURVE ( ( 0.9999999999999820144, 0.8660254037844566932, 1.000000000000000000, 0.8660254037844387076, 1.000000000000000000, 0.8660254037844148378, 1.000000000000023981 ) ) 
 REPRESENTATION_ITEM ( '' )  );
#28710 = CARTESIAN_POINT ( 'NONE',  ( 5.000000000000000000, 8.660254037844385522, -93.62500000409677625 ) ) ;
#28711 = DIRECTION ( 'NONE',  ( -0.000000000000000000, -0.000000000000000000, -1.000000000000000000 ) ) ;
#28712 = CARTESIAN_POINT ( 'NONE',  ( 10.81189881249999907, 6.242252689847868297, -158.9062500020483810 ) ) ;
#28713 = CARTESIAN_POINT ( 'NONE',  ( 10.81189881249999907, 6.242252689847868297, -49.21875000204835970 ) ) ;
#28714 = VERTEX_POINT ( 'NONE', #7747 ) ;
#28715 = CARTESIAN_POINT ( 'NONE',  ( -9.999999999999998224, 1.224646799147353059E-15, -14.74999999999995737 ) ) ;
#28716 = CARTESIAN_POINT ( 'NONE',  ( -10.81189881249999729, 1.324075727343319199E-15, -24.78125000204836681 ) ) ;
#28717 = CARTESIAN_POINT ( 'NONE',  ( -5.000000000000003553, -8.660254037844383745, -151.0000000000000000 ) ) ;
#28718 = CARTESIAN_POINT ( 'NONE',  ( -10.00000000000000000, -5.773502691896251982, -22.50000000409676915 ) ) ;
#28719 = VECTOR ( 'NONE', #184, 1000.000000000000000 ) ;
#28720 = CARTESIAN_POINT ( 'NONE',  ( 7.070501591499377789E-16, 11.54700538379251284, -198.1250000000000000 ) ) ;
#28722 = EDGE_LOOP ( 'NONE', ( #26245, #29871, #6622, #30418 ) ) ;
#28721 = CARTESIAN_POINT ( 'NONE',  ( 5.405949406249992428, -9.363379034771808662, -129.2812500020483810 ) ) ;
#28723 = CARTESIAN_POINT ( 'NONE',  ( 9.999999999999998224, 0.000000000000000000, -170.0000000000000000 ) ) ;
#28724 = EDGE_LOOP ( 'NONE', ( #32580, #12237, #9621, #39781 ) ) ;
#28725 = CARTESIAN_POINT ( 'NONE',  ( 5.405949406249992428, -9.363379034771808662, -57.28125000204836681 ) ) ;
#28726 = DATE_AND_TIME ( #29345, #2177 ) ;
#28727 = CARTESIAN_POINT ( 'NONE',  ( -10.81189881249999729, 6.242252689847871849, -105.7187500020483668 ) ) ;
#28729 = ORIENTED_EDGE ( 'NONE', *, *, #5611, .F. ) ;
#28728 = EDGE_LOOP ( 'NONE', ( #34808, #14279, #3230, #26663 ) ) ;
#28730 = CARTESIAN_POINT ( 'NONE',  ( -5.000000000000003553, -8.660254037844383745, -175.3750000040967905 ) ) ;
#28731 = CARTESIAN_POINT ( 'NONE',  ( 4.999999999999992006, -8.660254037844389075, -197.6250000040967905 ) ) ;
#28732 = CARTESIAN_POINT ( 'NONE',  ( -5.405949406249996869, 9.363379034771805109, -161.3437500020484094 ) ) ;
#28733 = CARTESIAN_POINT ( 'NONE',  ( -5.405949406249996869, 9.363379034771805109, -191.5312500020484094 ) ) ;
#28734 = CARTESIAN_POINT ( 'NONE',  ( -2.293366432827344421E-15, -12.48450537969573659, -10.71875000204836681 ) ) ;
#28735 = DIRECTION ( 'NONE',  ( 1.000000000000000000, 0.000000000000000000, 0.000000000000000000 ) ) ;
#28736 = CARTESIAN_POINT ( 'NONE',  ( -5.405949406249996869, 9.363379034771805109, -143.3437500020483810 ) ) ;
#28737 = CARTESIAN_POINT ( 'NONE',  ( -10.81189881249999729, 1.324075727343319199E-15, -110.0937500020483810 ) ) ;
#28738 = FACE_OUTER_BOUND ( 'NONE', #4553, .T. ) ;
#28739 = CARTESIAN_POINT ( 'NONE',  ( 7.644554776091147741E-16, 12.48450537969573659, -115.1562500020483952 ) ) ;
#28740 = CARTESIAN_POINT ( 'NONE',  ( 5.000000000000000000, 8.660254037844385522, -195.6250000040967905 ) ) ;
#28741 = CARTESIAN_POINT ( 'NONE',  ( 10.81189881249999551, -6.242252689847874514, -122.9687500020483952 ) ) ;
#28742 = CARTESIAN_POINT ( 'NONE',  ( -5.405949406250003975, -9.363379034771801557, -192.5312500020484094 ) ) ;
#28743 = CARTESIAN_POINT ( 'NONE',  ( 7.070501591499376803E-16, 11.54700538379251284, -12.12499999999996270 ) ) ;
#28744 = APPROVAL_PERSON_ORGANIZATION ( #39627, #32804, #798 ) ;
#28745 = CARTESIAN_POINT ( 'NONE',  ( -4.999999999999996447, 8.660254037844387298, -139.5000000000000000 ) ) ;
#28746 = CARTESIAN_POINT ( 'NONE',  ( -4.999999999999996447, 8.660254037844387298, -11.99999999999995559 ) ) ;
#28747 = CARTESIAN_POINT ( 'NONE',  ( -5.405949406249996869, 9.363379034771805109, -71.34375000204836681 ) ) ;
#28748 = CARTESIAN_POINT ( 'NONE',  ( -2.293366432827344421E-15, -12.48450537969573659, -54.21875000204838102 ) ) ;
#28749 = CARTESIAN_POINT ( 'NONE',  ( 9.999999999999996447, -5.773502691896262640, -185.5000000040967905 ) ) ;
#28750 = CARTESIAN_POINT ( 'NONE',  ( 10.81189881249999907, 6.242252689847868297, -26.90625000204838102 ) ) ;
#28751 = CARTESIAN_POINT ( 'NONE',  ( -2.293366432827344421E-15, -12.48450537969573659, -40.71875000204835970 ) ) ;
#28752 = CARTESIAN_POINT ( 'NONE',  ( -9.999999999999998224, 1.224646799147353059E-15, -8.749999999999952038 ) ) ;
#28753 = CARTESIAN_POINT ( 'NONE',  ( 10.81189881249999551, -6.242252689847874514, -148.4687500020484094 ) ) ;
#28754 = CARTESIAN_POINT ( 'NONE',  ( -5.000000000000003553, -8.660254037844383745, -111.9999999999999858 ) ) ;
#28755 = ADVANCED_FACE ( 'NONE', ( #37952 ), #21110, .T. ) ;
#28756 = CARTESIAN_POINT ( 'NONE',  ( -9.999999999999998224, 1.224646799147353059E-15, -102.1250000040967905 ) ) ;
#28757 = CARTESIAN_POINT ( 'NONE',  ( 9.999999999999996447, -5.773502691896262640, -75.62499999999998579 ) ) ;
#28758 = CARTESIAN_POINT ( 'NONE',  ( -2.293366432827344421E-15, -12.48450537969573659, -141.4062500020483810 ) ) ;
#28759 = CARTESIAN_POINT ( 'NONE',  ( -10.81189881249999729, 6.242252689847871849, -12.90625000204835970 ) ) ;
#28760 = ORIENTED_EDGE ( 'NONE', *, *, #18012, .F. ) ;
#28761 = DIRECTION ( 'NONE',  ( -0.000000000000000000, -0.000000000000000000, 1.000000000000000000 ) ) ;
#28762 = CARTESIAN_POINT ( 'NONE',  ( -4.999999999999996447, 8.660254037844387298, -115.8750000040967905 ) ) ;
#28763 = CARTESIAN_POINT ( 'NONE',  ( -99.99999999999994316, -40.00000000000000711, -160.0000000000000000 ) ) ;
#28764 = CARTESIAN_POINT ( 'NONE',  ( 10.81189881249999551, -6.242252689847874514, -74.96875000204838102 ) ) ;
#28765 = CARTESIAN_POINT ( 'NONE',  ( -10.00000000000000000, -5.773502691896251982, -40.12499999999996447 ) ) ;
#28766 = CARTESIAN_POINT ( 'NONE',  ( 4.999999999999992006, -8.660254037844389075, -25.12500000409675849 ) ) ;
#28767 = CARTESIAN_POINT ( 'NONE',  ( 5.405949406249999534, 9.363379034771803333, -52.28125000204835970 ) ) ;
#28768 = DIRECTION ( 'NONE',  ( -0.7071067811865463515, 0.000000000000000000, -0.7071067811865487940 ) ) ;
#28769 = CARTESIAN_POINT ( 'NONE',  ( -5.405949406249996869, 9.363379034771805109, -34.03125000204837391 ) ) ;
#28770 = CARTESIAN_POINT ( 'NONE',  ( 9.999999999999998224, 0.000000000000000000, -137.0000000000000000 ) ) ;
#28771 = CARTESIAN_POINT ( 'NONE',  ( -5.405949406250003975, -9.363379034771801557, -147.5312500020483810 ) ) ;
#28772 = CARTESIAN_POINT ( 'NONE',  ( 7.644554776091147741E-16, 12.48450537969573659, -146.6562500020484379 ) ) ;
#28773 = DIRECTION ( 'NONE',  ( 1.000000000000000000, 0.000000000000000000, 0.000000000000000000 ) ) ;
#28774 =( BOUNDED_CURVE ( )  B_SPLINE_CURVE ( 2, ( #10018, #23196, #36356, #14082, #30321, #30957, #40850 ),
 .UNSPECIFIED., .F., .F. ) 
 B_SPLINE_CURVE_WITH_KNOTS ( ( 3, 2, 2, 3 ),
 ( 0.4776119402985076756, 0.4788557213930350054, 0.4800995024875623352, 0.4813432835820896649 ),
 .UNSPECIFIED. ) 
 CURVE ( )  GEOMETRIC_REPRESENTATION_ITEM ( )  RATIONAL_B_SPLINE_CURVE ( ( 0.9999999999999761302, 0.8660254037844625774, 1.000000000000000000, 0.8660254037844387076, 1.000000000000000000, 0.8660254037844267172, 1.000000000000011990 ) ) 
 REPRESENTATION_ITEM ( '' )  );
#28775 = CARTESIAN_POINT ( 'NONE',  ( -9.999999999998969713, -5.773502691896847949, -58.12499999999997158 ) ) ;
#28776 = ORIENTED_EDGE ( 'NONE', *, *, #38356, .T. ) ;
#28777 = VERTEX_POINT ( 'NONE', #10963 ) ;
#28778 = ORIENTED_EDGE ( 'NONE', *, *, #36000, .F. ) ;
#28779 = CARTESIAN_POINT ( 'NONE',  ( -2.121150477449813534E-15, -11.54700538379251284, -100.2500000040967905 ) ) ;
#28780 = CARTESIAN_POINT ( 'NONE',  ( -10.81189881249999907, -6.242252689847864744, -184.9687500020484094 ) ) ;
#28781 = CARTESIAN_POINT ( 'NONE',  ( 10.81189881249999907, 6.242252689847868297, -29.71875000204834194 ) ) ;
#28782 = CARTESIAN_POINT ( 'NONE',  ( 5.000000000000000000, 8.660254037844385522, -118.7500000000000000 ) ) ;
#28783 = CARTESIAN_POINT ( 'NONE',  ( -10.81189881249999729, -6.242252689847864744, -163.9687500020483526 ) ) ;
#28784 = CARTESIAN_POINT ( 'NONE',  ( 10.81189881249999729, 0.000000000000000000, -152.8437500020483810 ) ) ;
#28785 = DIRECTION ( 'NONE',  ( 1.000000000000000000, 0.000000000000000000, 0.000000000000000000 ) ) ;
#28786 = CARTESIAN_POINT ( 'NONE',  ( -10.81189881249999729, 6.242252689847871849, -131.2187500020483810 ) ) ;
#28787 = CARTESIAN_POINT ( 'NONE',  ( 10.81189881249999907, 6.242252689847868297, -137.9062500020483810 ) ) ;
#28788 = CARTESIAN_POINT ( 'NONE',  ( 10.81189881249999729, 0.000000000000000000, -16.34375000204835260 ) ) ;
#28789 = CARTESIAN_POINT ( 'NONE',  ( -5.405949406250003975, -9.363379034771801557, -150.3437500020483810 ) ) ;
#28790 = LINE ( 'NONE', #22513, #34355 ) ;
#28791 = CARTESIAN_POINT ( 'NONE',  ( 5.000000000000000000, 8.660254037844385522, -177.6250000040968189 ) ) ;
#28792 = CARTESIAN_POINT ( 'NONE',  ( -9.999999999999998224, 5.773502691896259087, -167.8749999999999716 ) ) ;
#28793 = CARTESIAN_POINT ( 'NONE',  ( -10.81189881249999907, -6.242252689847864744, -84.46875000204836681 ) ) ;
#28794 = CARTESIAN_POINT ( 'NONE',  ( -4.999999999999996447, 8.660254037844387298, -184.8750000040967905 ) ) ;
#28795 = CARTESIAN_POINT ( 'NONE',  ( 5.405949406249992428, -9.363379034771808662, -51.28125000204835970 ) ) ;
#28796 = CARTESIAN_POINT ( 'NONE',  ( -2.293366432827344421E-15, -12.48450537969573659, -61.71875000204837391 ) ) ;
#28797 = DIRECTION ( 'NONE',  ( -1.000000000000000000, 0.000000000000000000, 0.000000000000000000 ) ) ;
#28798 = CARTESIAN_POINT ( 'NONE',  ( 10.81189881249999907, 6.242252689847868297, -169.2187500020483810 ) ) ;
#28799 = CARTESIAN_POINT ( 'NONE',  ( 4.999999999999992006, -8.660254037844389075, -137.2499999999999716 ) ) ;
#28800 = CARTESIAN_POINT ( 'NONE',  ( 7.644554776091147741E-16, 12.48450537969573659, -143.6562500020484094 ) ) ;
#28801 = CARTESIAN_POINT ( 'NONE',  ( 0.000000000000000000, 0.000000000000000000, -200.0000000000000000 ) ) ;
#28802 = CARTESIAN_POINT ( 'NONE',  ( 10.81189881249999551, -6.242252689847874514, -37.65625000204836681 ) ) ;
#28803 = CARTESIAN_POINT ( 'NONE',  ( -10.00000000000000000, -5.773502691896251982, -126.0000000040967905 ) ) ;
#28804 = CARTESIAN_POINT ( 'NONE',  ( -9.999999999999998224, 5.773502691896259087, -103.3750000000000000 ) ) ;
#28805 = VERTEX_POINT ( 'NONE', #17863 ) ;
#28806 = CARTESIAN_POINT ( 'NONE',  ( 7.644554776091147741E-16, 12.48450537969573659, -118.1562500020483952 ) ) ;
#28807 = CARTESIAN_POINT ( 'NONE',  ( -9.999999999999998224, 1.224646799147353059E-15, -138.1250000040967620 ) ) ;
#28808 = CARTESIAN_POINT ( 'NONE',  ( -4.999999999999996447, 8.660254037844387298, -52.49999999999996447 ) ) ;
#28809 = CARTESIAN_POINT ( 'NONE',  ( -5.405949406250003975, -9.363379034771801557, -171.5312500020484094 ) ) ;
#28810 = CARTESIAN_POINT ( 'NONE',  ( 9.999999999999996447, -5.773502691896262640, -50.50000000409675494 ) ) ;
#28811 = EDGE_CURVE ( 'NONE', #35065, #16036, #37303, .T. ) ;
#28812 = FACE_OUTER_BOUND ( 'NONE', #19042, .T. ) ;
#28813 = ADVANCED_FACE ( 'NONE', ( #11180 ), #37087, .T. ) ;
#28814 = CARTESIAN_POINT ( 'NONE',  ( 7.644554776091147741E-16, 12.48450537969573659, -61.15625000204838102 ) ) ;
#28815 =( BOUNDED_CURVE ( )  B_SPLINE_CURVE ( 2, ( #1016, #1876, #4666, #40902, #1656, #33821, #17597 ),
 .UNSPECIFIED., .F., .F. ) 
 B_SPLINE_CURVE_WITH_KNOTS ( ( 3, 2, 2, 3 ),
 ( 0.000000000000000000, 0.001243781094527364461, 0.002487562189054728923, 0.003731343283582092950 ),
 .UNSPECIFIED. ) 
 CURVE ( )  GEOMETRIC_REPRESENTATION_ITEM ( )  RATIONAL_B_SPLINE_CURVE ( ( 1.000000000000000000, 0.8660254037844387076, 1.000000000000000000, 0.8660254037844387076, 1.000000000000000000, 0.8660254037844383745, 1.000000000000000444 ) ) 
 REPRESENTATION_ITEM ( '' )  );
#28816 = CARTESIAN_POINT ( 'NONE',  ( -9.999999999999998224, 1.224646799147353059E-15, -83.74999999999997158 ) ) ;
#28817 = CARTESIAN_POINT ( 'NONE',  ( 7.644554776091147741E-16, 12.48450537969573659, -172.1562500020484094 ) ) ;
#28818 = CARTESIAN_POINT ( 'NONE',  ( 4.999999999999992006, -8.660254037844389075, -106.1250000040967763 ) ) ;
#28819 = VECTOR ( 'NONE', #24810, 1000.000000000000000 ) ;
#28820 = ORIENTED_EDGE ( 'NONE', *, *, #34065, .T. ) ;
#28821 = CARTESIAN_POINT ( 'NONE',  ( -4.999999999999996447, 8.660254037844387298, -177.0000000000000000 ) ) ;
#28822 = CARTESIAN_POINT ( 'NONE',  ( 5.000000000000000000, 8.660254037844385522, -137.1250000040967620 ) ) ;
#28824 = VERTEX_POINT ( 'NONE', #34297 ) ;
#28823 = CARTESIAN_POINT ( 'NONE',  ( -2.293366432827344421E-15, -12.48450537969573659, -75.40625000204838102 ) ) ;
#28826 = ORIENTED_EDGE ( 'NONE', *, *, #19513, .T. ) ;
#28825 = CARTESIAN_POINT ( 'NONE',  ( -5.000000000000003553, -8.660254037844383745, -178.3750000040967905 ) ) ;
#28827 = EDGE_LOOP ( 'NONE', ( #21193, #2947, #31852, #16459 ) ) ;
#28828 = CARTESIAN_POINT ( 'NONE',  ( 5.405949406249999534, 9.363379034771803333, -26.59375000204835970 ) ) ;
#28829 = CARTESIAN_POINT ( 'NONE',  ( -5.000000000000003553, -8.660254037844383745, -170.8750000040968189 ) ) ;
#28830 = CARTESIAN_POINT ( 'NONE',  ( 10.81189881249999551, -6.242252689847874514, -6.156250002048360592 ) ) ;
#28832 = ORIENTED_EDGE ( 'NONE', *, *, #31491, .T. ) ;
#28831 = CARTESIAN_POINT ( 'NONE',  ( -10.81189881249999907, -6.242252689847864744, -52.96875000204838102 ) ) ;
#28833 = CYLINDRICAL_SURFACE ( 'NONE', #25465, 9.999999999999998224 ) ;
#28834 = CARTESIAN_POINT ( 'NONE',  ( 9.999999999999996447, -5.773502691896262640, -32.12499999999995737 ) ) ;
#28835 = CARTESIAN_POINT ( 'NONE',  ( 10.81189881249999729, 0.000000000000000000, -187.3437500020483810 ) ) ;
#28836 = CARTESIAN_POINT ( 'NONE',  ( -5.405949406250003975, -9.363379034771801557, -174.3437500020484094 ) ) ;
#28837 = CARTESIAN_POINT ( 'NONE',  ( -10.81189881249999729, 6.242252689847871849, -158.2187500020483810 ) ) ;
#28838 = CARTESIAN_POINT ( 'NONE',  ( 10.81189881249999551, -6.242252689847874514, -169.4687500020483810 ) ) ;
#28839 = CARTESIAN_POINT ( 'NONE',  ( -9.999999999999998224, 1.224646799147353059E-15, -192.1250000040967905 ) ) ;
#28840 = CARTESIAN_POINT ( 'NONE',  ( 9.999999999999998224, 0.000000000000000000, -198.5000000000000000 ) ) ;
#28841 = CARTESIAN_POINT ( 'NONE',  ( 10.81189881249999551, -6.242252689847874514, -101.9687500020483810 ) ) ;
#28842 = CARTESIAN_POINT ( 'NONE',  ( 5.000000000000000000, 8.660254037844385522, -18.24999999999996092 ) ) ;
#28843 = CARTESIAN_POINT ( 'NONE',  ( 10.81189881249999551, -6.242252689847874514, -75.15625000204838102 ) ) ;
#28844 = CARTESIAN_POINT ( 'NONE',  ( -10.81189881249999729, 1.324075727343319199E-15, -93.59375000204838102 ) ) ;
#28845 = VECTOR ( 'NONE', #39167, 1000.000000000000000 ) ;
#28846 = CARTESIAN_POINT ( 'NONE',  ( -5.405949406250003975, -9.363379034771801557, -57.53125000204836681 ) ) ;
#28847 = CARTESIAN_POINT ( 'NONE',  ( 7.070501591499377789E-16, 11.54700538379251284, -144.5000000040967905 ) ) ;
#28848 = CARTESIAN_POINT ( 'NONE',  ( 4.999999999999992006, -8.660254037844389075, -126.7499999999999716 ) ) ;
#28849 = VERTEX_POINT ( 'NONE', #20681 ) ;
#28850 = CARTESIAN_POINT ( 'NONE',  ( 10.81189881249999551, -6.242252689847874514, -141.1562500020484094 ) ) ;
#28851 = CARTESIAN_POINT ( 'NONE',  ( 10.81189881249999907, 6.242252689847868297, -154.4062500020484094 ) ) ;
#28852 = CARTESIAN_POINT ( 'NONE',  ( 10.81189881249999729, 0.000000000000000000, -199.5312500020484094 ) ) ;
#28853 = LINE ( 'NONE', #8989, #19920 ) ;
#28854 = CARTESIAN_POINT ( 'NONE',  ( 10.81189881249999551, -6.242252689847874514, -88.46875000204836681 ) ) ;
#28855 = ORIENTED_EDGE ( 'NONE', *, *, #26353, .F. ) ;
#28856 = CARTESIAN_POINT ( 'NONE',  ( -9.999999999999998224, 1.224646799147353059E-15, -67.24999999999997158 ) ) ;
#28857 = CARTESIAN_POINT ( 'NONE',  ( -5.405949406250003975, -9.363379034771801557, -184.8437500020483810 ) ) ;
#28858 = CARTESIAN_POINT ( 'NONE',  ( 5.000000000000000000, 8.660254037844385522, -77.12500000409677625 ) ) ;
#28859 = EDGE_CURVE ( 'NONE', #17374, #5087, #27598, .T. ) ;
#28860 = DIRECTION ( 'NONE',  ( -0.000000000000000000, -0.000000000000000000, 1.000000000000000000 ) ) ;
#28861 = DIRECTION ( 'NONE',  ( -0.000000000000000000, -0.000000000000000000, 1.000000000000000000 ) ) ;
#28862 = CARTESIAN_POINT ( 'NONE',  ( -5.405949406249996869, 9.363379034771805109, -80.53125000204838102 ) ) ;
#28863 = CARTESIAN_POINT ( 'NONE',  ( 10.81189881249999729, 6.242252689847867408, -64.40625000204838102 ) ) ;
#28864 = EDGE_CURVE ( 'NONE', #37716, #31913, #17685, .T. ) ;
#28865 = CARTESIAN_POINT ( 'NONE',  ( -2.121150477449813534E-15, -11.54700538379251284, -70.25000000409679046 ) ) ;
#28866 = CARTESIAN_POINT ( 'NONE',  ( 7.070501591499376803E-16, 11.54700538379251284, -93.50000000409676204 ) ) ;
#28867 = CARTESIAN_POINT ( 'NONE',  ( -5.405949406249996869, 9.363379034771805109, -20.34375000204835615 ) ) ;
#28868 = CARTESIAN_POINT ( 'NONE',  ( 7.070501591499376803E-16, 11.54700538379251284, -47.00000000409676915 ) ) ;
#28869 = CARTESIAN_POINT ( 'NONE',  ( -2.293366432827344421E-15, -12.48450537969573659, -189.4062500020484094 ) ) ;
#28870 = CARTESIAN_POINT ( 'NONE',  ( 10.81189881249999907, 6.242252689847868297, -19.40625000204837747 ) ) ;
#28871 = CARTESIAN_POINT ( 'NONE',  ( -10.81189881249999729, -6.242252689847864744, -4.968750002048339276 ) ) ;
#28872 = CARTESIAN_POINT ( 'NONE',  ( 9.999999999999998224, 0.000000000000000000, -6.875000004096742501 ) ) ;
#28873 = CARTESIAN_POINT ( 'NONE',  ( -5.000000000000003553, -8.660254037844383745, -37.37500000409676915 ) ) ;
#28874 = CC_DESIGN_PERSON_AND_ORGANIZATION_ASSIGNMENT ( #31755, #20563, ( #10394 ) ) ;
#28875 = CARTESIAN_POINT ( 'NONE',  ( 0.000000000000000000, 0.000000000000000000, -200.0000000000000000 ) ) ;
#28876 = CARTESIAN_POINT ( 'NONE',  ( 7.070501591499377789E-16, 11.54700538379251284, -175.6250000000000000 ) ) ;
#28877 = CARTESIAN_POINT ( 'NONE',  ( 9.999999999999479527, 5.773502691896553074, -97.87499999999997158 ) ) ;
#28879 = ORIENTED_EDGE ( 'NONE', *, *, #7820, .F. ) ;
#28878 = CARTESIAN_POINT ( 'NONE',  ( 5.405949406249992428, -9.363379034771808662, -102.2812500020483952 ) ) ;
#28880 = CARTESIAN_POINT ( 'NONE',  ( 4.999999999999992006, -8.660254037844389075, -179.6250000040968189 ) ) ;
#28881 = VECTOR ( 'NONE', #7603, 1000.000000000000000 ) ;
#28882 = ORIENTED_EDGE ( 'NONE', *, *, #13919, .T. ) ;
#28883 = ORIENTED_EDGE ( 'NONE', *, *, #32265, .T. ) ;
#28884 = CARTESIAN_POINT ( 'NONE',  ( 7.644554776091147741E-16, 12.48450537969573659, -26.65625000204837747 ) ) ;
#28885 = COORDINATED_UNIVERSAL_TIME_OFFSET ( 6, 0, .AHEAD. ) ;
#28886 = EDGE_CURVE ( 'NONE', #3335, #32995, #29793, .T. ) ;
#28887 = CARTESIAN_POINT ( 'NONE',  ( -5.405949406249996869, 9.363379034771805109, -78.84375000204838102 ) ) ;
#28888 = LINE ( 'NONE', #2349, #18072 ) ;
#28889 = CARTESIAN_POINT ( 'NONE',  ( 9.999999999999998224, 0.000000000000000000, -126.5000000000000000 ) ) ;
#28890 = CARTESIAN_POINT ( 'NONE',  ( 9.999999999998969713, 5.773502691896851502, -69.75000000409677625 ) ) ;
#28891 = DIRECTION ( 'NONE',  ( 1.000000000000000000, 0.000000000000000000, -0.000000000000000000 ) ) ;
#28892 = CARTESIAN_POINT ( 'NONE',  ( 10.81189881249999729, 0.000000000000000000, -160.5312500020484094 ) ) ;
#28893 = CARTESIAN_POINT ( 'NONE',  ( -9.999999999999998224, 5.773502691896259087, -9.250000004096756712 ) ) ;
#28894 = CARTESIAN_POINT ( 'NONE',  ( -9.999999999999998224, 1.224646799147353059E-15, -77.74999999999998579 ) ) ;
#28895 = CARTESIAN_POINT ( 'NONE',  ( -10.81189881249999729, 6.242252689847871849, -131.2187500020483810 ) ) ;
#28896 = CARTESIAN_POINT ( 'NONE',  ( -10.81189881249999729, 1.324075727343319199E-15, -114.5937500020483810 ) ) ;
#28897 = CARTESIAN_POINT ( 'NONE',  ( -5.405949406250003975, -9.363379034771801557, -75.34375000204838102 ) ) ;
#28898 = CARTESIAN_POINT ( 'NONE',  ( -10.81189881249999729, 6.242252689847871849, -86.40625000204836681 ) ) ;
#28899 = CARTESIAN_POINT ( 'NONE',  ( 9.999999999999998224, 0.000000000000000000, -167.3750000040967905 ) ) ;
#28900 = FACE_OUTER_BOUND ( 'NONE', #35670, .T. ) ;
#28901 = CARTESIAN_POINT ( 'NONE',  ( 5.405949406249999534, 9.363379034771803333, -166.2812500020484094 ) ) ;
#28902 = CARTESIAN_POINT ( 'NONE',  ( 5.405949406249999534, 9.363379034771803333, -179.7812500020484094 ) ) ;
#28903 = CARTESIAN_POINT ( 'NONE',  ( -10.81189881249999729, 1.324075727343319199E-15, -45.59375000204838102 ) ) ;
#28904 = CARTESIAN_POINT ( 'NONE',  ( -5.000000000000003553, -8.660254037844383745, -161.8750000040967905 ) ) ;
#28905 = CARTESIAN_POINT ( 'NONE',  ( 7.644554776091147741E-16, 12.48450537969573659, -2.656250002048344161 ) ) ;
#28906 = CARTESIAN_POINT ( 'NONE',  ( 5.405949406249992428, -9.363379034771808662, -16.59375000204835260 ) ) ;
#28907 = CARTESIAN_POINT ( 'NONE',  ( 10.00000000000038369, -5.773502691896038819, -156.6250000000000284 ) ) ;
#28908 = CARTESIAN_POINT ( 'NONE',  ( -5.405949406250003975, -9.363379034771801557, -112.8437500020483810 ) ) ;
#28909 = CARTESIAN_POINT ( 'NONE',  ( 10.00000000000000000, 5.773502691896255534, -91.87499999999998579 ) ) ;
#28910 = CARTESIAN_POINT ( 'NONE',  ( -10.81189881249999729, 6.242252689847871849, -21.90625000204837391 ) ) ;
#28911 = CARTESIAN_POINT ( 'NONE',  ( 9.999999999999998224, 0.000000000000000000, -95.37500000409677625 ) ) ;
#28912 = CYLINDRICAL_SURFACE ( 'NONE', #2440, 9.999999999999998224 ) ;
#28913 = CARTESIAN_POINT ( 'NONE',  ( 7.644554776091147741E-16, 12.48450537969573659, -116.6562500020483952 ) ) ;
#28914 = CARTESIAN_POINT ( 'NONE',  ( 7.644554776091147741E-16, 12.48450537969573659, -92.65625000204838102 ) ) ;
#28915 = ORIENTED_EDGE ( 'NONE', *, *, #14492, .F. ) ;
#28916 = CARTESIAN_POINT ( 'NONE',  ( 7.070501591499377789E-16, 11.54700538379251284, -92.00000000409677625 ) ) ;
#28917 = CARTESIAN_POINT ( 'NONE',  ( 0.000000000000000000, 0.000000000000000000, -203.0000000000000000 ) ) ;
#28918 = CARTESIAN_POINT ( 'NONE',  ( 10.81189881249999729, 0.000000000000000000, -49.34375000204838102 ) ) ;
#28919 = ORIENTED_EDGE ( 'NONE', *, *, #8901, .F. ) ;
#28920 = CARTESIAN_POINT ( 'NONE',  ( 4.999999999999992006, -8.660254037844389075, -17.24999999999996092 ) ) ;
#28921 = AXIS2_PLACEMENT_3D ( 'NONE', #28433, #41127, #31453 ) ;
#28922 = CARTESIAN_POINT ( 'NONE',  ( -2.293366432827344421E-15, -12.48450537969573659, -22.90625000204837391 ) ) ;
#28923 = CARTESIAN_POINT ( 'NONE',  ( 7.070501591499377789E-16, 11.54700538379251284, -150.1250000000000000 ) ) ;
#28924 = CARTESIAN_POINT ( 'NONE',  ( 9.999999999999998224, 0.000000000000000000, -23.37500000409675849 ) ) ;
#28925 = AXIS2_PLACEMENT_3D ( 'NONE', #39323, #22514, #16857 ) ;
#28926 = EDGE_CURVE ( 'NONE', #21693, #17213, #29094, .T. ) ;
#28928 = EDGE_LOOP ( 'NONE', ( #12134, #39782, #16521, #30756 ) ) ;
#28927 = CARTESIAN_POINT ( 'NONE',  ( 7.644554776091147741E-16, 12.48450537969573659, -124.1562500020483952 ) ) ;
#28929 = CARTESIAN_POINT ( 'NONE',  ( 7.070501591499376803E-16, 11.54700538379251284, -90.12500000000000000 ) ) ;
#28930 = EDGE_LOOP ( 'NONE', ( #26307, #10453, #7022, #34934 ) ) ;
#28931 =( BOUNDED_CURVE ( )  B_SPLINE_CURVE ( 2, ( #23026, #28877, #13068, #22597, #16092, #32329, #39205 ),
 .UNSPECIFIED., .F., .F. ) 
 B_SPLINE_CURVE_WITH_KNOTS ( ( 3, 2, 2, 3 ),
 ( 0.5074626865671643117, 0.5087064676616916969, 0.5099502487562189712, 0.5111940298507463565 ),
 .UNSPECIFIED. ) 
 CURVE ( )  GEOMETRIC_REPRESENTATION_ITEM ( )  RATIONAL_B_SPLINE_CURVE ( ( 0.9999999999999880096, 0.8660254037844506980, 1.000000000000000000, 0.8660254037844387076, 1.000000000000000000, 0.8660254037844267172, 1.000000000000011990 ) ) 
 REPRESENTATION_ITEM ( '' )  );
#28932 = CARTESIAN_POINT ( 'NONE',  ( -5.405949406249996869, 9.363379034771805109, -53.53125000204836681 ) ) ;
#28933 = APPROVAL_ROLE ( '' ) ;
#28934 = CARTESIAN_POINT ( 'NONE',  ( 7.644554776091147741E-16, 12.48450537969573659, -105.9687500020483668 ) ) ;
#28936 = ORIENTED_EDGE ( 'NONE', *, *, #19100, .F. ) ;
#28935 = ORIENTED_EDGE ( 'NONE', *, *, #19755, .F. ) ;
#28937 = DIRECTION ( 'NONE',  ( 1.000000000000000000, 0.000000000000000000, 0.000000000000000000 ) ) ;
#28938 = CARTESIAN_POINT ( 'NONE',  ( -5.000000000000003553, -8.660254037844383745, -184.0000000000000000 ) ) ;
#28939 = CARTESIAN_POINT ( 'NONE',  ( 5.405949406249999534, 9.363379034771803333, -151.0937500020483810 ) ) ;
#28940 = CARTESIAN_POINT ( 'NONE',  ( 10.81189881249999729, 0.000000000000000000, -184.5312500020484094 ) ) ;
#28941 = CARTESIAN_POINT ( 'NONE',  ( -10.81189881249999729, 1.324075727343319199E-15, -3.593750002048368142 ) ) ;
#28942 = CARTESIAN_POINT ( 'NONE',  ( -9.999999999999227285, -5.773502691896698735, -133.1249999999999716 ) ) ;
#28943 = CARTESIAN_POINT ( 'NONE',  ( 5.405949406249992428, -9.363379034771808662, -139.5937500020483810 ) ) ;
#28944 = CARTESIAN_POINT ( 'NONE',  ( 5.405949406249992428, -9.363379034771808662, -105.0937500020483810 ) ) ;
#28945 = CARTESIAN_POINT ( 'NONE',  ( 10.00000000000025402, -5.773502691896113426, -158.1250000000000284 ) ) ;
#28946 = CARTESIAN_POINT ( 'NONE',  ( 10.81189881249999907, 6.242252689847868297, -118.4062500020484094 ) ) ;
#28947 = CARTESIAN_POINT ( 'NONE',  ( 5.000000000000000000, 8.660254037844385522, -191.1250000040967905 ) ) ;
#28948 = CARTESIAN_POINT ( 'NONE',  ( -2.293366432827344421E-15, -12.48450537969573659, -120.2187500020483952 ) ) ;
#28949 = CARTESIAN_POINT ( 'NONE',  ( -10.81189881249999729, 6.242252689847871849, -195.9062500020484094 ) ) ;
#28950 = FACE_OUTER_BOUND ( 'NONE', #22443, .T. ) ;
#28951 = CARTESIAN_POINT ( 'NONE',  ( -2.121150477449813534E-15, -11.54700538379251284, -140.3750000000000000 ) ) ;
#28952 = CARTESIAN_POINT ( 'NONE',  ( -9.999999999999998224, 5.773502691896259087, -10.37499999999996803 ) ) ;
#28953 = CARTESIAN_POINT ( 'NONE',  ( -5.405949406250003975, -9.363379034771801557, -64.84375000204836681 ) ) ;
#28954 = CARTESIAN_POINT ( 'NONE',  ( -10.81189881249999729, 1.324075727343319199E-15, -53.09375000204835970 ) ) ;
#28955 = CARTESIAN_POINT ( 'NONE',  ( -2.121150477449813534E-15, -11.54700538379251284, -190.2500000040967905 ) ) ;
#28956 = CARTESIAN_POINT ( 'NONE',  ( -2.293366432827344421E-15, -12.48450537969573659, -24.40625000204838457 ) ) ;
#28957 = CARTESIAN_POINT ( 'NONE',  ( 10.81189881249999729, 0.000000000000000000, -38.84375000204837391 ) ) ;
#28958 = CARTESIAN_POINT ( 'NONE',  ( -5.000000000000003553, -8.660254037844383745, -8.499999999999952038 ) ) ;
#28959 = CARTESIAN_POINT ( 'NONE',  ( -10.81189881249999729, 1.324075727343319199E-15, -146.0937500020483810 ) ) ;
#28960 = CARTESIAN_POINT ( 'NONE',  ( 7.070501591499377789E-16, 11.54700538379251284, -115.6249999999999858 ) ) ;
#28961 = CARTESIAN_POINT ( 'NONE',  ( -9.999999999999998224, 5.773502691896259087, -65.87499999999998579 ) ) ;
#28962 = CARTESIAN_POINT ( 'NONE',  ( -2.293366432827344421E-15, -12.48450537969573659, -138.4062500020483810 ) ) ;
#28963 = CARTESIAN_POINT ( 'NONE',  ( 5.405949406249999534, 9.363379034771803333, -115.2812500020483952 ) ) ;
#28964 = ORIENTED_EDGE ( 'NONE', *, *, #42062, .T. ) ;
#28965 = DIRECTION ( 'NONE',  ( -0.000000000000000000, -0.000000000000000000, 1.000000000000000000 ) ) ;
#28966 = CARTESIAN_POINT ( 'NONE',  ( 9.999999999999996447, -5.773502691896262640, -116.5000000040967763 ) ) ;
#28967 = DIRECTION ( 'NONE',  ( 1.734723475976807094E-16, 1.000000000000000000, 0.000000000000000000 ) ) ;
#28968 = CARTESIAN_POINT ( 'NONE',  ( 5.405949406249992428, -9.363379034771808662, -70.59375000204836681 ) ) ;
#28969 = CARTESIAN_POINT ( 'NONE',  ( 5.000000000000000000, 8.660254037844385522, -37.74999999999997868 ) ) ;
#28970 = CARTESIAN_POINT ( 'NONE',  ( 9.999999999999996447, -5.773502691896262640, -28.00000000409678336 ) ) ;
#28971 = CARTESIAN_POINT ( 'NONE',  ( -5.405949406250003975, -9.363379034771801557, -50.03125000204838813 ) ) ;
#28972 = CARTESIAN_POINT ( 'NONE',  ( 10.81189881249999551, -6.242252689847874514, -33.15625000204835970 ) ) ;
#28973 = EDGE_CURVE ( 'NONE', #3228, #35088, #38374, .T. ) ;
#28974 = CARTESIAN_POINT ( 'NONE',  ( -9.999999999999227285, -5.773502691896698735, -139.1249999999999716 ) ) ;
#28975 = CARTESIAN_POINT ( 'NONE',  ( -10.81189881249999907, -6.242252689847864744, -143.1562500020484094 ) ) ;
#28976 = AXIS2_PLACEMENT_3D ( 'NONE', #29499, #42010, #32739 ) ;
#28977 = CARTESIAN_POINT ( 'NONE',  ( 10.81189881249999729, 0.000000000000000000, -148.5312500020483810 ) ) ;
#28978 = CARTESIAN_POINT ( 'NONE',  ( -10.00000000000019185, 5.773502691896147176, -190.3750000000000284 ) ) ;
#28979 = DIRECTION ( 'NONE',  ( 0.08715574274765837404, 0.000000000000000000, -0.9961946980917455452 ) ) ;
#28980 = EDGE_LOOP ( 'NONE', ( #27909, #19287, #166, #20775 ) ) ;
#28981 = ORIENTED_EDGE ( 'NONE', *, *, #25637, .T. ) ;
#28982 = VERTEX_POINT ( 'NONE', #25020 ) ;
#28983 = ADVANCED_FACE ( 'NONE', ( #6003 ), #31705, .T. ) ;
#28984 = CYLINDRICAL_SURFACE ( 'NONE', #13174, 9.999999999999998224 ) ;
#28985 = CARTESIAN_POINT ( 'NONE',  ( 5.405949406249999534, 9.363379034771803333, -182.5937500020483810 ) ) ;
#28986 = CARTESIAN_POINT ( 'NONE',  ( -10.81189881249999729, 6.242252689847871849, -27.71875000204838102 ) ) ;
#28987 = DIRECTION ( 'NONE',  ( 1.000000000000000000, 0.000000000000000000, 0.000000000000000000 ) ) ;
#28988 = CARTESIAN_POINT ( 'NONE',  ( -10.81189881249999729, 1.324075727343319199E-15, -165.5937500020484094 ) ) ;
#28989 = CARTESIAN_POINT ( 'NONE',  ( 10.81189881249999551, -6.242252689847874514, -143.9687500020483810 ) ) ;
#28990 = CARTESIAN_POINT ( 'NONE',  ( 9.999999999999998224, 0.000000000000000000, -125.3750000040967905 ) ) ;
#28991 = CARTESIAN_POINT ( 'NONE',  ( -10.81189881249999907, -6.242252689847864744, -130.9687500020483810 ) ) ;
#28992 = CARTESIAN_POINT ( 'NONE',  ( 5.405949406249992428, -9.363379034771808662, -142.7812500020483810 ) ) ;
#28993 = CARTESIAN_POINT ( 'NONE',  ( 5.405949406249992428, -9.363379034771808662, -19.59375000204835615 ) ) ;
#28994 = CARTESIAN_POINT ( 'NONE',  ( 7.644554776091147741E-16, 12.48450537969573659, -149.4687500020484663 ) ) ;
#28995 = CARTESIAN_POINT ( 'NONE',  ( -4.999999999999996447, 8.660254037844387298, -135.0000000000000000 ) ) ;
#28996 = CARTESIAN_POINT ( 'NONE',  ( -9.999999999999998224, 0.000000000000000000, -99.99999999999998579 ) ) ;
#28997 = CARTESIAN_POINT ( 'NONE',  ( -2.121150477449813534E-15, -11.54700538379251284, -164.3750000000000000 ) ) ;
#28998 = CARTESIAN_POINT ( 'NONE',  ( 10.81189881249999551, -6.242252689847874514, -80.96875000204838102 ) ) ;
#28999 = CARTESIAN_POINT ( 'NONE',  ( -5.405949406250003975, -9.363379034771801557, -50.03125000204838813 ) ) ;
#29000 = CARTESIAN_POINT ( 'NONE',  ( 5.405949406249992428, -9.363379034771808662, -64.59375000204836681 ) ) ;
#29001 = CARTESIAN_POINT ( 'NONE',  ( -9.999999999999998224, 1.224646799147353059E-15, -90.12500000409677625 ) ) ;
#29002 = CARTESIAN_POINT ( 'NONE',  ( -10.81189881249999907, -6.242252689847864744, -168.4687500020483526 ) ) ;
#29003 = VECTOR ( 'NONE', #12332, 1000.000000000000114 ) ;
#29004 = CARTESIAN_POINT ( 'NONE',  ( -2.121150477449813534E-15, -11.54700538379251284, -134.3750000000000000 ) ) ;
#29005 = CARTESIAN_POINT ( 'NONE',  ( 10.81189881249999729, 0.000000000000000000, -145.5312500020483810 ) ) ;
#29006 = LINE ( 'NONE', #5709, #28243 ) ;
#29007 = CARTESIAN_POINT ( 'NONE',  ( 7.070501591499377789E-16, 11.54700538379251284, -119.0000000040967763 ) ) ;
#29008 = CARTESIAN_POINT ( 'NONE',  ( -9.999999999999998224, 1.224646799147353059E-15, -94.24999999999998579 ) ) ;
#29009 = ORIENTED_EDGE ( 'NONE', *, *, #38610, .T. ) ;
#29010 = CARTESIAN_POINT ( 'NONE',  ( -10.81189881249999729, -6.242252689847864744, -117.6562500020483952 ) ) ;
#29011 = CARTESIAN_POINT ( 'NONE',  ( -4.999999999999996447, 8.660254037844387298, -142.8750000040967905 ) ) ;
#29012 = CARTESIAN_POINT ( 'NONE',  ( 9.999999999999998224, 0.000000000000000000, -158.0000000000000000 ) ) ;
#29013 = ADVANCED_FACE ( 'NONE', ( #32340 ), #41807, .T. ) ;
#29014 = CARTESIAN_POINT ( 'NONE',  ( 5.405949406249992428, -9.363379034771808662, -171.2812500020484094 ) ) ;
#29015 = CARTESIAN_POINT ( 'NONE',  ( -9.999999999999998224, 5.773502691896259087, -49.75000000409675494 ) ) ;
#29016 =( BOUNDED_CURVE ( )  B_SPLINE_CURVE ( 2, ( #29418, #3729, #26600, #13196, #16859, #6745, #42346 ),
 .UNSPECIFIED., .F., .F. ) 
 B_SPLINE_CURVE_WITH_KNOTS ( ( 3, 2, 2, 3 ),
 ( 0.7089552238805972850, 0.7101990049751245593, 0.7114427860696519446, 0.7126865671641793298 ),
 .UNSPECIFIED. ) 
 CURVE ( )  GEOMETRIC_REPRESENTATION_ITEM ( )  RATIONAL_B_SPLINE_CURVE ( ( 0.9999999999999761302, 0.8660254037844625774, 1.000000000000000000, 0.8660254037844387076, 1.000000000000000000, 0.8660254037844148378, 1.000000000000023981 ) ) 
 REPRESENTATION_ITEM ( '' )  );
#29017 = LINE ( 'NONE', #19279, #21465 ) ;
#29018 = CARTESIAN_POINT ( 'NONE',  ( -5.405949406249996869, 9.363379034771805109, -61.03125000204837391 ) ) ;
#29019 = ADVANCED_FACE ( 'NONE', ( #8812 ), #19151, .T. ) ;
#29020 = CARTESIAN_POINT ( 'NONE',  ( 10.81189881249999551, -6.242252689847874514, -166.6562500020484094 ) ) ;
#29021 = CARTESIAN_POINT ( 'NONE',  ( -9.999999999999998224, 1.224646799147353059E-15, -183.1250000040967905 ) ) ;
#29022 = CARTESIAN_POINT ( 'NONE',  ( 9.999999999999998224, 0.000000000000000000, -188.3750000040967905 ) ) ;
#29023 = ORIENTED_EDGE ( 'NONE', *, *, #9068, .T. ) ;
#29024 = PLANE ( 'NONE',  #27274 ) ;
#29025 = DIRECTION ( 'NONE',  ( 0.000000000000000000, 0.000000000000000000, 1.000000000000000000 ) ) ;
#29026 =( GEOMETRIC_REPRESENTATION_CONTEXT ( 3 ) GLOBAL_UNCERTAINTY_ASSIGNED_CONTEXT ( ( #6998 ) ) GLOBAL_UNIT_ASSIGNED_CONTEXT ( ( #1003, #30782, #40672 ) ) REPRESENTATION_CONTEXT ( 'NONE', 'WORKASPACE' ) );
#29028 = ORIENTED_EDGE ( 'NONE', *, *, #40673, .T. ) ;
#29027 = CARTESIAN_POINT ( 'NONE',  ( 5.405949406249992428, -9.363379034771808662, -78.28125000204838102 ) ) ;
#29029 = DIRECTION ( 'NONE',  ( 0.000000000000000000, 0.000000000000000000, 1.000000000000000000 ) ) ;
#29031 = EDGE_LOOP ( 'NONE', ( #34559, #24898, #253, #18427 ) ) ;
#29030 = CARTESIAN_POINT ( 'NONE',  ( -9.999999999999479527, -5.773502691896549521, -119.6249999999999858 ) ) ;
#29032 = ORIENTED_EDGE ( 'NONE', *, *, #38372, .F. ) ;
#29033 = CARTESIAN_POINT ( 'NONE',  ( -10.81189881249999729, -6.242252689847864744, -30.46875000204834549 ) ) ;
#29034 = CARTESIAN_POINT ( 'NONE',  ( 5.000000000000000000, 8.660254037844385522, -126.6250000040967620 ) ) ;
#29035 = CARTESIAN_POINT ( 'NONE',  ( -10.81189881249999729, 1.324075727343319199E-15, -5.281250002048376579 ) ) ;
#29037 = ORIENTED_EDGE ( 'NONE', *, *, #5674, .T. ) ;
#29036 = CARTESIAN_POINT ( 'NONE',  ( 10.81189881249999729, 0.000000000000000000, -52.34375000204835260 ) ) ;
#29038 = DIRECTION ( 'NONE',  ( 1.000000000000000000, 0.000000000000000000, 0.000000000000000000 ) ) ;
#29039 = EDGE_CURVE ( 'NONE', #14564, #10480, #26530, .T. ) ;
#29040 = CARTESIAN_POINT ( 'NONE',  ( 4.999999999999992006, -8.660254037844389075, -32.24999999999997158 ) ) ;
#29041 = CARTESIAN_POINT ( 'NONE',  ( 10.81189881249999551, -6.242252689847874514, -191.9687500020484379 ) ) ;
#29042 = CARTESIAN_POINT ( 'NONE',  ( 5.405949406249992428, -9.363379034771808662, -175.5937500020484094 ) ) ;
#29043 = CARTESIAN_POINT ( 'NONE',  ( 10.81189881249999729, 0.000000000000000000, -160.3437500020484094 ) ) ;
#29044 = CARTESIAN_POINT ( 'NONE',  ( -10.81189881249999729, -6.242252689847864744, -169.9687500020483526 ) ) ;
#29045 = CARTESIAN_POINT ( 'NONE',  ( 9.999999999999998224, 0.000000000000000000, -153.5000000000000000 ) ) ;
#29046 = CARTESIAN_POINT ( 'NONE',  ( -2.121150477449813534E-15, -11.54700538379251284, -126.8749999999999858 ) ) ;
#29047 = CARTESIAN_POINT ( 'NONE',  ( 4.999999999999992006, -8.660254037844389075, -183.7500000000000000 ) ) ;
#29048 = CARTESIAN_POINT ( 'NONE',  ( 5.405949406249999534, 9.363379034771803333, -107.5937500020483810 ) ) ;
#29049 = DIRECTION ( 'NONE',  ( -0.000000000000000000, -0.000000000000000000, 1.000000000000000000 ) ) ;
#29050 = CARTESIAN_POINT ( 'NONE',  ( 10.81189881249999551, -6.242252689847874514, -73.65625000204836681 ) ) ;
#29051 = CARTESIAN_POINT ( 'NONE',  ( 9.999999999999998224, 1.224646799147353059E-15, -99.99999999999998579 ) ) ;
#29052 = CARTESIAN_POINT ( 'NONE',  ( 5.405949406249992428, -9.363379034771808662, -84.09375000204836681 ) ) ;
#29053 = CARTESIAN_POINT ( 'NONE',  ( 7.644554776091147741E-16, 12.48450537969573659, -59.65625000204838102 ) ) ;
#29054 = CARTESIAN_POINT ( 'NONE',  ( -4.999999999999996447, 8.660254037844387298, -148.8750000040967905 ) ) ;
#29055 = CARTESIAN_POINT ( 'NONE',  ( -5.000000000000003553, -8.660254037844383745, -124.0000000000000000 ) ) ;
#29056 =( BOUNDED_CURVE ( )  B_SPLINE_CURVE ( 2, ( #38109, #15839, #9388, #18243, #12397, #15630, #21703 ),
 .UNSPECIFIED., .F., .F. ) 
 B_SPLINE_CURVE_WITH_KNOTS ( ( 3, 2, 2, 3 ),
 ( 0.4440298507462688282, 0.4452736318407962135, 0.4465174129353234878, 0.4477611940298508730 ),
 .UNSPECIFIED. ) 
 CURVE ( )  GEOMETRIC_REPRESENTATION_ITEM ( )  RATIONAL_B_SPLINE_CURVE ( ( 0.9999999999999820144, 0.8660254037844566932, 1.000000000000000000, 0.8660254037844387076, 1.000000000000000000, 0.8660254037844267172, 1.000000000000011990 ) ) 
 REPRESENTATION_ITEM ( '' )  );
#29057 = VERTEX_POINT ( 'NONE', #9444 ) ;
#29058 = CARTESIAN_POINT ( 'NONE',  ( 7.644554776091147741E-16, 12.48450537969573659, -139.1562500020484094 ) ) ;
#29059 = CARTESIAN_POINT ( 'NONE',  ( 10.81189881249999551, -6.242252689847874514, -154.6562500020484379 ) ) ;
#29060 = LOCAL_TIME ( 11, 57, 6.000000000000000000, #17643 ) ;
#29061 = CARTESIAN_POINT ( 'NONE',  ( 5.405949406249992428, -9.363379034771808662, -195.2812500020484094 ) ) ;
#29062 = CARTESIAN_POINT ( 'NONE',  ( -9.999999999999998224, 1.224646799147353059E-15, -179.7500000000000284 ) ) ;
#29063 = CARTESIAN_POINT ( 'NONE',  ( -2.293366432827344421E-15, -12.48450537969573659, -93.21875000204838102 ) ) ;
#29064 = ORIENTED_EDGE ( 'NONE', *, *, #3276, .F. ) ;
#29065 = CARTESIAN_POINT ( 'NONE',  ( -10.00000000000000000, -5.773502691896251982, -68.62499999999998579 ) ) ;
#29066 = CARTESIAN_POINT ( 'NONE',  ( 10.81189881249999907, 6.242252689847868297, -185.7187500020483810 ) ) ;
#29067 = CARTESIAN_POINT ( 'NONE',  ( 7.070501591499377789E-16, 11.54700538379251284, -71.00000000409676204 ) ) ;
#29068 = CARTESIAN_POINT ( 'NONE',  ( 8.660254037844463681, -15.00000000000009948, 49.99999999999998579 ) ) ;
#29069 = DIRECTION ( 'NONE',  ( 1.000000000000000000, 0.000000000000000000, 0.000000000000000000 ) ) ;
#29070 = CARTESIAN_POINT ( 'NONE',  ( -10.81189881249999729, 6.242252689847871849, -86.40625000204836681 ) ) ;
#29071 = CARTESIAN_POINT ( 'NONE',  ( 5.405949406249992428, -9.363379034771808662, -67.78125000204838102 ) ) ;
#29072 = CARTESIAN_POINT ( 'NONE',  ( -5.000000000000003553, -8.660254037844383745, -58.37500000409676204 ) ) ;
#29073 = CARTESIAN_POINT ( 'NONE',  ( -10.81189881249999729, 6.242252689847871849, -14.21875000204836326 ) ) ;
#29074 = ORIENTED_EDGE ( 'NONE', *, *, #26750, .F. ) ;
#29075 = CARTESIAN_POINT ( 'NONE',  ( 5.405949406249999534, 9.363379034771803333, -196.2812500020484094 ) ) ;
#29076 = AXIS2_PLACEMENT_3D ( 'NONE', #30041, #9749, #39102 ) ;
#29077 = CARTESIAN_POINT ( 'NONE',  ( 5.405949406249992428, -9.363379034771808662, -15.28125000204835793 ) ) ;
#29078 = CARTESIAN_POINT ( 'NONE',  ( 10.81189881249999729, 0.000000000000000000, -7.343750002048343717 ) ) ;
#29079 = CARTESIAN_POINT ( 'NONE',  ( 0.000000000000000000, 0.000000000000000000, -200.0000000000000000 ) ) ;
#29080 = DIRECTION ( 'NONE',  ( -0.000000000000000000, -0.000000000000000000, 1.000000000000000000 ) ) ;
#29081 = CARTESIAN_POINT ( 'NONE',  ( -9.999999999999227285, -5.773502691896698735, -137.6249999999999716 ) ) ;
#29082 = CARTESIAN_POINT ( 'NONE',  ( -2.121150477449813534E-15, -11.54700538379251284, -174.8750000000000000 ) ) ;
#29083 = LINE ( 'NONE', #9641, #17911 ) ;
#29085 = ORIENTED_EDGE ( 'NONE', *, *, #16511, .T. ) ;
#29084 = CARTESIAN_POINT ( 'NONE',  ( 10.81189881249999907, 6.242252689847868297, -100.4062500020483952 ) ) ;
#29086 = CARTESIAN_POINT ( 'NONE',  ( -2.121150477449813534E-15, -11.54700538379251284, -179.7500000040967905 ) ) ;
#29087 = VERTEX_POINT ( 'NONE', #15891 ) ;
#29088 = ORIENTED_EDGE ( 'NONE', *, *, #7502, .T. ) ;
#29089 = CONICAL_SURFACE ( 'NONE', #841, 22.00000000000000711, 0.7853981633974466137 ) ;
#29090 = CARTESIAN_POINT ( 'NONE',  ( 10.81189881249999729, 0.000000000000000000, -30.03125000204837036 ) ) ;
#29091 = APPROVAL_DATE_TIME ( #15267, #23300 ) ;
#29092 = EDGE_CURVE ( 'NONE', #32177, #3335, #42233, .T. ) ;
#29093 = CARTESIAN_POINT ( 'NONE',  ( 5.405949406249992428, -9.363379034771808662, -79.59375000204838102 ) ) ;
#29094 = LINE ( 'NONE', #11819, #2926 ) ;
#29095 = EDGE_CURVE ( 'NONE', #30038, #26823, #28888, .T. ) ;
#29096 = CARTESIAN_POINT ( 'NONE',  ( 5.405949406249999534, 9.363379034771803333, -199.0937500020484094 ) ) ;
#29097 = EDGE_CURVE ( 'NONE', #3542, #18815, #31873, .T. ) ;
#29098 = CARTESIAN_POINT ( 'NONE',  ( -4.999999999999996447, 8.660254037844387298, -69.37500000409677625 ) ) ;
#29099 = DIRECTION ( 'NONE',  ( 1.000000000000000000, 0.000000000000000000, 0.000000000000000000 ) ) ;
#29100 = CARTESIAN_POINT ( 'NONE',  ( 5.405949406249992428, -9.363379034771808662, -157.7812500020484094 ) ) ;
#29101 = CARTESIAN_POINT ( 'NONE',  ( -5.000000000000003553, -8.660254037844383745, -14.87500000409674961 ) ) ;
#29102 = VECTOR ( 'NONE', #33111, 1000.000000000000000 ) ;
#29103 = CARTESIAN_POINT ( 'NONE',  ( 9.999999999999998224, 0.000000000000000000, -126.5000000000000000 ) ) ;
#29104 = CARTESIAN_POINT ( 'NONE',  ( -10.81189881249999907, -6.242252689847864744, -126.4687500020483810 ) ) ;
#29105 = CARTESIAN_POINT ( 'NONE',  ( 10.81189881249999729, 0.000000000000000000, -96.03125000204838102 ) ) ;
#29106 = CARTESIAN_POINT ( 'NONE',  ( 5.405949406249992428, -9.363379034771808662, -109.5937500020483810 ) ) ;
#29107 = CARTESIAN_POINT ( 'NONE',  ( 10.81189881249999729, 0.000000000000000000, -79.34375000204838102 ) ) ;
#29108 = CARTESIAN_POINT ( 'NONE',  ( -10.81189881249999729, 1.324075727343319199E-15, -86.28125000204838102 ) ) ;
#29109 = CARTESIAN_POINT ( 'NONE',  ( 4.999999999999992006, -8.660254037844389075, -166.1250000040967905 ) ) ;
#29110 = CARTESIAN_POINT ( 'NONE',  ( 9.999999999998969713, 5.773502691896851502, -81.75000000409673362 ) ) ;
#29111 = CARTESIAN_POINT ( 'NONE',  ( -5.405949406250003975, -9.363379034771801557, -167.0312500020484094 ) ) ;
#29112 = CARTESIAN_POINT ( 'NONE',  ( 10.81189881249999729, 0.000000000000000000, -183.0312500020484094 ) ) ;
#29113 = CARTESIAN_POINT ( 'NONE',  ( 4.999999999999992006, -8.660254037844389075, -160.1250000040967905 ) ) ;
#29114 = CARTESIAN_POINT ( 'NONE',  ( 9.999999999998969713, 5.773502691896851502, -86.25000000409676204 ) ) ;
#29115 = CARTESIAN_POINT ( 'NONE',  ( -5.405949406249996869, 9.363379034771805109, -2.343750002048366810 ) ) ;
#29116 = CARTESIAN_POINT ( 'NONE',  ( -4.999999999999996447, 8.660254037844387298, -162.3750000040967905 ) ) ;
#29117 = CARTESIAN_POINT ( 'NONE',  ( -2.293366432827344421E-15, -12.48450537969573659, -115.7187500020483952 ) ) ;
#29118 = CARTESIAN_POINT ( 'NONE',  ( -10.00000000000000000, -5.773502691896251982, -89.62499999999997158 ) ) ;
#29119 = CARTESIAN_POINT ( 'NONE',  ( 7.644554776091147741E-16, 12.48450537969573659, -16.15625000204837391 ) ) ;
#29120 = CARTESIAN_POINT ( 'NONE',  ( -5.000000000000003553, -8.660254037844383745, -101.8750000040967905 ) ) ;
#29121 = EDGE_CURVE ( 'NONE', #223, #516, #20807, .T. ) ;
#29122 = CARTESIAN_POINT ( 'NONE',  ( -5.000000000000003553, -8.660254037844383745, -170.8750000040968189 ) ) ;
#29123 = CARTESIAN_POINT ( 'NONE',  ( -2.293366432827344421E-15, -12.48450537969573659, -109.9062500020483952 ) ) ;
#29124 = CARTESIAN_POINT ( 'NONE',  ( -2.293366432827344421E-15, -12.48450537969573659, -91.90625000204838102 ) ) ;
#29125 = ORIENTED_EDGE ( 'NONE', *, *, #2743, .T. ) ;
#29126 = CARTESIAN_POINT ( 'NONE',  ( 10.00000000000000000, 5.773502691896255534, -83.25000000409677625 ) ) ;
#29127 = CARTESIAN_POINT ( 'NONE',  ( -2.121150477449813534E-15, -11.54700538379251284, -101.3750000000000000 ) ) ;
#29128 = CARTESIAN_POINT ( 'NONE',  ( -5.405949406250003975, -9.363379034771801557, -43.84375000204837391 ) ) ;
#29129 = ORIENTED_EDGE ( 'NONE', *, *, #31759, .F. ) ;
#29130 = CARTESIAN_POINT ( 'NONE',  ( -9.999999999999998224, 5.773502691896259087, -19.37499999999998224 ) ) ;
#29131 = CARTESIAN_POINT ( 'NONE',  ( -2.121150477449813534E-15, -11.54700538379251284, -155.3750000000000000 ) ) ;
#29132 = EDGE_CURVE ( 'NONE', #10904, #10629, #22375, .T. ) ;
#29133 = CARTESIAN_POINT ( 'NONE',  ( -4.999999999999996447, 8.660254037844387298, -19.87500000409675494 ) ) ;
#29134 = CYLINDRICAL_SURFACE ( 'NONE', #33235, 35.00000000000000711 ) ;
#29136 = ORIENTED_EDGE ( 'NONE', *, *, #33578, .T. ) ;
#29135 = CARTESIAN_POINT ( 'NONE',  ( 10.81189881249999551, -6.242252689847874514, -126.1562500020483810 ) ) ;
#29137 = ORIENTED_EDGE ( 'NONE', *, *, #42633, .T. ) ;
#29138 = CARTESIAN_POINT ( 'NONE',  ( -5.405949406250003975, -9.363379034771801557, -50.03125000204838813 ) ) ;
#29139 = DATE_AND_TIME ( #2811, #38691 ) ;
#29140 = CARTESIAN_POINT ( 'NONE',  ( 10.81189881249999551, -6.242252689847874514, -100.4687500020483952 ) ) ;
#29142 = ORIENTED_EDGE ( 'NONE', *, *, #889, .T. ) ;
#29141 = ORIENTED_EDGE ( 'NONE', *, *, #9126, .F. ) ;
#29143 = LINE ( 'NONE', #25491, #23176 ) ;
#29144 = CARTESIAN_POINT ( 'NONE',  ( -9.999999999999998224, 1.224646799147353059E-15, -32.74999999999997158 ) ) ;
#29145 = EDGE_CURVE ( 'NONE', #1637, #8492, #5789, .T. ) ;
#29146 = CARTESIAN_POINT ( 'NONE',  ( 10.81189881249999907, 6.242252689847868297, -181.4062500020484379 ) ) ;
#29147 = CARTESIAN_POINT ( 'NONE',  ( 9.999999999999998224, 0.000000000000000000, -200.0000000000000000 ) ) ;
#29148 = FACE_OUTER_BOUND ( 'NONE', #13742, .T. ) ;
#29149 = EDGE_CURVE ( 'NONE', #36438, #40511, #2976, .T. ) ;
#29150 = CARTESIAN_POINT ( 'NONE',  ( 10.81189881249999551, -6.242252689847874514, -142.4687500020483810 ) ) ;
#29151 = CARTESIAN_POINT ( 'NONE',  ( -5.405949406250003975, -9.363379034771801557, -97.84375000204838102 ) ) ;
#29152 = CARTESIAN_POINT ( 'NONE',  ( -5.000000000000003553, -8.660254037844383745, -143.5000000000000000 ) ) ;
#29153 = CARTESIAN_POINT ( 'NONE',  ( -2.293366432827344421E-15, -12.48450537969573659, -106.9062500020483952 ) ) ;
#29154 = CARTESIAN_POINT ( 'NONE',  ( 9.999999999999996447, -5.773502691896262640, -193.0000000040968473 ) ) ;
#29155 = CARTESIAN_POINT ( 'NONE',  ( -10.81189881249999729, 1.324075727343319199E-15, -120.5937500020483952 ) ) ;
#29156 = CARTESIAN_POINT ( 'NONE',  ( 10.81189881249999729, 6.242252689847867408, -187.4062500020484094 ) ) ;
#29157 = CARTESIAN_POINT ( 'NONE',  ( -9.999999999999479527, -5.773502691896549521, -47.62499999999995737 ) ) ;
#29158 = CARTESIAN_POINT ( 'NONE',  ( 4.999999999999992006, -8.660254037844389075, -143.2500000000000000 ) ) ;
#29159 = CARTESIAN_POINT ( 'NONE',  ( -9.999999999999998224, 5.773502691896259087, -1.374999999999959588 ) ) ;
#29160 = CARTESIAN_POINT ( 'NONE',  ( 10.81189881249999551, -6.242252689847874514, -65.96875000204836681 ) ) ;
#29161 = CARTESIAN_POINT ( 'NONE',  ( -5.405949406250003975, -9.363379034771801557, -48.34375000204838102 ) ) ;
#29162 = CARTESIAN_POINT ( 'NONE',  ( 10.00000000000000000, 5.773502691896255534, -177.7500000040967905 ) ) ;
#29163 = CARTESIAN_POINT ( 'NONE',  ( -10.81189881249999907, -6.242252689847864744, -29.15625000204835970 ) ) ;
#29164 = CARTESIAN_POINT ( 'NONE',  ( -10.81189881249999729, 6.242252689847871849, -30.71875000204834905 ) ) ;
#29165 = CARTESIAN_POINT ( 'NONE',  ( -9.999999999999479527, -5.773502691896549521, -142.5000000040967620 ) ) ;
#29166 = CARTESIAN_POINT ( 'NONE',  ( -5.405949406249996869, 9.363379034771805109, -141.8437500020483810 ) ) ;
#29167 = CARTESIAN_POINT ( 'NONE',  ( 9.999999999999998224, 0.000000000000000000, -112.9999999999999858 ) ) ;
#29168 = CARTESIAN_POINT ( 'NONE',  ( 9.999999999999998224, 0.000000000000000000, -147.5000000000000000 ) ) ;
#29169 = CARTESIAN_POINT ( 'NONE',  ( -9.999999999999998224, 1.224646799147353059E-15, -65.74999999999997158 ) ) ;
#29170 = CARTESIAN_POINT ( 'NONE',  ( -10.81189881249999729, 6.242252689847871849, -134.4062500020484094 ) ) ;
#29171 = CARTESIAN_POINT ( 'NONE',  ( -10.81189881249999729, 1.324075727343319199E-15, -117.7812500020483952 ) ) ;
#29172 = EDGE_CURVE ( 'NONE', #5198, #37673, #10254, .T. ) ;
#29173 = EDGE_LOOP ( 'NONE', ( #12132, #36868, #5942, #39775 ) ) ;
#29174 = DIRECTION ( 'NONE',  ( 0.000000000000000000, 0.000000000000000000, -1.000000000000000000 ) ) ;
#29175 = CARTESIAN_POINT ( 'NONE',  ( 4.999999999999992006, -8.660254037844389075, -119.6250000040967905 ) ) ;
#29176 = CYLINDRICAL_SURFACE ( 'NONE', #36026, 9.999999999999998224 ) ;
#29177 = CARTESIAN_POINT ( 'NONE',  ( 5.405949406249992428, -9.363379034771808662, -66.09375000204836681 ) ) ;
#29178 = CARTESIAN_POINT ( 'NONE',  ( 9.999999999999996447, -5.773502691896262640, -44.12499999999997158 ) ) ;
#29179 = CARTESIAN_POINT ( 'NONE',  ( 9.999999999999996447, -5.773502691896262640, -25.00000000409676915 ) ) ;
#29180 = CARTESIAN_POINT ( 'NONE',  ( 10.81189881249999729, 6.242252689847867408, -44.90625000204836681 ) ) ;
#29181 = CARTESIAN_POINT ( 'NONE',  ( 4.999999999999992006, -8.660254037844389075, -157.1250000040967905 ) ) ;
#29182 = CARTESIAN_POINT ( 'NONE',  ( -10.00000000000000000, -5.773502691896251982, -48.00000000409676204 ) ) ;
#29183 = CARTESIAN_POINT ( 'NONE',  ( -5.405949406250003975, -9.363379034771801557, -33.53125000204837391 ) ) ;
#29184 =( BOUNDED_CURVE ( )  B_SPLINE_CURVE ( 2, ( #37023, #6611, #13910, #10682, #13488, #7463, #30355 ),
 .UNSPECIFIED., .F., .F. ) 
 B_SPLINE_CURVE_WITH_KNOTS ( ( 3, 2, 2, 3 ),
 ( 0.1902985074626866169, 0.1915422885572139744, 0.1927860696517413319, 0.1940298507462686894 ),
 .UNSPECIFIED. ) 
 CURVE ( )  GEOMETRIC_REPRESENTATION_ITEM ( )  RATIONAL_B_SPLINE_CURVE ( ( 0.9999999999999940048, 0.8660254037844447028, 1.000000000000000000, 0.8660254037844387076, 1.000000000000000000, 0.8660254037844357100, 1.000000000000003109 ) ) 
 REPRESENTATION_ITEM ( '' )  );
#29185 = DIRECTION ( 'NONE',  ( -1.000000000000000000, 0.000000000000000000, 0.000000000000000000 ) ) ;
#29186 = CARTESIAN_POINT ( 'NONE',  ( 10.81189881249999907, 6.242252689847868297, -139.4062500020484094 ) ) ;
#29187 = CARTESIAN_POINT ( 'NONE',  ( -5.405949406250003975, -9.363379034771801557, -147.5312500020483810 ) ) ;
#29188 = CARTESIAN_POINT ( 'NONE',  ( 0.000000000000000000, 0.000000000000000000, -99.99999999999998579 ) ) ;
#29189 = EDGE_LOOP ( 'NONE', ( #29505, #32836 ) ) ;
#29190 = ORIENTED_EDGE ( 'NONE', *, *, #34818, .F. ) ;
#29191 = ORIENTED_EDGE ( 'NONE', *, *, #10587, .T. ) ;
#29192 = CARTESIAN_POINT ( 'NONE',  ( -10.00000000000076916, 5.773502691895813221, -135.2500000040967905 ) ) ;
#29193 = CARTESIAN_POINT ( 'NONE',  ( 10.81189881249999729, 0.000000000000000000, -170.8437500020484094 ) ) ;
#29194 = CARTESIAN_POINT ( 'NONE',  ( -5.405949406249996869, 9.363379034771805109, -29.34375000204836326 ) ) ;
#29195 = CARTESIAN_POINT ( 'NONE',  ( 7.070501591499376803E-16, 11.54700538379251284, -144.5000000040967905 ) ) ;
#29196 = CARTESIAN_POINT ( 'NONE',  ( 10.81189881249999729, 0.000000000000000000, -167.8437500020484094 ) ) ;
#29197 = CARTESIAN_POINT ( 'NONE',  ( -5.405949406250003975, -9.363379034771801557, -147.3437500020483810 ) ) ;
#29198 = CARTESIAN_POINT ( 'NONE',  ( 4.999999999999992006, -8.660254037844389075, -176.2500000000000284 ) ) ;
#29199 = CARTESIAN_POINT ( 'NONE',  ( 5.405949406249992428, -9.363379034771808662, -126.0937500020483668 ) ) ;
#29200 = CARTESIAN_POINT ( 'NONE',  ( 5.405949406249992428, -9.363379034771808662, -133.7812500020483810 ) ) ;
#29201 = CARTESIAN_POINT ( 'NONE',  ( -10.81189881249999907, -6.242252689847864744, -15.46875000204835793 ) ) ;
#29202 = CARTESIAN_POINT ( 'NONE',  ( 10.81189881249999729, 6.242252689847867408, -146.7187500020484094 ) ) ;
#29203 = CARTESIAN_POINT ( 'NONE',  ( 10.26323035265758499, -3.418996386904107787, -180.0000000000000000 ) ) ;
#29204 = CARTESIAN_POINT ( 'NONE',  ( -10.00000000000102496, 5.773502691895664007, -43.75000000409673362 ) ) ;
#29205 = CARTESIAN_POINT ( 'NONE',  ( -9.999999999999998224, 5.773502691896259087, -164.8749999999999716 ) ) ;
#29206 = CARTESIAN_POINT ( 'NONE',  ( 9.999999999999998224, 0.000000000000000000, -16.99999999999996092 ) ) ;
#29207 = EDGE_CURVE ( 'NONE', #3061, #24037, #30943, .T. ) ;
#29208 = CARTESIAN_POINT ( 'NONE',  ( 10.81189881249999729, 0.000000000000000000, -70.34375000204836681 ) ) ;
#29209 = CARTESIAN_POINT ( 'NONE',  ( 10.81189881249999907, 6.242252689847868297, -53.90625000204838102 ) ) ;
#29210 = CARTESIAN_POINT ( 'NONE',  ( 10.81189881249999729, 0.000000000000000000, -62.84375000204836681 ) ) ;
#29211 = CARTESIAN_POINT ( 'NONE',  ( -9.999999999999998224, 1.224646799147353059E-15, -56.74999999999996447 ) ) ;
#29212 = CARTESIAN_POINT ( 'NONE',  ( 10.81189881249999729, 0.000000000000000000, -163.3437500020484094 ) ) ;
#29213 = CARTESIAN_POINT ( 'NONE',  ( 5.000000000000000000, 8.660254037844385522, -138.2499999999999716 ) ) ;
#29214 = CARTESIAN_POINT ( 'NONE',  ( -2.293366432827344421E-15, -12.48450537969573659, -147.4062500020483810 ) ) ;
#29215 = CARTESIAN_POINT ( 'NONE',  ( 9.999999999999998224, 0.000000000000000000, -16.99999999999996092 ) ) ;
#29216 = CARTESIAN_POINT ( 'NONE',  ( -5.000000000000003553, -8.660254037844383745, -113.8750000040967763 ) ) ;
#29217 = CARTESIAN_POINT ( 'NONE',  ( 10.00000000000000000, 5.773502691896255534, -90.37499999999998579 ) ) ;
#29218 = ORIENTED_EDGE ( 'NONE', *, *, #22114, .T. ) ;
#29219 = CARTESIAN_POINT ( 'NONE',  ( -10.81189881249999729, 1.324075727343319199E-15, -122.2812500020483952 ) ) ;
#29220 = CARTESIAN_POINT ( 'NONE',  ( -9.999999999999998224, 5.773502691896259087, -141.2500000040967905 ) ) ;
#29221 = CYLINDRICAL_SURFACE ( 'NONE', #9124, 9.999999999999998224 ) ;
#29222 = CARTESIAN_POINT ( 'NONE',  ( 5.405949406249992428, -9.363379034771808662, -175.7812500020484094 ) ) ;
#29223 = CARTESIAN_POINT ( 'NONE',  ( -5.000000000000003553, -8.660254037844383745, -47.87500000409677625 ) ) ;
#29224 = DIRECTION ( 'NONE',  ( 1.000000000000000000, 0.000000000000000000, 0.000000000000000000 ) ) ;
#29225 = CARTESIAN_POINT ( 'NONE',  ( 7.644554776091147741E-16, 12.48450537969573659, -64.15625000204838102 ) ) ;
#29226 = ADVANCED_FACE ( 'NONE', ( #23036 ), #29296, .T. ) ;
#29227 = CARTESIAN_POINT ( 'NONE',  ( -9.999999999999998224, 0.000000000000000000, -99.99999999999998579 ) ) ;
#29228 = CARTESIAN_POINT ( 'NONE',  ( -10.81189881249999729, 1.324075727343319199E-15, -158.2812500020484094 ) ) ;
#29229 = CARTESIAN_POINT ( 'NONE',  ( -2.293366432827344421E-15, -12.48450537969573659, -144.2187500020483810 ) ) ;
#29230 = DIRECTION ( 'NONE',  ( -0.000000000000000000, -0.000000000000000000, 1.000000000000000000 ) ) ;
#29231 = ORIENTED_EDGE ( 'NONE', *, *, #16931, .F. ) ;
#29232 = CYLINDRICAL_SURFACE ( 'NONE', #34172, 9.999999999999998224 ) ;
#29234 = ORIENTED_EDGE ( 'NONE', *, *, #10620, .F. ) ;
#29233 = CARTESIAN_POINT ( 'NONE',  ( 7.644554776091147741E-16, 12.48450537969573659, -68.65625000204840944 ) ) ;
#29235 = DATE_AND_TIME ( #36549, #26257 ) ;
#29237 = VERTEX_POINT ( 'NONE', #23463 ) ;
#29236 = CARTESIAN_POINT ( 'NONE',  ( -5.405949406249996869, 9.363379034771805109, -116.3437500020483810 ) ) ;
#29238 = ORIENTED_EDGE ( 'NONE', *, *, #27350, .T. ) ;
#29239 = CARTESIAN_POINT ( 'NONE',  ( 10.81189881249999729, 6.242252689847867408, -32.71875000204834549 ) ) ;
#29240 = CARTESIAN_POINT ( 'NONE',  ( -5.405949406249996869, 9.363379034771805109, -194.3437500020484094 ) ) ;
#29241 = CARTESIAN_POINT ( 'NONE',  ( -10.81189881249999907, -6.242252689847864744, -51.46875000204837391 ) ) ;
#29242 = DIRECTION ( 'NONE',  ( -0.000000000000000000, -0.000000000000000000, -1.000000000000000000 ) ) ;
#29243 = CARTESIAN_POINT ( 'NONE',  ( -9.999999999999998224, 5.773502691896259087, -26.87499999999998579 ) ) ;
#29244 = CARTESIAN_POINT ( 'NONE',  ( 10.81189881249999729, 0.000000000000000000, -190.3437500020484094 ) ) ;
#29245 = CARTESIAN_POINT ( 'NONE',  ( 5.405949406249992428, -9.363379034771808662, -171.0937500020484094 ) ) ;
#29246 = CARTESIAN_POINT ( 'NONE',  ( -5.405949406249996869, 9.363379034771805109, -147.8437500020483810 ) ) ;
#29248 = EDGE_CURVE ( 'NONE', #17582, #23938, #14667, .T. ) ;
#29247 = CARTESIAN_POINT ( 'NONE',  ( 10.81189881249999551, -6.242252689847874514, -172.4687500020483810 ) ) ;
#29249 = CARTESIAN_POINT ( 'NONE',  ( 5.000000000000000000, 8.660254037844385522, -124.7500000000000000 ) ) ;
#29250 = CARTESIAN_POINT ( 'NONE',  ( 5.000000000000000000, 8.660254037844385522, -20.12500000409675494 ) ) ;
#29251 = CARTESIAN_POINT ( 'NONE',  ( -5.000000000000003553, -8.660254037844383745, -187.0000000000000000 ) ) ;
#29252 = CARTESIAN_POINT ( 'NONE',  ( -2.293366432827344421E-15, -12.48450537969573659, -94.71875000204838102 ) ) ;
#29253 = FACE_OUTER_BOUND ( 'NONE', #22444, .T. ) ;
#29254 = CARTESIAN_POINT ( 'NONE',  ( -10.81189881249999729, 6.242252689847871849, -72.90625000204838102 ) ) ;
#29255 = CARTESIAN_POINT ( 'NONE',  ( -9.999999999999998224, 1.224646799147353059E-15, -88.62500000409677625 ) ) ;
#29256 = CARTESIAN_POINT ( 'NONE',  ( -5.405949406250003975, -9.363379034771801557, -195.3437500020484094 ) ) ;
#29257 = CARTESIAN_POINT ( 'NONE',  ( 5.405949406249999534, 9.363379034771803333, -88.09375000204836681 ) ) ;
#29258 =( BOUNDED_CURVE ( )  B_SPLINE_CURVE ( 2, ( #26072, #16749, #42661, #39851, #29951, #33405, #9660 ),
 .UNSPECIFIED., .F., .F. ) 
 B_SPLINE_CURVE_WITH_KNOTS ( ( 3, 2, 2, 3 ),
 ( 0.4738805970149255198, 0.4751243781094529051, 0.4763681592039803459, 0.4776119402985076756 ),
 .UNSPECIFIED. ) 
 CURVE ( )  GEOMETRIC_REPRESENTATION_ITEM ( )  RATIONAL_B_SPLINE_CURVE ( ( 0.9999999999999820144, 0.8660254037844566932, 1.000000000000000000, 0.8660254037844387076, 1.000000000000000000, 0.8660254037844148378, 1.000000000000023981 ) ) 
 REPRESENTATION_ITEM ( '' )  );
#29259 = CARTESIAN_POINT ( 'NONE',  ( 5.405949406249992428, -9.363379034771808662, -58.78125000204836681 ) ) ;
#29260 = CARTESIAN_POINT ( 'NONE',  ( 7.070501591499377789E-16, 11.54700538379251284, -147.5000000040968189 ) ) ;
#29261 = CARTESIAN_POINT ( 'NONE',  ( -2.121150477449813534E-15, -11.54700538379251284, -111.8749999999999858 ) ) ;
#29262 = ORIENTED_EDGE ( 'NONE', *, *, #27056, .F. ) ;
#29263 = CARTESIAN_POINT ( 'NONE',  ( 5.405949406249992428, -9.363379034771808662, -141.2812500020483810 ) ) ;
#29264 = CARTESIAN_POINT ( 'NONE',  ( -2.293366432827344421E-15, -12.48450537969573659, -153.4062500020483810 ) ) ;
#29265 = FACE_OUTER_BOUND ( 'NONE', #41904, .T. ) ;
#29266 = CARTESIAN_POINT ( 'NONE',  ( 5.000000000000000000, 8.660254037844385522, -105.2499999999999858 ) ) ;
#29267 = CARTESIAN_POINT ( 'NONE',  ( -5.405949406250003975, -9.363379034771801557, -91.84375000204838102 ) ) ;
#29268 = ORIENTED_EDGE ( 'NONE', *, *, #17169, .T. ) ;
#29269 = CARTESIAN_POINT ( 'NONE',  ( 4.999999999999992006, -8.660254037844389075, -59.24999999999997158 ) ) ;
#29270 = CARTESIAN_POINT ( 'NONE',  ( -2.293366432827344421E-15, -12.48450537969573659, -189.2187500020484094 ) ) ;
#29271 = CARTESIAN_POINT ( 'NONE',  ( -10.00000000000000000, -5.773502691896251982, -73.50000000409674783 ) ) ;
#29272 = EDGE_CURVE ( 'NONE', #40567, #14344, #39216, .T. ) ;
#29273 = CARTESIAN_POINT ( 'NONE',  ( 10.00000000000012257, -5.773502691896187144, -169.0000000040967620 ) ) ;
#29274 = DIRECTION ( 'NONE',  ( -0.000000000000000000, -0.000000000000000000, 1.000000000000000000 ) ) ;
#29275 = CARTESIAN_POINT ( 'NONE',  ( 5.405949406249999534, 9.363379034771803333, -82.28125000204838102 ) ) ;
#29276 = CARTESIAN_POINT ( 'NONE',  ( 10.81189881249999729, 6.242252689847867408, -70.40625000204839523 ) ) ;
#29277 = CARTESIAN_POINT ( 'NONE',  ( 4.999999999999992006, -8.660254037844389075, -64.12500000409676204 ) ) ;
#29278 = CARTESIAN_POINT ( 'NONE',  ( 7.644554776091147741E-16, 12.48450537969573659, -21.96875000204837391 ) ) ;
#29279 = CARTESIAN_POINT ( 'NONE',  ( -9.999999999999998224, 1.224646799147353059E-15, -16.24999999999995737 ) ) ;
#29280 = CARTESIAN_POINT ( 'NONE',  ( 7.644554776091147741E-16, 12.48450537969573659, -184.1562500020484094 ) ) ;
#29281 = CARTESIAN_POINT ( 'NONE',  ( 10.81189881249999551, -6.242252689847874514, -10.65625000204836859 ) ) ;
#29282 = CARTESIAN_POINT ( 'NONE',  ( -4.999999999999996447, 8.660254037844387298, -79.49999999999998579 ) ) ;
#29283 = CARTESIAN_POINT ( 'NONE',  ( 5.000000000000000000, 8.660254037844385522, -186.6250000040967905 ) ) ;
#29284 = CARTESIAN_POINT ( 'NONE',  ( -4.999999999999996447, 8.660254037844387298, -159.3750000040967905 ) ) ;
#29285 = CARTESIAN_POINT ( 'NONE',  ( 4.999999999999992006, -8.660254037844389075, -177.7500000000000284 ) ) ;
#29286 = CARTESIAN_POINT ( 'NONE',  ( 9.999999999999998224, 0.000000000000000000, -36.49999999999997868 ) ) ;
#29288 = VERTEX_POINT ( 'NONE', #36610 ) ;
#29287 = CARTESIAN_POINT ( 'NONE',  ( -5.405949406249996869, 9.363379034771805109, -95.53125000204838102 ) ) ;
#29289 = ORIENTED_EDGE ( 'NONE', *, *, #22023, .F. ) ;
#29290 = ORIENTED_EDGE ( 'NONE', *, *, #13398, .T. ) ;
#29291 = CARTESIAN_POINT ( 'NONE',  ( 10.81189881249999551, -6.242252689847874514, -37.46875000204836681 ) ) ;
#29292 = CIRCLE ( 'NONE', #32748, 10.00000000000000178 ) ;
#29293 = CARTESIAN_POINT ( 'NONE',  ( -5.405949406249996869, 9.363379034771805109, -29.53125000204837036 ) ) ;
#29294 = APPROVAL_STATUS ( 'not_yet_approved' ) ;
#29295 = CARTESIAN_POINT ( 'NONE',  ( -10.81189881249999729, 1.324075727343319199E-15, -80.09375000204838102 ) ) ;
#29296 = PLANE ( 'NONE',  #8449 ) ;
#29297 = CARTESIAN_POINT ( 'NONE',  ( -5.405949406249996869, 9.363379034771805109, -189.8437500020483810 ) ) ;
#29298 =( BOUNDED_CURVE ( )  B_SPLINE_CURVE ( 2, ( #9214, #28234, #22384, #5777, #8799, #1906, #15036 ),
 .UNSPECIFIED., .F., .F. ) 
 B_SPLINE_CURVE_WITH_KNOTS ( ( 3, 2, 2, 3 ),
 ( 0.4514925373134329734, 0.4527363184079603031, 0.4539800995024877439, 0.4552238805970150737 ),
 .UNSPECIFIED. ) 
 CURVE ( )  GEOMETRIC_REPRESENTATION_ITEM ( )  RATIONAL_B_SPLINE_CURVE ( ( 0.9999999999999880096, 0.8660254037844506980, 1.000000000000000000, 0.8660254037844387076, 1.000000000000000000, 0.8660254037844207220, 1.000000000000017986 ) ) 
 REPRESENTATION_ITEM ( '' )  );
#29299 = CARTESIAN_POINT ( 'NONE',  ( 9.999999999999998224, 0.000000000000000000, -167.0000000000000000 ) ) ;
#29300 = MANIFOLD_SOLID_BREP ( 'Chamfer1', #41117 ) ;
#29301 = LINE ( 'NONE', #42236, #30202 ) ;
#29302 = CARTESIAN_POINT ( 'NONE',  ( 10.81189881249999907, 6.242252689847868297, -154.4062500020484094 ) ) ;
#29303 = CARTESIAN_POINT ( 'NONE',  ( 7.070501591499377789E-16, 11.54700538379251284, -8.000000004096747830 ) ) ;
#29304 = FACE_OUTER_BOUND ( 'NONE', #21674, .T. ) ;
#29305 = CARTESIAN_POINT ( 'NONE',  ( 10.81189881249999907, 6.242252689847868297, -131.7187500020483810 ) ) ;
#29306 = CARTESIAN_POINT ( 'NONE',  ( 5.405949406249992428, -9.363379034771808662, -102.2812500020483952 ) ) ;
#29307 = CARTESIAN_POINT ( 'NONE',  ( -10.81189881249999729, 6.242252689847871849, -105.7187500020483668 ) ) ;
#29308 = CARTESIAN_POINT ( 'NONE',  ( 5.405949406249992428, -9.363379034771808662, -78.09375000204838102 ) ) ;
#29309 = CIRCLE ( 'NONE', #22438, 42.00000000000001421 ) ;
#29310 = CARTESIAN_POINT ( 'NONE',  ( -5.405949406249996869, 9.363379034771805109, -86.53125000204838102 ) ) ;
#29311 = CARTESIAN_POINT ( 'NONE',  ( 10.00000000000000000, 5.773502691896255534, -173.2500000040967905 ) ) ;
#29312 =( BOUNDED_CURVE ( )  B_SPLINE_CURVE ( 2, ( #15665, #18923, #32107, #28866, #38781, #9207, #35554 ),
 .UNSPECIFIED., .F., .F. ) 
 B_SPLINE_CURVE_WITH_KNOTS ( ( 3, 2, 2, 3 ),
 ( 0.5223880597014926019, 0.5236318407960199872, 0.5248756218905473725, 0.5261194029850747578 ),
 .UNSPECIFIED. ) 
 CURVE ( )  GEOMETRIC_REPRESENTATION_ITEM ( )  RATIONAL_B_SPLINE_CURVE ( ( 0.9999999999999880096, 0.8660254037844506980, 1.000000000000000000, 0.8660254037844387076, 1.000000000000000000, 0.8660254037844267172, 1.000000000000011990 ) ) 
 REPRESENTATION_ITEM ( '' )  );
#29313 = DIRECTION ( 'NONE',  ( -0.000000000000000000, -0.000000000000000000, 1.000000000000000000 ) ) ;
#29314 = CARTESIAN_POINT ( 'NONE',  ( -5.405949406249996869, 9.363379034771805109, -167.5312500020484094 ) ) ;
#29315 = CARTESIAN_POINT ( 'NONE',  ( -10.81189881249999907, -6.242252689847864744, -177.6562500020484094 ) ) ;
#29316 = CARTESIAN_POINT ( 'NONE',  ( 9.999999999999998224, 0.000000000000000000, -155.3750000040967905 ) ) ;
#29317 = FACE_OUTER_BOUND ( 'NONE', #3740, .T. ) ;
#29318 = CARTESIAN_POINT ( 'NONE',  ( -5.405949406249996869, 9.363379034771805109, -6.843750002048371250 ) ) ;
#29319 = CARTESIAN_POINT ( 'NONE',  ( -10.00000000000076916, 5.773502691895813221, -127.3749999999999858 ) ) ;
#29320 = CARTESIAN_POINT ( 'NONE',  ( -10.81189881249999729, 1.324075727343319199E-15, -117.5937500020483810 ) ) ;
#29321 = CARTESIAN_POINT ( 'NONE',  ( 10.00000000000000000, 5.773502691896255534, -82.87499999999997158 ) ) ;
#29322 = CARTESIAN_POINT ( 'NONE',  ( 10.81189881249999907, 6.242252689847868297, -16.40625000204837036 ) ) ;
#29323 = CARTESIAN_POINT ( 'NONE',  ( 9.999999999999998224, 0.000000000000000000, -98.37500000409677625 ) ) ;
#29324 = CARTESIAN_POINT ( 'NONE',  ( 0.000000000000000000, 0.000000000000000000, -200.0000000000000000 ) ) ;
#29325 = CARTESIAN_POINT ( 'NONE',  ( 7.644554776091147741E-16, 12.48450537969573659, -110.6562500020483952 ) ) ;
#29326 = CARTESIAN_POINT ( 'NONE',  ( 10.81189881249999551, -6.242252689847874514, -94.65625000204838102 ) ) ;
#29327 = ORIENTED_EDGE ( 'NONE', *, *, #12535, .T. ) ;
#29328 = VECTOR ( 'NONE', #35176, 1000.000000000000000 ) ;
#29329 = CARTESIAN_POINT ( 'NONE',  ( 4.999999999999992006, -8.660254037844389075, -88.12500000409677625 ) ) ;
#29330 = LINE ( 'NONE', #26096, #16711 ) ;
#29331 = CARTESIAN_POINT ( 'NONE',  ( 10.81189881249999729, 0.000000000000000000, -38.84375000204837391 ) ) ;
#29332 = ORIENTED_EDGE ( 'NONE', *, *, #37811, .T. ) ;
#29333 = CARTESIAN_POINT ( 'NONE',  ( 5.000000000000000000, 8.660254037844385522, -15.24999999999995737 ) ) ;
#29334 = ADVANCED_FACE ( 'NONE', ( #42443 ), #19566, .T. ) ;
#29335 = CARTESIAN_POINT ( 'NONE',  ( 9.999999999999996447, -5.773502691896262640, -152.1250000000000284 ) ) ;
#29336 = CARTESIAN_POINT ( 'NONE',  ( 5.000000000000000000, 8.660254037844385522, -9.625000004096746054 ) ) ;
#29337 = EDGE_CURVE ( 'NONE', #35521, #21267, #19084, .T. ) ;
#29338 = CARTESIAN_POINT ( 'NONE',  ( -5.000000000000003553, -8.660254037844383745, -199.0000000000000000 ) ) ;
#29340 = ORIENTED_EDGE ( 'NONE', *, *, #13676, .T. ) ;
#29339 = CARTESIAN_POINT ( 'NONE',  ( 10.81189881249999729, 0.000000000000000000, -124.5312500020483952 ) ) ;
#29341 = VECTOR ( 'NONE', #35260, 1000.000000000000000 ) ;
#29342 = VERTEX_POINT ( 'NONE', #39629 ) ;
#29343 = AXIS2_PLACEMENT_3D ( 'NONE', #11586, #8384, #3705 ) ;
#29344 = CARTESIAN_POINT ( 'NONE',  ( 5.405949406249999534, 9.363379034771803333, -56.78125000204836681 ) ) ;
#29345 = CALENDAR_DATE ( 2026, 28, 9 ) ;
#29346 = CARTESIAN_POINT ( 'NONE',  ( 7.644554776091147741E-16, 12.48450537969573659, -99.96875000204839523 ) ) ;
#29348 = VERTEX_POINT ( 'NONE', #20417 ) ;
#29347 = ORIENTED_EDGE ( 'NONE', *, *, #252, .F. ) ;
#29349 = AXIS2_PLACEMENT_3D ( 'NONE', #19715, #29873, #10211 ) ;
#29350 = DIRECTION ( 'NONE',  ( 1.000000000000000000, 0.000000000000000000, 0.000000000000000000 ) ) ;
#29351 = CARTESIAN_POINT ( 'NONE',  ( -10.00000000000051337, 5.773502691895962435, -32.87499999999995026 ) ) ;
#29352 = CARTESIAN_POINT ( 'NONE',  ( 5.405949406249992428, -9.363379034771808662, -177.2812500020484094 ) ) ;
#29353 = CARTESIAN_POINT ( 'NONE',  ( -10.81189881249999729, 6.242252689847871849, -0.7187500020483512664 ) ) ;
#29354 = CARTESIAN_POINT ( 'NONE',  ( 0.000000000000000000, 0.000000000000000000, -99.99999999999998579 ) ) ;
#29355 = CARTESIAN_POINT ( 'NONE',  ( -10.81189881249999729, -6.242252689847864744, -135.4687500020483810 ) ) ;
#29356 = CARTESIAN_POINT ( 'NONE',  ( -10.81189881249999729, 1.324075727343319199E-15, -102.5937500020483810 ) ) ;
#29357 = CARTESIAN_POINT ( 'NONE',  ( 0.000000000000000000, 0.000000000000000000, 0.000000000000000000 ) ) ;
#29358 = CARTESIAN_POINT ( 'NONE',  ( -10.81189881249999907, -6.242252689847864744, -108.6562500020483952 ) ) ;
#29359 = CARTESIAN_POINT ( 'NONE',  ( 4.999999999999992006, -8.660254037844389075, -197.6250000040967905 ) ) ;
#29360 = CARTESIAN_POINT ( 'NONE',  ( -2.293366432827344421E-15, -12.48450537969573659, -112.7187500020483668 ) ) ;
#29361 = CARTESIAN_POINT ( 'NONE',  ( -10.81189881249999729, -6.242252689847864744, -186.6562500020484094 ) ) ;
#29362 = CARTESIAN_POINT ( 'NONE',  ( 9.999999999999998224, 0.000000000000000000, -200.0000000000000000 ) ) ;
#29363 = CARTESIAN_POINT ( 'NONE',  ( 9.999999999999998224, 0.000000000000000000, -140.0000000000000000 ) ) ;
#29364 = CARTESIAN_POINT ( 'NONE',  ( 7.070501591499377789E-16, 11.54700538379251284, -7.624999999999965361 ) ) ;
#29365 = CARTESIAN_POINT ( 'NONE',  ( -2.293366432827344421E-15, -12.48450537969573659, -57.21875000204835970 ) ) ;
#29366 = CARTESIAN_POINT ( 'NONE',  ( 10.81189881249999729, 0.000000000000000000, -49.34375000204838102 ) ) ;
#29367 = CARTESIAN_POINT ( 'NONE',  ( -9.999999999999998224, 1.224646799147353059E-15, -180.1250000040968189 ) ) ;
#29368 = CARTESIAN_POINT ( 'NONE',  ( -5.405949406250003975, -9.363379034771801557, -17.03125000204835970 ) ) ;
#29369 = CARTESIAN_POINT ( 'NONE',  ( -10.81189881249999907, -6.242252689847864744, -27.46875000204837391 ) ) ;
#29370 = CARTESIAN_POINT ( 'NONE',  ( -2.121150477449813534E-15, -11.54700538379251284, -8.374999999999976907 ) ) ;
#29371 = CARTESIAN_POINT ( 'NONE',  ( 5.405949406249999534, 9.363379034771803333, -137.5937500020483810 ) ) ;
#29372 = CARTESIAN_POINT ( 'NONE',  ( -10.00000000000000000, -5.773502691896251982, -112.1249999999999858 ) ) ;
#29373 = DIRECTION ( 'NONE',  ( 1.000000000000000000, 0.000000000000000000, 0.000000000000000000 ) ) ;
#29374 = AXIS2_PLACEMENT_3D ( 'NONE', #6004, #11820, #1923 ) ;
#29375 = CARTESIAN_POINT ( 'NONE',  ( 9.999999999999996447, -5.773502691896262640, -65.12499999999998579 ) ) ;
#29376 = CARTESIAN_POINT ( 'NONE',  ( 10.81189881249999907, 6.242252689847868297, -134.9062500020483810 ) ) ;
#29377 = CARTESIAN_POINT ( 'NONE',  ( 10.81189881249999551, -6.242252689847874514, -112.6562500020483952 ) ) ;
#29378 = EDGE_LOOP ( 'NONE', ( #23498, #39000, #32332, #640 ) ) ;
#29379 = DIRECTION ( 'NONE',  ( 1.000000000000000000, 0.000000000000000000, 0.000000000000000000 ) ) ;
#29380 = CARTESIAN_POINT ( 'NONE',  ( 9.999999999999996447, -5.773502691896262640, -110.5000000040967763 ) ) ;
#29381 = CARTESIAN_POINT ( 'NONE',  ( 9.999999999999998224, 0.000000000000000000, -128.0000000000000000 ) ) ;
#29382 = CARTESIAN_POINT ( 'NONE',  ( 7.644554776091147741E-16, 12.48450537969573659, -68.46875000204838102 ) ) ;
#29383 = ORIENTED_EDGE ( 'NONE', *, *, #12974, .T. ) ;
#29384 = CARTESIAN_POINT ( 'NONE',  ( 9.999999999999998224, 0.000000000000000000, -45.49999999999998579 ) ) ;
#29385 = CARTESIAN_POINT ( 'NONE',  ( 9.999999999999998224, 0.000000000000000000, -18.87500000409675494 ) ) ;
#29386 = EDGE_CURVE ( 'NONE', #40028, #15924, #9862, .T. ) ;
#29387 = CARTESIAN_POINT ( 'NONE',  ( -10.81189881249999729, 6.242252689847871849, -44.40625000204835970 ) ) ;
#29388 =( BOUNDED_CURVE ( )  B_SPLINE_CURVE ( 2, ( #27358, #10303, #14159, #10939, #27574, #40285, #4267 ),
 .UNSPECIFIED., .F., .F. ) 
 B_SPLINE_CURVE_WITH_KNOTS ( ( 3, 2, 2, 3 ),
 ( 0.1380597014925373234, 0.1393034825870646809, 0.1405472636815920384, 0.1417910447761193959 ),
 .UNSPECIFIED. ) 
 CURVE ( )  GEOMETRIC_REPRESENTATION_ITEM ( )  RATIONAL_B_SPLINE_CURVE ( ( 1.000000000000000000, 0.8660254037844387076, 1.000000000000000000, 0.8660254037844387076, 1.000000000000000000, 0.8660254037844387076, 1.000000000000000000 ) ) 
 REPRESENTATION_ITEM ( '' )  );
#29389 = CARTESIAN_POINT ( 'NONE',  ( 9.999999999999479527, 5.773502691896553074, -119.2500000040967620 ) ) ;
#29390 = CARTESIAN_POINT ( 'NONE',  ( 9.999999999999996447, -5.773502691896262640, -35.50000000409675494 ) ) ;
#29391 = CARTESIAN_POINT ( 'NONE',  ( 10.81189881249999907, 6.242252689847868297, -37.40625000204836681 ) ) ;
#29392 = EDGE_CURVE ( 'NONE', #31963, #38940, #384, .T. ) ;
#29393 = CARTESIAN_POINT ( 'NONE',  ( 0.000000000000000000, 0.000000000000000000, -200.0000000000000000 ) ) ;
#29394 = CARTESIAN_POINT ( 'NONE',  ( -5.405949406250003975, -9.363379034771801557, -137.0312500020484094 ) ) ;
#29395 = ADVANCED_FACE ( 'NONE', ( #6839 ), #19992, .T. ) ;
#29396 = CARTESIAN_POINT ( 'NONE',  ( 10.81189881249999907, 6.242252689847868297, -146.9062500020484094 ) ) ;
#29397 = CC_DESIGN_PERSON_AND_ORGANIZATION_ASSIGNMENT ( #13340, #220, ( #18390 ) ) ;
#29398 = CARTESIAN_POINT ( 'NONE',  ( 4.999999999999992006, -8.660254037844389075, -123.7500000000000000 ) ) ;
#29399 = ORIENTED_EDGE ( 'NONE', *, *, #29039, .F. ) ;
#29400 = ORIENTED_EDGE ( 'NONE', *, *, #37817, .T. ) ;
#29401 = ORIENTED_EDGE ( 'NONE', *, *, #26995, .T. ) ;
#29402 = CARTESIAN_POINT ( 'NONE',  ( 100.0000000000000142, 19.99999999999999645, -160.0000000000000000 ) ) ;
#29403 = CARTESIAN_POINT ( 'NONE',  ( -10.81189881249999729, 1.324075727343319199E-15, -176.0937500020484094 ) ) ;
#29404 = LOCAL_TIME ( 11, 57, 6.000000000000000000, #15683 ) ;
#29405 = EDGE_CURVE ( 'NONE', #4750, #37499, #32089, .T. ) ;
#29406 = CARTESIAN_POINT ( 'NONE',  ( 7.644554776091147741E-16, 12.48450537969573659, -24.96875000204837036 ) ) ;
#29407 = CYLINDRICAL_SURFACE ( 'NONE', #33650, 9.999999999999998224 ) ;
#29408 = CARTESIAN_POINT ( 'NONE',  ( 7.644554776091147741E-16, 12.48450537969573659, -153.9687500020484094 ) ) ;
#29409 = CARTESIAN_POINT ( 'NONE',  ( -5.405949406250003975, -9.363379034771801557, -142.8437500020483810 ) ) ;
#29410 = CARTESIAN_POINT ( 'NONE',  ( -2.121150477449813534E-15, -11.54700538379251284, -116.3749999999999858 ) ) ;
#29411 = CARTESIAN_POINT ( 'NONE',  ( -10.81189881249999907, -6.242252689847864744, -126.4687500020483810 ) ) ;
#29412 = CARTESIAN_POINT ( 'NONE',  ( 5.405949406249999534, 9.363379034771803333, -130.2812500020483810 ) ) ;
#29413 = CARTESIAN_POINT ( 'NONE',  ( 10.81189881249999729, 0.000000000000000000, -22.34375000204835615 ) ) ;
#29414 = CARTESIAN_POINT ( 'NONE',  ( 5.405949406249999534, 9.363379034771803333, -139.0937500020483810 ) ) ;
#29415 = CARTESIAN_POINT ( 'NONE',  ( 10.83509278446304691, 0.07525214450409632716, -180.0000000000000000 ) ) ;
#29416 = CARTESIAN_POINT ( 'NONE',  ( -10.00000000000051337, 5.773502691895962435, -119.8749999999999858 ) ) ;
#29417 = CARTESIAN_POINT ( 'NONE',  ( 4.999999999999992006, -8.660254037844389075, -159.7500000000000000 ) ) ;
#29418 = CARTESIAN_POINT ( 'NONE',  ( 9.999999999999998224, 0.000000000000000000, -56.37500000409676204 ) ) ;
#29419 = CARTESIAN_POINT ( 'NONE',  ( -5.405949406249996869, 9.363379034771805109, -69.84375000204836681 ) ) ;
#29420 = CARTESIAN_POINT ( 'NONE',  ( -2.293366432827344421E-15, -12.48450537969573659, -54.40625000204838102 ) ) ;
#29421 = CARTESIAN_POINT ( 'NONE',  ( -5.405949406250003975, -9.363379034771801557, -49.84375000204838102 ) ) ;
#29422 = CARTESIAN_POINT ( 'NONE',  ( 9.999999999999998224, 0.000000000000000000, -200.0000000000000000 ) ) ;
#29423 = CARTESIAN_POINT ( 'NONE',  ( -5.405949406249996869, 9.363379034771805109, -164.3437500020484094 ) ) ;
#29424 = CARTESIAN_POINT ( 'NONE',  ( -4.999999999999996447, 8.660254037844387298, -139.5000000000000000 ) ) ;
#29425 = CARTESIAN_POINT ( 'NONE',  ( -5.405949406249996869, 9.363379034771805109, -137.5312500020484094 ) ) ;
#29426 = DIRECTION ( 'NONE',  ( -0.000000000000000000, -0.000000000000000000, -1.000000000000000000 ) ) ;
#29427 = CARTESIAN_POINT ( 'NONE',  ( 9.999999999999998224, 0.000000000000000000, -116.3750000040967905 ) ) ;
#29428 = CARTESIAN_POINT ( 'NONE',  ( -10.00000000000000000, -5.773502691896251982, -89.62499999999997158 ) ) ;
#29429 =( BOUNDED_CURVE ( )  B_SPLINE_CURVE ( 2, ( #12130, #32435, #11700, #41481, #38045, #25321, #24896 ),
 .UNSPECIFIED., .F., .F. ) 
 B_SPLINE_CURVE_WITH_KNOTS ( ( 3, 2, 2, 3 ),
 ( 0.7388059701492539766, 0.7400497512437813619, 0.7412935323383087471, 0.7425373134328361324 ),
 .UNSPECIFIED. ) 
 CURVE ( )  GEOMETRIC_REPRESENTATION_ITEM ( )  RATIONAL_B_SPLINE_CURVE ( ( 0.9999999999999761302, 0.8660254037844625774, 1.000000000000000000, 0.8660254037844387076, 1.000000000000000000, 0.8660254037844028474, 1.000000000000035971 ) ) 
 REPRESENTATION_ITEM ( '' )  );
#29430 = ORIENTED_EDGE ( 'NONE', *, *, #1153, .T. ) ;
#29431 = CARTESIAN_POINT ( 'NONE',  ( 10.81189881249999729, 0.000000000000000000, -121.5312500020483952 ) ) ;
#29432 = CARTESIAN_POINT ( 'NONE',  ( 7.070501591499377789E-16, 11.54700538379251284, -134.0000000040967905 ) ) ;
#29433 = CARTESIAN_POINT ( 'NONE',  ( 9.999999999999742428, 5.773502691896404748, -159.3749999999999716 ) ) ;
#29434 = CARTESIAN_POINT ( 'NONE',  ( 7.644554776091147741E-16, 12.48450537969573659, -173.6562500020483810 ) ) ;
#29435 = CARTESIAN_POINT ( 'NONE',  ( 10.00000000000000000, 5.773502691896255534, -44.25000000409676204 ) ) ;
#29436 = ADVANCED_BREP_SHAPE_REPRESENTATION ( '', ( #1487, #39998 ), #13832 ) ;
#29437 = CARTESIAN_POINT ( 'NONE',  ( 0.000000000000000000, 0.000000000000000000, -200.0000000000000000 ) ) ;
#29438 = CARTESIAN_POINT ( 'NONE',  ( -10.81189881249999729, 1.324075727343319199E-15, -62.28125000204837391 ) ) ;
#29439 = CARTESIAN_POINT ( 'NONE',  ( -4.999999999999996447, 8.660254037844387298, -156.0000000000000000 ) ) ;
#29440 = CARTESIAN_POINT ( 'NONE',  ( 10.81189881249999907, 6.242252689847868297, -161.9062500020484094 ) ) ;
#29441 = CARTESIAN_POINT ( 'NONE',  ( -10.81189881249999729, 6.242252689847871849, -144.7187500020483810 ) ) ;
#29442 = CARTESIAN_POINT ( 'NONE',  ( -10.00000000000012434, 5.773502691896184480, -166.7500000040967905 ) ) ;
#29443 = CARTESIAN_POINT ( 'NONE',  ( -4.999999999999996447, 8.660254037844387298, -171.3750000040968189 ) ) ;
#29444 = ORIENTED_EDGE ( 'NONE', *, *, #25847, .F. ) ;
#29445 = CARTESIAN_POINT ( 'NONE',  ( -4.999999999999996447, 8.660254037844387298, -114.3750000040967763 ) ) ;
#29446 = EDGE_CURVE ( 'NONE', #23818, #18552, #39002, .T. ) ;
#29448 = ORIENTED_EDGE ( 'NONE', *, *, #17109, .T. ) ;
#29447 = CARTESIAN_POINT ( 'NONE',  ( 10.81189881249999907, 6.242252689847868297, -70.40625000204839523 ) ) ;
#29449 = APPLICATION_PROTOCOL_DEFINITION ( 'international standard', 'config_control_design', 1994, #13467 ) ;
#29451 = ORIENTED_EDGE ( 'NONE', *, *, #14281, .T. ) ;
#29450 = CARTESIAN_POINT ( 'NONE',  ( 5.405949406249999534, 9.363379034771803333, -119.5937500020483810 ) ) ;
#29452 = ORIENTED_EDGE ( 'NONE', *, *, #35558, .T. ) ;
#29453 = CARTESIAN_POINT ( 'NONE',  ( -5.405949406250003975, -9.363379034771801557, -18.34375000204835260 ) ) ;
#29454 = CARTESIAN_POINT ( 'NONE',  ( -10.81189881249999729, 1.324075727343319199E-15, -0.7812500020483725827 ) ) ;
#29455 = CARTESIAN_POINT ( 'NONE',  ( -10.81189881249999907, -6.242252689847864744, -48.46875000204837391 ) ) ;
#29456 = CARTESIAN_POINT ( 'NONE',  ( 9.999999999999998224, 0.000000000000000000, -111.8750000040967763 ) ) ;
#29457 = CARTESIAN_POINT ( 'NONE',  ( -5.000000000000003553, -8.660254037844383745, -32.49999999999997158 ) ) ;
#29458 = CARTESIAN_POINT ( 'NONE',  ( -10.81189881249999729, 1.324075727343319199E-15, -185.0937500020483810 ) ) ;
#29459 = CARTESIAN_POINT ( 'NONE',  ( -10.81189881249999729, 1.324075727343319199E-15, -165.5937500020484094 ) ) ;
#29460 = CARTESIAN_POINT ( 'NONE',  ( 5.405949406249992428, -9.363379034771808662, -147.0937500020483810 ) ) ;
#29461 = CARTESIAN_POINT ( 'NONE',  ( -10.81189881249999729, -6.242252689847864744, -166.9687500020484094 ) ) ;
#29462 = CARTESIAN_POINT ( 'NONE',  ( 0.000000000000000000, 0.000000000000000000, -200.0000000000000000 ) ) ;
#29463 = CYLINDRICAL_SURFACE ( 'NONE', #35038, 9.999999999999998224 ) ;
#29464 = CARTESIAN_POINT ( 'NONE',  ( -2.121150477449813534E-15, -11.54700538379251284, -185.3750000000000284 ) ) ;
#29465 = CARTESIAN_POINT ( 'NONE',  ( 10.81189881249999907, 6.242252689847868297, -95.71875000204838102 ) ) ;
#29466 = CARTESIAN_POINT ( 'NONE',  ( 5.000000000000000000, 8.660254037844385522, -196.7500000000000000 ) ) ;
#29467 = CARTESIAN_POINT ( 'NONE',  ( -10.81189881249999907, -6.242252689847864744, -77.15625000204836681 ) ) ;
#29468 = CARTESIAN_POINT ( 'NONE',  ( 9.999999999999479527, 5.773502691896553074, -89.25000000409674783 ) ) ;
#29469 = CARTESIAN_POINT ( 'NONE',  ( 10.81189881249999907, 6.242252689847868297, -182.7187500020484094 ) ) ;
#29470 = CARTESIAN_POINT ( 'NONE',  ( -10.81189881249999729, 1.324075727343319199E-15, -162.7812500020484094 ) ) ;
#29471 = CARTESIAN_POINT ( 'NONE',  ( 5.405949406249999534, 9.363379034771803333, -62.78125000204837391 ) ) ;
#29472 = CARTESIAN_POINT ( 'NONE',  ( 9.999999999999996447, -5.773502691896262640, -140.5000000040967905 ) ) ;
#29473 = CARTESIAN_POINT ( 'NONE',  ( 9.999999999999996447, -5.773502691896262640, -111.6249999999999858 ) ) ;
#29474 = VERTEX_POINT ( 'NONE', #17811 ) ;
#29475 = CARTESIAN_POINT ( 'NONE',  ( 5.405949406249999534, 9.363379034771803333, -139.2812500020483810 ) ) ;
#29476 = CARTESIAN_POINT ( 'NONE',  ( 5.405949406249999534, 9.363379034771803333, -155.7812500020484094 ) ) ;
#29477 = CARTESIAN_POINT ( 'NONE',  ( 5.405949406249999534, 9.363379034771803333, -197.7812500020484094 ) ) ;
#29478 = CARTESIAN_POINT ( 'NONE',  ( -9.999999999999998224, 1.224646799147353059E-15, -130.6250000040967620 ) ) ;
#29479 = CARTESIAN_POINT ( 'NONE',  ( -2.293366432827344421E-15, -12.48450537969573659, -87.21875000204838102 ) ) ;
#29480 = VECTOR ( 'NONE', #26908, 1000.000000000000000 ) ;
#29481 = EDGE_LOOP ( 'NONE', ( #12015, #28080, #7685, #38614 ) ) ;
#29482 = CARTESIAN_POINT ( 'NONE',  ( -4.999999999999996447, 8.660254037844387298, -53.99999999999996447 ) ) ;
#29483 = CARTESIAN_POINT ( 'NONE',  ( -10.81189881249999729, 1.324075727343319199E-15, -188.0937500020483810 ) ) ;
#29484 = CARTESIAN_POINT ( 'NONE',  ( 9.999999999999996447, -5.773502691896262640, -68.50000000409677625 ) ) ;
#29485 = VECTOR ( 'NONE', #6842, 1000.000000000000000 ) ;
#29486 = CARTESIAN_POINT ( 'NONE',  ( -10.00000000000000000, -5.773502691896252870, -169.5000000040967905 ) ) ;
#29487 = CARTESIAN_POINT ( 'NONE',  ( 7.071067811865472841, -7.071067811865472841, -200.0000000000000000 ) ) ;
#29488 = CARTESIAN_POINT ( 'NONE',  ( 10.81189881249999907, 6.242252689847868297, -80.90625000204839523 ) ) ;
#29489 = CARTESIAN_POINT ( 'NONE',  ( -2.293366432827344421E-15, -12.48450537969573659, -69.40625000204839523 ) ) ;
#29490 = CARTESIAN_POINT ( 'NONE',  ( 9.999999999999996447, -5.773502691896262640, -59.50000000409677625 ) ) ;
#29491 = CARTESIAN_POINT ( 'NONE',  ( 5.405949406249992428, -9.363379034771808662, -21.09375000204835615 ) ) ;
#29492 = DIRECTION ( 'NONE',  ( -0.000000000000000000, -0.000000000000000000, 1.000000000000000000 ) ) ;
#29493 = CARTESIAN_POINT ( 'NONE',  ( 10.81189881249999907, 6.242252689847868297, -188.9062500020484379 ) ) ;
#29494 = CARTESIAN_POINT ( 'NONE',  ( 5.405949406249999534, 9.363379034771803333, -16.28125000204835970 ) ) ;
#29495 = LINE ( 'NONE', #33167, #19946 ) ;
#29496 = CARTESIAN_POINT ( 'NONE',  ( 5.000000000000000000, 8.660254037844385522, -114.6250000040967763 ) ) ;
#29497 = DIRECTION ( 'NONE',  ( -1.000000000000000000, 0.000000000000000000, 0.000000000000000000 ) ) ;
#29498 = CARTESIAN_POINT ( 'NONE',  ( -4.999999999999996447, 8.660254037844387298, -168.0000000000000000 ) ) ;
#29499 = CARTESIAN_POINT ( 'NONE',  ( 0.000000000000000000, 0.000000000000000000, -200.0000000000000000 ) ) ;
#29501 = ORIENTED_EDGE ( 'NONE', *, *, #6508, .F. ) ;
#29500 = CARTESIAN_POINT ( 'NONE',  ( -10.81189881249999729, 6.242252689847871849, -95.40625000204838102 ) ) ;
#29502 = CARTESIAN_POINT ( 'NONE',  ( -2.121150477449813534E-15, -11.54700538379251284, -181.2500000040967905 ) ) ;
#29504 = ORIENTED_EDGE ( 'NONE', *, *, #4339, .T. ) ;
#29503 = CARTESIAN_POINT ( 'NONE',  ( 10.81189881249999551, -6.242252689847874514, -100.4687500020483952 ) ) ;
#29505 = ORIENTED_EDGE ( 'NONE', *, *, #40709, .T. ) ;
#29506 = CARTESIAN_POINT ( 'NONE',  ( 5.405949406249999534, 9.363379034771803333, -34.09375000204836681 ) ) ;
#29507 = CARTESIAN_POINT ( 'NONE',  ( 5.405949406249999534, 9.363379034771803333, -25.28125000204836681 ) ) ;
#29508 = ITEM_DEFINED_TRANSFORMATION ( 'NONE', 'NONE', #42107,  #39998 ) ;
#29509 = CARTESIAN_POINT ( 'NONE',  ( -10.81189881249999729, 6.242252689847871849, -71.21875000204839523 ) ) ;
#29510 = CARTESIAN_POINT ( 'NONE',  ( 9.999999999999998224, 0.000000000000000000, -114.8750000040967905 ) ) ;
#29511 = AXIS2_PLACEMENT_3D ( 'NONE', #17976, #755, #41058 ) ;
#29512 = AXIS2_PLACEMENT_3D ( 'NONE', #36409, #13298, #23680 ) ;
#29513 = CARTESIAN_POINT ( 'NONE',  ( 5.405949406249992428, -9.363379034771808662, -193.5937500020484094 ) ) ;
#29514 =( BOUNDED_CURVE ( )  B_SPLINE_CURVE ( 2, ( #22729, #35894, #16218, #26389, #9971, #23151, #36312 ),
 .UNSPECIFIED., .F., .F. ) 
 B_SPLINE_CURVE_WITH_KNOTS ( ( 3, 2, 2, 3 ),
 ( 0.1529850746268656692, 0.1542288557213930267, 0.1554726368159203842, 0.1567164179104477695 ),
 .UNSPECIFIED. ) 
 CURVE ( )  GEOMETRIC_REPRESENTATION_ITEM ( )  RATIONAL_B_SPLINE_CURVE ( ( 1.000000000000000000, 0.8660254037844387076, 1.000000000000000000, 0.8660254037844387076, 1.000000000000000000, 0.8660254037844387076, 1.000000000000000000 ) ) 
 REPRESENTATION_ITEM ( '' )  );
#29515 = EDGE_CURVE ( 'NONE', #34935, #40566, #11120, .T. ) ;
#29516 = CARTESIAN_POINT ( 'NONE',  ( -9.999999999999998224, 1.224646799147353059E-15, -100.6250000040967905 ) ) ;
#29517 = CARTESIAN_POINT ( 'NONE',  ( -5.405949406250003975, -9.363379034771801557, -159.5312500020484094 ) ) ;
#29518 = CARTESIAN_POINT ( 'NONE',  ( -10.00000000000000000, -5.773502691896251982, -4.500000004096765593 ) ) ;
#29519 = CARTESIAN_POINT ( 'NONE',  ( -10.00000000000025580, 5.773502691896109873, -121.3749999999999858 ) ) ;
#29520 = CARTESIAN_POINT ( 'NONE',  ( -10.81189881249999907, -6.242252689847864744, -124.9687500020483810 ) ) ;
#29521 = CARTESIAN_POINT ( 'NONE',  ( 5.405949406249999534, 9.363379034771803333, -97.28125000204839523 ) ) ;
#29522 = CARTESIAN_POINT ( 'NONE',  ( -10.81189881249999729, 6.242252689847871849, -111.7187500020483810 ) ) ;
#29523 = CARTESIAN_POINT ( 'NONE',  ( 5.405949406249992428, -9.363379034771808662, -75.09375000204838102 ) ) ;
#29524 = CARTESIAN_POINT ( 'NONE',  ( 10.81189881249999907, 6.242252689847868297, -85.40625000204839523 ) ) ;
#29525 = CARTESIAN_POINT ( 'NONE',  ( -10.00000000000000000, -5.773502691896251982, -162.0000000040967620 ) ) ;
#29526 = CARTESIAN_POINT ( 'NONE',  ( -9.999999999999998224, 1.224646799147353059E-15, -200.0000000000000000 ) ) ;
#29527 = CARTESIAN_POINT ( 'NONE',  ( 5.405949406249999534, 9.363379034771803333, -167.7812500020484094 ) ) ;
#29528 = CARTESIAN_POINT ( 'NONE',  ( -10.81189881249999729, 6.242252689847871849, -176.4062500020484094 ) ) ;
#29529 = CARTESIAN_POINT ( 'NONE',  ( -9.999999999999998224, 1.224646799147353059E-15, -153.1250000040967905 ) ) ;
#29530 = CARTESIAN_POINT ( 'NONE',  ( -9.999999999999998224, 1.224646799147353059E-15, -157.2500000000000000 ) ) ;
#29531 = CARTESIAN_POINT ( 'NONE',  ( -5.405949406249996869, 9.363379034771805109, -5.343750002048369474 ) ) ;
#29532 = CARTESIAN_POINT ( 'NONE',  ( -4.999999999999996447, 8.660254037844387298, -127.5000000000000000 ) ) ;
#29533 = CARTESIAN_POINT ( 'NONE',  ( 7.644554776091147741E-16, 12.48450537969573659, -114.9687500020483668 ) ) ;
#29534 = CARTESIAN_POINT ( 'NONE',  ( -2.121150477449813534E-15, -11.54700538379251284, -84.87500000000000000 ) ) ;
#29535 = CARTESIAN_POINT ( 'NONE',  ( -5.405949406250003975, -9.363379034771801557, -11.03125000204835438 ) ) ;
#29536 = CARTESIAN_POINT ( 'NONE',  ( -2.121150477449813534E-15, -11.54700538379251284, -100.2500000040967905 ) ) ;
#29537 = CARTESIAN_POINT ( 'NONE',  ( 7.070501591499376803E-16, 11.54700538379251284, -150.5000000040968189 ) ) ;
#29538 = CARTESIAN_POINT ( 'NONE',  ( -5.405949406249996869, 9.363379034771805109, -112.0312500020483810 ) ) ;
#29539 = CARTESIAN_POINT ( 'NONE',  ( 7.644554776091147741E-16, 12.48450537969573659, -88.15625000204838102 ) ) ;
#29540 = ORIENTED_EDGE ( 'NONE', *, *, #12511, .T. ) ;
#29541 = CARTESIAN_POINT ( 'NONE',  ( 9.999999999999998224, 0.000000000000000000, -81.87500000409676204 ) ) ;
#29542 = CARTESIAN_POINT ( 'NONE',  ( -9.999999999999998224, 1.224646799147353059E-15, -47.74999999999998579 ) ) ;
#29543 = CARTESIAN_POINT ( 'NONE',  ( -5.405949406249996869, 9.363379034771805109, -39.84375000204837391 ) ) ;
#29544 = ORIENTED_EDGE ( 'NONE', *, *, #37625, .T. ) ;
#29545 = CARTESIAN_POINT ( 'NONE',  ( 9.999999999999996447, -5.773502691896262640, -8.124999999999975131 ) ) ;
#29546 = CARTESIAN_POINT ( 'NONE',  ( -5.000000000000003553, -8.660254037844383745, -149.5000000000000000 ) ) ;
#29547 = AXIS2_PLACEMENT_3D ( 'NONE', #23202, #16485, #22565 ) ;
#29548 = CARTESIAN_POINT ( 'NONE',  ( 9.999999999999998224, 0.000000000000000000, -11.37500000409674783 ) ) ;
#29549 = CARTESIAN_POINT ( 'NONE',  ( 7.070501591499377789E-16, 11.54700538379251284, -187.6250000000000284 ) ) ;
#29551 = ORIENTED_EDGE ( 'NONE', *, *, #25109, .T. ) ;
#29550 = CARTESIAN_POINT ( 'NONE',  ( 10.81189881249999551, -6.242252689847874514, -114.1562500020483952 ) ) ;
#29552 = CARTESIAN_POINT ( 'NONE',  ( 7.070501591499376803E-16, 11.54700538379251284, -13.62499999999996803 ) ) ;
#29553 = ORIENTED_EDGE ( 'NONE', *, *, #34899, .T. ) ;
#29554 =( BOUNDED_CURVE ( )  B_SPLINE_CURVE ( 2, ( #10683, #1210, #997, #37453, #40247, #13696, #8108 ),
 .UNSPECIFIED., .F., .F. ) 
 B_SPLINE_CURVE_WITH_KNOTS ( ( 3, 2, 2, 3 ),
 ( 0.2238805970149254365, 0.2251243781094527940, 0.2263681592039801793, 0.2276119402985075368 ),
 .UNSPECIFIED. ) 
 CURVE ( )  GEOMETRIC_REPRESENTATION_ITEM ( )  RATIONAL_B_SPLINE_CURVE ( ( 0.9999999999999940048, 0.8660254037844447028, 1.000000000000000000, 0.8660254037844387076, 1.000000000000000000, 0.8660254037844297148, 1.000000000000008882 ) ) 
 REPRESENTATION_ITEM ( '' )  );
#29555 = CARTESIAN_POINT ( 'NONE',  ( -2.293366432827344421E-15, -12.48450537969573659, -46.90625000204836681 ) ) ;
#29556 = SECURITY_CLASSIFICATION_LEVEL ( 'unclassified' ) ;
#29557 = CARTESIAN_POINT ( 'NONE',  ( 10.81189881249999729, 0.000000000000000000, -103.3437500020483668 ) ) ;
#29558 = CARTESIAN_POINT ( 'NONE',  ( -10.81189881249999729, -6.242252689847864744, -122.1562500020483810 ) ) ;
#29559 = ORIENTED_EDGE ( 'NONE', *, *, #37458, .F. ) ;
#29560 = CARTESIAN_POINT ( 'NONE',  ( 10.00000000000102318, -5.773502691895667560, -83.12499999999992895 ) ) ;
#29561 = DIRECTION ( 'NONE',  ( 1.000000000000000000, 0.000000000000000000, 0.000000000000000000 ) ) ;
#29562 =( BOUNDED_CURVE ( )  B_SPLINE_CURVE ( 2, ( #27578, #24138, #30610, #28010, #14604, #1684, #8375 ),
 .UNSPECIFIED., .F., .F. ) 
 B_SPLINE_CURVE_WITH_KNOTS ( ( 3, 2, 2, 3 ),
 ( 0.4253731343283583266, 0.4266169154228856564, 0.4278606965174130417, 0.4291044776119404269 ),
 .UNSPECIFIED. ) 
 CURVE ( )  GEOMETRIC_REPRESENTATION_ITEM ( )  RATIONAL_B_SPLINE_CURVE ( ( 0.9999999999999880096, 0.8660254037844506980, 1.000000000000000000, 0.8660254037844387076, 1.000000000000000000, 0.8660254037844267172, 1.000000000000011990 ) ) 
 REPRESENTATION_ITEM ( '' )  );
#29563 = CARTESIAN_POINT ( 'NONE',  ( 7.644554776091147741E-16, 12.48450537969573659, -181.1562500020484094 ) ) ;
#29564 = CARTESIAN_POINT ( 'NONE',  ( 0.000000000000000000, 0.000000000000000000, -200.0000000000000000 ) ) ;
#29565 = EDGE_CURVE ( 'NONE', #20303, #9851, #27664, .T. ) ;
#29566 = CARTESIAN_POINT ( 'NONE',  ( -10.81189881249999729, -6.242252689847864744, -130.9687500020483810 ) ) ;
#29567 = AXIS2_PLACEMENT_3D ( 'NONE', #39125, #35692, #35899 ) ;
#29568 = CARTESIAN_POINT ( 'NONE',  ( 10.81189881249999551, -6.242252689847874514, -100.4687500020483952 ) ) ;
#29569 = FACE_OUTER_BOUND ( 'NONE', #33567, .T. ) ;
#29570 = CARTESIAN_POINT ( 'NONE',  ( -10.81189881249999729, 6.242252689847871849, -108.9062500020483810 ) ) ;
#29571 = CARTESIAN_POINT ( 'NONE',  ( 9.999999999999998224, 0.000000000000000000, -191.3750000040967905 ) ) ;
#29572 = CARTESIAN_POINT ( 'NONE',  ( -5.405949406250003975, -9.363379034771801557, -111.3437500020483810 ) ) ;
#29573 = CARTESIAN_POINT ( 'NONE',  ( -2.293366432827344421E-15, -12.48450537969573659, -183.4062500020484094 ) ) ;
#29574 = CARTESIAN_POINT ( 'NONE',  ( 10.00000000000102318, -5.773502691895667560, -47.12499999999992895 ) ) ;
#29575 = LINE ( 'NONE', #25555, #13438 ) ;
#29576 = CARTESIAN_POINT ( 'NONE',  ( 5.000000000000000000, 8.660254037844385522, -139.7499999999999716 ) ) ;
#29577 = CARTESIAN_POINT ( 'NONE',  ( -9.999999999999998224, 5.773502691896259087, -2.874999999999960920 ) ) ;
#29578 = CARTESIAN_POINT ( 'NONE',  ( -10.81189881249999729, -6.242252689847864744, -58.96875000204836681 ) ) ;
#29579 = VECTOR ( 'NONE', #36159, 1000.000000000000000 ) ;
#29580 = CARTESIAN_POINT ( 'NONE',  ( -10.81189881249999729, 1.324075727343319199E-15, -51.59375000204835260 ) ) ;
#29581 = DESIGN_CONTEXT ( 'detailed design', #3865, 'design' ) ;
#29582 = CARTESIAN_POINT ( 'NONE',  ( 5.000000000000000000, 8.660254037844385522, -179.1250000040968189 ) ) ;
#29583 = CARTESIAN_POINT ( 'NONE',  ( -10.81189881249999907, -6.242252689847864744, -15.65625000204837569 ) ) ;
#29584 = CARTESIAN_POINT ( 'NONE',  ( -5.405949406250003975, -9.363379034771801557, -33.34375000204836681 ) ) ;
#29585 = CARTESIAN_POINT ( 'NONE',  ( -2.275517850991317657E-15, -20.00000000000000000, -220.0000000000000000 ) ) ;
#29586 = CARTESIAN_POINT ( 'NONE',  ( -2.293366432827344421E-15, -12.48450537969573659, -141.2187500020483810 ) ) ;
#29587 = CARTESIAN_POINT ( 'NONE',  ( -9.999999999999998224, 5.773502691896259087, -103.3750000000000000 ) ) ;
#29588 = CARTESIAN_POINT ( 'NONE',  ( 10.81189881249999551, -6.242252689847874514, -34.65625000204835970 ) ) ;
#29589 = CARTESIAN_POINT ( 'NONE',  ( 0.000000000000000000, 0.000000000000000000, -99.99999999999998579 ) ) ;
#29590 = CARTESIAN_POINT ( 'NONE',  ( -9.999999999999998224, 5.773502691896259087, -68.87499999999998579 ) ) ;
#29591 = CARTESIAN_POINT ( 'NONE',  ( 10.81189881249999729, 0.000000000000000000, -130.5312500020484094 ) ) ;
#29592 = CARTESIAN_POINT ( 'NONE',  ( 10.81189881249999729, 0.000000000000000000, -115.5312500020483952 ) ) ;
#29593 = ORIENTED_EDGE ( 'NONE', *, *, #40713, .F. ) ;
#29594 = VECTOR ( 'NONE', #16644, 1000.000000000000000 ) ;
#29595 = CARTESIAN_POINT ( 'NONE',  ( 9.999999999999998224, 0.000000000000000000, -131.0000000000000000 ) ) ;
#29596 = CARTESIAN_POINT ( 'NONE',  ( 9.999999999999998224, 0.000000000000000000, -110.3750000040967763 ) ) ;
#29597 = CARTESIAN_POINT ( 'NONE',  ( -4.999999999999996447, 8.660254037844387298, -100.8750000040967905 ) ) ;
#29598 = CARTESIAN_POINT ( 'NONE',  ( 10.81189881249999907, 6.242252689847868297, -68.71875000204838102 ) ) ;
#29599 = ORIENTED_EDGE ( 'NONE', *, *, #32291, .T. ) ;
#29600 = CARTESIAN_POINT ( 'NONE',  ( -9.999999999999998224, 5.773502691896259087, -31.37499999999995737 ) ) ;
#29601 = CARTESIAN_POINT ( 'NONE',  ( 10.00000000000000000, 5.773502691896255534, -21.75000000409676559 ) ) ;
#29602 = CARTESIAN_POINT ( 'NONE',  ( -5.405949406250003975, -9.363379034771801557, -47.03125000204838813 ) ) ;
#29603 = CARTESIAN_POINT ( 'NONE',  ( 9.999999999999998224, 0.000000000000000000, -125.3750000040967905 ) ) ;
#29604 = CARTESIAN_POINT ( 'NONE',  ( 5.000000000000000000, 8.660254037844385522, -38.12500000409676915 ) ) ;
#29605 = CARTESIAN_POINT ( 'NONE',  ( -5.405949406249996869, 9.363379034771805109, -140.5312500020484094 ) ) ;
#29606 = CARTESIAN_POINT ( 'NONE',  ( -5.405949406250003975, -9.363379034771801557, -143.0312500020483810 ) ) ;
#29607 = FACE_OUTER_BOUND ( 'NONE', #19656, .T. ) ;
#29608 = ORIENTED_EDGE ( 'NONE', *, *, #34141, .F. ) ;
#29609 = VECTOR ( 'NONE', #41096, 1000.000000000000000 ) ;
#29610 = ORIENTED_EDGE ( 'NONE', *, *, #33366, .F. ) ;
#29611 = ORIENTED_EDGE ( 'NONE', *, *, #39233, .T. ) ;
#29612 = CARTESIAN_POINT ( 'NONE',  ( 4.999999999999992006, -8.660254037844389075, -121.1250000040967905 ) ) ;
#29613 = CARTESIAN_POINT ( 'NONE',  ( 10.81189881249999729, 0.000000000000000000, -176.8437500020483810 ) ) ;
#29614 = VECTOR ( 'NONE', #36421, 1000.000000000000000 ) ;
#29615 = CARTESIAN_POINT ( 'NONE',  ( -2.293366432827344421E-15, -12.48450537969573659, -25.71875000204837391 ) ) ;
#29616 = CARTESIAN_POINT ( 'NONE',  ( -9.999999999998969713, -5.773502691896847949, -61.50000000409675494 ) ) ;
#29617 = EDGE_CURVE ( 'NONE', #25832, #37214, #16917, .T. ) ;
#29618 = CARTESIAN_POINT ( 'NONE',  ( 7.644554776091147741E-16, 12.48450537969573659, -159.9687500020484094 ) ) ;
#29619 = CARTESIAN_POINT ( 'NONE',  ( 7.644554776091147741E-16, 12.48450537969573659, -146.4687500020484094 ) ) ;
#29620 = ADVANCED_FACE ( 'NONE', ( #31007 ), #37899, .T. ) ;
#29621 = CARTESIAN_POINT ( 'NONE',  ( -5.405949406250003975, -9.363379034771801557, -127.8437500020483952 ) ) ;
#29622 = CARTESIAN_POINT ( 'NONE',  ( -10.81189881249999729, 6.242252689847871849, -135.9062500020484094 ) ) ;
#29623 = CARTESIAN_POINT ( 'NONE',  ( 10.81189881249999729, 0.000000000000000000, -17.84375000204835260 ) ) ;
#29625 = ADVANCED_FACE ( 'NONE', ( #27331 ), #24532, .T. ) ;
#29624 = CARTESIAN_POINT ( 'NONE',  ( 5.405949406249992428, -9.363379034771808662, -141.0937500020483810 ) ) ;
#29626 = FACE_OUTER_BOUND ( 'NONE', #32389, .T. ) ;
#29627 = CARTESIAN_POINT ( 'NONE',  ( 4.999999999999992006, -8.660254037844389075, -102.7500000000000000 ) ) ;
#29628 = CARTESIAN_POINT ( 'NONE',  ( 10.00000000000000000, 5.773502691896255534, -162.3750000000000000 ) ) ;
#29629 = CARTESIAN_POINT ( 'NONE',  ( -9.999999999998456346, -5.773502691897145489, -17.62499999999993250 ) ) ;
#29630 = CARTESIAN_POINT ( 'NONE',  ( 10.81189881249999907, 6.242252689847868297, -73.21875000204836681 ) ) ;
#29631 = CARTESIAN_POINT ( 'NONE',  ( 10.81189881249999729, 0.000000000000000000, -40.53125000204838102 ) ) ;
#29632 = CARTESIAN_POINT ( 'NONE',  ( 10.81189881249999729, 0.000000000000000000, -55.34375000204835970 ) ) ;
#29633 = DIRECTION ( 'NONE',  ( 0.7071067811865483499, 0.000000000000000000, 0.7071067811865466846 ) ) ;
#29634 = CARTESIAN_POINT ( 'NONE',  ( 5.405949406249999534, 9.363379034771803333, -163.0937500020484094 ) ) ;
#29635 = CARTESIAN_POINT ( 'NONE',  ( -2.121150477449813534E-15, -11.54700538379251284, -131.3750000000000000 ) ) ;
#29636 = CARTESIAN_POINT ( 'NONE',  ( -5.405949406249996869, 9.363379034771805109, -134.5312500020484094 ) ) ;
#29637 =( BOUNDED_CURVE ( )  B_SPLINE_CURVE ( 2, ( #3310, #16655, #22737, #42567, #7178, #13415, #294 ),
 .UNSPECIFIED., .F., .F. ) 
 B_SPLINE_CURVE_WITH_KNOTS ( ( 3, 2, 2, 3 ),
 ( 0.2425373134328359381, 0.2437810945273632957, 0.2450248756218906532, 0.2462686567164180107 ),
 .UNSPECIFIED. ) 
 CURVE ( )  GEOMETRIC_REPRESENTATION_ITEM ( )  RATIONAL_B_SPLINE_CURVE ( ( 0.9999999999999880096, 0.8660254037844506980, 1.000000000000000000, 0.8660254037844387076, 1.000000000000000000, 0.8660254037844267172, 1.000000000000011990 ) ) 
 REPRESENTATION_ITEM ( '' )  );
#29638 = APPROVAL ( #36189, 'UNKNOWN' ) ;
#29639 = CARTESIAN_POINT ( 'NONE',  ( -9.999999999999998224, 1.224646799147353059E-15, -114.1250000040967763 ) ) ;
#29640 = CARTESIAN_POINT ( 'NONE',  ( -5.000000000000003553, -8.660254037844383745, -92.49999999999998579 ) ) ;
#29641 = ORIENTED_EDGE ( 'NONE', *, *, #37969, .F. ) ;
#29642 = CARTESIAN_POINT ( 'NONE',  ( -2.293366432827344421E-15, -12.48450537969573659, -106.9062500020483810 ) ) ;
#29643 = CARTESIAN_POINT ( 'NONE',  ( -2.121150477449813534E-15, -11.54700538379251284, -130.2500000040967905 ) ) ;
#29644 = CARTESIAN_POINT ( 'NONE',  ( 0.000000000000000000, 0.000000000000000000, -99.99999999999998579 ) ) ;
#29645 = VECTOR ( 'NONE', #23666, 1000.000000000000000 ) ;
#29646 = CARTESIAN_POINT ( 'NONE',  ( 5.405949406249999534, 9.363379034771803333, -172.2812500020484094 ) ) ;
#29647 = CARTESIAN_POINT ( 'NONE',  ( 10.00000000000000000, 5.773502691896255534, -38.25000000409676204 ) ) ;
#29648 = ADVANCED_FACE ( 'NONE', ( #27118 ), #10913, .F. ) ;
#29649 = FACE_OUTER_BOUND ( 'NONE', #10846, .T. ) ;
#29650 = CARTESIAN_POINT ( 'NONE',  ( 10.81189881249999907, 6.242252689847868297, -56.90625000204837391 ) ) ;
#29651 = CARTESIAN_POINT ( 'NONE',  ( 5.000000000000000000, 8.660254037844385522, -101.1250000040967905 ) ) ;
#29652 = CARTESIAN_POINT ( 'NONE',  ( 10.81189881249999729, 0.000000000000000000, -160.5312500020484094 ) ) ;
#29653 = EDGE_CURVE ( 'NONE', #13705, #20043, #36485, .T. ) ;
#29654 = CARTESIAN_POINT ( 'NONE',  ( 10.81189881249999551, -6.242252689847874514, -131.9687500020483810 ) ) ;
#29655 = CARTESIAN_POINT ( 'NONE',  ( 7.070501591499376803E-16, 11.54700538379251284, -167.0000000040967905 ) ) ;
#29656 = CARTESIAN_POINT ( 'NONE',  ( 7.070501591499376803E-16, 11.54700538379251284, -150.1250000000000000 ) ) ;
#29657 = ADVANCED_FACE ( 'NONE', ( #8342 ), #34028, .T. ) ;
#29658 = ORIENTED_EDGE ( 'NONE', *, *, #41740, .T. ) ;
#29659 = CARTESIAN_POINT ( 'NONE',  ( -9.999999999999479527, -5.773502691896549521, -79.12499999999997158 ) ) ;
#29661 = ORIENTED_EDGE ( 'NONE', *, *, #25421, .F. ) ;
#29660 = CARTESIAN_POINT ( 'NONE',  ( 5.405949406249999534, 9.363379034771803333, -67.28125000204838102 ) ) ;
#29663 = EDGE_LOOP ( 'NONE', ( #33389, #39835, #39720, #19486 ) ) ;
#29662 = CARTESIAN_POINT ( 'NONE',  ( 10.81189881249999551, -6.242252689847874514, -118.4687500020483810 ) ) ;
#29664 = EDGE_CURVE ( 'NONE', #3284, #8850, #6990, .T. ) ;
#29665 = EDGE_CURVE ( 'NONE', #13539, #35190, #29056, .T. ) ;
#29666 = VERTEX_POINT ( 'NONE', #42177 ) ;
#29667 = CARTESIAN_POINT ( 'NONE',  ( -10.81189881249999729, 1.324075727343319199E-15, -21.59375000204835615 ) ) ;
#29668 = CARTESIAN_POINT ( 'NONE',  ( 10.81189881249999907, 6.242252689847868297, 0.09374999795163654892 ) ) ;
#29669 = AXIS2_PLACEMENT_3D ( 'NONE', #6669, #20036, #26319 ) ;
#29670 = CARTESIAN_POINT ( 'NONE',  ( 10.81189881249999551, -6.242252689847874514, -50.96875000204836681 ) ) ;
#29671 = CYLINDRICAL_SURFACE ( 'NONE', #23290, 9.999999999999998224 ) ;
#29672 = CARTESIAN_POINT ( 'NONE',  ( 9.999999999999996447, -5.773502691896262640, -27.62499999999998224 ) ) ;
#29673 = CARTESIAN_POINT ( 'NONE',  ( -5.405949406250003975, -9.363379034771801557, -183.3437500020483810 ) ) ;
#29674 = CARTESIAN_POINT ( 'NONE',  ( -2.293366432827344421E-15, -12.48450537969573659, -166.7187500020484094 ) ) ;
#29675 = CARTESIAN_POINT ( 'NONE',  ( -10.81189881249999729, 6.242252689847871849, -153.7187500020483526 ) ) ;
#29676 =( BOUNDED_CURVE ( )  B_SPLINE_CURVE ( 2, ( #9247, #26299, #22417, #5596, #2786, #6237, #18749 ),
 .UNSPECIFIED., .F., .F. ) 
 B_SPLINE_CURVE_WITH_KNOTS ( ( 3, 2, 2, 3 ),
 ( 0.9626865671641793298, 0.9639303482587067151, 0.9651741293532341004, 0.9664179104477613746 ),
 .UNSPECIFIED. ) 
 CURVE ( )  GEOMETRIC_REPRESENTATION_ITEM ( )  RATIONAL_B_SPLINE_CURVE ( ( 0.9999999999999761302, 0.8660254037844625774, 1.000000000000000000, 0.8660254037844387076, 1.000000000000000000, 0.8660254037844148378, 1.000000000000023981 ) ) 
 REPRESENTATION_ITEM ( '' )  );
#29677 = CARTESIAN_POINT ( 'NONE',  ( 7.644554776091147741E-16, 12.48450537969573659, -165.9687500020483810 ) ) ;
#29678 = CARTESIAN_POINT ( 'NONE',  ( 9.999999999999998224, 0.000000000000000000, -5.375000004096769146 ) ) ;
#29679 = CARTESIAN_POINT ( 'NONE',  ( 7.070501591499376803E-16, 11.54700538379251284, -20.00000000409677625 ) ) ;
#29680 = CARTESIAN_POINT ( 'NONE',  ( -4.999999999999996447, 8.660254037844387298, -189.0000000000000000 ) ) ;
#29681 = CARTESIAN_POINT ( 'NONE',  ( -5.405949406250003975, -9.363379034771801557, -93.34375000204838102 ) ) ;
#29682 = FACE_OUTER_BOUND ( 'NONE', #41430, .T. ) ;
#29683 = CARTESIAN_POINT ( 'NONE',  ( -10.81189881249999907, -6.242252689847864744, -69.65625000204839523 ) ) ;
#29684 = CARTESIAN_POINT ( 'NONE',  ( -10.00000000000051337, 5.773502691895962435, -88.75000000409676204 ) ) ;
#29685 = CARTESIAN_POINT ( 'NONE',  ( -5.405949406249996869, 9.363379034771805109, -183.8437500020483810 ) ) ;
#29686 = CARTESIAN_POINT ( 'NONE',  ( -10.81189881249999729, -6.242252689847864744, -162.6562500020483810 ) ) ;
#29687 = CARTESIAN_POINT ( 'NONE',  ( 10.81189881249999729, 0.000000000000000000, -61.53125000204837391 ) ) ;
#29688 = CARTESIAN_POINT ( 'NONE',  ( 10.00000000000000000, 5.773502691896255534, -137.2500000040967905 ) ) ;
#29689 = CARTESIAN_POINT ( 'NONE',  ( 9.999999999999998224, 0.000000000000000000, -114.4999999999999858 ) ) ;
#29690 = EDGE_LOOP ( 'NONE', ( #40460, #2487, #28131, #31427 ) ) ;
#29691 = CARTESIAN_POINT ( 'NONE',  ( 10.81189881249999729, 6.242252689847867408, -142.4062500020484094 ) ) ;
#29692 = CARTESIAN_POINT ( 'NONE',  ( -5.405949406249996869, 9.363379034771805109, -152.5312500020484094 ) ) ;
#29693 = CARTESIAN_POINT ( 'NONE',  ( -10.81189881249999729, 6.242252689847871849, -195.9062500020484094 ) ) ;
#29694 = CARTESIAN_POINT ( 'NONE',  ( 9.999999999999998224, 0.000000000000000000, -42.87500000409677625 ) ) ;
#29695 = CARTESIAN_POINT ( 'NONE',  ( 10.81189881249999729, 0.000000000000000000, -91.34375000204838102 ) ) ;
#29696 = ORIENTED_EDGE ( 'NONE', *, *, #889, .F. ) ;
#29697 = CARTESIAN_POINT ( 'NONE',  ( 9.999999999999996447, -5.773502691896262640, -60.62499999999998579 ) ) ;
#29698 = CARTESIAN_POINT ( 'NONE',  ( -5.405949406249996869, 9.363379034771805109, -191.3437500020484094 ) ) ;
#29699 = CARTESIAN_POINT ( 'NONE',  ( 5.000000000000000000, 8.660254037844385522, -69.62500000409677625 ) ) ;
#29700 = CARTESIAN_POINT ( 'NONE',  ( 9.999999999999998224, 0.000000000000000000, -102.5000000000000000 ) ) ;
#29701 = CARTESIAN_POINT ( 'NONE',  ( 10.00000000000051159, -5.773502691895965988, -144.6250000000000000 ) ) ;
#29702 = CARTESIAN_POINT ( 'NONE',  ( -10.81189881249999907, -6.242252689847864744, -83.15625000204836681 ) ) ;
#29703 = CARTESIAN_POINT ( 'NONE',  ( 7.644554776091147741E-16, 12.48450537969573659, -58.15625000204838102 ) ) ;
#29704 = EDGE_CURVE ( 'NONE', #16918, #21964, #11387, .T. ) ;
#29705 = CARTESIAN_POINT ( 'NONE',  ( -2.121150477449813534E-15, -11.54700538379251284, -59.75000000409678336 ) ) ;
#29706 = CARTESIAN_POINT ( 'NONE',  ( -2.293366432827344421E-15, -12.48450537969573659, -18.21875000204836681 ) ) ;
#29707 = FACE_OUTER_BOUND ( 'NONE', #30675, .T. ) ;
#29708 = CARTESIAN_POINT ( 'NONE',  ( 5.405949406249992428, -9.363379034771808662, -184.7812500020484094 ) ) ;
#29709 = AXIS2_PLACEMENT_3D ( 'NONE', #38518, #32063, #2494 ) ;
#29710 = CARTESIAN_POINT ( 'NONE',  ( -5.405949406250003975, -9.363379034771801557, -14.03125000204835615 ) ) ;
#29711 = CARTESIAN_POINT ( 'NONE',  ( -10.81189881249999729, -6.242252689847864744, -0.4687500020483501006 ) ) ;
#29712 = FACE_OUTER_BOUND ( 'NONE', #35622, .T. ) ;
#29713 = AXIS2_PLACEMENT_3D ( 'NONE', #4007, #30772, #40661 ) ;
#29714 = CARTESIAN_POINT ( 'NONE',  ( -2.121150477449813534E-15, -11.54700538379251284, -62.75000000409679046 ) ) ;
#29715 = DIRECTION ( 'NONE',  ( -0.000000000000000000, -0.000000000000000000, 1.000000000000000000 ) ) ;
#29716 = CARTESIAN_POINT ( 'NONE',  ( -9.999999999999998224, 1.224646799147353059E-15, -169.2500000000000000 ) ) ;
#29717 = CARTESIAN_POINT ( 'NONE',  ( 10.00000000000102318, -5.773502691895667560, -62.12499999999992895 ) ) ;
#29719 = ORIENTED_EDGE ( 'NONE', *, *, #8536, .T. ) ;
#29718 = CARTESIAN_POINT ( 'NONE',  ( 7.644554776091147741E-16, 12.48450537969573659, -95.65625000204838102 ) ) ;
#29720 = CARTESIAN_POINT ( 'NONE',  ( -4.999999999999996447, 8.660254037844387298, -82.87500000409676204 ) ) ;
#29722 = ORIENTED_EDGE ( 'NONE', *, *, #41868, .F. ) ;
#29721 = CARTESIAN_POINT ( 'NONE',  ( 9.999999999999872102, 5.773502691896329253, -162.3750000000000000 ) ) ;
#29723 = EDGE_LOOP ( 'NONE', ( #35861, #6177, #19807, #3991 ) ) ;
#29724 = CARTESIAN_POINT ( 'NONE',  ( 10.81189881249999907, 6.242252689847868297, -35.71875000204835970 ) ) ;
#29725 = CARTESIAN_POINT ( 'NONE',  ( -10.81189881249999907, -6.242252689847864744, -24.65625000204838457 ) ) ;
#29726 = CARTESIAN_POINT ( 'NONE',  ( -10.81189881249999729, 6.242252689847871849, -72.71875000204835260 ) ) ;
#29727 = CARTESIAN_POINT ( 'NONE',  ( -9.999999999999479527, -5.773502691896549521, -115.5000000040967763 ) ) ;
#29728 = CARTESIAN_POINT ( 'NONE',  ( -10.81189881249999729, 1.324075727343319199E-15, -192.5937500020484094 ) ) ;
#29729 = CARTESIAN_POINT ( 'NONE',  ( 5.405949406249999534, 9.363379034771803333, -149.5937500020483810 ) ) ;
#29730 = AXIS2_PLACEMENT_3D ( 'NONE', #42578, #39141, #39557 ) ;
#29731 = CARTESIAN_POINT ( 'NONE',  ( 10.00000000000025402, -5.773502691896113426, -121.0000000040967763 ) ) ;
#29732 = CARTESIAN_POINT ( 'NONE',  ( 0.000000000000000000, 0.000000000000000000, -160.0000000000000000 ) ) ;
#29733 = CARTESIAN_POINT ( 'NONE',  ( -10.81189881249999907, -6.242252689847864744, -146.1562500020484094 ) ) ;
#29734 = CARTESIAN_POINT ( 'NONE',  ( -9.999999999999998224, 1.224646799147353059E-15, -0.1250000040967647053 ) ) ;
#29735 = CYLINDRICAL_SURFACE ( 'NONE', #32932, 9.999999999999998224 ) ;
#29736 = CC_DESIGN_APPROVAL ( #9846, ( #20655 ) ) ;
#29737 = CARTESIAN_POINT ( 'NONE',  ( -10.81189881249999729, 1.324075727343319199E-15, -122.0937500020483952 ) ) ;
#29738 = CARTESIAN_POINT ( 'NONE',  ( -10.81189881249999729, 1.324075727343319199E-15, -95.28125000204838102 ) ) ;
#29739 = CARTESIAN_POINT ( 'NONE',  ( -10.81189881249999729, 1.324075727343319199E-15, -107.0937500020483810 ) ) ;
#29740 = CARTESIAN_POINT ( 'NONE',  ( -10.81189881249999729, 6.242252689847871849, -77.21875000204838102 ) ) ;
#29741 = CARTESIAN_POINT ( 'NONE',  ( 5.405949406249992428, -9.363379034771808662, -84.28125000204838102 ) ) ;
#29742 = CARTESIAN_POINT ( 'NONE',  ( -2.121150477449813534E-15, -11.54700538379251284, -161.7500000040967620 ) ) ;
#29743 = DIRECTION ( 'NONE',  ( -0.000000000000000000, -0.000000000000000000, 1.000000000000000000 ) ) ;
#29744 = CARTESIAN_POINT ( 'NONE',  ( -10.81189881249999729, 1.324075727343319199E-15, -162.7812500020484094 ) ) ;
#29745 = CARTESIAN_POINT ( 'NONE',  ( 10.81189881249999907, 6.242252689847868297, -181.4062500020484379 ) ) ;
#29746 = EDGE_CURVE ( 'NONE', #13020, #36434, #12189, .T. ) ;
#29747 = CARTESIAN_POINT ( 'NONE',  ( -5.000000000000003553, -8.660254037844383745, -152.8750000040967905 ) ) ;
#29748 = CARTESIAN_POINT ( 'NONE',  ( 10.00000000000025402, -5.773502691896113426, -189.6250000000000000 ) ) ;
#29749 = CARTESIAN_POINT ( 'NONE',  ( 7.644554776091147741E-16, 12.48450537969573659, -8.468750002048359704 ) ) ;
#29750 = CARTESIAN_POINT ( 'NONE',  ( 9.999999999999998224, 0.000000000000000000, -104.3750000040967763 ) ) ;
#29751 = CARTESIAN_POINT ( 'NONE',  ( 10.81189881249999551, -6.242252689847874514, -113.9687500020483810 ) ) ;
#29752 = CARTESIAN_POINT ( 'NONE',  ( 9.999999999999998224, 0.000000000000000000, -82.99999999999997158 ) ) ;
#29753 = CARTESIAN_POINT ( 'NONE',  ( -10.81189881249999729, 1.324075727343319199E-15, -9.781250002048352599 ) ) ;
#29754 = CARTESIAN_POINT ( 'NONE',  ( 10.00000000000000000, 5.773502691896255534, -89.25000000409677625 ) ) ;
#29755 = DIRECTION ( 'NONE',  ( -0.000000000000000000, -0.000000000000000000, -1.000000000000000000 ) ) ;
#29756 = CARTESIAN_POINT ( 'NONE',  ( -5.405949406250003975, -9.363379034771801557, -105.5312500020483810 ) ) ;
#29757 = CARTESIAN_POINT ( 'NONE',  ( -10.81189881249999729, 6.242252689847871849, -87.90625000204838102 ) ) ;
#29758 = ORIENTED_EDGE ( 'NONE', *, *, #25190, .F. ) ;
#29759 = CARTESIAN_POINT ( 'NONE',  ( 9.999999999999996447, -5.773502691896262640, -86.50000000409676204 ) ) ;
#29760 = CARTESIAN_POINT ( 'NONE',  ( 9.999999999999998224, 0.000000000000000000, -200.0000000000000000 ) ) ;
#29761 = CARTESIAN_POINT ( 'NONE',  ( 7.644554776091147741E-16, 12.48450537969573659, -44.46875000204836681 ) ) ;
#29762 = EDGE_LOOP ( 'NONE', ( #3548, #33173, #1155, #29559 ) ) ;
#29763 = CARTESIAN_POINT ( 'NONE',  ( -9.999999999999998224, 5.773502691896259087, -11.87499999999996092 ) ) ;
#29764 = CARTESIAN_POINT ( 'NONE',  ( -10.00000000000000000, -5.773502691896251982, -142.1250000000000000 ) ) ;
#29765 = CYLINDRICAL_SURFACE ( 'NONE', #31042, 9.999999999999998224 ) ;
#29766 = CARTESIAN_POINT ( 'NONE',  ( 9.999999999999998224, 0.000000000000000000, -15.87500000409675138 ) ) ;
#29767 = ADVANCED_FACE ( 'NONE', ( #19101 ), #22346, .F. ) ;
#29768 = AXIS2_PLACEMENT_3D ( 'NONE', #41737, #21902, #5507 ) ;
#29769 = CC_DESIGN_APPROVAL ( #5371, ( #37345 ) ) ;
#29770 = CARTESIAN_POINT ( 'NONE',  ( 5.000000000000000000, 8.660254037844385522, -190.7500000000000000 ) ) ;
#29771 = CARTESIAN_POINT ( 'NONE',  ( 9.999999999999998224, 0.000000000000000000, -183.8750000040967905 ) ) ;
#29772 = APPLICATION_CONTEXT ( 'configuration controlled 3d designs of mechanical parts and assemblies' ) ;
#29774 = VERTEX_POINT ( 'NONE', #34674 ) ;
#29773 = CARTESIAN_POINT ( 'NONE',  ( -2.293366432827344421E-15, -12.48450537969573659, -115.9062500020483810 ) ) ;
#29775 = CARTESIAN_POINT ( 'NONE',  ( -9.999999999999998224, 1.224646799147353059E-15, -200.0000000000000000 ) ) ;
#29776 =( BOUNDED_CURVE ( )  B_SPLINE_CURVE ( 2, ( #4595, #8054, #30295, #21201, #10414, #34387, #4804 ),
 .UNSPECIFIED., .F., .F. ) 
 B_SPLINE_CURVE_WITH_KNOTS ( ( 3, 2, 2, 3 ),
 ( 0.04104477611940302029, 0.04228855721393039169, 0.04353233830845775615, 0.04477611940298512061 ),
 .UNSPECIFIED. ) 
 CURVE ( )  GEOMETRIC_REPRESENTATION_ITEM ( )  RATIONAL_B_SPLINE_CURVE ( ( 0.9999999999999963363, 0.8660254037844424824, 1.000000000000000000, 0.8660254037844387076, 1.000000000000000000, 0.8660254037844334896, 1.000000000000005329 ) ) 
 REPRESENTATION_ITEM ( '' )  );
#29777 = ORIENTED_EDGE ( 'NONE', *, *, #21736, .F. ) ;
#29778 = CARTESIAN_POINT ( 'NONE',  ( 5.405949406249992428, -9.363379034771808662, -49.78125000204838813 ) ) ;
#29779 = DATE_AND_TIME ( #16577, #1489 ) ;
#29780 = AXIS2_PLACEMENT_3D ( 'NONE', #22117, #34867, #15195 ) ;
#29781 = CARTESIAN_POINT ( 'NONE',  ( 10.81189881249999551, -6.242252689847874514, -92.96875000204838102 ) ) ;
#29782 = CARTESIAN_POINT ( 'NONE',  ( 5.405949406249992428, -9.363379034771808662, -120.2812500020483952 ) ) ;
#29783 = VERTEX_POINT ( 'NONE', #25591 ) ;
#29784 = CARTESIAN_POINT ( 'NONE',  ( -9.999999999999998224, 1.224646799147353059E-15, -138.1250000040967620 ) ) ;
#29785 = CARTESIAN_POINT ( 'NONE',  ( 5.405949406249999534, 9.363379034771803333, -178.2812500020484094 ) ) ;
#29786 = CARTESIAN_POINT ( 'NONE',  ( 0.000000000000000000, 0.000000000000000000, -200.0000000000000000 ) ) ;
#29787 = CARTESIAN_POINT ( 'NONE',  ( -5.405949406250003975, -9.363379034771801557, -130.8437500020484094 ) ) ;
#29788 = CARTESIAN_POINT ( 'NONE',  ( 10.81189881249999729, 0.000000000000000000, -103.3437500020483668 ) ) ;
#29789 = FACE_OUTER_BOUND ( 'NONE', #14486, .T. ) ;
#29790 = CARTESIAN_POINT ( 'NONE',  ( 7.644554776091147741E-16, 12.48450537969573659, -109.1562500020483810 ) ) ;
#29791 = CARTESIAN_POINT ( 'NONE',  ( 5.000000000000000000, 8.660254037844385522, -182.1250000040967905 ) ) ;
#29792 = CARTESIAN_POINT ( 'NONE',  ( -10.81189881249999729, 6.242252689847871849, -111.7187500020483810 ) ) ;
#29793 = CIRCLE ( 'NONE', #39423, 20.00000000000000000 ) ;
#29794 = CARTESIAN_POINT ( 'NONE',  ( 5.405949406249999534, 9.363379034771803333, -182.7812500020484094 ) ) ;
#29795 = ADVANCED_FACE ( 'NONE', ( #38746 ), #28833, .T. ) ;
#29796 = CARTESIAN_POINT ( 'NONE',  ( 9.999999999999998224, 0.000000000000000000, -185.3750000040967905 ) ) ;
#29797 = CARTESIAN_POINT ( 'NONE',  ( 4.999999999999992006, -8.660254037844389075, -132.7499999999999716 ) ) ;
#29798 = CARTESIAN_POINT ( 'NONE',  ( -2.121150477449813534E-15, -11.54700538379251284, -8.374999999999964473 ) ) ;
#29799 = CARTESIAN_POINT ( 'NONE',  ( -5.405949406249996869, 9.363379034771805109, -59.34375000204835970 ) ) ;
#29800 = CARTESIAN_POINT ( 'NONE',  ( -10.81189881249999729, 1.324075727343319199E-15, -47.09375000204838102 ) ) ;
#29801 = CARTESIAN_POINT ( 'NONE',  ( -9.999999999999998224, 5.773502691896259087, -181.7500000040967905 ) ) ;
#29802 = CARTESIAN_POINT ( 'NONE',  ( -10.81189881249999907, -6.242252689847864744, -18.65625000204837036 ) ) ;
#29803 = CARTESIAN_POINT ( 'NONE',  ( 10.81189881249999551, -6.242252689847874514, -32.96875000204835260 ) ) ;
#29804 = CARTESIAN_POINT ( 'NONE',  ( 5.000000000000000000, 8.660254037844385522, -145.7500000000000000 ) ) ;
#29805 = CARTESIAN_POINT ( 'NONE',  ( -10.81189881249999729, 1.324075727343319199E-15, -140.0937500020483810 ) ) ;
#29806 = CARTESIAN_POINT ( 'NONE',  ( 7.070501591499377789E-16, 11.54700538379251284, -102.1250000000000000 ) ) ;
#29807 = CARTESIAN_POINT ( 'NONE',  ( 7.644554776091147741E-16, 12.48450537969573659, -40.15625000204836681 ) ) ;
#29808 = CARTESIAN_POINT ( 'NONE',  ( 0.000000000000000000, 0.000000000000000000, -200.0000000000000000 ) ) ;
#29809 = CARTESIAN_POINT ( 'NONE',  ( 4.999999999999992006, -8.660254037844389075, -63.74999999999997158 ) ) ;
#29810 = CARTESIAN_POINT ( 'NONE',  ( 5.405949406249992428, -9.363379034771808662, -129.2812500020483810 ) ) ;
#29811 = CARTESIAN_POINT ( 'NONE',  ( 10.81189881249999729, 6.242252689847867408, -112.4062500020483952 ) ) ;
#29812 = ORIENTED_EDGE ( 'NONE', *, *, #28084, .T. ) ;
#29813 = CARTESIAN_POINT ( 'NONE',  ( 9.999999999999479527, 5.773502691896553074, -142.8749999999999716 ) ) ;
#29814 = CARTESIAN_POINT ( 'NONE',  ( -5.000000000000003553, -8.660254037844383745, -106.3750000040967763 ) ) ;
#29815 = CARTESIAN_POINT ( 'NONE',  ( -5.000000000000003553, -8.660254037844383745, -146.5000000000000000 ) ) ;
#29816 = CARTESIAN_POINT ( 'NONE',  ( -10.81189881249999729, 6.242252689847871849, -63.71875000204838102 ) ) ;
#29817 = VERTEX_POINT ( 'NONE', #41550 ) ;
#29818 = CARTESIAN_POINT ( 'NONE',  ( 9.999999999999998224, 0.000000000000000000, -33.49999999999997158 ) ) ;
#29819 = AXIS2_PLACEMENT_3D ( 'NONE', #3059, #32211, #35864 ) ;
#29820 = CARTESIAN_POINT ( 'NONE',  ( -4.999999999999996447, 8.660254037844387298, -16.87500000409675138 ) ) ;
#29821 = CARTESIAN_POINT ( 'NONE',  ( -5.405949406249996869, 9.363379034771805109, -40.03125000204838102 ) ) ;
#29822 = LINE ( 'NONE', #3703, #30419 ) ;
#29823 = CARTESIAN_POINT ( 'NONE',  ( 9.999999999999998224, 0.000000000000000000, -35.37500000409676915 ) ) ;
#29824 =( BOUNDED_CURVE ( )  B_SPLINE_CURVE ( 2, ( #6792, #17123, #30326, #23200, #26434, #33354, #10652 ),
 .UNSPECIFIED., .F., .F. ) 
 B_SPLINE_CURVE_WITH_KNOTS ( ( 3, 2, 2, 3 ),
 ( 0.4888059701492538101, 0.4900497512437811398, 0.4912935323383085806, 0.4925373134328359104 ),
 .UNSPECIFIED. ) 
 CURVE ( )  GEOMETRIC_REPRESENTATION_ITEM ( )  RATIONAL_B_SPLINE_CURVE ( ( 0.9999999999999940048, 0.8660254037844447028, 1.000000000000000000, 0.8660254037844387076, 1.000000000000000000, 0.8660254037844267172, 1.000000000000011990 ) ) 
 REPRESENTATION_ITEM ( '' )  );
#29825 = CARTESIAN_POINT ( 'NONE',  ( 9.999999999999742428, 5.773502691896404748, -156.7500000040967905 ) ) ;
#29826 = CARTESIAN_POINT ( 'NONE',  ( 5.405949406249992428, -9.363379034771808662, -144.2812500020483810 ) ) ;
#29827 = ADVANCED_FACE ( 'NONE', ( #9175 ), #25798, .T. ) ;
#29828 = CARTESIAN_POINT ( 'NONE',  ( 9.999999999999998224, 0.000000000000000000, -15.49999999999995737 ) ) ;
#29829 = VERTEX_POINT ( 'NONE', #21915 ) ;
#29830 =( BOUNDED_CURVE ( )  B_SPLINE_CURVE ( 2, ( #9160, #15613, #21471, #35292, #28818, #41948, #41310 ),
 .UNSPECIFIED., .F., .F. ) 
 B_SPLINE_CURVE_WITH_KNOTS ( ( 3, 2, 2, 3 ),
 ( 0.4589552238805971740, 0.4601990049751245593, 0.4614427860696518890, 0.4626865671641792743 ),
 .UNSPECIFIED. ) 
 CURVE ( )  GEOMETRIC_REPRESENTATION_ITEM ( )  RATIONAL_B_SPLINE_CURVE ( ( 0.9999999999999820144, 0.8660254037844566932, 1.000000000000000000, 0.8660254037844387076, 1.000000000000000000, 0.8660254037844207220, 1.000000000000017986 ) ) 
 REPRESENTATION_ITEM ( '' )  );
#29831 = ORIENTED_EDGE ( 'NONE', *, *, #11491, .T. ) ;
#29832 = EDGE_LOOP ( 'NONE', ( #11799, #33053, #21205, #22019 ) ) ;
#29833 = CARTESIAN_POINT ( 'NONE',  ( -9.999999999999998224, 1.224646799147353059E-15, -200.0000000000000000 ) ) ;
#29834 = CARTESIAN_POINT ( 'NONE',  ( 10.81189881249999551, -6.242252689847874514, -173.9687500020484094 ) ) ;
#29835 = VECTOR ( 'NONE', #38352, 1000.000000000000000 ) ;
#29836 = CARTESIAN_POINT ( 'NONE',  ( -5.405949406250003975, -9.363379034771801557, -24.34375000204835970 ) ) ;
#29837 = CARTESIAN_POINT ( 'NONE',  ( -9.999999999999998224, 1.224646799147353059E-15, -144.1250000040967905 ) ) ;
#29838 = CARTESIAN_POINT ( 'NONE',  ( 7.644554776091147741E-16, 12.48450537969573659, -152.4687500020484094 ) ) ;
#29839 = CARTESIAN_POINT ( 'NONE',  ( 10.81189881249999551, -6.242252689847874514, -145.4687500020483810 ) ) ;
#29840 = CARTESIAN_POINT ( 'NONE',  ( -7.071067811865477282, 7.071067811865471064, -200.0000000000000000 ) ) ;
#29841 = CARTESIAN_POINT ( 'NONE',  ( 5.405949406249992428, -9.363379034771808662, -124.5937500020483952 ) ) ;
#29842 = CARTESIAN_POINT ( 'NONE',  ( 5.405949406249999534, 9.363379034771803333, -128.7812500020483810 ) ) ;
#29843 = CARTESIAN_POINT ( 'NONE',  ( -5.405949406249996869, 9.363379034771805109, -6.843750002048371250 ) ) ;
#29844 = CARTESIAN_POINT ( 'NONE',  ( -10.81189881249999729, 6.242252689847871849, -137.2187500020483810 ) ) ;
#29845 = FACE_OUTER_BOUND ( 'NONE', #19146, .T. ) ;
#29846 = CARTESIAN_POINT ( 'NONE',  ( 9.999999999999998224, 0.000000000000000000, -200.0000000000000000 ) ) ;
#29847 = CARTESIAN_POINT ( 'NONE',  ( -5.000000000000003553, -8.660254037844383745, -164.5000000000000000 ) ) ;
#29848 = DIRECTION ( 'NONE',  ( -0.000000000000000000, -0.000000000000000000, -1.000000000000000000 ) ) ;
#29849 = CARTESIAN_POINT ( 'NONE',  ( -10.81189881249999729, 1.324075727343319199E-15, -75.59375000204838102 ) ) ;
#29850 = CARTESIAN_POINT ( 'NONE',  ( -10.81189881249999729, 1.324075727343319199E-15, -41.28125000204838102 ) ) ;
#29851 = CARTESIAN_POINT ( 'NONE',  ( -10.81189881249999729, 6.242252689847871849, -53.21875000204836681 ) ) ;
#29852 = LINE ( 'NONE', #32875, #23352 ) ;
#29853 = CARTESIAN_POINT ( 'NONE',  ( 10.81189881249999551, -6.242252689847874514, -161.9687500020484094 ) ) ;
#29854 = CARTESIAN_POINT ( 'NONE',  ( 9.999999999999996447, -5.773502691896262640, -126.6250000000000000 ) ) ;
#29855 = CARTESIAN_POINT ( 'NONE',  ( 10.81189881249999551, -6.242252689847874514, -139.6562500020484094 ) ) ;
#29856 = CARTESIAN_POINT ( 'NONE',  ( 9.999999999999998224, 0.000000000000000000, -23.37500000409675849 ) ) ;
#29857 = CARTESIAN_POINT ( 'NONE',  ( -10.00000000000000000, -5.773502691896251982, -115.5000000040967905 ) ) ;
#29858 = CARTESIAN_POINT ( 'NONE',  ( 7.070501591499377789E-16, 11.54700538379251284, -93.12500000000000000 ) ) ;
#29859 = EDGE_LOOP ( 'NONE', ( #3074, #29023, #10690, #4016 ) ) ;
#29860 = CARTESIAN_POINT ( 'NONE',  ( 7.644554776091147741E-16, 12.48450537969573659, -113.6562500020483952 ) ) ;
#29861 = CARTESIAN_POINT ( 'NONE',  ( -9.999999999999998224, 5.773502691896259087, -132.2500000040967905 ) ) ;
#29862 = DIRECTION ( 'NONE',  ( -1.000000000000000000, 0.000000000000000000, 0.000000000000000000 ) ) ;
#29863 = CARTESIAN_POINT ( 'NONE',  ( -2.293366432827344421E-15, -12.48450537969573659, -165.4062500020483810 ) ) ;
#29864 = CARTESIAN_POINT ( 'NONE',  ( 7.070501591499377789E-16, 11.54700538379251284, -41.00000000409676204 ) ) ;
#29865 = CARTESIAN_POINT ( 'NONE',  ( 10.81189881249999907, 6.242252689847868297, -50.90625000204837391 ) ) ;
#29866 = CARTESIAN_POINT ( 'NONE',  ( -10.81189881249999907, -6.242252689847864744, -164.1562500020484094 ) ) ;
#29867 = CARTESIAN_POINT ( 'NONE',  ( -5.405949406249996869, 9.363379034771805109, -137.3437500020484094 ) ) ;
#29868 = CARTESIAN_POINT ( 'NONE',  ( 7.070501591499376803E-16, 11.54700538379251284, -100.6250000000000000 ) ) ;
#29870 = ADVANCED_FACE ( 'NONE', ( #2707 ), #5521, .F. ) ;
#29869 = DIRECTION ( 'NONE',  ( 1.000000000000000000, 0.000000000000000000, 0.000000000000000000 ) ) ;
#29871 = ORIENTED_EDGE ( 'NONE', *, *, #15271, .F. ) ;
#29872 = EDGE_CURVE ( 'NONE', #38366, #19560, #3963, .T. ) ;
#29873 = DIRECTION ( 'NONE',  ( 0.000000000000000000, -1.000000000000000000, 0.000000000000000000 ) ) ;
#29875 = EDGE_LOOP ( 'NONE', ( #34877, #25846 ) ) ;
#29874 = CARTESIAN_POINT ( 'NONE',  ( -5.405949406250003975, -9.363379034771801557, -72.53125000204838102 ) ) ;
#29876 = PERSON_AND_ORGANIZATION ( #11915, #17965 ) ;
#29878 = ORIENTED_EDGE ( 'NONE', *, *, #25157, .T. ) ;
#29877 = CARTESIAN_POINT ( 'NONE',  ( -10.81189881249999907, -6.242252689847864744, -118.9687500020483810 ) ) ;
#29879 = ORIENTED_EDGE ( 'NONE', *, *, #5615, .F. ) ;
#29880 = CARTESIAN_POINT ( 'NONE',  ( 10.81189881249999729, 6.242252689847867408, -19.21875000204837747 ) ) ;
#29881 = CARTESIAN_POINT ( 'NONE',  ( -2.293366432827344421E-15, -12.48450537969573659, -0.4062500020483658103 ) ) ;
#29882 = CARTESIAN_POINT ( 'NONE',  ( -5.405949406250003975, -9.363379034771801557, -45.34375000204838102 ) ) ;
#29883 = CARTESIAN_POINT ( 'NONE',  ( -2.121150477449813534E-15, -11.54700538379251284, -134.3750000000000000 ) ) ;
#29884 = CARTESIAN_POINT ( 'NONE',  ( 0.000000000000000000, 0.000000000000000000, -200.0000000000000000 ) ) ;
#29885 = CARTESIAN_POINT ( 'NONE',  ( 10.81189881249999551, -6.242252689847874514, -178.4687500020484094 ) ) ;
#29886 = CARTESIAN_POINT ( 'NONE',  ( 10.81189881249999729, 0.000000000000000000, -169.3437500020484094 ) ) ;
#29887 =( BOUNDED_CURVE ( )  B_SPLINE_CURVE ( 2, ( #25562, #41290, #1830, #22524, #35697, #11944, #5270 ),
 .UNSPECIFIED., .F., .F. ) 
 B_SPLINE_CURVE_WITH_KNOTS ( ( 3, 2, 2, 3 ),
 ( 0.9104477611940301474, 0.9116915422885575326, 0.9129353233830848069, 0.9141791044776121922 ),
 .UNSPECIFIED. ) 
 CURVE ( )  GEOMETRIC_REPRESENTATION_ITEM ( )  RATIONAL_B_SPLINE_CURVE ( ( 0.9999999999999641398, 0.8660254037844745678, 1.000000000000000000, 0.8660254037844387076, 1.000000000000000000, 0.8660254037844148378, 1.000000000000023981 ) ) 
 REPRESENTATION_ITEM ( '' )  );
#29888 = CARTESIAN_POINT ( 'NONE',  ( 5.405949406249992428, -9.363379034771808662, -148.5937500020483810 ) ) ;
#29889 = CARTESIAN_POINT ( 'NONE',  ( 10.81189881249999729, 6.242252689847867408, -166.2187500020483810 ) ) ;
#29890 = CARTESIAN_POINT ( 'NONE',  ( -10.00000000000076916, 5.773502691895813221, -106.7500000040967620 ) ) ;
#29891 = CARTESIAN_POINT ( 'NONE',  ( 10.00000000000012257, -5.773502691896188921, -161.5000000040968189 ) ) ;
#29892 = CARTESIAN_POINT ( 'NONE',  ( -9.999999999999998224, 1.224646799147353059E-15, -190.2500000000000000 ) ) ;
#29893 = CARTESIAN_POINT ( 'NONE',  ( 5.405949406249999534, 9.363379034771803333, -97.09375000204838102 ) ) ;
#29894 = CARTESIAN_POINT ( 'NONE',  ( -4.999999999999996447, 8.660254037844387298, -34.49999999999997158 ) ) ;
#29895 = CARTESIAN_POINT ( 'NONE',  ( 5.405949406249992428, -9.363379034771808662, -69.28125000204838102 ) ) ;
#29896 = FACE_OUTER_BOUND ( 'NONE', #6972, .T. ) ;
#29897 = CARTESIAN_POINT ( 'NONE',  ( -2.293366432827344421E-15, -12.48450537969573659, -186.2187500020484094 ) ) ;
#29898 = EDGE_CURVE ( 'NONE', #516, #223, #12335, .T. ) ;
#29899 = CARTESIAN_POINT ( 'NONE',  ( -10.81189881249999729, 1.324075727343319199E-15, -119.2812500020483952 ) ) ;
#29900 = CARTESIAN_POINT ( 'NONE',  ( -10.81189881249999729, 6.242252689847871849, -165.9062500020483810 ) ) ;
#29901 = CARTESIAN_POINT ( 'NONE',  ( 5.405949406249992428, -9.363379034771808662, -55.78125000204836681 ) ) ;
#29902 = CARTESIAN_POINT ( 'NONE',  ( -9.999999999999998224, 1.224646799147353059E-15, -141.1250000040967905 ) ) ;
#29903 = CARTESIAN_POINT ( 'NONE',  ( 9.999999999999998224, 0.000000000000000000, -112.9999999999999858 ) ) ;
#29904 = ORIENTED_EDGE ( 'NONE', *, *, #23199, .T. ) ;
#29905 = CARTESIAN_POINT ( 'NONE',  ( -10.81189881249999729, 6.242252689847871849, -134.4062500020483810 ) ) ;
#29906 = CARTESIAN_POINT ( 'NONE',  ( -2.293366432827344421E-15, -12.48450537969573659, -151.9062500020483810 ) ) ;
#29907 = CARTESIAN_POINT ( 'NONE',  ( -10.81189881249999729, 6.242252689847871849, -185.4062500020484094 ) ) ;
#29908 = CARTESIAN_POINT ( 'NONE',  ( 4.999999999999992006, -8.660254037844389075, -43.12500000409677625 ) ) ;
#29909 = CARTESIAN_POINT ( 'NONE',  ( -2.293366432827344421E-15, -12.48450537969573659, -81.21875000204838102 ) ) ;
#29910 = ORIENTED_EDGE ( 'NONE', *, *, #18589, .F. ) ;
#29911 = CARTESIAN_POINT ( 'NONE',  ( 9.999999999999996447, -5.773502691896262640, -59.12499999999999289 ) ) ;
#29912 = CARTESIAN_POINT ( 'NONE',  ( 7.644554776091147741E-16, 12.48450537969573659, -179.4687500020483810 ) ) ;
#29913 = CARTESIAN_POINT ( 'NONE',  ( -9.999999999999998224, 5.773502691896259087, -67.75000000409677625 ) ) ;
#29914 = CARTESIAN_POINT ( 'NONE',  ( -2.121150477449813534E-15, -11.54700538379251284, -171.8750000000000284 ) ) ;
#29915 = CARTESIAN_POINT ( 'NONE',  ( -9.999999999999998224, 1.224646799147353059E-15, -175.6250000040968189 ) ) ;
#29916 = CARTESIAN_POINT ( 'NONE',  ( -10.81189881249999729, 6.242252689847871849, -77.40625000204838102 ) ) ;
#29917 = CARTESIAN_POINT ( 'NONE',  ( 10.81189881249999729, 0.000000000000000000, -57.03125000204836681 ) ) ;
#29918 = CARTESIAN_POINT ( 'NONE',  ( -2.121150477449813534E-15, -11.54700538379251284, -56.75000000409676915 ) ) ;
#29919 = CARTESIAN_POINT ( 'NONE',  ( -10.81189881249999907, -6.242252689847864744, -9.468750002048357928 ) ) ;
#29920 = CYLINDRICAL_SURFACE ( 'NONE', #33841, 9.999999999999998224 ) ;
#29921 = CARTESIAN_POINT ( 'NONE',  ( 7.644554776091147741E-16, 12.48450537969573659, -187.1562500020484094 ) ) ;
#29922 = CARTESIAN_POINT ( 'NONE',  ( -5.405949406249996869, 9.363379034771805109, -16.03125000204835970 ) ) ;
#29923 = CARTESIAN_POINT ( 'NONE',  ( -5.405949406250003975, -9.363379034771801557, -0.3437500020483652552 ) ) ;
#29925 = EDGE_CURVE ( 'NONE', #27517, #34879, #1202, .T. ) ;
#29924 = CARTESIAN_POINT ( 'NONE',  ( -9.999999999999742428, -5.773502691896402084, -118.1249999999999858 ) ) ;
#29926 = CARTESIAN_POINT ( 'NONE',  ( -2.121150477449813534E-15, -11.54700538379251284, -45.87499999999996447 ) ) ;
#29927 = FACE_OUTER_BOUND ( 'NONE', #11115, .T. ) ;
#29928 = EDGE_CURVE ( 'NONE', #30365, #12272, #9593, .T. ) ;
#29929 = CARTESIAN_POINT ( 'NONE',  ( 9.999999999999998224, 0.000000000000000000, -168.5000000000000000 ) ) ;
#29930 = CARTESIAN_POINT ( 'NONE',  ( -9.999999999999998224, 1.224646799147353059E-15, -200.0000000000000000 ) ) ;
#29931 = EDGE_CURVE ( 'NONE', #6986, #3313, #26424, .T. ) ;
#29933 = EDGE_LOOP ( 'NONE', ( #12085, #13556, #38848, #21796 ) ) ;
#29932 = CARTESIAN_POINT ( 'NONE',  ( 10.81189881249999729, 0.000000000000000000, -94.53125000204838102 ) ) ;
#29934 = CARTESIAN_POINT ( 'NONE',  ( 5.000000000000000000, 8.660254037844385522, -107.1250000040967763 ) ) ;
#29936 = VERTEX_POINT ( 'NONE', #22767 ) ;
#29935 = CARTESIAN_POINT ( 'NONE',  ( -5.000000000000003553, -8.660254037844383745, -154.0000000000000000 ) ) ;
#29937 = ORIENTED_EDGE ( 'NONE', *, *, #42299, .T. ) ;
#29938 =( BOUNDED_CURVE ( )  B_SPLINE_CURVE ( 2, ( #24015, #3734, #16864, #30067, #39969, #37156, #20121 ),
 .UNSPECIFIED., .F., .F. ) 
 B_SPLINE_CURVE_WITH_KNOTS ( ( 3, 2, 2, 3 ),
 ( 0.2947761194029852039, 0.2960199004975125336, 0.2972636815920398634, 0.2985074626865671932 ),
 .UNSPECIFIED. ) 
 CURVE ( )  GEOMETRIC_REPRESENTATION_ITEM ( )  RATIONAL_B_SPLINE_CURVE ( ( 0.9999999999999880096, 0.8660254037844506980, 1.000000000000000000, 0.8660254037844387076, 1.000000000000000000, 0.8660254037844327124, 1.000000000000005995 ) ) 
 REPRESENTATION_ITEM ( '' )  );
#29939 = CARTESIAN_POINT ( 'NONE',  ( 10.81189881249999551, -6.242252689847874514, -35.96875000204835260 ) ) ;
#29940 = CARTESIAN_POINT ( 'NONE',  ( -5.405949406250003975, -9.363379034771801557, -18.53125000204835970 ) ) ;
#29941 = CARTESIAN_POINT ( 'NONE',  ( -10.81189881249999729, 1.324075727343319199E-15, -71.09375000204836681 ) ) ;
#29942 = CARTESIAN_POINT ( 'NONE',  ( 4.999999999999992006, -8.660254037844389075, -115.1250000040967905 ) ) ;
#29943 = CARTESIAN_POINT ( 'NONE',  ( -10.81189881249999729, 6.242252689847871849, -192.7187500020483810 ) ) ;
#29944 = CARTESIAN_POINT ( 'NONE',  ( 10.81189881249999551, -6.242252689847874514, -149.9687500020483810 ) ) ;
#29945 = EDGE_CURVE ( 'NONE', #25155, #10539, #33479, .T. ) ;
#29946 = CARTESIAN_POINT ( 'NONE',  ( -9.999999999999998224, 1.224646799147353059E-15, -79.62500000409677625 ) ) ;
#29947 = MANIFOLD_SOLID_BREP ( 'Cut-Extrude1', #28070 ) ;
#29948 = CARTESIAN_POINT ( 'NONE',  ( -1.040834085586084257E-14, 145.0000000000000000, 7.500000000000007105 ) ) ;
#29949 = CARTESIAN_POINT ( 'NONE',  ( -5.405949406250003975, -9.363379034771801557, -147.5312500020483810 ) ) ;
#29950 = CARTESIAN_POINT ( 'NONE',  ( 7.070501591499377789E-16, 11.54700538379251284, -3.500000004096760264 ) ) ;
#29951 = CARTESIAN_POINT ( 'NONE',  ( 4.999999999999992006, -8.660254037844389075, -103.1250000040967763 ) ) ;
#29952 = CARTESIAN_POINT ( 'NONE',  ( -2.293366432827344421E-15, -12.48450537969573659, -117.2187500020483952 ) ) ;
#29953 = CARTESIAN_POINT ( 'NONE',  ( -1.040834085586084257E-14, 20.00000000000000711, 32.49999999999999289 ) ) ;
#29954 = CARTESIAN_POINT ( 'NONE',  ( -5.405949406250003975, -9.363379034771801557, -87.53125000204838102 ) ) ;
#29955 = CARTESIAN_POINT ( 'NONE',  ( -10.81189881249999729, -6.242252689847864744, -111.4687500020483810 ) ) ;
#29956 = CARTESIAN_POINT ( 'NONE',  ( 7.644554776091147741E-16, 12.48450537969573659, -72.96875000204835260 ) ) ;
#29957 = CARTESIAN_POINT ( 'NONE',  ( 7.644554776091147741E-16, 12.48450537969573659, -76.15625000204839523 ) ) ;
#29958 = CARTESIAN_POINT ( 'NONE',  ( -10.00000000000000000, -5.773502691896251982, -160.5000000040967905 ) ) ;
#29959 = FACE_OUTER_BOUND ( 'NONE', #25746, .T. ) ;
#29960 = CARTESIAN_POINT ( 'NONE',  ( 10.81189881249999729, 6.242252689847867408, -158.9062500020483810 ) ) ;
#29961 = CARTESIAN_POINT ( 'NONE',  ( -5.405949406250003975, -9.363379034771801557, -176.0312500020483810 ) ) ;
#29962 = CARTESIAN_POINT ( 'NONE',  ( 9.999999999999998224, 0.000000000000000000, -129.5000000000000000 ) ) ;
#29963 = CARTESIAN_POINT ( 'NONE',  ( -5.405949406249996869, 9.363379034771805109, -8.343750002048345493 ) ) ;
#29964 = CARTESIAN_POINT ( 'NONE',  ( -9.999999999999998224, 1.224646799147353059E-15, -109.2499999999999858 ) ) ;
#29965 = CARTESIAN_POINT ( 'NONE',  ( 5.405949406249999534, 9.363379034771803333, -109.0937500020483810 ) ) ;
#29966 = CARTESIAN_POINT ( 'NONE',  ( -9.999999999999998224, 1.224646799147353059E-15, -83.74999999999997158 ) ) ;
#29967 = CARTESIAN_POINT ( 'NONE',  ( 10.81189881249999729, 0.000000000000000000, -9.031250002048352599 ) ) ;
#29968 = CARTESIAN_POINT ( 'NONE',  ( 7.070501591499377789E-16, 11.54700538379251284, -87.50000000409677625 ) ) ;
#29969 = CARTESIAN_POINT ( 'NONE',  ( -9.999999999999998224, 1.224646799147353059E-15, -115.2499999999999858 ) ) ;
#29970 = CARTESIAN_POINT ( 'NONE',  ( 10.81189881249999907, 6.242252689847868297, -104.9062500020483952 ) ) ;
#29971 = CARTESIAN_POINT ( 'NONE',  ( 10.81189881249999551, -6.242252689847874514, -82.65625000204838102 ) ) ;
#29972 = ORIENTED_EDGE ( 'NONE', *, *, #19620, .F. ) ;
#29973 = CARTESIAN_POINT ( 'NONE',  ( 5.000000000000000000, 8.660254037844385522, -87.62500000409677625 ) ) ;
#29974 = CARTESIAN_POINT ( 'NONE',  ( -9.999999999999998224, 1.224646799147353059E-15, -121.6250000040967905 ) ) ;
#29975 = CARTESIAN_POINT ( 'NONE',  ( 10.81189881249999729, 0.000000000000000000, -41.84375000204837391 ) ) ;
#29976 = ORIENTED_EDGE ( 'NONE', *, *, #8284, .T. ) ;
#29977 = CARTESIAN_POINT ( 'NONE',  ( -2.121150477449813534E-15, -11.54700538379251284, -8.374999999999976907 ) ) ;
#29978 = CARTESIAN_POINT ( 'NONE',  ( 10.00000000000000000, 5.773502691896255534, -142.8750000000000000 ) ) ;
#29979 = CARTESIAN_POINT ( 'NONE',  ( 0.000000000000000000, 0.000000000000000000, -200.0000000000000000 ) ) ;
#29980 = CARTESIAN_POINT ( 'NONE',  ( -5.000000000000003553, -8.660254037844383745, -10.37500000409674605 ) ) ;
#29981 = AXIS2_PLACEMENT_3D ( 'NONE', #31376, #1810, #14505 ) ;
#29982 = CARTESIAN_POINT ( 'NONE',  ( 5.000000000000000000, 8.660254037844385522, -193.7500000000000000 ) ) ;
#29983 = CARTESIAN_POINT ( 'NONE',  ( 0.000000000000000000, 0.000000000000000000, -99.99999999999998579 ) ) ;
#29985 = ORIENTED_EDGE ( 'NONE', *, *, #26372, .T. ) ;
#29984 = CARTESIAN_POINT ( 'NONE',  ( 10.81189881249999551, -6.242252689847874514, -121.6562500020483952 ) ) ;
#29986 = VERTEX_POINT ( 'NONE', #3553 ) ;
#29987 = CARTESIAN_POINT ( 'NONE',  ( -10.81189881249999729, 6.242252689847871849, -45.90625000204836681 ) ) ;
#29988 = APPROVAL_ROLE ( '' ) ;
#29989 = EDGE_CURVE ( 'NONE', #22184, #37944, #10220, .T. ) ;
#29990 = CARTESIAN_POINT ( 'NONE',  ( -5.405949406250003975, -9.363379034771801557, -97.84375000204838102 ) ) ;
#29991 = CARTESIAN_POINT ( 'NONE',  ( 10.81189881249999551, -6.242252689847874514, -124.6562500020483952 ) ) ;
#29992 = ORIENTED_EDGE ( 'NONE', *, *, #36775, .T. ) ;
#29993 = CARTESIAN_POINT ( 'NONE',  ( 9.999999999999998224, 0.000000000000000000, -111.4999999999999858 ) ) ;
#29994 = CARTESIAN_POINT ( 'NONE',  ( -9.999999999999227285, -5.773502691896698735, -126.0000000040967478 ) ) ;
#29995 = CARTESIAN_POINT ( 'NONE',  ( -2.293366432827344421E-15, -12.48450537969573659, -174.4062500020483810 ) ) ;
#29996 = CARTESIAN_POINT ( 'NONE',  ( -4.999999999999996447, 8.660254037844387298, -154.8750000040967905 ) ) ;
#29997 = CARTESIAN_POINT ( 'NONE',  ( -10.81189881249999729, 1.324075727343319199E-15, -131.0937500020483810 ) ) ;
#29998 = CARTESIAN_POINT ( 'NONE',  ( -10.81189881249999907, -6.242252689847864744, -93.46875000204836681 ) ) ;
#29999 = CARTESIAN_POINT ( 'NONE',  ( -9.999999999999998224, 1.224646799147353059E-15, -112.6250000040967763 ) ) ;
#30000 = CARTESIAN_POINT ( 'NONE',  ( -10.81189881249999729, 6.242252689847871849, -104.4062500020483810 ) ) ;
#30001 = CARTESIAN_POINT ( 'NONE',  ( 9.999999999999996447, -5.773502691896262640, -184.0000000040968189 ) ) ;
#30002 = CARTESIAN_POINT ( 'NONE',  ( -5.405949406250003975, -9.363379034771801557, -114.3437500020483810 ) ) ;
#30003 = CARTESIAN_POINT ( 'NONE',  ( 5.405949406249999534, 9.363379034771803333, -184.2812500020484094 ) ) ;
#30004 = AXIS2_PLACEMENT_3D ( 'NONE', #41185, #28059, #31732 ) ;
#30005 = CARTESIAN_POINT ( 'NONE',  ( 9.999999999999227285, 5.773502691896701400, -108.3749999999999289 ) ) ;
#30006 = CARTESIAN_POINT ( 'NONE',  ( 10.00000000000051159, -5.773502691895965988, -113.5000000040967620 ) ) ;
#30007 = CARTESIAN_POINT ( 'NONE',  ( -5.000000000000003553, -8.660254037844383745, -0.9999999999999731326 ) ) ;
#30008 = CARTESIAN_POINT ( 'NONE',  ( -10.81189881249999729, 6.242252689847871849, -56.21875000204837391 ) ) ;
#30009 = CARTESIAN_POINT ( 'NONE',  ( 5.405949406249992428, -9.363379034771808662, -40.59375000204837391 ) ) ;
#30010 = CARTESIAN_POINT ( 'NONE',  ( -2.121150477449813534E-15, -11.54700538379251284, -181.2500000040967905 ) ) ;
#30011 = CARTESIAN_POINT ( 'NONE',  ( 10.81189881249999551, -6.242252689847874514, -19.65625000204837747 ) ) ;
#30012 = CARTESIAN_POINT ( 'NONE',  ( -5.405949406250003975, -9.363379034771801557, -31.84375000204836681 ) ) ;
#30013 = CARTESIAN_POINT ( 'NONE',  ( -9.999999999999998224, 1.224646799147353059E-15, -120.1250000040967905 ) ) ;
#30014 = CARTESIAN_POINT ( 'NONE',  ( 5.405949406249992428, -9.363379034771808662, -138.0937500020483810 ) ) ;
#30015 = CARTESIAN_POINT ( 'NONE',  ( -4.999999999999996447, 8.660254037844387298, -109.4999999999999858 ) ) ;
#30016 = CARTESIAN_POINT ( 'NONE',  ( -2.293366432827344421E-15, -12.48450537969573659, -34.90625000204835970 ) ) ;
#30017 = CARTESIAN_POINT ( 'NONE',  ( 9.999999999999998224, 1.224646799147353059E-15, -99.99999999999998579 ) ) ;
#30018 = CARTESIAN_POINT ( 'NONE',  ( 10.00000000000000000, 5.773502691896255534, -57.37499999999997868 ) ) ;
#30019 = CARTESIAN_POINT ( 'NONE',  ( -2.293366432827344421E-15, -12.48450537969573659, -132.4062500020483810 ) ) ;
#30020 = CARTESIAN_POINT ( 'NONE',  ( -10.81189881249999729, 6.242252689847871849, -107.4062500020483668 ) ) ;
#30021 = ORIENTED_EDGE ( 'NONE', *, *, #7149, .T. ) ;
#30022 = DIRECTION ( 'NONE',  ( -0.000000000000000000, -0.000000000000000000, 1.000000000000000000 ) ) ;
#30023 = CARTESIAN_POINT ( 'NONE',  ( -9.999999999999998224, 1.224646799147353059E-15, -105.1250000040967763 ) ) ;
#30024 = MANIFOLD_SOLID_BREP ( 'Cut-Extrude1', #38410 ) ;
#30025 = CARTESIAN_POINT ( 'NONE',  ( 9.999999999999998224, 0.000000000000000000, -106.9999999999999858 ) ) ;
#30026 = CARTESIAN_POINT ( 'NONE',  ( -10.81189881249999729, 6.242252689847871849, -68.21875000204838102 ) ) ;
#30027 = VERTEX_POINT ( 'NONE', #16051 ) ;
#30028 = CARTESIAN_POINT ( 'NONE',  ( -2.121150477449813534E-15, -11.54700538379251284, -33.87499999999996447 ) ) ;
#30029 = CARTESIAN_POINT ( 'NONE',  ( 10.00000000000000000, 5.773502691896255534, -18.75000000409676915 ) ) ;
#30030 = CARTESIAN_POINT ( 'NONE',  ( -5.405949406249996869, 9.363379034771805109, -44.53125000204838102 ) ) ;
#30031 = CARTESIAN_POINT ( 'NONE',  ( -10.00000000000051337, 5.773502691895962435, -124.7500000040967620 ) ) ;
#30032 =( BOUNDED_CURVE ( )  B_SPLINE_CURVE ( 2, ( #41369, #11806, #13806, #40149, #5139, #28018, #14012 ),
 .UNSPECIFIED., .F., .F. ) 
 B_SPLINE_CURVE_WITH_KNOTS ( ( 3, 2, 2, 3 ),
 ( 0.1865671641791045166, 0.1878109452736318741, 0.1890547263681592594, 0.1902985074626866169 ),
 .UNSPECIFIED. ) 
 CURVE ( )  GEOMETRIC_REPRESENTATION_ITEM ( )  RATIONAL_B_SPLINE_CURVE ( ( 0.9999999999999970024, 0.8660254037844417052, 1.000000000000000000, 0.8660254037844387076, 1.000000000000000000, 0.8660254037844327124, 1.000000000000005995 ) ) 
 REPRESENTATION_ITEM ( '' )  );
#30033 = CARTESIAN_POINT ( 'NONE',  ( 5.000000000000000000, 8.660254037844385522, -39.62500000409676915 ) ) ;
#30034 = VECTOR ( 'NONE', #36167, 1000.000000000000000 ) ;
#30035 = CARTESIAN_POINT ( 'NONE',  ( 9.999999999999998224, 0.000000000000000000, -57.87500000409676204 ) ) ;
#30036 = CARTESIAN_POINT ( 'NONE',  ( -2.293366432827344421E-15, -12.48450537969573659, -141.4062500020483810 ) ) ;
#30037 = CARTESIAN_POINT ( 'NONE',  ( 5.000000000000000000, 8.660254037844385522, -122.1250000040967905 ) ) ;
#30038 = VERTEX_POINT ( 'NONE', #16257 ) ;
#30039 = ORIENTED_EDGE ( 'NONE', *, *, #33871, .F. ) ;
#30040 = CARTESIAN_POINT ( 'NONE',  ( -4.999999999999996447, 8.660254037844387298, -126.3750000040967905 ) ) ;
#30041 = CARTESIAN_POINT ( 'NONE',  ( 0.000000000000000000, 0.000000000000000000, -99.99999999999998579 ) ) ;
#30042 = CARTESIAN_POINT ( 'NONE',  ( 10.81189881249999551, -6.242252689847874514, -170.9687500020483810 ) ) ;
#30043 = CARTESIAN_POINT ( 'NONE',  ( -10.81189881249999729, 1.324075727343319199E-15, -192.7812500020484094 ) ) ;
#30044 = CARTESIAN_POINT ( 'NONE',  ( 10.81189881249999729, 0.000000000000000000, -25.34375000204835970 ) ) ;
#30045 = CARTESIAN_POINT ( 'NONE',  ( -9.999999999998969713, -5.773502691896847949, -33.00000000409673362 ) ) ;
#30046 = CARTESIAN_POINT ( 'NONE',  ( 5.000000000000000000, 8.660254037844385522, -171.2500000000000000 ) ) ;
#30047 = CARTESIAN_POINT ( 'NONE',  ( 7.644554776091147741E-16, 12.48450537969573659, -158.4687500020483810 ) ) ;
#30048 = CARTESIAN_POINT ( 'NONE',  ( 10.81189881249999729, 0.000000000000000000, -133.3437500020484094 ) ) ;
#30049 = ADVANCED_FACE ( 'NONE', ( #115 ), #6570, .F. ) ;
#30050 = CARTESIAN_POINT ( 'NONE',  ( 7.070501591499376803E-16, 11.54700538379251284, -173.0000000040967905 ) ) ;
#30051 = CARTESIAN_POINT ( 'NONE',  ( -2.293366432827344421E-15, -12.48450537969573659, -123.2187500020483952 ) ) ;
#30052 = CARTESIAN_POINT ( 'NONE',  ( -9.999999999999998224, 5.773502691896259087, -193.7500000040967905 ) ) ;
#30053 = VECTOR ( 'NONE', #38479, 1000.000000000000000 ) ;
#30054 = CARTESIAN_POINT ( 'NONE',  ( -10.81189881249999729, 1.324075727343319199E-15, -134.2812500020483810 ) ) ;
#30056 = CARTESIAN_POINT ( 'NONE',  ( 10.81189881249999729, 0.000000000000000000, -10.34375000204834549 ) ) ;
#30055 =( BOUNDED_CURVE ( )  B_SPLINE_CURVE ( 2, ( #37352, #1318, #4758, #31535, #27642, #15093, #11224 ),
 .UNSPECIFIED., .F., .F. ) 
 B_SPLINE_CURVE_WITH_KNOTS ( ( 3, 2, 2, 3 ),
 ( 0.7611940298507464675, 0.7624378109452738528, 0.7636815920398011270, 0.7649253731343285123 ),
 .UNSPECIFIED. ) 
 CURVE ( )  GEOMETRIC_REPRESENTATION_ITEM ( )  RATIONAL_B_SPLINE_CURVE ( ( 0.9999999999999761302, 0.8660254037844625774, 1.000000000000000000, 0.8660254037844387076, 1.000000000000000000, 0.8660254037844267172, 1.000000000000011990 ) ) 
 REPRESENTATION_ITEM ( '' )  );
#30057 = CARTESIAN_POINT ( 'NONE',  ( -10.81189881249999729, 1.324075727343319199E-15, -140.0937500020483810 ) ) ;
#30058 = CARTESIAN_POINT ( 'NONE',  ( -1.040834085586084257E-14, -125.0000000000000000, 42.49999999999999289 ) ) ;
#30059 = VECTOR ( 'NONE', #2547, 1000.000000000000000 ) ;
#30060 = CARTESIAN_POINT ( 'NONE',  ( 5.000000000000000000, 8.660254037844385522, -25.74999999999996803 ) ) ;
#30061 = CARTESIAN_POINT ( 'NONE',  ( -9.999999999999998224, 5.773502691896259087, -152.8749999999999716 ) ) ;
#30062 = DIRECTION ( 'NONE',  ( -0.000000000000000000, -0.000000000000000000, 1.000000000000000000 ) ) ;
#30063 = CARTESIAN_POINT ( 'NONE',  ( -2.293366432827344421E-15, -12.48450537969573659, -84.21875000204835260 ) ) ;
#30064 = CARTESIAN_POINT ( 'NONE',  ( 5.405949406249999534, 9.363379034771803333, -71.59375000204836681 ) ) ;
#30065 = CARTESIAN_POINT ( 'NONE',  ( 5.405949406249992428, -9.363379034771808662, -45.28125000204838102 ) ) ;
#30066 = CARTESIAN_POINT ( 'NONE',  ( -5.405949406250003975, -9.363379034771801557, -57.34375000204835970 ) ) ;
#30067 = CARTESIAN_POINT ( 'NONE',  ( -2.121150477449813534E-15, -11.54700538379251284, -139.2500000040967905 ) ) ;
#30068 = CARTESIAN_POINT ( 'NONE',  ( -2.293366432827344421E-15, -12.48450537969573659, -165.2187500020484094 ) ) ;
#30069 = CARTESIAN_POINT ( 'NONE',  ( 7.070501591499377789E-16, 11.54700538379251284, -130.6250000000000000 ) ) ;
#30070 = CARTESIAN_POINT ( 'NONE',  ( 5.405949406249999534, 9.363379034771803333, -140.7812500020483810 ) ) ;
#30071 = FACE_OUTER_BOUND ( 'NONE', #2107, .T. ) ;
#30072 = CARTESIAN_POINT ( 'NONE',  ( 9.999999999999996447, -5.773502691896262640, -81.62499999999998579 ) ) ;
#30073 = CARTESIAN_POINT ( 'NONE',  ( -10.81189881249999729, 1.324075727343319199E-15, -20.28125000204836326 ) ) ;
#30074 = ORIENTED_EDGE ( 'NONE', *, *, #32848, .F. ) ;
#30075 =( BOUNDED_CURVE ( )  B_SPLINE_CURVE ( 2, ( #29796, #452, #6692, #5482, #28794, #25341, #3679 ),
 .UNSPECIFIED., .F., .F. ) 
 B_SPLINE_CURVE_WITH_KNOTS ( ( 3, 2, 2, 3 ),
 ( 0.06716417910447768091, 0.06840796019900503844, 0.06965174129353240984, 0.07089552238805976736 ),
 .UNSPECIFIED. ) 
 CURVE ( )  GEOMETRIC_REPRESENTATION_ITEM ( )  RATIONAL_B_SPLINE_CURVE ( ( 0.9999999999999924505, 0.8660254037844461461, 1.000000000000000000, 0.8660254037844387076, 1.000000000000000000, 0.8660254037844312691, 1.000000000000007550 ) ) 
 REPRESENTATION_ITEM ( '' )  );
#30076 = CARTESIAN_POINT ( 'NONE',  ( 5.405949406249999534, 9.363379034771803333, -113.7812500020483952 ) ) ;
#30077 = CARTESIAN_POINT ( 'NONE',  ( -9.999999999999998224, 1.224646799147353059E-15, -129.1250000040967620 ) ) ;
#30078 = LINE ( 'NONE', #16661, #7792 ) ;
#30079 = CARTESIAN_POINT ( 'NONE',  ( -10.81189881249999729, 6.242252689847871849, -167.4062500020483810 ) ) ;
#30080 = CARTESIAN_POINT ( 'NONE',  ( 9.999999999999998224, 0.000000000000000000, -39.87500000409676915 ) ) ;
#30081 = DIRECTION ( 'NONE',  ( -0.000000000000000000, -0.000000000000000000, 1.000000000000000000 ) ) ;
#30082 = CARTESIAN_POINT ( 'NONE',  ( 10.81189881249999907, 6.242252689847868297, -52.40625000204838102 ) ) ;
#30083 =( BOUNDED_CURVE ( )  B_SPLINE_CURVE ( 2, ( #20984, #21409, #21196, #41031, #30924, #34383, #8479 ),
 .UNSPECIFIED., .F., .F. ) 
 B_SPLINE_CURVE_WITH_KNOTS ( ( 3, 2, 2, 3 ),
 ( 0.09328358208955218889, 0.09452736318407958804, 0.09577114427860700108, 0.09701492537313441411 ),
 .UNSPECIFIED. ) 
 CURVE ( )  GEOMETRIC_REPRESENTATION_ITEM ( )  RATIONAL_B_SPLINE_CURVE ( ( 1.000000000000005995, 0.8660254037844327124, 1.000000000000000000, 0.8660254037844387076, 1.000000000000000000, 0.8660254037844297148, 1.000000000000008882 ) ) 
 REPRESENTATION_ITEM ( '' )  );
#30084 = CARTESIAN_POINT ( 'NONE',  ( 5.000000000000000000, 8.660254037844385522, -45.24999999999998579 ) ) ;
#30085 = CARTESIAN_POINT ( 'NONE',  ( -10.81189881249999907, -6.242252689847864744, -161.1562500020484094 ) ) ;
#30086 = CARTESIAN_POINT ( 'NONE',  ( -10.81189881249999729, 1.324075727343319199E-15, -135.5937500020483810 ) ) ;
#30087 = DIRECTION ( 'NONE',  ( -0.000000000000000000, -0.000000000000000000, 1.000000000000000000 ) ) ;
#30088 = CARTESIAN_POINT ( 'NONE',  ( -10.00000000000051337, 5.773502691895962435, -149.8750000000000000 ) ) ;
#30089 = ORIENTED_EDGE ( 'NONE', *, *, #17764, .T. ) ;
#30090 = CARTESIAN_POINT ( 'NONE',  ( -79.99999999999995737, -40.00000000000000711, -160.0000000000000000 ) ) ;
#30091 = VECTOR ( 'NONE', #605, 1000.000000000000000 ) ;
#30093 = ORIENTED_EDGE ( 'NONE', *, *, #27968, .F. ) ;
#30092 = CARTESIAN_POINT ( 'NONE',  ( 7.644554776091147741E-16, 12.48450537969573659, -73.15625000204836681 ) ) ;
#30095 = EDGE_LOOP ( 'NONE', ( #39732, #1740, #12414, #32062 ) ) ;
#30094 = CARTESIAN_POINT ( 'NONE',  ( -10.81189881249999729, 6.242252689847871849, -117.7187500020483952 ) ) ;
#30096 = CARTESIAN_POINT ( 'NONE',  ( -10.81189881249999729, 6.242252689847871849, -24.71875000204837036 ) ) ;
#30097 = CARTESIAN_POINT ( 'NONE',  ( -10.81189881249999729, 6.242252689847871849, -197.2187500020484379 ) ) ;
#30098 = CARTESIAN_POINT ( 'NONE',  ( -10.81189881249999907, -6.242252689847864744, -46.96875000204835970 ) ) ;
#30099 = CYLINDRICAL_SURFACE ( 'NONE', #26066, 9.999999999999998224 ) ;
#30100 = DIRECTION ( 'NONE',  ( -0.000000000000000000, -0.000000000000000000, -1.000000000000000000 ) ) ;
#30101 = CARTESIAN_POINT ( 'NONE',  ( -2.293366432827344421E-15, -12.48450537969573659, -180.2187500020484094 ) ) ;
#30102 = CARTESIAN_POINT ( 'NONE',  ( 10.81189881249999729, 0.000000000000000000, -172.3437500020484094 ) ) ;
#30103 = CARTESIAN_POINT ( 'NONE',  ( -2.293366432827344421E-15, -12.48450537969573659, -153.2187500020483810 ) ) ;
#30104 = CARTESIAN_POINT ( 'NONE',  ( -10.81189881249999729, 6.242252689847871849, -161.2187500020483810 ) ) ;
#30105 = DIRECTION ( 'NONE',  ( 1.000000000000000000, 0.000000000000000000, 0.000000000000000000 ) ) ;
#30106 = FACE_OUTER_BOUND ( 'NONE', #26419, .T. ) ;
#30107 = CARTESIAN_POINT ( 'NONE',  ( -5.000000000000003553, -8.660254037844383745, -181.0000000000000000 ) ) ;
#30108 = CARTESIAN_POINT ( 'NONE',  ( -5.405949406249996869, 9.363379034771805109, -99.84375000204838102 ) ) ;
#30109 = CYLINDRICAL_SURFACE ( 'NONE', #7252, 9.999999999999998224 ) ;
#30110 = CARTESIAN_POINT ( 'NONE',  ( 5.405949406249992428, -9.363379034771808662, -66.28125000204838102 ) ) ;
#30111 = CARTESIAN_POINT ( 'NONE',  ( 9.999999999999998224, 0.000000000000000000, -134.0000000000000000 ) ) ;
#30112 = EDGE_CURVE ( 'NONE', #31960, #24932, #3714, .T. ) ;
#30113 = CARTESIAN_POINT ( 'NONE',  ( -2.293366432827344421E-15, -12.48450537969573659, -183.2187500020484094 ) ) ;
#30114 = CARTESIAN_POINT ( 'NONE',  ( -10.81189881249999729, 6.242252689847871849, -125.4062500020483810 ) ) ;
#30115 = CARTESIAN_POINT ( 'NONE',  ( -10.81189881249999729, 1.324075727343319199E-15, -161.2812500020484094 ) ) ;
#30116 = CARTESIAN_POINT ( 'NONE',  ( -2.293366432827344421E-15, -12.48450537969573659, -55.90625000204838102 ) ) ;
#30117 = CARTESIAN_POINT ( 'NONE',  ( -9.999999999999998224, 5.773502691896259087, -139.7500000040967905 ) ) ;
#30118 = CARTESIAN_POINT ( 'NONE',  ( -2.121150477449813534E-15, -11.54700538379251284, -119.3749999999999858 ) ) ;
#30119 = ORIENTED_EDGE ( 'NONE', *, *, #21426, .T. ) ;
#30120 = CARTESIAN_POINT ( 'NONE',  ( 10.81189881249999729, 0.000000000000000000, -138.0312500020484094 ) ) ;
#30121 = CARTESIAN_POINT ( 'NONE',  ( -10.81189881249999907, -6.242252689847864744, -144.6562500020484094 ) ) ;
#30122 = CARTESIAN_POINT ( 'NONE',  ( -10.81189881249999907, -6.242252689847864744, -189.6562500020484094 ) ) ;
#30123 = CARTESIAN_POINT ( 'NONE',  ( -9.999999999999998224, 0.000000000000000000, -99.99999999999998579 ) ) ;
#30124 = CARTESIAN_POINT ( 'NONE',  ( -10.81189881249999729, 6.242252689847871849, -80.21875000204838102 ) ) ;
#30125 = ORIENTED_EDGE ( 'NONE', *, *, #20022, .T. ) ;
#30126 = CARTESIAN_POINT ( 'NONE',  ( -9.999999999999998224, 5.773502691896259087, -55.37499999999997868 ) ) ;
#30127 = CARTESIAN_POINT ( 'NONE',  ( -10.81189881249999729, 1.324075727343319199E-15, -182.0937500020483810 ) ) ;
#30128 = CARTESIAN_POINT ( 'NONE',  ( 4.999999999999992006, -8.660254037844389075, -68.62500000409677625 ) ) ;
#30129 = DIRECTION ( 'NONE',  ( -0.000000000000000000, -0.000000000000000000, 1.000000000000000000 ) ) ;
#30130 = CYLINDRICAL_SURFACE ( 'NONE', #11782, 9.999999999999998224 ) ;
#30131 = CARTESIAN_POINT ( 'NONE',  ( 5.405949406249999534, 9.363379034771803333, -73.28125000204838102 ) ) ;
#30132 = CARTESIAN_POINT ( 'NONE',  ( 10.81189881249999729, 6.242252689847867408, -56.90625000204838102 ) ) ;
#30133 = CARTESIAN_POINT ( 'NONE',  ( -4.999999999999996447, 8.660254037844387298, -51.37500000409675494 ) ) ;
#30134 = CARTESIAN_POINT ( 'NONE',  ( 10.81189881249999551, -6.242252689847874514, -13.46875000204836503 ) ) ;
#30135 = CARTESIAN_POINT ( 'NONE',  ( 10.00000000000051159, -5.773502691895965988, -151.0000000040967905 ) ) ;
#30136 = CARTESIAN_POINT ( 'NONE',  ( -10.81189881249999907, -6.242252689847864744, -182.1562500020483810 ) ) ;
#30137 = CARTESIAN_POINT ( 'NONE',  ( -10.81189881249999729, 6.242252689847871849, -6.906250002048365033 ) ) ;
#30138 = CARTESIAN_POINT ( 'NONE',  ( 9.999999999998969713, 5.773502691896851502, -85.87499999999995737 ) ) ;
#30139 = DIRECTION ( 'NONE',  ( 1.000000000000000000, 0.000000000000000000, 0.000000000000000000 ) ) ;
#30140 = CARTESIAN_POINT ( 'NONE',  ( -9.999999999999998224, 1.224646799147353059E-15, -57.12500000409676204 ) ) ;
#30141 = DIRECTION ( 'NONE',  ( -0.000000000000000000, -0.000000000000000000, -1.000000000000000000 ) ) ;
#30142 = DIRECTION ( 'NONE',  ( 1.000000000000000000, 0.000000000000000000, 0.000000000000000000 ) ) ;
#30144 = ORIENTED_EDGE ( 'NONE', *, *, #13116, .F. ) ;
#30143 = CARTESIAN_POINT ( 'NONE',  ( -2.293366432827344421E-15, -12.48450537969573659, -93.40625000204839523 ) ) ;
#30145 = CARTESIAN_POINT ( 'NONE',  ( -9.999999999999998224, 1.224646799147353059E-15, -106.6250000040967763 ) ) ;
#30147 = ORIENTED_EDGE ( 'NONE', *, *, #20349, .F. ) ;
#30146 = CARTESIAN_POINT ( 'NONE',  ( 10.81189881249999551, -6.242252689847874514, -101.9687500020483810 ) ) ;
#30148 =( BOUNDED_CURVE ( )  B_SPLINE_CURVE ( 2, ( #9712, #19634, #13357, #32817, #33027, #3457, #16592 ),
 .UNSPECIFIED., .F., .F. ) 
 B_SPLINE_CURVE_WITH_KNOTS ( ( 3, 2, 2, 3 ),
 ( 0.9552238805970153512, 0.9564676616915426255, 0.9577114427860698997, 0.9589552238805971740 ),
 .UNSPECIFIED. ) 
 CURVE ( )  GEOMETRIC_REPRESENTATION_ITEM ( )  RATIONAL_B_SPLINE_CURVE ( ( 0.9999999999999521494, 0.8660254037844865582, 1.000000000000000000, 0.8660254037844387076, 1.000000000000000000, 0.8660254037844267172, 1.000000000000011990 ) ) 
 REPRESENTATION_ITEM ( '' )  );
#30149 = VERTEX_POINT ( 'NONE', #36555 ) ;
#30150 = CARTESIAN_POINT ( 'NONE',  ( 7.644554776091147741E-16, 12.48450537969573659, -23.46875000204836326 ) ) ;
#30151 = CARTESIAN_POINT ( 'NONE',  ( 5.405949406249999534, 9.363379034771803333, -22.28125000204836326 ) ) ;
#30152 = CALENDAR_DATE ( 2026, 28, 9 ) ;
#30153 = CARTESIAN_POINT ( 'NONE',  ( 7.644554776091147741E-16, 12.48450537969573659, -68.46875000204838102 ) ) ;
#30154 = CARTESIAN_POINT ( 'NONE',  ( -5.000000000000003553, -8.660254037844383745, -173.8750000040968189 ) ) ;
#30155 = CARTESIAN_POINT ( 'NONE',  ( 5.000000000000000000, 8.660254037844385522, -48.24999999999998579 ) ) ;
#30156 = CARTESIAN_POINT ( 'NONE',  ( -5.405949406250003975, -9.363379034771801557, -195.3437500020484094 ) ) ;
#30157 = CARTESIAN_POINT ( 'NONE',  ( 10.81189881249999551, -6.242252689847874514, -148.4687500020484094 ) ) ;
#30158 = CARTESIAN_POINT ( 'NONE',  ( -9.999999999999998224, 1.224646799147353059E-15, -72.12500000409677625 ) ) ;
#30159 = LINE ( 'NONE', #23251, #42583 ) ;
#30160 = CARTESIAN_POINT ( 'NONE',  ( -10.81189881249999729, 1.324075727343319199E-15, -144.7812500020483810 ) ) ;
#30161 = CARTESIAN_POINT ( 'NONE',  ( -5.000000000000003553, -8.660254037844383745, -2.875000004096767370 ) ) ;
#30162 = CARTESIAN_POINT ( 'NONE',  ( 9.999999999999998224, 0.000000000000000000, -89.37500000409677625 ) ) ;
#30163 = CARTESIAN_POINT ( 'NONE',  ( 10.81189881249999907, 6.242252689847868297, -124.2187500020483952 ) ) ;
#30164 = CARTESIAN_POINT ( 'NONE',  ( -10.00000000000051337, 5.773502691895962435, -140.8750000000000000 ) ) ;
#30165 = CARTESIAN_POINT ( 'NONE',  ( 10.81189881249999729, 0.000000000000000000, -88.53125000204838102 ) ) ;
#30166 = ADVANCED_FACE ( 'NONE', ( #32907 ), #36349, .T. ) ;
#30167 = CARTESIAN_POINT ( 'NONE',  ( -10.81189881249999729, -6.242252689847864744, -100.9687500020483668 ) ) ;
#30168 = EDGE_CURVE ( 'NONE', #15363, #25538, #42599, .T. ) ;
#30169 = CARTESIAN_POINT ( 'NONE',  ( -10.81189881249999729, 6.242252689847871849, -69.71875000204838102 ) ) ;
#30170 = CARTESIAN_POINT ( 'NONE',  ( -2.293366432827344421E-15, -12.48450537969573659, -75.40625000204838102 ) ) ;
#30171 = CARTESIAN_POINT ( 'NONE',  ( -4.999999999999996447, 8.660254037844387298, -162.3750000040967905 ) ) ;
#30172 = ADVANCED_FACE ( 'NONE', ( #16897 ), #29671, .T. ) ;
#30173 = CARTESIAN_POINT ( 'NONE',  ( -10.81189881249999729, -6.242252689847864744, -156.6562500020484094 ) ) ;
#30174 = CARTESIAN_POINT ( 'NONE',  ( -2.293366432827344421E-15, -12.48450537969573659, -171.4062500020484379 ) ) ;
#30175 = FACE_OUTER_BOUND ( 'NONE', #33600, .T. ) ;
#30176 = CARTESIAN_POINT ( 'NONE',  ( 0.000000000000000000, 0.000000000000000000, -99.99999999999998579 ) ) ;
#30177 = LINE ( 'NONE', #40279, #31658 ) ;
#30178 = CARTESIAN_POINT ( 'NONE',  ( 10.81189881249999729, 0.000000000000000000, -104.8437500020483810 ) ) ;
#30179 = CARTESIAN_POINT ( 'NONE',  ( -10.00000000000000000, -5.773502691896251982, -80.62499999999998579 ) ) ;
#30180 = CARTESIAN_POINT ( 'NONE',  ( 10.81189881249999907, 6.242252689847868297, -7.406250002048365033 ) ) ;
#30181 = CARTESIAN_POINT ( 'NONE',  ( 4.999999999999992006, -8.660254037844389075, -88.12500000409677625 ) ) ;
#30182 = CARTESIAN_POINT ( 'NONE',  ( -10.00000000000000000, -5.773502691896252870, -169.1249999999999716 ) ) ;
#30183 = CC_DESIGN_PERSON_AND_ORGANIZATION_ASSIGNMENT ( #12913, #32386, ( #22864 ) ) ;
#30184 = CARTESIAN_POINT ( 'NONE',  ( -5.405949406250003975, -9.363379034771801557, -102.5312500020483952 ) ) ;
#30185 = CARTESIAN_POINT ( 'NONE',  ( 5.405949406249992428, -9.363379034771808662, -81.28125000204839523 ) ) ;
#30186 = ORIENTED_EDGE ( 'NONE', *, *, #42537, .F. ) ;
#30187 = CARTESIAN_POINT ( 'NONE',  ( -9.999999999999998224, 1.224646799147353059E-15, -76.62500000409677625 ) ) ;
#30188 = DIRECTION ( 'NONE',  ( -0.000000000000000000, -0.000000000000000000, -1.000000000000000000 ) ) ;
#30189 = CARTESIAN_POINT ( 'NONE',  ( -10.81189881249999729, 1.324075727343319199E-15, -30.59375000204836326 ) ) ;
#30190 = ORIENTED_EDGE ( 'NONE', *, *, #34899, .F. ) ;
#30191 = CARTESIAN_POINT ( 'NONE',  ( 7.070501591499377789E-16, 11.54700538379251284, -9.124999999999978684 ) ) ;
#30192 = CARTESIAN_POINT ( 'NONE',  ( -2.293366432827344421E-15, -12.48450537969573659, -30.40625000204835615 ) ) ;
#30193 = CARTESIAN_POINT ( 'NONE',  ( -2.121150477449813534E-15, -11.54700538379251284, -147.8750000000000000 ) ) ;
#30194 = CARTESIAN_POINT ( 'NONE',  ( -4.999999999999996447, 8.660254037844387298, -139.5000000000000000 ) ) ;
#30195 = CARTESIAN_POINT ( 'NONE',  ( 10.00000000000000000, 5.773502691896255534, -14.25000000409676382 ) ) ;
#30196 =( BOUNDED_CURVE ( )  B_SPLINE_CURVE ( 2, ( #24916, #38271, #35686, #11933, #28995, #5478, #1821 ),
 .UNSPECIFIED., .F., .F. ) 
 B_SPLINE_CURVE_WITH_KNOTS ( ( 3, 2, 2, 3 ),
 ( 0.3208955223880597396, 0.3221393034825871804, 0.3233830845771145657, 0.3246268656716419510 ),
 .UNSPECIFIED. ) 
 CURVE ( )  GEOMETRIC_REPRESENTATION_ITEM ( )  RATIONAL_B_SPLINE_CURVE ( ( 0.9999999999999940048, 0.8660254037844447028, 1.000000000000000000, 0.8660254037844387076, 1.000000000000000000, 0.8660254037844207220, 1.000000000000017986 ) ) 
 REPRESENTATION_ITEM ( '' )  );
#30197 = ADVANCED_FACE ( 'NONE', ( #6782 ), #30099, .T. ) ;
#30198 = CARTESIAN_POINT ( 'NONE',  ( -10.00000000000000000, -5.773502691896251982, -190.1250000000000284 ) ) ;
#30199 = CARTESIAN_POINT ( 'NONE',  ( 9.999999999999479527, 5.773502691896553074, -123.3749999999999858 ) ) ;
#30201 = EDGE_LOOP ( 'NONE', ( #21265, #14396, #33007, #16351 ) ) ;
#30200 = CARTESIAN_POINT ( 'NONE',  ( 7.644554776091147741E-16, 12.48450537969573659, -118.1562500020483952 ) ) ;
#30202 = VECTOR ( 'NONE', #21384, 1000.000000000000114 ) ;
#30203 = ORIENTED_EDGE ( 'NONE', *, *, #25160, .F. ) ;
#30204 = ORIENTED_EDGE ( 'NONE', *, *, #36000, .T. ) ;
#30205 = CARTESIAN_POINT ( 'NONE',  ( 5.405949406249999534, 9.363379034771803333, -43.28125000204838102 ) ) ;
#30206 = PERSON_AND_ORGANIZATION_ROLE ( 'creator' ) ;
#30207 = CARTESIAN_POINT ( 'NONE',  ( 10.81189881249999551, -6.242252689847874514, -98.96875000204838102 ) ) ;
#30208 = CARTESIAN_POINT ( 'NONE',  ( 10.81189881249999551, -6.242252689847874514, -120.1562500020483952 ) ) ;
#30209 = ORIENTED_EDGE ( 'NONE', *, *, #31375, .F. ) ;
#30210 = ADVANCED_FACE ( 'NONE', ( #13656 ), #19299, .T. ) ;
#30211 = CARTESIAN_POINT ( 'NONE',  ( -9.999999999999998224, 1.224646799147353059E-15, -118.2500000000000000 ) ) ;
#30212 = CARTESIAN_POINT ( 'NONE',  ( -5.405949406249996869, 9.363379034771805109, -198.8437500020484094 ) ) ;
#30213 = CARTESIAN_POINT ( 'NONE',  ( 5.405949406249999534, 9.363379034771803333, -169.2812500020484094 ) ) ;
#30214 = CARTESIAN_POINT ( 'NONE',  ( -4.999999999999996447, 8.660254037844387298, -13.87500000409674961 ) ) ;
#30215 = CARTESIAN_POINT ( 'NONE',  ( -5.405949406249996869, 9.363379034771805109, -134.3437500020484094 ) ) ;
#30216 = CARTESIAN_POINT ( 'NONE',  ( 10.81189881249999551, -6.242252689847874514, -97.46875000204838102 ) ) ;
#30217 = CARTESIAN_POINT ( 'NONE',  ( 9.999999999999998224, 0.000000000000000000, -113.3750000040967763 ) ) ;
#30218 = CARTESIAN_POINT ( 'NONE',  ( -5.405949406249996869, 9.363379034771805109, -98.53125000204839523 ) ) ;
#30219 = CARTESIAN_POINT ( 'NONE',  ( 4.999999999999992006, -8.660254037844389075, -188.6250000040967905 ) ) ;
#30220 = CARTESIAN_POINT ( 'NONE',  ( -2.293366432827344421E-15, -12.48450537969573659, -117.2187500020483668 ) ) ;
#30221 = CARTESIAN_POINT ( 'NONE',  ( -10.81189881249999729, -6.242252689847864744, -176.1562500020484094 ) ) ;
#30222 = CARTESIAN_POINT ( 'NONE',  ( 10.00000000000076916, -5.773502691895816774, -107.1249999999999574 ) ) ;
#30223 = CARTESIAN_POINT ( 'NONE',  ( 10.81189881249999551, -6.242252689847874514, -178.6562500020484094 ) ) ;
#30224 = CARTESIAN_POINT ( 'NONE',  ( 10.81189881249999729, 0.000000000000000000, -193.5312500020484094 ) ) ;
#30225 = CARTESIAN_POINT ( 'NONE',  ( 10.81189881249999729, 0.000000000000000000, -59.84375000204835970 ) ) ;
#30226 = CARTESIAN_POINT ( 'NONE',  ( -5.405949406249996869, 9.363379034771805109, -44.34375000204837391 ) ) ;
#30227 = CARTESIAN_POINT ( 'NONE',  ( -5.000000000000003553, -8.660254037844383745, -175.3750000040967905 ) ) ;
#30228 = CARTESIAN_POINT ( 'NONE',  ( 10.81189881249999907, 6.242252689847868297, -16.40625000204838102 ) ) ;
#30229 = CARTESIAN_POINT ( 'NONE',  ( 7.644554776091147741E-16, 12.48450537969573659, -21.96875000204837391 ) ) ;
#30230 = CYLINDRICAL_SURFACE ( 'NONE', #26117, 9.999999999999998224 ) ;
#30231 = CARTESIAN_POINT ( 'NONE',  ( -5.405949406250003975, -9.363379034771801557, -126.3437500020483952 ) ) ;
#30232 = CARTESIAN_POINT ( 'NONE',  ( 7.070501591499377789E-16, 11.54700538379251284, -108.1249999999999716 ) ) ;
#30233 = CARTESIAN_POINT ( 'NONE',  ( -10.81189881249999729, 6.242252689847871849, -24.90625000204838102 ) ) ;
#30234 = AXIS2_PLACEMENT_3D ( 'NONE', #10600, #7383, #20530 ) ;
#30235 = CARTESIAN_POINT ( 'NONE',  ( 9.999999999999998224, 0.000000000000000000, -164.0000000000000000 ) ) ;
#30236 = CARTESIAN_POINT ( 'NONE',  ( 9.999999999999998224, 0.000000000000000000, -55.99999999999996447 ) ) ;
#30237 = CARTESIAN_POINT ( 'NONE',  ( 5.405949406249999534, 9.363379034771803333, -124.2812500020483952 ) ) ;
#30238 = CARTESIAN_POINT ( 'NONE',  ( 10.81189881249999551, -6.242252689847874514, -109.6562500020483810 ) ) ;
#30239 = ORIENTED_EDGE ( 'NONE', *, *, #24757, .F. ) ;
#30240 = DIRECTION ( 'NONE',  ( 1.000000000000000000, 0.000000000000000000, 0.000000000000000000 ) ) ;
#30241 = CARTESIAN_POINT ( 'NONE',  ( 10.00000000000000000, 5.773502691896255534, -107.2500000040967763 ) ) ;
#30242 = CARTESIAN_POINT ( 'NONE',  ( -5.000000000000003553, -8.660254037844383745, -107.4999999999999858 ) ) ;
#30243 = CARTESIAN_POINT ( 'NONE',  ( 10.81189881249999907, 6.242252689847868297, -59.71875000204838102 ) ) ;
#30244 = VERTEX_POINT ( 'NONE', #35729 ) ;
#30245 = CARTESIAN_POINT ( 'NONE',  ( 10.00000000000000000, 5.773502691896255534, -36.37499999999996447 ) ) ;
#30246 = EDGE_CURVE ( 'NONE', #7470, #6263, #2920, .T. ) ;
#30247 = CARTESIAN_POINT ( 'NONE',  ( -10.81189881249999729, -6.242252689847864744, -39.65625000204835970 ) ) ;
#30248 = CARTESIAN_POINT ( 'NONE',  ( 9.999999999999998224, 0.000000000000000000, -132.8750000040967905 ) ) ;
#30249 = CARTESIAN_POINT ( 'NONE',  ( -2.121150477449813534E-15, -11.54700538379251284, -38.75000000409676204 ) ) ;
#30250 = LINE ( 'NONE', #1907, #28680 ) ;
#30251 = CARTESIAN_POINT ( 'NONE',  ( 7.644554776091147741E-16, 12.48450537969573659, -139.1562500020483810 ) ) ;
#30252 = CARTESIAN_POINT ( 'NONE',  ( -10.00000000000012434, 5.773502691896184480, -162.2500000040967905 ) ) ;
#30253 = ORIENTED_EDGE ( 'NONE', *, *, #13888, .F. ) ;
#30254 = ORIENTED_EDGE ( 'NONE', *, *, #2100, .F. ) ;
#30255 = VECTOR ( 'NONE', #7127, 1000.000000000000000 ) ;
#30256 = CARTESIAN_POINT ( 'NONE',  ( 9.999999999999227285, 5.773502691896701400, -108.3749999999999289 ) ) ;
#30257 = DIRECTION ( 'NONE',  ( 1.000000000000000000, 0.000000000000000000, 0.000000000000000000 ) ) ;
#30258 = CARTESIAN_POINT ( 'NONE',  ( 10.81189881249999551, -6.242252689847874514, -167.9687500020483810 ) ) ;
#30259 = CARTESIAN_POINT ( 'NONE',  ( -10.81189881249999907, -6.242252689847864744, -198.6562500020484094 ) ) ;
#30260 = CARTESIAN_POINT ( 'NONE',  ( 10.81189881249999907, 6.242252689847868297, -16.21875000204836326 ) ) ;
#30261 = CARTESIAN_POINT ( 'NONE',  ( -9.999999999999998224, 1.224646799147353059E-15, -170.7500000000000000 ) ) ;
#30262 = CARTESIAN_POINT ( 'NONE',  ( 5.405949406249999534, 9.363379034771803333, -157.0937500020483810 ) ) ;
#30263 = CARTESIAN_POINT ( 'NONE',  ( -10.81189881249999729, 1.324075727343319199E-15, -138.5937500020483810 ) ) ;
#30264 = CARTESIAN_POINT ( 'NONE',  ( 5.000000000000000000, 8.660254037844385522, -67.74999999999997158 ) ) ;
#30265 = CARTESIAN_POINT ( 'NONE',  ( 10.81189881249999729, 0.000000000000000000, -119.8437500020483810 ) ) ;
#30266 = CARTESIAN_POINT ( 'NONE',  ( 9.999999999999996447, -5.773502691896262640, -194.5000000040968189 ) ) ;
#30267 = CARTESIAN_POINT ( 'NONE',  ( 7.644554776091147741E-16, 12.48450537969573659, -122.6562500020483952 ) ) ;
#30268 = CARTESIAN_POINT ( 'NONE',  ( 7.644554776091147741E-16, 12.48450537969573659, -8.468750002048357928 ) ) ;
#30269 = CARTESIAN_POINT ( 'NONE',  ( 10.81189881249999729, 0.000000000000000000, -136.3437500020484094 ) ) ;
#30270 = DIRECTION ( 'NONE',  ( -0.000000000000000000, -0.000000000000000000, 1.000000000000000000 ) ) ;
#30271 = VECTOR ( 'NONE', #18628, 1000.000000000000000 ) ;
#30272 = CARTESIAN_POINT ( 'NONE',  ( -10.00000000000051337, 5.773502691895962435, -124.7500000040967620 ) ) ;
#30273 = CARTESIAN_POINT ( 'NONE',  ( 7.070501591499377789E-16, 11.54700538379251284, -151.6250000000000000 ) ) ;
#30274 = CARTESIAN_POINT ( 'NONE',  ( 10.00000000000000000, 5.773502691896255534, -22.87499999999997868 ) ) ;
#30275 = CARTESIAN_POINT ( 'NONE',  ( -2.293366432827344421E-15, -12.48450537969573659, -82.71875000204838102 ) ) ;
#30276 = CARTESIAN_POINT ( 'NONE',  ( 10.81189881249999729, 0.000000000000000000, -64.34375000204836681 ) ) ;
#30277 = CARTESIAN_POINT ( 'NONE',  ( 9.999999999999998224, 0.000000000000000000, -116.3750000040967905 ) ) ;
#30278 = CARTESIAN_POINT ( 'NONE',  ( -10.81189881249999729, 6.242252689847871849, -42.90625000204838102 ) ) ;
#30279 = CARTESIAN_POINT ( 'NONE',  ( 10.81189881249999551, -6.242252689847874514, -44.96875000204835970 ) ) ;
#30280 = CARTESIAN_POINT ( 'NONE',  ( 9.999999999999998224, 0.000000000000000000, -141.5000000000000000 ) ) ;
#30281 = CARTESIAN_POINT ( 'NONE',  ( 5.405949406249992428, -9.363379034771808662, -157.5937500020483810 ) ) ;
#30282 = CARTESIAN_POINT ( 'NONE',  ( -5.000000000000003553, -8.660254037844383745, -131.5000000000000000 ) ) ;
#30283 = CARTESIAN_POINT ( 'NONE',  ( 5.405949406249992428, -9.363379034771808662, -138.2812500020483810 ) ) ;
#30284 = DIRECTION ( 'NONE',  ( 1.000000000000000000, 0.000000000000000000, -0.000000000000000000 ) ) ;
#30285 = CARTESIAN_POINT ( 'NONE',  ( 5.000000000000000000, 8.660254037844385522, -84.24999999999997158 ) ) ;
#30286 = CARTESIAN_POINT ( 'NONE',  ( -10.81189881249999729, 1.324075727343319199E-15, -18.78125000204835970 ) ) ;
#30287 = ORIENTED_EDGE ( 'NONE', *, *, #2632, .T. ) ;
#30288 = CARTESIAN_POINT ( 'NONE',  ( -2.293366432827344421E-15, -12.48450537969573659, -108.4062500020483810 ) ) ;
#30289 = CARTESIAN_POINT ( 'NONE',  ( -4.999999999999996447, 8.660254037844387298, -133.8750000040967905 ) ) ;
#30290 = CARTESIAN_POINT ( 'NONE',  ( -9.999999999999998224, 1.224646799147353059E-15, -142.2500000000000000 ) ) ;
#30291 = ADVANCED_FACE ( 'NONE', ( #956 ), #24266, .F. ) ;
#30292 = CARTESIAN_POINT ( 'NONE',  ( 7.070501591499377789E-16, 11.54700538379251284, -45.50000000409676915 ) ) ;
#30293 = FACE_OUTER_BOUND ( 'NONE', #33527, .T. ) ;
#30294 = CARTESIAN_POINT ( 'NONE',  ( -10.81189881249999907, -6.242252689847864744, -50.15625000204837391 ) ) ;
#30295 = CARTESIAN_POINT ( 'NONE',  ( -5.000000000000003553, -8.660254037844383745, -191.5000000000000000 ) ) ;
#30296 = CARTESIAN_POINT ( 'NONE',  ( -10.81189881249999907, -6.242252689847864744, -156.6562500020483810 ) ) ;
#30297 = VECTOR ( 'NONE', #8532, 1000.000000000000000 ) ;
#30298 = CARTESIAN_POINT ( 'NONE',  ( 5.405949406249999534, 9.363379034771803333, -133.0937500020483810 ) ) ;
#30299 = CARTESIAN_POINT ( 'NONE',  ( -9.999999999999479527, -5.773502691896549521, -115.5000000040967763 ) ) ;
#30300 = ORIENTED_EDGE ( 'NONE', *, *, #6863, .F. ) ;
#30301 = DIRECTION ( 'NONE',  ( -0.000000000000000000, -0.000000000000000000, 1.000000000000000000 ) ) ;
#30302 = EDGE_CURVE ( 'NONE', #23494, #21425, #21357, .T. ) ;
#30303 = AXIS2_PLACEMENT_3D ( 'NONE', #37587, #7595, #27452 ) ;
#30305 = ORIENTED_EDGE ( 'NONE', *, *, #15852, .T. ) ;
#30304 = CARTESIAN_POINT ( 'NONE',  ( 10.81189881249999551, -6.242252689847874514, -64.65625000204839523 ) ) ;
#30306 = APPLICATION_PROTOCOL_DEFINITION ( 'international standard', 'config_control_design', 1994, #17898 ) ;
#30308 = ORIENTED_EDGE ( 'NONE', *, *, #15854, .F. ) ;
#30307 = CARTESIAN_POINT ( 'NONE',  ( -2.293366432827344421E-15, -12.48450537969573659, -111.2187500020483668 ) ) ;
#30309 =( BOUNDED_CURVE ( )  B_SPLINE_CURVE ( 2, ( #35348, #42216, #41793, #12644, #25836, #5776, #3171 ),
 .UNSPECIFIED., .F., .F. ) 
 B_SPLINE_CURVE_WITH_KNOTS ( ( 3, 2, 2, 3 ),
 ( 0.4365671641791046276, 0.4378109452736320129, 0.4390547263681593981, 0.4402985074626867279 ),
 .UNSPECIFIED. ) 
 CURVE ( )  GEOMETRIC_REPRESENTATION_ITEM ( )  RATIONAL_B_SPLINE_CURVE ( ( 0.9999999999999820144, 0.8660254037844566932, 1.000000000000000000, 0.8660254037844387076, 1.000000000000000000, 0.8660254037844207220, 1.000000000000017986 ) ) 
 REPRESENTATION_ITEM ( '' )  );
#30310 = CARTESIAN_POINT ( 'NONE',  ( 7.644554776091147741E-16, 12.48450537969573659, -21.96875000204837036 ) ) ;
#30311 = CARTESIAN_POINT ( 'NONE',  ( -5.405949406249996869, 9.363379034771805109, -191.3437500020484094 ) ) ;
#30312 = CARTESIAN_POINT ( 'NONE',  ( 5.405949406249992428, -9.363379034771808662, -46.59375000204838102 ) ) ;
#30313 = CARTESIAN_POINT ( 'NONE',  ( -0.02412132759690014186, -10.44061561015125505, -5.090678961559005602E-15 ) ) ;
#30314 = CARTESIAN_POINT ( 'NONE',  ( 7.070501591499376803E-16, 11.54700538379251284, -152.0000000040967905 ) ) ;
#30315 = CARTESIAN_POINT ( 'NONE',  ( 10.81189881249999729, 6.242252689847867408, -181.2187500020484094 ) ) ;
#30316 = CARTESIAN_POINT ( 'NONE',  ( -10.81189881249999907, -6.242252689847864744, -159.4687500020484094 ) ) ;
#30317 = CARTESIAN_POINT ( 'NONE',  ( -10.81189881249999729, 6.242252689847871849, -144.7187500020483810 ) ) ;
#30318 = CARTESIAN_POINT ( 'NONE',  ( 5.405949406249992428, -9.363379034771808662, -159.0937500020484094 ) ) ;
#30319 = DIRECTION ( 'NONE',  ( 1.000000000000000000, 0.000000000000000000, 0.000000000000000000 ) ) ;
#30320 =( BOUNDED_CURVE ( )  B_SPLINE_CURVE ( 2, ( #27125, #18847, #32027, #13929, #40267, #10704, #23900 ),
 .UNSPECIFIED., .F., .F. ) 
 B_SPLINE_CURVE_WITH_KNOTS ( ( 3, 2, 2, 3 ),
 ( 0.2761194029850747578, 0.2773631840796020875, 0.2786069651741294728, 0.2798507462686568026 ),
 .UNSPECIFIED. ) 
 CURVE ( )  GEOMETRIC_REPRESENTATION_ITEM ( )  RATIONAL_B_SPLINE_CURVE ( ( 0.9999999999999880096, 0.8660254037844506980, 1.000000000000000000, 0.8660254037844387076, 1.000000000000000000, 0.8660254037844267172, 1.000000000000011990 ) ) 
 REPRESENTATION_ITEM ( '' )  );
#30321 = CARTESIAN_POINT ( 'NONE',  ( -4.999999999999996447, 8.660254037844387298, -102.3750000040967905 ) ) ;
#30322 = CARTESIAN_POINT ( 'NONE',  ( 5.000000000000000000, 8.660254037844385522, -183.2500000000000000 ) ) ;
#30323 = VECTOR ( 'NONE', #16242, 1000.000000000000000 ) ;
#30324 = CARTESIAN_POINT ( 'NONE',  ( -5.405949406249996869, 9.363379034771805109, -89.34375000204838102 ) ) ;
#30325 = EDGE_CURVE ( 'NONE', #18400, #33859, #20745, .T. ) ;
#30326 = CARTESIAN_POINT ( 'NONE',  ( -5.000000000000003553, -8.660254037844383745, -101.5000000000000000 ) ) ;
#30327 = CARTESIAN_POINT ( 'NONE',  ( -10.81189881249999729, 1.324075727343319199E-15, -66.78125000204838102 ) ) ;
#30328 = CARTESIAN_POINT ( 'NONE',  ( -4.999999999999996447, 8.660254037844387298, -168.3750000040967905 ) ) ;
#30329 = CARTESIAN_POINT ( 'NONE',  ( 5.405949406249992428, -9.363379034771808662, -184.5937500020483810 ) ) ;
#30330 = CARTESIAN_POINT ( 'NONE',  ( 5.405949406249992428, -9.363379034771808662, -121.7812500020483952 ) ) ;
#30331 = CARTESIAN_POINT ( 'NONE',  ( 5.405949406249992428, -9.363379034771808662, -165.2812500020484094 ) ) ;
#30332 = CARTESIAN_POINT ( 'NONE',  ( 10.81189881249999551, -6.242252689847874514, -52.65625000204837391 ) ) ;
#30333 = CARTESIAN_POINT ( 'NONE',  ( -4.999999999999996447, 8.660254037844387298, -136.8750000040967905 ) ) ;
#30334 = CARTESIAN_POINT ( 'NONE',  ( 5.000000000000000000, 8.660254037844385522, -109.7499999999999858 ) ) ;
#30335 = EDGE_CURVE ( 'NONE', #317, #2293, #5617, .T. ) ;
#30336 = ORIENTED_EDGE ( 'NONE', *, *, #29272, .T. ) ;
#30337 = CARTESIAN_POINT ( 'NONE',  ( 5.405949406249992428, -9.363379034771808662, -132.2812500020483810 ) ) ;
#30338 = CARTESIAN_POINT ( 'NONE',  ( -10.81189881249999907, -6.242252689847864744, -147.6562500020483810 ) ) ;
#30339 = CARTESIAN_POINT ( 'NONE',  ( -5.405949406250003975, -9.363379034771801557, -189.5312500020484094 ) ) ;
#30340 = CARTESIAN_POINT ( 'NONE',  ( -5.405949406250003975, -9.363379034771801557, -78.34375000204838102 ) ) ;
#30341 = ORIENTED_EDGE ( 'NONE', *, *, #9425, .T. ) ;
#30342 = CARTESIAN_POINT ( 'NONE',  ( 7.070501591499377789E-16, 11.54700538379251284, -48.12499999999997158 ) ) ;
#30343 = CARTESIAN_POINT ( 'NONE',  ( 5.405949406249999534, 9.363379034771803333, -178.0937500020484094 ) ) ;
#30344 = CARTESIAN_POINT ( 'NONE',  ( 4.999999999999992006, -8.660254037844389075, -62.62500000409676204 ) ) ;
#30345 = CARTESIAN_POINT ( 'NONE',  ( 10.00000000000051159, -5.773502691895965988, -110.1249999999999858 ) ) ;
#30346 = CARTESIAN_POINT ( 'NONE',  ( 9.999999999999998224, 0.000000000000000000, -165.5000000000000000 ) ) ;
#30347 = CARTESIAN_POINT ( 'NONE',  ( 10.81189881249999907, 6.242252689847868297, -79.40625000204839523 ) ) ;
#30348 = CARTESIAN_POINT ( 'NONE',  ( 10.81189881249999729, 6.242252689847867408, -62.90625000204838813 ) ) ;
#30349 = CARTESIAN_POINT ( 'NONE',  ( 9.999999999999998224, 0.000000000000000000, -54.87500000409675494 ) ) ;
#30350 = CARTESIAN_POINT ( 'NONE',  ( -2.293366432827344421E-15, -12.48450537969573659, -13.71875000204836326 ) ) ;
#30351 = CARTESIAN_POINT ( 'NONE',  ( -9.999999999999998224, 1.224646799147353059E-15, -132.1250000040967620 ) ) ;
#30352 = CARTESIAN_POINT ( 'NONE',  ( -10.81189881249999729, 1.324075727343319199E-15, -179.2812500020484094 ) ) ;
#30353 = CARTESIAN_POINT ( 'NONE',  ( 5.405949406249992428, -9.363379034771808662, -4.781250002048375691 ) ) ;
#30354 = CARTESIAN_POINT ( 'NONE',  ( -9.999999999999998224, 1.224646799147353059E-15, -147.1250000040967905 ) ) ;
#30355 = CARTESIAN_POINT ( 'NONE',  ( 9.999999999999998224, 0.000000000000000000, -161.0000000000000000 ) ) ;
#30356 = CARTESIAN_POINT ( 'NONE',  ( 7.070501591499376803E-16, 11.54700538379251284, -177.5000000040967905 ) ) ;
#30357 = CARTESIAN_POINT ( 'NONE',  ( 0.000000000000000000, 0.000000000000000000, -200.0000000000000000 ) ) ;
#30358 = AXIS2_PLACEMENT_3D ( 'NONE', #2491, #18658, #41742 ) ;
#30360 = VERTEX_POINT ( 'NONE', #17326 ) ;
#30359 = CARTESIAN_POINT ( 'NONE',  ( 10.81189881249999907, 6.242252689847868297, -86.90625000204836681 ) ) ;
#30361 = CARTESIAN_POINT ( 'NONE',  ( 9.999999999999227285, 5.773502691896701400, -107.2500000040967620 ) ) ;
#30362 = EDGE_CURVE ( 'NONE', #6831, #22759, #40616, .T. ) ;
#30364 = EDGE_LOOP ( 'NONE', ( #22855, #13336, #19125, #36531 ) ) ;
#30363 = CARTESIAN_POINT ( 'NONE',  ( 10.81189881249999729, 6.242252689847867408, -100.2187500020483810 ) ) ;
#30365 = VERTEX_POINT ( 'NONE', #30529 ) ;
#30366 = CARTESIAN_POINT ( 'NONE',  ( -10.81189881249999907, -6.242252689847864744, -27.46875000204838457 ) ) ;
#30367 = CARTESIAN_POINT ( 'NONE',  ( 7.644554776091147741E-16, 12.48450537969573659, -25.15625000204838457 ) ) ;
#30368 = DATE_AND_TIME ( #4022, #6000 ) ;
#30369 = CARTESIAN_POINT ( 'NONE',  ( -5.405949406250003975, -9.363379034771801557, -67.84375000204836681 ) ) ;
#30370 = CARTESIAN_POINT ( 'NONE',  ( 10.00000000000102318, -5.773502691895667560, -17.50000000409673362 ) ) ;
#30371 = CARTESIAN_POINT ( 'NONE',  ( 10.00000000000000000, 5.773502691896255534, -46.87499999999997158 ) ) ;
#30372 = CARTESIAN_POINT ( 'NONE',  ( -5.405949406249996869, 9.363379034771805109, -182.3437500020483810 ) ) ;
#30373 = CARTESIAN_POINT ( 'NONE',  ( 9.999999999999998224, 0.000000000000000000, -25.99999999999996803 ) ) ;
#30374 = CYLINDRICAL_SURFACE ( 'NONE', #2631, 9.999999999999998224 ) ;
#30375 = CARTESIAN_POINT ( 'NONE',  ( -9.999999999999998224, 1.224646799147353059E-15, -70.62500000409677625 ) ) ;
#30376 = CARTESIAN_POINT ( 'NONE',  ( -5.000000000000003553, -8.660254037844383745, -5.875000004096770034 ) ) ;
#30377 = DIRECTION ( 'NONE',  ( 1.000000000000000000, 0.000000000000000000, 0.000000000000000000 ) ) ;
#30378 = CARTESIAN_POINT ( 'NONE',  ( 10.81189881249999907, 6.242252689847868297, -118.2187500020483810 ) ) ;
#30379 = CARTESIAN_POINT ( 'NONE',  ( -10.00000000000051337, 5.773502691895962435, -109.3749999999999858 ) ) ;
#30380 = CARTESIAN_POINT ( 'NONE',  ( 5.405949406249992428, -9.363379034771808662, -90.28125000204838102 ) ) ;
#30381 = CARTESIAN_POINT ( 'NONE',  ( -2.293366432827344421E-15, -12.48450537969573659, -103.7187500020483668 ) ) ;
#30382 = CARTESIAN_POINT ( 'NONE',  ( -10.81189881249999729, 1.324075727343319199E-15, -66.59375000204836681 ) ) ;
#30383 = CARTESIAN_POINT ( 'NONE',  ( 5.405949406249992428, -9.363379034771808662, -78.28125000204838102 ) ) ;
#30384 = CARTESIAN_POINT ( 'NONE',  ( 4.999999999999992006, -8.660254037844389075, -160.1250000040967905 ) ) ;
#30385 = CARTESIAN_POINT ( 'NONE',  ( -2.293366432827344421E-15, -12.48450537969573659, -154.9062500020483810 ) ) ;
#30386 = CARTESIAN_POINT ( 'NONE',  ( -10.81189881249999729, 6.242252689847871849, -173.4062500020483810 ) ) ;
#30387 = AXIS2_PLACEMENT_3D ( 'NONE', #37945, #15043, #1700 ) ;
#30388 = CYLINDRICAL_SURFACE ( 'NONE', #15085, 9.999999999999998224 ) ;
#30389 = LINE ( 'NONE', #23696, #9576 ) ;
#30390 = CARTESIAN_POINT ( 'NONE',  ( -2.293366432827344421E-15, -12.48450537969573659, -106.7187500020483668 ) ) ;
#30391 = CARTESIAN_POINT ( 'NONE',  ( -10.00000000000025580, 5.773502691896109873, -120.2500000040967905 ) ) ;
#30392 = CARTESIAN_POINT ( 'NONE',  ( 7.070501591499377789E-16, 11.54700538379251284, -76.62499999999997158 ) ) ;
#30393 = CARTESIAN_POINT ( 'NONE',  ( 7.644554776091147741E-16, 12.48450537969573659, -7.156250002048364145 ) ) ;
#30394 = CARTESIAN_POINT ( 'NONE',  ( -10.00000000000000000, -5.773502691896251982, -90.00000000409677625 ) ) ;
#30395 = VECTOR ( 'NONE', #39559, 1000.000000000000114 ) ;
#30396 = FACE_OUTER_BOUND ( 'NONE', #5950, .T. ) ;
#30397 = CARTESIAN_POINT ( 'NONE',  ( -10.81189881249999907, -6.242252689847864744, -101.1562500020483952 ) ) ;
#30398 = CARTESIAN_POINT ( 'NONE',  ( -10.81189881249999729, 6.242252689847871849, -83.40625000204838102 ) ) ;
#30399 = CARTESIAN_POINT ( 'NONE',  ( 4.999999999999992006, -8.660254037844389075, -77.62500000409677625 ) ) ;
#30400 = CARTESIAN_POINT ( 'NONE',  ( -9.999999999999998224, 1.224646799147353059E-15, -20.74999999999996447 ) ) ;
#30401 = CARTESIAN_POINT ( 'NONE',  ( -5.405949406249996869, 9.363379034771805109, -33.84375000204836681 ) ) ;
#30402 = ORIENTED_EDGE ( 'NONE', *, *, #8296, .F. ) ;
#30403 = CARTESIAN_POINT ( 'NONE',  ( -9.999999999999998224, 5.773502691896259087, -7.374999999999970690 ) ) ;
#30404 = CARTESIAN_POINT ( 'NONE',  ( -5.405949406250003975, -9.363379034771801557, -30.53125000204837036 ) ) ;
#30405 = CARTESIAN_POINT ( 'NONE',  ( 9.999999999999996447, -5.773502691896262640, -143.1250000000000000 ) ) ;
#30406 = DIRECTION ( 'NONE',  ( 1.000000000000000000, 0.000000000000000000, 0.000000000000000000 ) ) ;
#30407 =( BOUNDED_CURVE ( )  B_SPLINE_CURVE ( 2, ( #13928, #27337, #10703, #37045, #10919, #17387, #24113 ),
 .UNSPECIFIED., .F., .F. ) 
 B_SPLINE_CURVE_WITH_KNOTS ( ( 3, 2, 2, 3 ),
 ( 0.2611940298507463565, 0.2624378109452737418, 0.2636815920398011270, 0.2649253731343284568 ),
 .UNSPECIFIED. ) 
 CURVE ( )  GEOMETRIC_REPRESENTATION_ITEM ( )  RATIONAL_B_SPLINE_CURVE ( ( 0.9999999999999880096, 0.8660254037844506980, 1.000000000000000000, 0.8660254037844387076, 1.000000000000000000, 0.8660254037844267172, 1.000000000000011990 ) ) 
 REPRESENTATION_ITEM ( '' )  );
#30408 = CARTESIAN_POINT ( 'NONE',  ( 9.999999999999996447, -5.773502691896262640, -2.500000004096753159 ) ) ;
#30409 = CARTESIAN_POINT ( 'NONE',  ( 10.81189881249999551, -6.242252689847874514, -135.1562500020484094 ) ) ;
#30410 = CARTESIAN_POINT ( 'NONE',  ( -10.00000000000000000, -5.773502691896251982, -188.6250000000000284 ) ) ;
#30411 = FACE_OUTER_BOUND ( 'NONE', #5738, .T. ) ;
#30413 = ORIENTED_EDGE ( 'NONE', *, *, #31759, .T. ) ;
#30412 = CARTESIAN_POINT ( 'NONE',  ( -5.405949406249996869, 9.363379034771805109, -107.5312500020483810 ) ) ;
#30414 = CARTESIAN_POINT ( 'NONE',  ( -9.999999999999998224, 1.224646799147353059E-15, -36.12500000409676915 ) ) ;
#30415 = ADVANCED_FACE ( 'NONE', ( #12344 ), #38476, .T. ) ;
#30416 = VERTEX_POINT ( 'NONE', #41913 ) ;
#30417 = EDGE_CURVE ( 'NONE', #19501, #36017, #18840, .T. ) ;
#30418 = ORIENTED_EDGE ( 'NONE', *, *, #2764, .T. ) ;
#30419 = VECTOR ( 'NONE', #477, 1000.000000000000000 ) ;
#30420 = CARTESIAN_POINT ( 'NONE',  ( -2.293366432827344421E-15, -12.48450537969573659, -45.40625000204837391 ) ) ;
#30421 = COORDINATED_UNIVERSAL_TIME_OFFSET ( 6, 0, .AHEAD. ) ;
#30422 = CARTESIAN_POINT ( 'NONE',  ( -5.405949406250003975, -9.363379034771801557, -94.84375000204838102 ) ) ;
#30423 = CARTESIAN_POINT ( 'NONE',  ( 10.81189881249999729, 6.242252689847867408, -125.9062500020483810 ) ) ;
#30424 = ORIENTED_EDGE ( 'NONE', *, *, #3091, .T. ) ;
#30425 = CARTESIAN_POINT ( 'NONE',  ( 9.999999999999994671, -5.773502691896262640, -132.6250000000000000 ) ) ;
#30426 = CARTESIAN_POINT ( 'NONE',  ( 7.644554776091147741E-16, 12.48450537969573659, -195.9687500020484094 ) ) ;
#30427 = CARTESIAN_POINT ( 'NONE',  ( -10.81189881249999729, 6.242252689847871849, -170.4062500020484094 ) ) ;
#30428 = CYLINDRICAL_SURFACE ( 'NONE', #35711, 9.999999999999998224 ) ;
#30429 = EDGE_CURVE ( 'NONE', #37069, #12598, #28570, .T. ) ;
#30430 = CARTESIAN_POINT ( 'NONE',  ( 5.405949406249999534, 9.363379034771803333, -124.0937500020483952 ) ) ;
#30431 = CARTESIAN_POINT ( 'NONE',  ( -5.405949406250003975, -9.363379034771801557, -96.34375000204838102 ) ) ;
#30432 = DIRECTION ( 'NONE',  ( -0.000000000000000000, -0.000000000000000000, 1.000000000000000000 ) ) ;
#30433 = CARTESIAN_POINT ( 'NONE',  ( -2.293366432827344421E-15, -12.48450537969573659, -100.9062500020483952 ) ) ;
#30434 = CARTESIAN_POINT ( 'NONE',  ( -10.00000000000000000, -5.773502691896251982, -187.5000000040967905 ) ) ;
#30435 = CARTESIAN_POINT ( 'NONE',  ( -2.293366432827344421E-15, -12.48450537969573659, -103.7187500020483668 ) ) ;
#30436 = CARTESIAN_POINT ( 'NONE',  ( 10.81189881249999729, 6.242252689847867408, -176.9062500020484094 ) ) ;
#30437 = DIRECTION ( 'NONE',  ( 0.000000000000000000, -1.000000000000000000, 0.000000000000000000 ) ) ;
#30438 = CARTESIAN_POINT ( 'NONE',  ( -10.81189881249999907, -6.242252689847864744, -192.6562500020484094 ) ) ;
#30439 = CARTESIAN_POINT ( 'NONE',  ( 10.81189881249999729, 0.000000000000000000, -50.84375000204835260 ) ) ;
#30440 = CARTESIAN_POINT ( 'NONE',  ( 10.81189881249999551, -6.242252689847874514, -43.46875000204836681 ) ) ;
#30441 = CARTESIAN_POINT ( 'NONE',  ( 9.999999999999996447, -5.773502691896262640, -170.5000000040967905 ) ) ;
#30442 = CARTESIAN_POINT ( 'NONE',  ( 5.405949406249999534, 9.363379034771803333, -7.281250002048378356 ) ) ;
#30443 = CARTESIAN_POINT ( 'NONE',  ( 10.81189881249999907, 6.242252689847868297, -25.21875000204837747 ) ) ;
#30444 = DIRECTION ( 'NONE',  ( -0.000000000000000000, -1.000000000000000000, -0.000000000000000000 ) ) ;
#30445 = CARTESIAN_POINT ( 'NONE',  ( 5.405949406249992428, -9.363379034771808662, -129.0937500020483810 ) ) ;
#30446 = CARTESIAN_POINT ( 'NONE',  ( -2.121150477449813534E-15, -11.54700538379251284, -102.8749999999999858 ) ) ;
#30447 = CARTESIAN_POINT ( 'NONE',  ( 10.81189881249999907, 6.242252689847868297, -28.40625000204838457 ) ) ;
#30448 = EDGE_CURVE ( 'NONE', #4764, #25488, #2597, .T. ) ;
#30449 = LINE ( 'NONE', #20495, #42393 ) ;
#30450 = CARTESIAN_POINT ( 'NONE',  ( 9.999999999999996447, -5.773502691896262640, -56.12499999999997868 ) ) ;
#30451 = CARTESIAN_POINT ( 'NONE',  ( 5.405949406249992428, -9.363379034771808662, -124.7812500020483952 ) ) ;
#30452 = CARTESIAN_POINT ( 'NONE',  ( 7.644554776091147741E-16, 12.48450537969573659, -106.1562500020483810 ) ) ;
#30453 = VERTEX_POINT ( 'NONE', #2027 ) ;
#30454 = AXIS2_PLACEMENT_3D ( 'NONE', #15330, #37795, #38012 ) ;
#30455 =( BOUNDED_CURVE ( )  B_SPLINE_CURVE ( 2, ( #19570, #26696, #176, #36615, #13081, #805, #16745 ),
 .UNSPECIFIED., .F., .F. ) 
 B_SPLINE_CURVE_WITH_KNOTS ( ( 3, 2, 2, 3 ),
 ( 0.5000000000000001110, 0.5012437810945274963, 0.5024875621890548816, 0.5037313432835821558 ),
 .UNSPECIFIED. ) 
 CURVE ( )  GEOMETRIC_REPRESENTATION_ITEM ( )  RATIONAL_B_SPLINE_CURVE ( ( 0.9999999999999880096, 0.8660254037844506980, 1.000000000000000000, 0.8660254037844387076, 1.000000000000000000, 0.8660254037844267172, 1.000000000000011990 ) ) 
 REPRESENTATION_ITEM ( '' )  );
#30456 = CARTESIAN_POINT ( 'NONE',  ( -5.000000000000003553, -8.660254037844383745, -6.999999999999978684 ) ) ;
#30457 = CARTESIAN_POINT ( 'NONE',  ( 10.00000000000000000, 5.773502691896255534, -98.25000000409677625 ) ) ;
#30458 = DIRECTION ( 'NONE',  ( -0.000000000000000000, -0.000000000000000000, 1.000000000000000000 ) ) ;
#30459 = CARTESIAN_POINT ( 'NONE',  ( -10.81189881249999729, 6.242252689847871849, -57.71875000204837391 ) ) ;
#30460 = ORIENTED_EDGE ( 'NONE', *, *, #30112, .F. ) ;
#30461 = CARTESIAN_POINT ( 'NONE',  ( -5.000000000000003553, -8.660254037844383745, -30.99999999999997158 ) ) ;
#30462 = LOCAL_TIME ( 11, 57, 6.000000000000000000, #20039 ) ;
#30463 = CARTESIAN_POINT ( 'NONE',  ( 5.405949406249999534, 9.363379034771803333, -35.78125000204837391 ) ) ;
#30464 = CARTESIAN_POINT ( 'NONE',  ( -5.000000000000003553, -8.660254037844383745, -90.99999999999998579 ) ) ;
#30465 = CARTESIAN_POINT ( 'NONE',  ( -2.121150477449813534E-15, -11.54700538379251284, -26.75000000409677270 ) ) ;
#30466 = DIRECTION ( 'NONE',  ( -0.000000000000000000, -0.000000000000000000, 1.000000000000000000 ) ) ;
#30467 = AXIS2_PLACEMENT_3D ( 'NONE', #12706, #3026, #19831 ) ;
#30468 = CARTESIAN_POINT ( 'NONE',  ( -10.81189881249999907, -6.242252689847864744, -138.6562500020484094 ) ) ;
#30469 = CARTESIAN_POINT ( 'NONE',  ( -2.121150477449813534E-15, -11.54700538379251284, -119.7500000040967905 ) ) ;
#30470 = VERTEX_POINT ( 'NONE', #9127 ) ;
#30471 = EDGE_CURVE ( 'NONE', #31040, #9902, #9997, .T. ) ;
#30472 = ADVANCED_FACE ( 'NONE', ( #35257 ), #25331, .T. ) ;
#30473 = ORIENTED_EDGE ( 'NONE', *, *, #28025, .T. ) ;
#30474 = CARTESIAN_POINT ( 'NONE',  ( 4.999999999999992006, -8.660254037844389075, -106.1250000040967763 ) ) ;
#30475 = DIRECTION ( 'NONE',  ( 1.000000000000000000, 0.000000000000000000, 0.000000000000000000 ) ) ;
#30476 = CARTESIAN_POINT ( 'NONE',  ( 5.405949406249999534, 9.363379034771803333, -164.5937500020484094 ) ) ;
#30477 = DIRECTION ( 'NONE',  ( -1.000000000000000000, 0.000000000000000000, 0.000000000000000000 ) ) ;
#30478 = CARTESIAN_POINT ( 'NONE',  ( 7.644554776091147741E-16, 12.48450537969573659, -17.46875000204836681 ) ) ;
#30479 = CARTESIAN_POINT ( 'NONE',  ( -2.121150477449813534E-15, -11.54700538379251284, -157.2500000040968189 ) ) ;
#30480 = CARTESIAN_POINT ( 'NONE',  ( -10.81189881249999729, -6.242252689847864744, -144.4687500020484094 ) ) ;
#30481 = CARTESIAN_POINT ( 'NONE',  ( 7.644554776091147741E-16, 12.48450537969573659, -134.4687500020483810 ) ) ;
#30482 = CARTESIAN_POINT ( 'NONE',  ( -10.81189881249999907, -6.242252689847864744, -110.1562500020483952 ) ) ;
#30483 = CARTESIAN_POINT ( 'NONE',  ( 7.644554776091147741E-16, 12.48450537969573659, -116.4687500020483952 ) ) ;
#30484 = CARTESIAN_POINT ( 'NONE',  ( 4.999999999999992006, -8.660254037844389075, -197.6250000040967905 ) ) ;
#30485 = CARTESIAN_POINT ( 'NONE',  ( -10.81189881249999729, 6.242252689847871849, -123.9062500020483952 ) ) ;
#30486 = CARTESIAN_POINT ( 'NONE',  ( -5.405949406250003975, -9.363379034771801557, -13.84375000204834905 ) ) ;
#30488 = EDGE_CURVE ( 'NONE', #8277, #42072, #15787, .T. ) ;
#30487 = CARTESIAN_POINT ( 'NONE',  ( 10.81189881249999729, 0.000000000000000000, -130.3437500020484094 ) ) ;
#30489 = LINE ( 'NONE', #4780, #39176 ) ;
#30490 = CARTESIAN_POINT ( 'NONE',  ( 4.999999999999992006, -8.660254037844389075, -96.74999999999998579 ) ) ;
#30491 = CARTESIAN_POINT ( 'NONE',  ( 7.070501591499377789E-16, 11.54700538379251284, -153.1250000000000000 ) ) ;
#30492 = CARTESIAN_POINT ( 'NONE',  ( 9.999999999999996447, -5.773502691896262640, -24.62499999999998224 ) ) ;
#30493 = AXIS2_PLACEMENT_3D ( 'NONE', #24421, #28287, #24846 ) ;
#30494 = CARTESIAN_POINT ( 'NONE',  ( 10.81189881249999551, -6.242252689847874514, -82.46875000204836681 ) ) ;
#30495 = CARTESIAN_POINT ( 'NONE',  ( 5.405949406249992428, -9.363379034771808662, -63.09375000204836681 ) ) ;
#30496 = CARTESIAN_POINT ( 'NONE',  ( 9.999999999999998224, 1.224646799147353059E-15, -99.99999999999998579 ) ) ;
#30497 = CARTESIAN_POINT ( 'NONE',  ( 10.81189881249999729, 0.000000000000000000, -39.03125000204838102 ) ) ;
#30498 = CARTESIAN_POINT ( 'NONE',  ( 10.81189881249999729, 0.000000000000000000, -46.34375000204838102 ) ) ;
#30499 = CARTESIAN_POINT ( 'NONE',  ( 10.00000000000051159, -5.773502691895965988, -141.6250000000000000 ) ) ;
#30500 = CARTESIAN_POINT ( 'NONE',  ( 10.81189881249999729, 0.000000000000000000, -152.8437500020483810 ) ) ;
#30501 = CARTESIAN_POINT ( 'NONE',  ( -5.000000000000003553, -8.660254037844383745, -128.5000000000000000 ) ) ;
#30502 = CARTESIAN_POINT ( 'NONE',  ( -10.81189881249999729, 6.242252689847871849, -128.4062500020483810 ) ) ;
#30503 = CARTESIAN_POINT ( 'NONE',  ( 2.746439794587930194, 9.968836831075687854, -180.0000000000001421 ) ) ;
#30504 = CARTESIAN_POINT ( 'NONE',  ( -4.999999999999996447, 8.660254037844387298, -86.99999999999998579 ) ) ;
#30505 = CARTESIAN_POINT ( 'NONE',  ( -10.81189881249999729, 6.242252689847871849, -18.90625000204837391 ) ) ;
#30506 = ORIENTED_EDGE ( 'NONE', *, *, #22815, .T. ) ;
#30507 = CARTESIAN_POINT ( 'NONE',  ( -5.405949406249996869, 9.363379034771805109, -112.0312500020483810 ) ) ;
#30508 = CARTESIAN_POINT ( 'NONE',  ( -2.121150477449813534E-15, -11.54700538379251284, -124.2500000040967763 ) ) ;
#30509 = DIRECTION ( 'NONE',  ( 0.000000000000000000, 0.000000000000000000, -1.000000000000000000 ) ) ;
#30510 = CARTESIAN_POINT ( 'NONE',  ( 10.00000000000000000, 5.773502691896255534, -35.25000000409675494 ) ) ;
#30511 = CYLINDRICAL_SURFACE ( 'NONE', #31812, 9.999999999999998224 ) ;
#30512 = CARTESIAN_POINT ( 'NONE',  ( 7.644554776091147741E-16, 12.48450537969573659, -52.15625000204838102 ) ) ;
#30513 = AXIS2_PLACEMENT_3D ( 'NONE', #21761, #21968, #34939 ) ;
#30514 = CARTESIAN_POINT ( 'NONE',  ( 5.000000000000000000, 8.660254037844385522, -76.74999999999998579 ) ) ;
#30515 = CARTESIAN_POINT ( 'NONE',  ( 10.81189881249999729, 0.000000000000000000, -153.0312500020484094 ) ) ;
#30516 = CARTESIAN_POINT ( 'NONE',  ( 10.81189881249999907, 6.242252689847868297, -131.7187500020483810 ) ) ;
#30517 = CARTESIAN_POINT ( 'NONE',  ( -9.999999999999998224, 1.224646799147353059E-15, -143.7500000000000000 ) ) ;
#30518 = VERTEX_POINT ( 'NONE', #15156 ) ;
#30519 = CARTESIAN_POINT ( 'NONE',  ( 9.999999999999998224, 0.000000000000000000, -15.87500000409675138 ) ) ;
#30520 = ORIENTED_EDGE ( 'NONE', *, *, #10764, .F. ) ;
#30521 = ORIENTED_EDGE ( 'NONE', *, *, #31252, .F. ) ;
#30522 = CALENDAR_DATE ( 2026, 28, 9 ) ;
#30524 = ORIENTED_EDGE ( 'NONE', *, *, #28347, .F. ) ;
#30523 = CARTESIAN_POINT ( 'NONE',  ( -5.405949406249996869, 9.363379034771805109, -110.3437500020483810 ) ) ;
#30525 = CARTESIAN_POINT ( 'NONE',  ( 9.999999999999998224, 0.000000000000000000, -103.9999999999999858 ) ) ;
#30526 = CARTESIAN_POINT ( 'NONE',  ( -2.293366432827344421E-15, -12.48450537969573659, -190.7187500020484094 ) ) ;
#30528 = EDGE_CURVE ( 'NONE', #5068, #28118, #2448, .T. ) ;
#30527 = CARTESIAN_POINT ( 'NONE',  ( -5.405949406249996869, 9.363379034771805109, -42.84375000204837391 ) ) ;
#30529 = CARTESIAN_POINT ( 'NONE',  ( -9.999999999999998224, 1.224646799147353059E-15, -94.62500000409677625 ) ) ;
#30530 = CARTESIAN_POINT ( 'NONE',  ( -2.121150477449813534E-15, -11.54700538379251284, -31.25000000409674783 ) ) ;
#30531 = CARTESIAN_POINT ( 'NONE',  ( 5.405949406249992428, -9.363379034771808662, -181.5937500020483810 ) ) ;
#30532 = CARTESIAN_POINT ( 'NONE',  ( -2.293366432827344421E-15, -12.48450537969573659, -159.2187500020483810 ) ) ;
#30533 = CARTESIAN_POINT ( 'NONE',  ( -9.999999999999479527, -5.773502691896549521, -123.0000000040967763 ) ) ;
#30534 = CARTESIAN_POINT ( 'NONE',  ( 10.81189881249999729, 0.000000000000000000, -143.8437500020483810 ) ) ;
#30535 = CARTESIAN_POINT ( 'NONE',  ( -10.81189881249999729, 6.242252689847871849, -164.2187500020483810 ) ) ;
#30536 = CARTESIAN_POINT ( 'NONE',  ( -10.00000000000076916, 5.773502691895813221, -133.7500000040967905 ) ) ;
#30537 = CARTESIAN_POINT ( 'NONE',  ( 7.070501591499376803E-16, 11.54700538379251284, -36.12499999999996447 ) ) ;
#30538 = CARTESIAN_POINT ( 'NONE',  ( -2.121150477449813534E-15, -11.54700538379251284, -176.3750000000000000 ) ) ;
#30539 = CARTESIAN_POINT ( 'NONE',  ( -10.81189881249999729, 6.242252689847871849, -87.71875000204838102 ) ) ;
#30540 = CARTESIAN_POINT ( 'NONE',  ( -4.999999999999996447, 8.660254037844387298, -151.5000000000000000 ) ) ;
#30541 = CARTESIAN_POINT ( 'NONE',  ( -10.81189881249999729, 6.242252689847871849, -63.90625000204836681 ) ) ;
#30542 = CARTESIAN_POINT ( 'NONE',  ( -10.81189881249999729, 1.324075727343319199E-15, -174.5937500020484094 ) ) ;
#30543 = CARTESIAN_POINT ( 'NONE',  ( 10.81189881249999729, 0.000000000000000000, -121.5312500020483952 ) ) ;
#30544 = CARTESIAN_POINT ( 'NONE',  ( 10.81189881249999729, 6.242252689847867408, -157.4062500020483810 ) ) ;
#30545 = CARTESIAN_POINT ( 'NONE',  ( 10.81189881249999551, -6.242252689847874514, -49.65625000204837391 ) ) ;
#30546 = CARTESIAN_POINT ( 'NONE',  ( -4.999999999999996447, 8.660254037844387298, -133.8750000040967905 ) ) ;
#30547 = CARTESIAN_POINT ( 'NONE',  ( 4.999999999999992006, -8.660254037844389075, -110.2499999999999858 ) ) ;
#30548 = EDGE_CURVE ( 'NONE', #14006, #30625, #8710, .T. ) ;
#30549 = EDGE_LOOP ( 'NONE', ( #9224, #20348, #31479, #22713 ) ) ;
#30550 = CARTESIAN_POINT ( 'NONE',  ( 5.405949406249992428, -9.363379034771808662, -135.2812500020483810 ) ) ;
#30551 = CARTESIAN_POINT ( 'NONE',  ( -4.999999999999996447, 8.660254037844387298, -157.8750000040967905 ) ) ;
#30552 = CARTESIAN_POINT ( 'NONE',  ( 10.81189881249999551, -6.242252689847874514, -150.1562500020484094 ) ) ;
#30553 = CARTESIAN_POINT ( 'NONE',  ( -5.405949406250003975, -9.363379034771801557, -185.0312500020484094 ) ) ;
#30554 = CARTESIAN_POINT ( 'NONE',  ( 10.81189881249999551, -6.242252689847874514, -82.46875000204836681 ) ) ;
#30555 = ORIENTED_EDGE ( 'NONE', *, *, #4854, .T. ) ;
#30556 = CARTESIAN_POINT ( 'NONE',  ( 4.999999999999992006, -8.660254037844389075, -47.24999999999998579 ) ) ;
#30557 = CARTESIAN_POINT ( 'NONE',  ( 10.81189881249999729, 0.000000000000000000, -179.8437500020483810 ) ) ;
#30558 = CARTESIAN_POINT ( 'NONE',  ( 5.000000000000000000, 8.660254037844385522, -57.62500000409676204 ) ) ;
#30559 = CARTESIAN_POINT ( 'NONE',  ( -10.81189881249999729, 1.324075727343319199E-15, -75.78125000204838102 ) ) ;
#30560 = CARTESIAN_POINT ( 'NONE',  ( 5.405949406249992428, -9.363379034771808662, -61.78125000204837391 ) ) ;
#30561 = CARTESIAN_POINT ( 'NONE',  ( 7.070501591499377789E-16, 11.54700538379251284, -51.50000000409676915 ) ) ;
#30562 = CARTESIAN_POINT ( 'NONE',  ( 5.405949406249992428, -9.363379034771808662, -10.59375000204834727 ) ) ;
#30563 = DIRECTION ( 'NONE',  ( -0.000000000000000000, -0.000000000000000000, 1.000000000000000000 ) ) ;
#30564 = CARTESIAN_POINT ( 'NONE',  ( -5.405949406250003975, -9.363379034771801557, -174.5312500020484094 ) ) ;
#30565 = CARTESIAN_POINT ( 'NONE',  ( 5.405949406249992428, -9.363379034771808662, -1.781250002048373471 ) ) ;
#30566 = CARTESIAN_POINT ( 'NONE',  ( -9.999999999999998224, 1.224646799147353059E-15, -73.62500000409677625 ) ) ;
#30567 = CARTESIAN_POINT ( 'NONE',  ( -9.999999999999998224, 1.224646799147353059E-15, -67.62500000409676204 ) ) ;
#30568 = CARTESIAN_POINT ( 'NONE',  ( 5.321294541346989426, 5.321294541346989426, -219.9999999999999716 ) ) ;
#30569 =( BOUNDED_CURVE ( )  B_SPLINE_CURVE ( 2, ( #36391, #16298, #39614, #20613, #20195, #23663, #366 ),
 .UNSPECIFIED., .F., .F. ) 
 B_SPLINE_CURVE_WITH_KNOTS ( ( 3, 2, 2, 3 ),
 ( 0.2500000000000001110, 0.2512437810945274963, 0.2524875621890548261, 0.2537313432835822113 ),
 .UNSPECIFIED. ) 
 CURVE ( )  GEOMETRIC_REPRESENTATION_ITEM ( )  RATIONAL_B_SPLINE_CURVE ( ( 0.9999999999999880096, 0.8660254037844506980, 1.000000000000000000, 0.8660254037844387076, 1.000000000000000000, 0.8660254037844267172, 1.000000000000011990 ) ) 
 REPRESENTATION_ITEM ( '' )  );
#30570 = FACE_OUTER_BOUND ( 'NONE', #19909, .T. ) ;
#30572 = ORIENTED_EDGE ( 'NONE', *, *, #6976, .F. ) ;
#30571 = CARTESIAN_POINT ( 'NONE',  ( -10.81189881249999729, 1.324075727343319199E-15, -84.78125000204838102 ) ) ;
#30574 = VERTEX_POINT ( 'NONE', #15581 ) ;
#30573 = CARTESIAN_POINT ( 'NONE',  ( 5.000000000000000000, 8.660254037844385522, -81.24999999999998579 ) ) ;
#30575 = ORIENTED_EDGE ( 'NONE', *, *, #41499, .F. ) ;
#30576 = EDGE_CURVE ( 'NONE', #14677, #21458, #8393, .T. ) ;
#30577 = CARTESIAN_POINT ( 'NONE',  ( 10.81189881249999907, 6.242252689847868297, -26.71875000204838102 ) ) ;
#30578 = CARTESIAN_POINT ( 'NONE',  ( 5.405949406249992428, -9.363379034771808662, -13.78125000204835615 ) ) ;
#30579 = CARTESIAN_POINT ( 'NONE',  ( 5.405949406249999534, 9.363379034771803333, -64.09375000204836681 ) ) ;
#30580 = CARTESIAN_POINT ( 'NONE',  ( 10.00000000000025402, -5.773502691896113426, -122.1250000000000000 ) ) ;
#30581 = CARTESIAN_POINT ( 'NONE',  ( 4.999999999999992006, -8.660254037844389075, -47.24999999999998579 ) ) ;
#30582 = CARTESIAN_POINT ( 'NONE',  ( -10.81189881249999907, -6.242252689847864744, -186.4687500020484094 ) ) ;
#30583 = CARTESIAN_POINT ( 'NONE',  ( 5.405949406249992428, -9.363379034771808662, -163.5937500020484094 ) ) ;
#30584 = CARTESIAN_POINT ( 'NONE',  ( 9.999999999999479527, 5.773502691896553074, -175.8749999999999716 ) ) ;
#30585 = CARTESIAN_POINT ( 'NONE',  ( -4.999999999999996447, 8.660254037844387298, -132.0000000000000000 ) ) ;
#30586 = CARTESIAN_POINT ( 'NONE',  ( 5.000000000000000000, 8.660254037844385522, -71.12500000409677625 ) ) ;
#30587 = CARTESIAN_POINT ( 'NONE',  ( 35.00000000000000711, 4.286263797015737285E-15, -176.9999999999999432 ) ) ;
#30588 = CARTESIAN_POINT ( 'NONE',  ( 10.81189881249999907, 6.242252689847868297, -115.2187500020483810 ) ) ;
#30589 = CARTESIAN_POINT ( 'NONE',  ( 9.999999999999998224, 0.000000000000000000, -63.49999999999997158 ) ) ;
#30590 = CARTESIAN_POINT ( 'NONE',  ( -2.293366432827344421E-15, -12.48450537969573659, -88.90625000204838102 ) ) ;
#30591 = CARTESIAN_POINT ( 'NONE',  ( -10.81189881249999729, 1.324075727343319199E-15, -101.0937500020483810 ) ) ;
#30592 = EDGE_CURVE ( 'NONE', #13797, #37668, #18187, .T. ) ;
#30593 = CARTESIAN_POINT ( 'NONE',  ( -10.81189881249999729, 1.324075727343319199E-15, -69.59375000204836681 ) ) ;
#30594 = CARTESIAN_POINT ( 'NONE',  ( -2.293366432827344421E-15, -12.48450537969573659, -76.90625000204839523 ) ) ;
#30595 = CARTESIAN_POINT ( 'NONE',  ( 4.999999999999992006, -8.660254037844389075, -151.1250000040967905 ) ) ;
#30596 = CARTESIAN_POINT ( 'NONE',  ( 10.00000000000000000, 5.773502691896255534, -129.3750000000000000 ) ) ;
#30597 = CARTESIAN_POINT ( 'NONE',  ( 5.405949406249999534, 9.363379034771803333, -157.2812500020484094 ) ) ;
#30598 = CARTESIAN_POINT ( 'NONE',  ( 10.81189881249999729, 0.000000000000000000, -175.5312500020483810 ) ) ;
#30599 = CARTESIAN_POINT ( 'NONE',  ( 10.81189881249999729, 0.000000000000000000, 0.1562499979516351889 ) ) ;
#30600 = DIRECTION ( 'NONE',  ( -0.000000000000000000, -0.000000000000000000, 1.000000000000000000 ) ) ;
#30601 = CARTESIAN_POINT ( 'NONE',  ( 10.81189881249999729, 0.000000000000000000, -106.3437500020483810 ) ) ;
#30602 = CARTESIAN_POINT ( 'NONE',  ( 9.999999999999998224, 0.000000000000000000, -176.0000000000000000 ) ) ;
#30603 = CARTESIAN_POINT ( 'NONE',  ( 7.070501591499377789E-16, 11.54700538379251284, -75.12500000000000000 ) ) ;
#30604 = CARTESIAN_POINT ( 'NONE',  ( -5.405949406250003975, -9.363379034771801557, -8.031250002048350822 ) ) ;
#30605 = CARTESIAN_POINT ( 'NONE',  ( -9.999999999999998224, 5.773502691896259087, -90.25000000409676204 ) ) ;
#30606 = CARTESIAN_POINT ( 'NONE',  ( 4.999999999999992006, -8.660254037844389075, -168.7500000000000000 ) ) ;
#30607 = CARTESIAN_POINT ( 'NONE',  ( -5.405949406249996869, 9.363379034771805109, -101.5312500020483952 ) ) ;
#30608 = CARTESIAN_POINT ( 'NONE',  ( -10.81189881249999729, 6.242252689847871849, -81.90625000204839523 ) ) ;
#30609 = CARTESIAN_POINT ( 'NONE',  ( 10.00000000000000000, 5.773502691896255534, -72.75000000409674783 ) ) ;
#30610 = CARTESIAN_POINT ( 'NONE',  ( 5.000000000000000000, 8.660254037844385522, -113.1250000040967763 ) ) ;
#30611 = CARTESIAN_POINT ( 'NONE',  ( 7.644554776091147741E-16, 12.48450537969573659, -33.96875000204835260 ) ) ;
#30612 = ORIENTED_EDGE ( 'NONE', *, *, #34237, .F. ) ;
#30613 = CARTESIAN_POINT ( 'NONE',  ( 5.000000000000000000, 8.660254037844385522, -3.249999999999975131 ) ) ;
#30614 = CARTESIAN_POINT ( 'NONE',  ( -10.81189881249999729, 1.324075727343319199E-15, -32.28125000204837391 ) ) ;
#30615 = CARTESIAN_POINT ( 'NONE',  ( 10.81189881249999729, 6.242252689847867408, -13.21875000204836326 ) ) ;
#30616 = FACE_OUTER_BOUND ( 'NONE', #39157, .T. ) ;
#30617 = CARTESIAN_POINT ( 'NONE',  ( 4.999999999999992006, -8.660254037844389075, -1.125000004096765593 ) ) ;
#30618 = CARTESIAN_POINT ( 'NONE',  ( -10.81189881249999729, 1.324075727343319199E-15, -128.2812500020483810 ) ) ;
#30619 = CARTESIAN_POINT ( 'NONE',  ( 9.999999999999998224, 0.000000000000000000, -179.0000000000000000 ) ) ;
#30620 = CARTESIAN_POINT ( 'NONE',  ( -9.999999999999678479, -5.773502691896439387, -184.5000000040968189 ) ) ;
#30622 = ORIENTED_EDGE ( 'NONE', *, *, #33066, .F. ) ;
#30621 = CARTESIAN_POINT ( 'NONE',  ( -5.405949406250003975, -9.363379034771801557, -107.0312500020483810 ) ) ;
#30623 = CYLINDRICAL_SURFACE ( 'NONE', #30387, 9.999999999999998224 ) ;
#30624 = ORIENTED_EDGE ( 'NONE', *, *, #21185, .T. ) ;
#30625 = VERTEX_POINT ( 'NONE', #14940 ) ;
#30626 = CARTESIAN_POINT ( 'NONE',  ( 5.405949406249999534, 9.363379034771803333, -34.28125000204837391 ) ) ;
#30627 = PERSON_AND_ORGANIZATION ( #11915, #17965 ) ;
#30628 = CARTESIAN_POINT ( 'NONE',  ( -5.405949406250003975, -9.363379034771801557, -96.34375000204838102 ) ) ;
#30629 = FACE_OUTER_BOUND ( 'NONE', #31400, .T. ) ;
#30630 = CARTESIAN_POINT ( 'NONE',  ( 10.00000000000025402, -5.773502691896113426, -128.5000000040967905 ) ) ;
#30631 = CARTESIAN_POINT ( 'NONE',  ( 5.405949406249999534, 9.363379034771803333, -196.0937500020484094 ) ) ;
#30632 = CARTESIAN_POINT ( 'NONE',  ( -10.81189881249999907, -6.242252689847864744, -174.6562500020483810 ) ) ;
#30633 = CARTESIAN_POINT ( 'NONE',  ( -2.121150477449813534E-15, -11.54700538379251284, -138.8750000000000000 ) ) ;
#30634 = CARTESIAN_POINT ( 'NONE',  ( 7.644554776091147741E-16, 12.48450537969573659, -125.4687500020483952 ) ) ;
#30635 = CARTESIAN_POINT ( 'NONE',  ( 10.81189881249999907, 6.242252689847868297, -95.71875000204838102 ) ) ;
#30636 = CARTESIAN_POINT ( 'NONE',  ( 7.070501591499376803E-16, 11.54700538379251284, -113.0000000040967763 ) ) ;
#30637 = CARTESIAN_POINT ( 'NONE',  ( 5.405949406249992428, -9.363379034771808662, -99.28125000204839523 ) ) ;
#30638 = CARTESIAN_POINT ( 'NONE',  ( 10.00000000000000000, 5.773502691896255534, -188.2500000040968189 ) ) ;
#30639 = CARTESIAN_POINT ( 'NONE',  ( 10.81189881249999729, 0.000000000000000000, -107.8437500020483810 ) ) ;
#30640 = CARTESIAN_POINT ( 'NONE',  ( 10.81189881249999551, -6.242252689847874514, -181.6562500020484379 ) ) ;
#30641 = CARTESIAN_POINT ( 'NONE',  ( -9.999999999999998224, 1.224646799147353059E-15, -1.625000004096766038 ) ) ;
#30642 = CARTESIAN_POINT ( 'NONE',  ( 4.999999999999992006, -8.660254037844389075, -152.6250000040967905 ) ) ;
#30643 = CARTESIAN_POINT ( 'NONE',  ( 7.070501591499377789E-16, 11.54700538379251284, -0.1249999999999584777 ) ) ;
#30644 = CARTESIAN_POINT ( 'NONE',  ( 10.81189881249999551, -6.242252689847874514, -49.46875000204835970 ) ) ;
#30645 = CARTESIAN_POINT ( 'NONE',  ( 10.81189881249999729, 0.000000000000000000, -44.84375000204837391 ) ) ;
#30646 = CARTESIAN_POINT ( 'NONE',  ( -9.999999999999998224, 5.773502691896259087, -168.2500000040967905 ) ) ;
#30647 = CARTESIAN_POINT ( 'NONE',  ( 10.81189881249999551, -6.242252689847874514, -9.156250002048375691 ) ) ;
#30648 = CARTESIAN_POINT ( 'NONE',  ( 10.81189881249999729, 0.000000000000000000, -23.84375000204835970 ) ) ;
#30649 = CARTESIAN_POINT ( 'NONE',  ( 9.999999999999998224, 0.000000000000000000, -10.99999999999995381 ) ) ;
#30650 = CARTESIAN_POINT ( 'NONE',  ( 7.644554776091147741E-16, 12.48450537969573659, -128.4687500020483810 ) ) ;
#30651 = EDGE_CURVE ( 'NONE', #34879, #42377, #40875, .T. ) ;
#30652 = CARTESIAN_POINT ( 'NONE',  ( -9.999999999999998224, 1.224646799147353059E-15, -98.74999999999998579 ) ) ;
#30653 = CARTESIAN_POINT ( 'NONE',  ( 7.644554776091147741E-16, 12.48450537969573659, -26.65625000204838102 ) ) ;
#30654 = CARTESIAN_POINT ( 'NONE',  ( -9.999999999999998224, 5.773502691896259087, -111.2500000040967763 ) ) ;
#30655 =( BOUNDED_CURVE ( )  B_SPLINE_CURVE ( 2, ( #13871, #23832, #7635 ),
 .UNSPECIFIED., .F., .F. ) 
 B_SPLINE_CURVE_WITH_KNOTS ( ( 3, 3 ),
 ( 0.09950248756218914303, 0.1007462686567163757 ),
 .UNSPECIFIED. ) 
 CURVE ( )  GEOMETRIC_REPRESENTATION_ITEM ( )  RATIONAL_B_SPLINE_CURVE ( ( 0.9999999999999910072, 0.8660254037844521413, 0.9999999999999955591 ) ) 
 REPRESENTATION_ITEM ( '' )  );
#30656 = CARTESIAN_POINT ( 'NONE',  ( 5.000000000000000000, 8.660254037844385522, -158.1250000040967905 ) ) ;
#30657 = EDGE_CURVE ( 'NONE', #29774, #23180, #2870, .T. ) ;
#30658 = CARTESIAN_POINT ( 'NONE',  ( 9.999999999999998224, 0.000000000000000000, -61.99999999999997158 ) ) ;
#30659 = CARTESIAN_POINT ( 'NONE',  ( -2.293366432827344421E-15, -12.48450537969573659, -123.4062500020484094 ) ) ;
#30660 = CARTESIAN_POINT ( 'NONE',  ( 10.81189881249999729, 0.000000000000000000, -105.0312500020483810 ) ) ;
#30661 = ORIENTED_EDGE ( 'NONE', *, *, #21376, .F. ) ;
#30662 = LINE ( 'NONE', #22164, #41704 ) ;
#30663 = CARTESIAN_POINT ( 'NONE',  ( 4.999999999999992006, -8.660254037844389075, -98.62500000409677625 ) ) ;
#30664 = CARTESIAN_POINT ( 'NONE',  ( -2.121150477449813534E-15, -11.54700538379251284, -151.2500000040968189 ) ) ;
#30665 = CARTESIAN_POINT ( 'NONE',  ( -10.81189881249999729, 6.242252689847871849, -60.71875000204838102 ) ) ;
#30666 = ORIENTED_EDGE ( 'NONE', *, *, #25456, .F. ) ;
#30667 = CARTESIAN_POINT ( 'NONE',  ( 4.999999999999992006, -8.660254037844389075, -23.24999999999996447 ) ) ;
#30668 = CARTESIAN_POINT ( 'NONE',  ( 5.405949406249999534, 9.363379034771803333, -38.78125000204838102 ) ) ;
#30669 = CARTESIAN_POINT ( 'NONE',  ( 7.070501591499377789E-16, 11.54700538379251284, -163.6250000000000000 ) ) ;
#30670 = CARTESIAN_POINT ( 'NONE',  ( -9.999999999999998224, 1.224646799147353059E-15, -103.2500000000000000 ) ) ;
#30671 = CARTESIAN_POINT ( 'NONE',  ( -9.999999999999998224, 1.224646799147353059E-15, -31.62500000409676559 ) ) ;
#30672 = CARTESIAN_POINT ( 'NONE',  ( -5.405949406249996869, 9.363379034771805109, -136.0312500020484094 ) ) ;
#30673 = CARTESIAN_POINT ( 'NONE',  ( 7.070501591499376803E-16, 11.54700538379251284, -167.0000000040967905 ) ) ;
#30674 = VERTEX_POINT ( 'NONE', #36302 ) ;
#30676 = ORIENTED_EDGE ( 'NONE', *, *, #3288, .T. ) ;
#30675 = EDGE_LOOP ( 'NONE', ( #14962, #25097, #38157, #41246 ) ) ;
#30677 = LINE ( 'NONE', #31110, #38305 ) ;
#30678 = DIRECTION ( 'NONE',  ( 8.659560562354918067E-17, -0.7071067811865487940, 0.7071067811865463515 ) ) ;
#30679 = CARTESIAN_POINT ( 'NONE',  ( -10.81189881249999907, -6.242252689847864744, -168.4687500020483526 ) ) ;
#30680 = AXIS2_PLACEMENT_3D ( 'NONE', #31198, #34434, #24940 ) ;
#30681 = CARTESIAN_POINT ( 'NONE',  ( 10.81189881249999551, -6.242252689847874514, -193.6562500020484379 ) ) ;
#30682 = CARTESIAN_POINT ( 'NONE',  ( -10.81189881249999907, -6.242252689847864744, -13.96875000204836681 ) ) ;
#30683 = CARTESIAN_POINT ( 'NONE',  ( 7.070501591499376803E-16, 11.54700538379251284, -150.1250000000000000 ) ) ;
#30684 = CARTESIAN_POINT ( 'NONE',  ( -2.293366432827344421E-15, -12.48450537969573659, -148.7187500020484094 ) ) ;
#30685 = CARTESIAN_POINT ( 'NONE',  ( -10.81189881249999907, -6.242252689847864744, -133.9687500020483810 ) ) ;
#30686 = CARTESIAN_POINT ( 'NONE',  ( 5.405949406249999534, 9.363379034771803333, -106.2812500020483810 ) ) ;
#30687 = CARTESIAN_POINT ( 'NONE',  ( 10.81189881249999551, -6.242252689847874514, -119.9687500020483952 ) ) ;
#30688 = CARTESIAN_POINT ( 'NONE',  ( -4.999999999999996447, 8.660254037844387298, -196.8750000040967905 ) ) ;
#30689 = CARTESIAN_POINT ( 'NONE',  ( 10.81189881249999729, 0.000000000000000000, -124.5312500020483952 ) ) ;
#30690 = CARTESIAN_POINT ( 'NONE',  ( 10.81189881249999907, 6.242252689847868297, -8.718750002048356151 ) ) ;
#30691 = CARTESIAN_POINT ( 'NONE',  ( -10.81189881249999729, 6.242252689847871849, -129.7187500020483810 ) ) ;
#30692 = CARTESIAN_POINT ( 'NONE',  ( 10.81189881249999729, 0.000000000000000000, -199.5312500020484094 ) ) ;
#30693 =( BOUNDED_CURVE ( )  B_SPLINE_CURVE ( 2, ( #7915, #40687, #11344, #14576, #30585, #41111, #14786 ),
 .UNSPECIFIED., .F., .F. ) 
 B_SPLINE_CURVE_WITH_KNOTS ( ( 3, 2, 2, 3 ),
 ( 0.3358208955223880854, 0.3370646766169154707, 0.3383084577114429670, 0.3395522388059703522 ),
 .UNSPECIFIED. ) 
 CURVE ( )  GEOMETRIC_REPRESENTATION_ITEM ( )  RATIONAL_B_SPLINE_CURVE ( ( 1.000000000000000000, 0.8660254037844387076, 1.000000000000000000, 0.8660254037844387076, 1.000000000000000000, 0.8660254037844148378, 1.000000000000023981 ) ) 
 REPRESENTATION_ITEM ( '' )  );
#30694 = CARTESIAN_POINT ( 'NONE',  ( 9.999999999999612754, 5.773502691896477579, -179.2500000040967905 ) ) ;
#30695 = CARTESIAN_POINT ( 'NONE',  ( -5.000000000000003553, -8.660254037844383745, -158.5000000000000000 ) ) ;
#30696 = CARTESIAN_POINT ( 'NONE',  ( -4.999999999999996447, 8.660254037844387298, -22.49999999999996447 ) ) ;
#30697 = CARTESIAN_POINT ( 'NONE',  ( -2.293366432827344421E-15, -12.48450537969573659, -79.71875000204838102 ) ) ;
#30698 = CARTESIAN_POINT ( 'NONE',  ( -5.405949406250003975, -9.363379034771801557, -61.84375000204836681 ) ) ;
#30699 = CARTESIAN_POINT ( 'NONE',  ( -9.999999999999872102, -5.773502691896326589, -167.6250000000000000 ) ) ;
#30700 = CARTESIAN_POINT ( 'NONE',  ( 5.405949406249992428, -9.363379034771808662, -33.28125000204837391 ) ) ;
#30701 = CARTESIAN_POINT ( 'NONE',  ( -5.405949406249996869, 9.363379034771805109, -44.34375000204837391 ) ) ;
#30702 = DIRECTION ( 'NONE',  ( 1.000000000000000000, 0.000000000000000000, 0.000000000000000000 ) ) ;
#30703 = CARTESIAN_POINT ( 'NONE',  ( 7.644554776091147741E-16, 12.48450537969573659, -150.9687500020483810 ) ) ;
#30704 = EDGE_CURVE ( 'NONE', #18780, #12159, #25752, .T. ) ;
#30705 = CARTESIAN_POINT ( 'NONE',  ( 9.999999999999998224, 0.000000000000000000, -123.5000000000000000 ) ) ;
#30706 = CARTESIAN_POINT ( 'NONE',  ( -2.293366432827344421E-15, -12.48450537969573659, -132.4062500020483810 ) ) ;
#30707 = CARTESIAN_POINT ( 'NONE',  ( -4.999999999999996447, 8.660254037844387298, -180.0000000000000000 ) ) ;
#30708 = AXIS2_PLACEMENT_3D ( 'NONE', #31606, #11292, #40635 ) ;
#30709 = CARTESIAN_POINT ( 'NONE',  ( -9.999999999999998224, 1.224646799147353059E-15, -85.24999999999997158 ) ) ;
#30710 = CARTESIAN_POINT ( 'NONE',  ( -5.405949406250003975, -9.363379034771801557, -15.53125000204835793 ) ) ;
#30711 = EDGE_CURVE ( 'NONE', #22759, #16098, #24657, .T. ) ;
#30712 = ORIENTED_EDGE ( 'NONE', *, *, #29653, .T. ) ;
#30713 =( BOUNDED_CURVE ( )  B_SPLINE_CURVE ( 2, ( #6248, #2168, #15506, #35395, #5819, #15303, #38405 ),
 .UNSPECIFIED., .F., .F. ) 
 B_SPLINE_CURVE_WITH_KNOTS ( ( 3, 2, 2, 3 ),
 ( 0.6343283582089553896, 0.6355721393034826638, 0.6368159203980100491, 0.6380597014925374344 ),
 .UNSPECIFIED. ) 
 CURVE ( )  GEOMETRIC_REPRESENTATION_ITEM ( )  RATIONAL_B_SPLINE_CURVE ( ( 0.9999999999999880096, 0.8660254037844506980, 1.000000000000000000, 0.8660254037844387076, 1.000000000000000000, 0.8660254037844267172, 1.000000000000011990 ) ) 
 REPRESENTATION_ITEM ( '' )  );
#30714 = CARTESIAN_POINT ( 'NONE',  ( -9.999999999999872102, -5.773502691896326589, -164.6249999999999716 ) ) ;
#30715 = CARTESIAN_POINT ( 'NONE',  ( 4.999999999999992006, -8.660254037844389075, -121.1250000040967905 ) ) ;
#30716 = CARTESIAN_POINT ( 'NONE',  ( 7.070501591499376803E-16, 11.54700538379251284, -9.124999999999978684 ) ) ;
#30717 = EDGE_CURVE ( 'NONE', #6996, #37716, #26278, .T. ) ;
#30718 = CARTESIAN_POINT ( 'NONE',  ( -9.999999999999998224, 5.773502691896259087, -33.25000000409676204 ) ) ;
#30719 = CARTESIAN_POINT ( 'NONE',  ( -9.999999999999998224, 1.224646799147353059E-15, -200.0000000000000000 ) ) ;
#30720 = APPROVAL ( #26532, 'UNSPECIFIED' ) ;
#30721 = CARTESIAN_POINT ( 'NONE',  ( -10.81189881249999907, -6.242252689847864744, -53.15625000204837391 ) ) ;
#30722 = CARTESIAN_POINT ( 'NONE',  ( 0.000000000000000000, 0.000000000000000000, -200.0000000000000000 ) ) ;
#30723 = CARTESIAN_POINT ( 'NONE',  ( -2.293366432827344421E-15, -12.48450537969573659, -153.4062500020483810 ) ) ;
#30724 = CARTESIAN_POINT ( 'NONE',  ( -10.81189881249999729, 1.324075727343319199E-15, -123.5937500020483952 ) ) ;
#30725 = CARTESIAN_POINT ( 'NONE',  ( -9.999999999999998224, 1.224646799147353059E-15, -165.1250000040967905 ) ) ;
#30726 = EDGE_LOOP ( 'NONE', ( #29812, #3815, #24583, #37568 ) ) ;
#30727 = DIRECTION ( 'NONE',  ( -0.000000000000000000, -0.000000000000000000, -1.000000000000000000 ) ) ;
#30728 = VERTEX_POINT ( 'NONE', #42547 ) ;
#30729 = EDGE_CURVE ( 'NONE', #20886, #12962, #12765, .T. ) ;
#30730 = VERTEX_POINT ( 'NONE', #6523 ) ;
#30732 = ORIENTED_EDGE ( 'NONE', *, *, #9216, .F. ) ;
#30731 = CARTESIAN_POINT ( 'NONE',  ( -5.405949406249996869, 9.363379034771805109, -111.8437500020483810 ) ) ;
#30733 = CARTESIAN_POINT ( 'NONE',  ( 10.81189881249999907, 6.242252689847868297, -187.2187500020484094 ) ) ;
#30734 = CARTESIAN_POINT ( 'NONE',  ( 7.644554776091147741E-16, 12.48450537969573659, -39.96875000204835970 ) ) ;
#30735 = CARTESIAN_POINT ( 'NONE',  ( -9.999999999999742428, -5.773502691896402084, -156.0000000040968473 ) ) ;
#30736 = CARTESIAN_POINT ( 'NONE',  ( -2.121150477449813534E-15, -11.54700538379251284, -10.25000000409676026 ) ) ;
#30737 = CARTESIAN_POINT ( 'NONE',  ( -2.293366432827344421E-15, -12.48450537969573659, -174.2187500020483810 ) ) ;
#30738 = AXIS2_PLACEMENT_3D ( 'NONE', #13177, #22493, #6100 ) ;
#30739 = CARTESIAN_POINT ( 'NONE',  ( 5.405949406249992428, -9.363379034771808662, -157.5937500020483810 ) ) ;
#30740 = CARTESIAN_POINT ( 'NONE',  ( 9.999999999999998224, 0.000000000000000000, -179.0000000000000000 ) ) ;
#30741 = CARTESIAN_POINT ( 'NONE',  ( -5.405949406250003975, -9.363379034771801557, -138.3437500020484094 ) ) ;
#30742 = CARTESIAN_POINT ( 'NONE',  ( -5.405949406250003975, -9.363379034771801557, -156.3437500020483810 ) ) ;
#30743 = CARTESIAN_POINT ( 'NONE',  ( 10.00000000000051159, -5.773502691895965988, -42.62499999999996447 ) ) ;
#30744 = CARTESIAN_POINT ( 'NONE',  ( -9.999999999999998224, 1.224646799147353059E-15, -36.12500000409676915 ) ) ;
#30745 = CARTESIAN_POINT ( 'NONE',  ( -2.121150477449813534E-15, -11.54700538379251284, -180.8750000000000000 ) ) ;
#30746 = CARTESIAN_POINT ( 'NONE',  ( 10.81189881249999907, 6.242252689847868297, -88.21875000204838102 ) ) ;
#30747 = CARTESIAN_POINT ( 'NONE',  ( -2.170677449821584837, 10.59771640374526314, -100.0000000000000000 ) ) ;
#30748 = CARTESIAN_POINT ( 'NONE',  ( -10.81189881249999729, 6.242252689847871849, -54.90625000204836681 ) ) ;
#30749 = CARTESIAN_POINT ( 'NONE',  ( -10.81189881249999907, -6.242252689847864744, -174.4687500020484094 ) ) ;
#30750 = CARTESIAN_POINT ( 'NONE',  ( -5.405949406249996869, 9.363379034771805109, -124.0312500020483952 ) ) ;
#30751 = CARTESIAN_POINT ( 'NONE',  ( 5.405949406249999534, 9.363379034771803333, -157.2812500020484094 ) ) ;
#30752 = DIRECTION ( 'NONE',  ( -0.000000000000000000, -0.000000000000000000, -1.000000000000000000 ) ) ;
#30753 = CARTESIAN_POINT ( 'NONE',  ( -5.405949406250003975, -9.363379034771801557, -42.53125000204838102 ) ) ;
#30754 = CARTESIAN_POINT ( 'NONE',  ( 9.999999999999996447, -5.773502691896262640, -130.0000000040967905 ) ) ;
#30755 = CARTESIAN_POINT ( 'NONE',  ( 5.000000000000000000, 8.660254037844385522, -103.7500000000000000 ) ) ;
#30756 = ORIENTED_EDGE ( 'NONE', *, *, #27372, .F. ) ;
#30757 = CARTESIAN_POINT ( 'NONE',  ( 7.644554776091147741E-16, 12.48450537969573659, -134.6562500020483810 ) ) ;
#30758 = CARTESIAN_POINT ( 'NONE',  ( 4.999999999999992006, -8.660254037844389075, -149.6250000040967905 ) ) ;
#30759 = CARTESIAN_POINT ( 'NONE',  ( -10.81189881249999729, 1.324075727343319199E-15, -146.2812500020483810 ) ) ;
#30760 = CARTESIAN_POINT ( 'NONE',  ( 5.405949406249999534, 9.363379034771803333, -188.7812500020484094 ) ) ;
#30761 = VERTEX_POINT ( 'NONE', #33070 ) ;
#30762 = CARTESIAN_POINT ( 'NONE',  ( -9.999999999999998224, 5.773502691896259087, -46.37499999999995737 ) ) ;
#30763 = CARTESIAN_POINT ( 'NONE',  ( -5.405949406249996869, 9.363379034771805109, -179.3437500020483810 ) ) ;
#30764 = CARTESIAN_POINT ( 'NONE',  ( -4.999999999999996447, 8.660254037844387298, -57.37500000409676204 ) ) ;
#30765 = CARTESIAN_POINT ( 'NONE',  ( -9.999999999999998224, 1.224646799147353059E-15, -152.7500000000000000 ) ) ;
#30766 = DIRECTION ( 'NONE',  ( -0.000000000000000000, -0.000000000000000000, -1.000000000000000000 ) ) ;
#30767 = CARTESIAN_POINT ( 'NONE',  ( -5.405949406250003975, -9.363379034771801557, -74.03125000204838102 ) ) ;
#30768 = AXIS2_PLACEMENT_3D ( 'NONE', #34895, #24542, #21504 ) ;
#30769 = CARTESIAN_POINT ( 'NONE',  ( 10.81189881249999729, 0.000000000000000000, -49.53125000204838813 ) ) ;
#30770 = CARTESIAN_POINT ( 'NONE',  ( 9.999999999999998224, 0.000000000000000000, -48.87500000409678336 ) ) ;
#30771 = CARTESIAN_POINT ( 'NONE',  ( -10.81189881249999907, -6.242252689847864744, -12.46875000204836326 ) ) ;
#30772 = DIRECTION ( 'NONE',  ( -0.000000000000000000, -0.000000000000000000, -1.000000000000000000 ) ) ;
#30773 = CARTESIAN_POINT ( 'NONE',  ( 7.644554776091147741E-16, 12.48450537969573659, -175.1562500020484094 ) ) ;
#30774 = EDGE_CURVE ( 'NONE', #40153, #32646, #22718, .T. ) ;
#30775 = CARTESIAN_POINT ( 'NONE',  ( 10.81189881249999907, 6.242252689847868297, -2.906250002048360592 ) ) ;
#30776 = DIRECTION ( 'NONE',  ( -0.7071067811865417996, 8.659560562354863833E-17, 0.7071067811865532349 ) ) ;
#30777 = DIRECTION ( 'NONE',  ( -1.000000000000000000, 0.000000000000000000, 0.000000000000000000 ) ) ;
#30778 = DIRECTION ( 'NONE',  ( -1.000000000000000000, 0.000000000000000000, 0.000000000000000000 ) ) ;
#30779 = CARTESIAN_POINT ( 'NONE',  ( -4.999999999999996447, 8.660254037844387298, -39.37500000409676915 ) ) ;
#30781 = ORIENTED_EDGE ( 'NONE', *, *, #1444, .F. ) ;
#30780 = CARTESIAN_POINT ( 'NONE',  ( -10.81189881249999907, -6.242252689847864744, -87.65625000204836681 ) ) ;
#30782 =( NAMED_UNIT ( * ) PLANE_ANGLE_UNIT ( ) SI_UNIT ( $, .RADIAN. ) );
#30784 = VERTEX_POINT ( 'NONE', #19673 ) ;
#30783 = DIRECTION ( 'NONE',  ( -1.000000000000000000, 0.000000000000000000, 0.000000000000000000 ) ) ;
#30785 = ORIENTED_EDGE ( 'NONE', *, *, #34658, .F. ) ;
#30786 = CARTESIAN_POINT ( 'NONE',  ( 5.405949406249992428, -9.363379034771808662, -36.09375000204836681 ) ) ;
#30787 = CARTESIAN_POINT ( 'NONE',  ( 10.81189881249999729, 0.000000000000000000, -26.84375000204835970 ) ) ;
#30788 = CARTESIAN_POINT ( 'NONE',  ( 10.81189881249999729, 0.000000000000000000, -15.03125000204835793 ) ) ;
#30789 = CARTESIAN_POINT ( 'NONE',  ( -2.293366432827344421E-15, -12.48450537969573659, -64.71875000204838102 ) ) ;
#30790 = CARTESIAN_POINT ( 'NONE',  ( 0.000000000000000000, 0.000000000000000000, -200.0000000000000000 ) ) ;
#30791 = CARTESIAN_POINT ( 'NONE',  ( -4.999999999999996447, 8.660254037844387298, -41.99999999999997868 ) ) ;
#30792 = CARTESIAN_POINT ( 'NONE',  ( -10.81189881249999729, 6.242252689847871849, -183.7187500020484379 ) ) ;
#30793 = CARTESIAN_POINT ( 'NONE',  ( -10.81189881249999729, 6.242252689847871849, -162.7187500020483810 ) ) ;
#30794 = CARTESIAN_POINT ( 'NONE',  ( -10.00000000000102496, 5.773502691895664007, -43.37499999999993605 ) ) ;
#30795 = LINE ( 'NONE', #27765, #7444 ) ;
#30796 = DIRECTION ( 'NONE',  ( -0.000000000000000000, -1.000000000000000000, -0.000000000000000000 ) ) ;
#30797 = CARTESIAN_POINT ( 'NONE',  ( 10.81189881249999729, 0.000000000000000000, -109.3437500020483810 ) ) ;
#30798 = CARTESIAN_POINT ( 'NONE',  ( 0.000000000000000000, 20.00000000000000000, -232.0000000000000000 ) ) ;
#30799 = CARTESIAN_POINT ( 'NONE',  ( -2.293366432827344421E-15, -12.48450537969573659, -82.90625000204838102 ) ) ;
#30800 = CARTESIAN_POINT ( 'NONE',  ( 10.81189881249999729, 0.000000000000000000, -103.3437500020483668 ) ) ;
#30801 = CARTESIAN_POINT ( 'NONE',  ( 5.405949406249992428, -9.363379034771808662, -69.09375000204836681 ) ) ;
#30802 = CARTESIAN_POINT ( 'NONE',  ( 10.81189881249999551, -6.242252689847874514, -76.65625000204838102 ) ) ;
#30803 = CARTESIAN_POINT ( 'NONE',  ( 10.00000000000000000, 5.773502691896255534, -152.2500000040967620 ) ) ;
#30804 = CARTESIAN_POINT ( 'NONE',  ( -2.121150477449813534E-15, -11.54700538379251284, -129.8750000000000000 ) ) ;
#30805 = CARTESIAN_POINT ( 'NONE',  ( 10.81189881249999729, 6.242252689847867408, -161.9062500020483810 ) ) ;
#30806 = CARTESIAN_POINT ( 'NONE',  ( 10.81189881249999729, 0.000000000000000000, -174.0312500020484094 ) ) ;
#30807 = CARTESIAN_POINT ( 'NONE',  ( 7.070501591499376803E-16, 11.54700538379251284, -153.5000000040967905 ) ) ;
#30808 = CARTESIAN_POINT ( 'NONE',  ( 4.999999999999992006, -8.660254037844389075, -197.2500000000000000 ) ) ;
#30809 = CARTESIAN_POINT ( 'NONE',  ( 10.81189881249999907, 6.242252689847868297, -109.2187500020483810 ) ) ;
#30810 = CARTESIAN_POINT ( 'NONE',  ( -10.00000000000038547, 5.773502691896036154, -155.8749999999999432 ) ) ;
#30811 = CARTESIAN_POINT ( 'NONE',  ( -9.999999999999998224, 5.773502691896259087, -74.87499999999997158 ) ) ;
#30812 = CARTESIAN_POINT ( 'NONE',  ( -10.81189881249999729, 6.242252689847871849, -0.9062500020483588159 ) ) ;
#30813 = CARTESIAN_POINT ( 'NONE',  ( -4.999999999999996447, 8.660254037844387298, -84.37500000409677625 ) ) ;
#30814 = CYLINDRICAL_SURFACE ( 'NONE', #36864, 9.999999999999998224 ) ;
#30815 = CARTESIAN_POINT ( 'NONE',  ( -5.405949406249996869, 9.363379034771805109, -97.03125000204839523 ) ) ;
#30816 = CARTESIAN_POINT ( 'NONE',  ( -10.81189881249999729, 1.324075727343319199E-15, -74.28125000204838102 ) ) ;
#30817 =( BOUNDED_SURFACE ( )  B_SPLINE_SURFACE ( 1, 2, ( 
 ( #14237, #7155, #10379, #36714, #4557, #14460, #40157, #30259, #20307, #24431, #906, #1111, #698, #4131, #10586, #34138, #27010, #13817, #23775, #33923, #10802, #37362, #20953, #21163, #37135, #7372, #20518, #490, #3716, #7805, #33706, #17272, #14021, #17697, #27214, #40361, #33500, #1328, #3924, #17488, #30891, #23993, #7583, #20736, #26797, #4347, #27650, #30681, #27438, #40575, #40791, #37574, #8019, #16845, #30043, #13603, #17917, #18358, #41654, #8871, #12091, #22033, #15325, #31333, #28733, #2192, #41860, #38217, #27867, #38644, #25072, #41001, #11657, #9078, #14893, #21603, #35205, #5635, #14680, #38007, #25284, #24856, #15530, #15104, #8452, #1764, #12297, #18784, #24645, #31972, #34782, #8662, #4768, #38429, #4996, #37788, #28091, #5203, #5424, #31763, #31547, #1547, #41218, #1980, #34996, #2400, #25494, #34350, #11445, #28301, #41438, #11876, #31114, #8232, #21815, #21382, #34565, #18137, #18576, #28523, #28940, #2817, #42285, #19414, #33017, #25702, #26539, #12707, #15949, #6054, #25905, #19621, #42077, #226, #3028, #39267, #8, #32182, #19205, #26328, #9702, #32393, #22881, #3446, #36040, #29146, #39056, #29563, #36250, #13132, #19833, #6680, #39479, #35834, #15740, #12508, #38852, #22450, #9495, #2610, #9279, #39688, #5841, #3238, #9912, #23088, #16364, #32806, #16583, #26113, #29785, #22662, #6476, #13348, #22245, #18998, #32604, #6268, #29352, #16155, #35416, #35628, #42491, #12918, #17647, #6893, #14187, #20264, #858, #33661, #33241, #33452, #27386, #27170, #13975, #4086, #13768, #30842, #33872, #30632, #23945, #29995, #36458, #36879, #17436, #20686, #3667, #34082, #20046, #20898, #39900, #37307, #40313, #3880, #1279, #4504, #16796, #26748, #13558, #26955, #10331, #17224, #20474, #7323, #441, #10754, #17015, #14407, #27601, #37090, #10124, #23302, #7533, #30427, #4297, #40110, #23520, #1063, #36668, #7110, #40522, #10966, #30213, #650, #24162, #10542, #23728, #7753, #14839, #31494, #14630, #4939, #41604, #31282, #4717, #34517, #8181, #28036, #1712, #37954, #28473, #2139, #5154, #27818, #8610, #34732, #41164, #38164, #12037, #18088, #15479, #11603, #31924, #24590, #21764, #1495, #17866, #31060, #25232, #8817, #24811, #11395, #34300, #5578, #8401, #34942, #37738, #21551, #18305, #38378, #21329, #1926, #15053, #28250, #41386, #5367, #15274, #40742, #11822, #25023, #18520, #37522, #11184, #31709, #21974, #35153, #18731, #2352, #24381, #7965, #40951, #21113, #28892, #42448, #42659, #42237, #2770, #19366, #2563, #35578, #29517, #19155, #35367, #22401, #38805, #15895, #32346, #25857, #16318, #32755, #35789, #15693, #39221, #22615, #29100, #26070, #13083, #6007, #3400, #12662, #19784, #12455, #9658, #32133, #5794, #18947, #26281, #39433, #39012, #42025, #22193, #36197, #9449, #22831, #25648, #6221, #32552, #9866, #9232, #2982, #16106, #29302, #12875, #35994, #3192, #28682, #6428, #19572, #23039, #25441, #41811, #6634, #32971, #12249, #38587, #9027, #16965, #7064, #10076, #14732, #16747, #30953, #31173, #26698, #7860, #40062, #39634, #39849, #34407, #34198, #21009, #10494, #20215, #37847, #40847, #37633, #1385, #36411, #178, #601, #24481, #27709, #23252, #41055, #13300, #27924, #3620, #1602, #4615, #10283, #8289, #11498, #6845, #33189, #19998, #33403, #29949, #23682, #26906, #13716, #26489, #17758, #23470, #24701, #34620, #14515, #16535, #29733, #11286, #37418, #8072, #3829, #390, #21222, #13508, #36617, #4827, #17973, #30160, #21436, #35474, #31599, #25757, #19054, #35048, #34835, #15796, #32236, #24913, #22509, #11716, #28360, #25123, #2256, #28992, #8500, #9341, #38269, #41497, #2032, #8715, #2454, #38059, #38910, #28575, #22087, #25548, #14945, #15161, #9132, #35262, #11931, #5696, #42131, #18846, #21869, #5475, #12350, #2662, #38698, #12563, #5047, #22302, #18625, #41278, #21653, #5258, #18410, #31821, #28145, #15375, #18192, #31384, #28787, #5900, #1819, #41918, #15586, #41705, #8925, #12143, #25336, #32026, #38481, #26593, #19258, #32865, #6528, #65, #29622, #35683, #19892, #19470, #33298, #499, #32449, #39743, #10178, #13401, #23363, #16640, #32655, #30054, #3502, #13614, #39535, #29200, #39957, #26383, #42340, #12976, #10388, #16211, #22940, #36515, #6952, #16005, #39319, #20108, #26173, #16853, #16424, #9759, #3083, #26806, #3723, #25964, #6111, #36093, #9965, #2875, #12771, #6325, #39113, #29412, #19679, #6738, #33075, #3297, #9549, #42552, #13190, #36307, #22723, #35888, #23144, #29842, #280, #20526, #20744, #1555, #40799, #40584, #27448, #4355, #27225, #14687, #4565, #1337, #37370, #706, #7163, #7591, #30902, #34147, #17070, #4777, #20315, #34361, #10597, #8027, #11025, #17280, #27876, #17925, #3932, #40165, #27018, #40369, #23783, #30689, #33932, #17496, #33509, #14245, #30485, #31122, #41008, #7813, #23577, #36724, #24219, #1122, #20961, #10810, #30267, #17707, #13825, #36938, #14468, #27658, #7380, #33714, #11240, #4139, #914, #37143, #24003, #24439, #14029, #37582, #21171, #1986, #18144, #5209, #21609, #28307, #15112, #8667, #41865, #15537, #18581, #28099, #22040, #5430, #41446, #8877, #12303, #18365, #28946, #31553, #2616, #38013, #35212, #14900, #31340, #1770, #25500, #22252, #11882, #24865, #5003, #19004, #38223, #5642, #8458, #25078, #21821, #38649, #34788, #35001, #31769, #41660, #2197, #18791, #28739, #11453, #15331, #28528, #12096, #8241, #24653, #2406, #25289, #38434, #31980, #9084, #35422, #5849, #41227, #32189, #11664, #15747, #37796, #21389, #34572, #22887, #22457, #22670, #16588, #16801, #32813, #12714, #39063, #38858, #42083, #33023, #32610, #3035, #42497, #6687, #12925, #16162, #35634, #39693, #42292, #13138, #13353, #9501, #3244, #36046, #6061, #35841, #29790, #16370, #29570, #6482, #29358, #20052, #23094, #19838, #26333, #19211, #25708, #26120, #3452, #9918, #32400, #23308, #9285, #10129, #29153, #26544, #15, #6273, #33246, #36463, #2823, #15956, #25911, #39274, #19419, #19629, #9708, #39485, #36257, #231, #6899, #3673, #12515, #1069, #30000, #4723, #33880, #13979, #27176, #33666, #39906, #17441, #446, #13563, #37095, #7538, #7115, #10337, #17653, #13775, #7970, #863, #4090, #20692, #3884, #36884, #30848, #20479, #36674, #23733, #40115, #17232, #30433, #40319, #1285, #34087, #4302, #17019, #40529, #23951, #10760, #27392, #14414, #7330, #26754, #30637, #21119, #26959, #10972, #33457, #20269, #30218, #27608, #40748, #14193, #657, #23525, #37529, #24168, #37315, #10548, #7761, #20905, #11190, #4510, #24388, #34308, #5375, #25029, #25240, #38172, #8616, #37744, #40958, #5586, #1718, #38594, #31502, #34738, #21772, #34524, #24817, #18739, #8407, #24595, #11609, #28043, #5160, #21558, #15059, #31931, #21982, #34950, #4947, #28479, #11829, #18312, #15281, #2358, #37962, #35373, #1932, #9034, #14847, #41610, #21335, #8188, #18094, #15485, #28690, #28257, #31289, #11401, #25448, #41394, #12044, #41170, #18526, #31715, #41817, #2146, #38384, #8825, #35160, #12255, #22199, #17872, #31068, #1502, #14636, #27824, #2570, #5800, #39440, #39020, #9456, #6228, #13090, #19374, #22622, #42032, #3407, #6014, #19579, #19791, #15904, #39228, #29310, #28898, #29108, #23047, #22839, #9666, #42455, #35797, #26498, #29524, #26290, #32763, #25655, #32140, #32561, #9874, #16325, #12462, #29741, #15699, #16542, #35586, #32978, #36002, #42244, #39643, #188, #38811, #22408, #9239, #2989, #19164, #12882, #16114, #26077, #32353, #6436, #12669, #13308, #23259, #3199, #18952, #2778, #42666, #36205, #6641, #10083, #25865, #23908, #36419, #11139, #1024, #24121, #17396, #33830, #14145, #40274, #37260, #16973, #10713, #4254, #27345, #20006, #33619, #7281, #815, #30383, #6853, #20643, #20222, #34043, #1240, #33198, #40480, #10927, #7710, #20859, #30594, #33412, #30802, #4464, #14364, #37053, #29957, #40696, #27131, #397, #13725, #3629, #30170, #23690, #17606, #27562, #16757, #40072, #13517, #26914, #26705, #17185, #10502, #3838, #39857, #10291, #23478, #36626, #36837, #7490, #7073, #609, #20434, #4040, #13938, #37913, #38122, #21717, #8357, #34262, #34474, #21508, #24981, #8775, #41562, #38332, #17826, #34690, #21288, #5110, #2312, #21931, #11561, #11353, #35110, #5535, #1451, #41770, #31021, #4896, #1667, #18259, #18684, #27775, #28637, #14796, #18044, #8140, #27992, #34900, #14586, #15439, #31448, #41343, #2097, #4678, #31240, #28426, #11779, #41121, #8567, #31882, #5322, #24769, #1882, #31663, #24339, #15227, #37480, #7924, #11995, #15011, #40911, #24547, #37698, #28208, #18476, #25191, #21073, #16488, #38541, #35944, #9404, #25812, #19314, #6174, #12202, #39177, #38762, #9817, #19742, #8982, #16272, #29471, #32712, #42613, #6387, #9188, #6586, #22784, #32922, #16066, #5752, #29687, #2937, #18905, #32301, #25395, #35535, #42192, #13040, #26235, #35324, #15855, #3145, #2722, #36153, #35746, #29053, #22359, #3356, #39384, #2520, #22998, #12619, #29259, #22149, #32086, #25604, #15646, #5964, #38968, #26024, #9610, #22567, #28846, #19115, #32508, #12834, #41981, #12411, #42402, #19528, #40019, #39804, #10449, #20804, #14091, #30116, #29901, #10871, #27292, #19954, #17552, #6800, #23423, #20171, #23641, #24064, #3570, #4413, #33360, #36572, #26654, #3780, #40224, #33142, #33992, #36787, #17131, #20588, #10026, #10236, #4198, #30332, #7018, #762, #37206, #13885, #16914, #553, #7435, #40428, #33776, #7653, #130, #17342, #13673, #36365, #16704, #339, #13461, #26865, #23207, #7224, #13253, #26440, #23851, #30545, #973, #37000, #10658, #39592, #3988, #20375, #33564, #27081, #41291, #21666, #14308, #14529, #8086, #28157, #7873, #8729, #11512, #5060, #8513, #40642, #27723, #34848, #18207, #40859, #31397, #11945, #1831, #11299, #24493, #38073, #2046, #5271, #28373, #15176, #18423, #1616, #24285, #37430, #21020, #30969, #34422, #11084, #4627, #35061, #27508, #11730, #31613, #41513, #24929, #25136, #38282, #34633, #21883, #37646, #14959, #5489, #30753, #34211, #27938, #14745, #37860, #24714, #1186, #17773, #21236, #1399, #4841, #17986, #31186, #41067, #8305, #21450, #247, #15600, #13578, #29807, #26769, #23111, #12156, #23541, #9932, #25349, #38715, #36690, #41934, #6496, #20068, #6915, #41719, #22316, #39708, #9148, #462, #31, #35489, #28802, #39922, #33263, #8939, #3689, #19645, #36273, #31833, #10145, #32042, #22103, #12365, #32829, #33041, #16604, #3260, #28588, #25563, #16388, #19856, #16817, #36480, #30016, #38495, #29588, #13154, #26348, #10352, #18639, #39501, #5710, #2269, #15391, #35277, #18861, #2471, #6704, #3469, #13369, #26561, #23325, #11414, #40335, #878, #37543, #11204, #14209, #23748, #17668, #1083, #10777, #4525, #7983, #13995, #24608, #27191, #40971, #33679, #30862, #10562, #13791, #26974, #21134, #17885, #23966, #20494, #673, #14650, #33895, #1298, #4106, #7554, #37110, #34322, #30447, #17247, #20707, #37330, #27408, #14429, #24402, #7130, #40544, #4317, #17456, #3899, #20284, #40762, #30653, #10988, #24183, #27622, #7777, #20920, #40133, #4739, #7345, #34102, #31083, #1516, #27839, #33473, #30233, #17034, #36901, #12057, #41623, #18539, #41408, #15711, #18753, #15497, #8840, #14860, #21350, #21785, #2371, #5599, #31302, #18965, #34536, #5812, #24830, #22212, #25253, #31515, #28910, #32152, #18107, #11623, #41183, #11842, #37976, #2160, #5388, #34965, #4960, #28491, #1945, #2582, #12473, #21996, #37757, #8201, #38398, #31730, #15294, #25043, #1734, #35174, #28057, #8420, #31943, #28703, #21571, #34752, #25463, #5172, #42047, #8629, #38185, #41830, #18326, #15070, #38608, #28272, #12267, #9047, #35388, #42466, #29322, #22850, #29119, #32365, #2789, #26508, #36429, #19384, #39031, #19176, #33209, #9677, #23060, #22635, #26088, #32574, #13319, #6240, #35808, #3000, #13103, #32774, #32990, #198, #407, #16337, #9466, #16125, #22420, #25668, #16555, #12894, #39239, #36012, #3418, #6449, #19591, #15918, #23270, #25877, #39451, #39655, #3210, #29535, #42677, #6026, #26302, #10092, #9886, #36216, #6652, #19802, #3640, #29753, #6865, #20016, #42255, #9251, #16767, #29967, #38822, #12680, #35598, #10301, #24349, #618, #40707, #30604, #7291, #4687, #37490, #36636, #30180, #16982, #30393, #13734, #20652, #23917, #40283, #39867, #4265, #20443, #7934, #31031, #27356, #13528, #26715, #17406, #10724, #37061, #17194, #23488, #1033, #7082, #20232, #33839, #14156, #33421, #3847, #1251, #40081, #34272, #27140, #826, #40491, #26923, #33628, #14375, #4050, #10512, #13947, #23699, #7500, #10937, #24130, #27572, #17617, #37272, #36848, #7721, #20869, #34053, #4475, #11150, #30812, #21084, #17836, #35336, #28002, #12007, #22161, #25202, #21942, #15240, #21298, #27786 ),
 ( #15021, #18269, #34910, #18055, #8369, #2322, #34700, #8150, #37923, #11572, #31458, #5120, #41353, #31894, #5546, #8577, #31250, #38343, #38134, #1892, #41574, #15451, #21519, #18916, #28220, #5763, #41132, #8785, #4908, #34486, #1678, #28649, #12213, #11790, #14806, #37708, #8993, #24992, #35122, #24778, #21727, #5332, #41779, #18487, #31675, #2109, #28438, #18698, #25406, #38552, #1463, #14596, #40920, #11363, #24558, #32099, #23010, #22580, #35758, #32520, #39396, #2949, #6186, #25616, #29698, #32312, #3156, #3367, #42204, #22795, #12845, #12422, #12630, #6597, #6398, #35957, #26037, #19325, #25824, #38979, #16077, #29270, #42414, #19753, #36164, #39189, #5976, #42623, #9623, #19539, #29483, #32935, #9415, #6812, #32723, #23219, #15865, #13053, #35546, #38774, #9200, #16500, #144, #16285, #2735, #22369, #39603, #26247, #9828, #29066, #13265, #26451, #10037, #36377, #2532, #15657, #28857, #41993, #19127, #37216, #37440, #10669, #33372, #16926, #16717, #19967, #10883, #10460, #23651, #20385, #27303, #33576, #36797, #13473, #17563, #20182, #33787, #34002, #30127, #23863, #772, #351, #564, #7663, #37011, #7447, #13898, #7235, #40651, #984, #40439, #4210, #39815, #3583, #3999, #24075, #30557, #26665, #1196, #29912, #30763, #7030, #4423, #20600, #13684, #17142, #20816, #40030, #14320, #27091, #30343, #26875, #27519, #11093, #10247, #24296, #40234, #17353, #33153, #23435, #3792, #36583, #14101, #11521, #28166, #41301, #24723, #17783, #21246, #41076, #1842, #2056, #5280, #15186, #30980, #37869, #8095, #8314, #38292, #31622, #27949, #11310, #28383, #41524, #1409, #14539, #18433, #37655, #8738, #21459, #14754, #18217, #40869, #17995, #11954, #31195, #27733, #4852, #34432, #34643, #5069, #31407, #25145, #34858, #14968, #24503, #11739, #24938, #1625, #38081, #21892, #8522, #7883, #21675, #21031, #34221, #4637, #17594, #41108, #37469, #21497, #40900, #7695, #37247, #4885, #11548, #18032, #37903, #24756, #31229, #11123, #33819, #4241, #17384, #40468, #1227, #7480, #14133, #1874, #23895, #21278, #1654, #27980, #34463, #37685, #14784, #1439, #8347, #20848, #14573, #8125, #34679, #37042, #7913, #24328, #4664, #34251, #40263, #24536, #24109, #5101, #18247, #20629, #31438, #15000, #10700, #30583, #1013, #34032, #27334, #10916, #4452, #27762, #30793, #14354, #31010, #27551, #40685, #21060, #17815, #11342, #5525, #18675, #38323, #31872, #5955, #2304, #9392, #8973, #15429, #25181, #22557, #29043, #18465, #15843, #28627, #32076, #41332, #19105, #41554, #31653, #8764, #41758, #41969, #25595, #12193, #38113, #21920, #25384, #28837, #12608, #2711, #42181, #34889, #38531, #2925, #35100, #2087, #22139, #35313, #5743, #18896, #32287, #2511, #35734, #15635, #12402, #38750, #6163, #25802, #15217, #38959, #9179, #22350, #11770, #19303, #11986, #28416, #35526, #32497, #28199, #24971, #8557, #21707, #5314, #29675, #16692, #542, #33348, #30103, #9598, #13241, #13029, #26428, #36773, #13660, #3344, #3132, #26852, #40006, #35933, #33552, #22772, #39371, #36143, #39579, #10437, #19517, #20363, #6574, #9807, #42603, #19730, #13447, #6373, #7211, #10015, #33130, #36560, #26013, #26223, #23192, #32912, #16902, #36353, #23628, #29888, #22986, #16476, #23411, #16055, #7006, #29246, #42390, #20157, #120, #32701, #16261, #29460, #6786, #19941, #39165, #3557, #12822, #327, #39791, #3768, #26642, #10224, #1384, #11285, #7859, #4826, #27277, #21008, #14514, #37632, #30317, #1171, #17539, #11070, #40628, #3977, #30952, #30534, #1601, #11497, #752, #8071, #21221, #24480, #34406, #27708, #961, #41054, #40846, #24700, #34197, #40212, #8288, #37417, #20791, #7640, #14295, #17972, #31172, #24271, #20573, #14731, #4614, #37191, #27922, #37846, #40415, #21435, #10859, #17117, #14079, #13874, #17757, #33978, #27069, #10644, #23838, #24050, #17331, #36987, #7423, #30741, #33763, #4400, #27494, #4186, #22301, #15160, #31598, #2031, #22086, #41703, #41917, #9131, #9339, #25335, #5257, #28359, #31383, #34619, #25547, #25122, #38267, #35047, #12349, #5474, #8714, #28144, #32235, #34833, #5695, #5898, #41496, #38480, #15374, #14944, #11930, #35473, #8924, #35261, #28574, #21868, #12562, #15585, #38697, #18845, #11715, #18191, #18624, #19053, #2452, #41277, #15795, #1818, #2661, #21652, #2255, #32025, #28786, #31820, #28991, #24912, #8499, #38058, #12142, #18409, #42130, #25756, #38909, #5046, #13189, #16209, #16852, #39955, #36306, #22508, #35682, #26382, #6527, #19677, #26172, #32448, #9964, #6110, #19257, #29621, #64, #42339, #2874, #10177, #6324, #497, #36092, #39318, #39534, #39112, #29411, #23362, #12975, #29199, #42551, #32654, #3296, #9758, #13612, #3501, #279, #6737, #12769, #16004, #32864, #29841, #33074, #25963, #3722, #9548, #33297, #22722, #16423, #19891, #16639, #22939, #30051, #35887, #19469, #3082, #23142, #13400, #26591, #39742, #36514, #6951, #20107, #26804, #4775, #27874, #24217, #10386, #23575, #14243, #37141, #7589, #14027, #20313, #40582, #36722, #7161, #17494, #30687, #30265, #33506, #40797, #36935, #31120, #24001, #27223, #1119, #27016, #17278, #11238, #912, #17068, #4137, #20524, #40367, #10808, #20742, #24437, #14466, #27446, #40163, #20959, #4353, #33930, #7811, #37580, #30483, #3930, #11023, #1553, #7378, #34145, #37368, #4563, #704, #27656, #21169, #17705, #23781, #13823, #17923, #30900, #1335, #33712, #8025, #34359, #14686, #10595, #38011, #8456, #28526, #5428, #5640, #15535, #15745, #31767, #11662, #21607, #37794, #41007, #31978, #31551, #1984, #41444, #18789, #11880, #15110, #34570, #38647, #41225, #12094, #12302, #34786, #2195, #21819, #21387, #5207, #28737, #15329, #41658, #18142, #24651, #25076, #2404, #8876, #5001, #22250, #8239, #9082, #28097, #8665, #38432, #35210, #28305, #35420, #31338, #14898, #1769, #38221, #24863, #18579, #34999, #25287, #18362, #22038, #41863, #5847, #11451, #25498, #19002, #32187, #2614, #12923, #26118, #32608, #38857, #16368, #28944, #3671, #36044, #6480, #6059, #9283, #16586, #12712, #6897, #42495, #3033, #19627, #2821, #35839, #29788, #19417, #35632, #22668, #39061, #16160, #29356, #39272, #229, #33021, #32811, #15954, #39483, #22885, #9707, #26332, #13351, #6271, #42081, #3242, #20050, #25909, #9916, #29568, #13, #12513, #3450, #39691, #13136, #42290, #22455, #36461, #23092, #36255, #9499, #6685, #19836, #26542, #10128, #23306, #33244, #25706, #19209, #32398, #29151, #34305, #7536, #30216, #13773, #13561, #16799, #7758, #7328, #20477, #17230, #24165, #30431, #33664, #10335, #14411, #17018, #30635, #30845, #26958, #20690, #40317, #39904, #40113, #34085, #33878, #4300, #10758, #4089, #37526, #40526, #37312, #1067, #17650, #10546, #29998, #23731, #7967, #655, #27389, #17439, #861, #444, #4507, #27605, #36882, #13977, #23523, #24385, #27174, #14190, #23949, #37093, #10969, #1282, #20902, #40745, #11187, #21116, #26752, #36672, #7113, #20267, #33455, #3883, #1715, #1499, #4720, #38382, #37959, #8404, #5157, #12042, #18309, #21555, #40955, #2357, #4944, #18524, #18737, #14844, #38169, #28254, #27821, #28040, #21980, #21769, #8613, #41391, #34735, #25447, #28477, #25238, #31713, #24592, #31065, #31499, #8823, #15279, #11398, #28689, #14633, #15484, #34521, #15056, #2144, #41608, #1929, #41816, #37741, #21332, #8185, #11826, #18091, #25026, #34947, #5372, #31286, #35158, #41167, #12254, #22198, #5584, #17869, #11606, #31929, #38593, #9033, #24814, #2569, #22838, #35372, #10082, #42454, #12881, #12461, #15698, #23046, #19163, #13307, #6227, #9455, #26076, #9238, #42243, #36203, #25863, #42031, #29107, #2777, #22621, #39019, #32560, #6640, #39439, #39227, #22407, #3198, #29308, #35796, #32761, #16541, #16113, #19373, #32352, #29740, #19790, #25654, #32977, #2988, #9665, #5799, #13089, #6013, #38810, #15903, #36001, #6435, #16324, #19578, #28897, #12668, #29523, #42665, #3406, #9873, #187, #35585, #26289, #26497, #39642, #18951, #32139, #10501, #10290, #34042, #37258, #396, #40695, #29956, #3836, #608, #20433, #4463, #26704, #27561, #13724, #16972, #7072, #26913, #20641, #13516, #1239, #4038, #40273, #1023, #33197, #20221, #17184, #40071, #24120, #33618, #17605, #23907, #33411, #30169, #30593, #7709, #14143, #20858, #30801, #27344, #36836, #16756, #39856, #23477, #36625, #23689, #3628, #7279, #23258, #6852, #4253, #40479, #10926, #17395, #33829, #14363, #27130, #36418, #30382, #10711, #20005, #814, #13937, #37052, #7489, #18257, #5109, #11137, #38708, #37697, #9349, #19265, #7923, #15804, #29000, #32244, #42141, #35483, #8139, #6120, #22310, #32458, #15594, #4677, #16014, #2464, #17825, #31239, #29210, #34473, #14585, #1665, #14795, #21287, #27990, #2671, #41120, #28796, #4895, #2884, #24338, #25557, #37479, #21071, #41927, #37912, #8356, #11560, #34261, #12359, #31020, #1450, #31447, #9142, #27773, #40910, #12572, #18043, #11352, #24768, #21507, #5910, #24545, #34689, #25765, #19063, #38918, #22518, #35691, #16433, #3305, #39543, #30066, #3733, #6748, #16221, #10188, #36316, #32874, #39753, #508, #36103, #17080, #6537, #33519, #26182, #23373, #3513, #29632, #42349, #16863, #10398, #19690, #12985, #35898, #7173, #26392, #36523, #39329, #75, #13199, #13624, #22949, #9769, #9974, #29851, #19901, #6963, #26816, #12781, #33085, #23154, #16650, #39124, #25973, #33308, #289, #13410, #26603, #20120, #39968, #23588, #6335, #36735, #42561, #20325, #3942, #9558, #22732, #19478, #32664, #3094, #29421, #4576, #34158, #11037, #33945, #8253, #11251, #8038, #1349, #7391, #13837, #14256, #37594, #40811, #23794, #11464, #27031, #41020, #17294, #40595, #27673, #24449, #4367, #24665, #10607, #4150, #33727, #17506, #30498, #37382, #24231, #27459, #40175, #36949, #20972, #24014, #37807, #5015, #14478, #30279, #718, #17718, #7825, #30913, #30701, #20538, #21182, #924, #14040, #34372, #4788, #27236, #40379, #17936, #10821, #21400, #1133, #31135, #1568, #37155, #7602, #14698, #20756, #27887, #34585, #28318, #35013, #21833, #15342, #5861, #22264, #25301, #34800, #28751, #12106, #8679, #15549, #19015, #11894, #35645, #25089, #9298, #1998, #41878, #22051, #5442, #18156, #35433, #28957, #38234, #31565, #11676, #25720, #2210, #12314, #15123, #18594, #31780, #32200, #41459, #28539, #41671, #5655, #38445, #25512, #2627, #31351, #8888, #35224, #18803, #14911, #1781, #9097, #31991, #2417, #38660, #15759, #42094, #12527, #24876, #38869, #18376, #22468, #28111, #41238, #38026, #8470, #21621, #5220, #23321, #23107, #9928, #29584, #9719, #26765, #29803, #26557, #19852, #25923, #32412, #32825, #13365, #16600, #42304, #30012, #2834, #16813, #35852, #16383, #3465, #243, #22902, #458, #29164, #22684, #9514, #36058, #6286, #13150, #27, #3256, #19222, #39705, #19431, #32621, #3046, #19641, #33036, #10141, #26345, #15968, #16174, #39497, #6700, #33259, #36476, #20064, #12726, #36269, #29369, #6910, #39918, #3685, #6493, #42510, #13574, #10348, #39075, #23536, #12937, #26133, #39286, #6075, #4735, #40128, #40967, #27187, #30443, #20490, #13990, #34099, #13787, #14646, #17452, #10984, #14425, #3895, #33676, #30648, #40331, #37539, #33891, #17882, #37326, #4102, #17243, #1295, #7979, #27618, #34318, #21129, #40758, #7550, #30229, #669, #26970, #36897, #10773, #17030, #10558, #11410, #20281, #17664, #11200, #24398, #30858, #4520, #31079, #40540, #1512, #874, #24179, #27835, #36686, #33469, #4313, #20703, #1079, #14205, #7126, #20916, #23962, #23744, #7341, #37106, #27404, #7773, #2367, #41826, #5595, #21567, #18961, #35170, #32148, #28487, #18103, #28906, #15290, #31298, #1941, #42043, #5168, #28053, #15067, #28267, #34748, #41404, #15494, #11838, #5808, #5384, #25039, #18322, #2578, #25459, #14856, #12263, #38181, #41619, #1730, #31511, #8625, #21781, #34961, #18535, #38604, #28699, #31726, #41179, #18748, #2155, #12053, #21992, #9043, #25249, #24604, #38394, #15707, #8416, #31940, #8836, #22208, #37753, #35383, #8197, #21346, #37972, #11618, #34532, #4956, #24826, #9463, #12890, #19380, #194, #35804, #22631, #6236, #42673, #19587, #19798, #29749, #29963, #3206, #25872, #32570, #9246, #12470, #3414, #2996, #16121, #26084, #32985, #39235, #29318, #6022, #10089, #12676, #26298, #26504, #42462, #16332, #36008, #35594, #9673, #13315, #29531, #13099, #6445, #22846, #33205, #36212, #16551, #39447, #32361, #38819, #32770, #39651, #23056, #19172, #36425, #22416, #23266, #42251, #9882, #6648, #6860, #20012, #3636, #2785, #29115, #15914, #16763, #39027, #25664, #10719, #27135, #26711, #33835, #36843, #37486, #17832, #14151, #403, #13525, #4260, #40278, #23912, #4045, #10297, #30599, #39863, #23484, #7495, #20648 ) ),
 .UNSPECIFIED., .F., .F., .F. ) 
 B_SPLINE_SURFACE_WITH_KNOTS ( ( 2, 2 ),
 ( 3, 2, 2, 2, 2, 2, 2, 2, 2, 2, 2, 2, 2, 2, 2, 2, 2, 2, 2, 2, 2, 2, 2, 2, 2, 2, 2, 2, 2, 2, 2, 2, 2, 2, 2, 2, 2, 2, 2, 2, 2, 2, 2, 2, 2, 2, 2, 2, 2, 2, 2, 2, 2, 2, 2, 2, 2, 2, 2, 2, 2, 2, 2, 2, 2, 2, 2, 2, 2, 2, 2, 2, 2, 2, 2, 2, 2, 2, 2, 2, 2, 2, 2, 2, 2, 2, 2, 2, 2, 2, 2, 2, 2, 2, 2, 2, 2, 2, 2, 2, 2, 2, 2, 2, 2, 2, 2, 2, 2, 2, 2, 2, 2, 2, 2, 2, 2, 2, 2, 2, 2, 2, 2, 2, 2, 2, 2, 2, 2, 2, 2, 2, 2, 2, 2, 2, 2, 2, 2, 2, 2, 2, 2, 2, 2, 2, 2, 2, 2, 2, 2, 2, 2, 2, 2, 2, 2, 2, 2, 2, 2, 2, 2, 2, 2, 2, 2, 2, 2, 2, 2, 2, 2, 2, 2, 2, 2, 2, 2, 2, 2, 2, 2, 2, 2, 2, 2, 2, 2, 2, 2, 2, 2, 2, 2, 2, 2, 2, 2, 2, 2, 2, 2, 2, 2, 2, 2, 2, 2, 2, 2, 2, 2, 2, 2, 2, 2, 2, 2, 2, 2, 2, 2, 2, 2, 2, 2, 2, 2, 2, 2, 2, 2, 2, 2, 2, 2, 2, 2, 2, 2, 2, 2, 2, 2, 2, 2, 2, 2, 2, 2, 2, 2, 2, 2, 2, 2, 2, 2, 2, 2, 2, 2, 2, 2, 2, 2, 2, 2, 2, 2, 2, 2, 2, 2, 2, 2, 2, 2, 2, 2, 2, 2, 2, 2, 2, 2, 2, 2, 2, 2, 2, 2, 2, 2, 2, 2, 2, 2, 2, 2, 2, 2, 2, 2, 2, 2, 2, 2, 2, 2, 2, 2, 2, 2, 2, 2, 2, 2, 2, 2, 2, 2, 2, 2, 2, 2, 2, 2, 2, 2, 2, 2, 2, 2, 2, 2, 2, 2, 2, 2, 2, 2, 2, 2, 2, 2, 2, 2, 2, 2, 2, 2, 2, 2, 2, 2, 2, 2, 2, 2, 2, 2, 2, 2, 2, 2, 2, 2, 2, 2, 2, 2, 2, 2, 2, 2, 2, 2, 2, 2, 2, 2, 2, 2, 2, 2, 2, 2, 2, 2, 2, 2, 2, 2, 2, 2, 2, 2, 2, 2, 2, 2, 2, 2, 2, 2, 2, 2, 2, 2, 2, 2, 2, 2, 2, 2, 2, 2, 2, 2, 2, 2, 2, 2, 2, 2, 2, 2, 2, 2, 2, 2, 2, 2, 2, 2, 2, 2, 2, 2, 2, 2, 2, 2, 2, 2, 2, 2, 2, 2, 2, 2, 2, 2, 2, 2, 2, 2, 2, 2, 2, 2, 2, 2, 2, 2, 2, 2, 2, 2, 2, 2, 2, 2, 2, 2, 2, 2, 2, 2, 2, 2, 2, 2, 2, 2, 2, 2, 2, 2, 2, 2, 2, 2, 2, 2, 2, 2, 2, 2, 2, 2, 2, 2, 2, 2, 2, 2, 2, 2, 2, 2, 2, 2, 2, 2, 2, 2, 2, 2, 2, 2, 2, 2, 2, 2, 2, 2, 2, 2, 2, 2, 2, 2, 2, 2, 2, 2, 2, 2, 2, 2, 2, 2, 2, 2, 2, 2, 2, 2, 2, 2, 2, 2, 2, 2, 2, 2, 2, 2, 2, 2, 2, 2, 2, 2, 2, 2, 2, 2, 2, 2, 2, 2, 2, 2, 2, 2, 2, 2, 2, 2, 2, 2, 2, 2, 2, 2, 2, 2, 2, 2, 2, 2, 2, 2, 2, 2, 2, 2, 2, 2, 2, 2, 2, 2, 2, 2, 2, 2, 2, 2, 2, 2, 2, 2, 2, 2, 2, 2, 2, 2, 2, 2, 2, 2, 2, 2, 2, 2, 2, 2, 2, 2, 2, 2, 2, 2, 2, 2, 2, 2, 2, 2, 2, 2, 2, 2, 2, 2, 2, 2, 2, 2, 2, 2, 2, 2, 2, 2, 2, 2, 2, 2, 2, 2, 2, 2, 2, 2, 2, 2, 2, 2, 2, 2, 2, 2, 2, 2, 2, 2, 2, 2, 2, 2, 2, 2, 2, 2, 2, 2, 2, 2, 2, 2, 2, 2, 2, 2, 2, 2, 2, 2, 2, 2, 2, 2, 2, 2, 2, 2, 2, 2, 2, 2, 2, 2, 2, 2, 2, 2, 2, 2, 2, 2, 2, 2, 2, 2, 2, 2, 2, 2, 2, 2, 2, 2, 2, 2, 2, 2, 2, 2, 2, 2, 2, 2, 2, 2, 2, 2, 2, 2, 2, 2, 2, 2, 2, 2, 2, 2, 2, 2, 2, 2, 2, 2, 2, 2, 2, 2, 2, 2, 2, 2, 2, 2, 2, 2, 2, 2, 2, 2, 2, 2, 2, 2, 2, 2, 2, 2, 2, 2, 2, 2, 2, 2, 2, 3 ),
 ( 0.000000000000000000, 1.000000000000000000 ),
 ( 0.000000000000000000, 0.001243781094527363160, 0.002487562189054726321, 0.003731343283582089481, 0.004975124378109452641, 0.006218905472636816235, 0.007462686567164178962, 0.008706467661691542556, 0.009950248756218905283, 0.01119402985074626801, 0.01243781094527363247, 0.01368159203980099520, 0.01492537313432835792, 0.01616915422885572065, 0.01741293532338308511, 0.01865671641791044610, 0.01990049751243781057, 0.02114427860696517503, 0.02238805970149253602, 0.02363184079601990048, 0.02487562189054726494, 0.02611940298507462593, 0.02736318407960199039, 0.02860696517412935486, 0.02985074626865671585, 0.03109452736318408031, 0.03233830845771144130, 0.03358208955223880576, 0.03482587064676617022, 0.03606965174129353469, 0.03731343283582089221, 0.03855721393034825667, 0.03980099502487562113, 0.04104477611940298559, 0.04228855721393035005, 0.04353233830845771452, 0.04477611940298507204, 0.04601990049751243650, 0.04726368159203980096, 0.04850746268656716542, 0.04975124378109452988, 0.05099502487562188741, 0.05223880597014925187, 0.05348258706467661633, 0.05472636815920398079, 0.05597014925373134525, 0.05721393034825870971, 0.05845771144278606724, 0.05970149253731343170, 0.06094527363184079616, 0.06218905472636816062, 0.06343283582089552508, 0.06467661691542288260, 0.06592039800995025400, 0.06716417910447761153, 0.06840796019900496905, 0.06965174129353234045, 0.07089552238805969797, 0.07213930348258706937, 0.07338308457711442689, 0.07462686567164178442, 0.07587064676616915582, 0.07711442786069651334, 0.07835820895522388474, 0.07960199004975124226, 0.08084577114427861366, 0.08208955223880597118, 0.08333333333333332871, 0.08457711442786070011, 0.08582089552238805763, 0.08706467661691542903, 0.08830845771144278655, 0.08955223880597014408, 0.09079601990049751548, 0.09203980099502487300, 0.09328358208955224440, 0.09452736318407960192, 0.09577114427860695944, 0.09701492537313433084, 0.09825870646766168837, 0.09950248756218905977, 0.1007462686567164173, 0.1019900497512437748, 0.1032338308457711462, 0.1044776119402985037, 0.1057213930348258751, 0.1069651741293532327, 0.1082089552238805902, 0.1094527363184079616, 0.1106965174129353191, 0.1119402985074626905, 0.1131840796019900480, 0.1144278606965174194, 0.1156716417910447769, 0.1169154228855721345, 0.1181592039800995059, 0.1194029850746268634, 0.1206467661691542348, 0.1218905472636815923, 0.1231343283582089498, 0.1243781094527363212, 0.1256218905472636926, 0.1268656716417910502, 0.1281094527363184077, 0.1293532338308457652, 0.1305970149253731227, 0.1318407960199005080, 0.1330845771144278655, 0.1343283582089552231, 0.1355721393034825806, 0.1368159203980099381, 0.1380597014925373234, 0.1393034825870646809, 0.1405472636815920384, 0.1417910447761193959, 0.1430348258706467535, 0.1442786069651741387, 0.1455223880597014963, 0.1467661691542288538, 0.1480099502487562113, 0.1492537313432835688, 0.1504975124378109541, 0.1517412935323383116, 0.1529850746268656692, 0.1542288557213930267, 0.1554726368159203842, 0.1567164179104477695, 0.1579601990049751270, 0.1592039800995024845, 0.1604477611940298420, 0.1616915422885572273, 0.1629353233830845848, 0.1641791044776119424, 0.1654228855721392999, 0.1666666666666666574, 0.1679104477611940427, 0.1691542288557214002, 0.1703980099502487577, 0.1716417910447761153, 0.1728855721393034728, 0.1741293532338308581, 0.1753731343283582156, 0.1766169154228855731, 0.1778606965174129306, 0.1791044776119402882, 0.1803482587064676734, 0.1815920398009950310, 0.1828358208955223885, 0.1840796019900497460, 0.1853233830845771035, 0.1865671641791044888, 0.1878109452736318463, 0.1890547263681592038, 0.1902985074626865614, 0.1915422885572139189, 0.1927860696517413042, 0.1940298507462686617, 0.1952736318407960192, 0.1965174129353233767, 0.1977611940298507343, 0.1990049751243781195, 0.2002487562189054771, 0.2014925373134328346, 0.2027363184079601921, 0.2039800995024875496, 0.2052238805970149349, 0.2064676616915422924, 0.2077114427860696499, 0.2089552238805970075, 0.2101990049751243650, 0.2114427860696517503, 0.2126865671641791078, 0.2139303482587064653, 0.2151741293532338228, 0.2164179104477611804, 0.2176616915422885656, 0.2189054726368159232, 0.2201492537313432807, 0.2213930348258706382, 0.2226368159203980235, 0.2238805970149253810, 0.2251243781094527385, 0.2263681592039800961, 0.2276119402985074536, 0.2288557213930348389, 0.2300995024875621964, 0.2313432835820895539, 0.2325870646766169114, 0.2338308457711442689, 0.2350746268656716542, 0.2363184079601990117, 0.2375621890547263693, 0.2388059701492537268, 0.2400497512437810843, 0.2412935323383084696, 0.2425373134328358271, 0.2437810945273631846, 0.2450248756218905422, 0.2462686567164178997, 0.2475124378109452850, 0.2487562189054726425, 0.2500000000000000000, 0.2512437810945273853, 0.2524875621890547150, 0.2537313432835821003, 0.2549751243781094301, 0.2562189054726368154, 0.2574626865671642006, 0.2587064676616915304, 0.2599502487562189157, 0.2611940298507462455, 0.2624378109452736307, 0.2636815920398010160, 0.2649253731343283458, 0.2661691542288557311, 0.2674129353233830608, 0.2686567164179104461, 0.2699004975124378314, 0.2711442786069651611, 0.2723880597014925464, 0.2736318407960198762, 0.2748756218905472615, 0.2761194029850746468, 0.2773631840796019765, 0.2786069651741293618, 0.2798507462686566916, 0.2810945273631840768, 0.2823383084577114621, 0.2835820895522387919, 0.2848258706467661772, 0.2860696517412935069, 0.2873134328358208922, 0.2885572139303482775, 0.2898009950248756073, 0.2910447761194029925, 0.2922885572139303223, 0.2935323383084577076, 0.2947761194029850929, 0.2960199004975124226, 0.2972636815920398079, 0.2985074626865671377, 0.2997512437810945229, 0.3009950248756219082, 0.3022388059701492380, 0.3034825870646766233, 0.3047263681592039530, 0.3059701492537313383, 0.3072139303482587236, 0.3084577114427860534, 0.3097014925373134386, 0.3109452736318407684, 0.3121890547263681537, 0.3134328358208955390, 0.3146766169154228687, 0.3159203980099502540, 0.3171641791044776393, 0.3184079601990049690, 0.3196517412935323543, 0.3208955223880596841, 0.3221393034825870694, 0.3233830845771144546, 0.3246268656716417844, 0.3258706467661691697, 0.3271144278606964995, 0.3283582089552238847, 0.3296019900497512700, 0.3308457711442785998, 0.3320895522388059851, 0.3333333333333333148, 0.3345771144278607001, 0.3358208955223880854, 0.3370646766169154152, 0.3383084577114428004, 0.3395522388059701302, 0.3407960199004975155, 0.3420398009950249008, 0.3432835820895522305, 0.3445273631840796158, 0.3457711442786069456, 0.3470149253731343308, 0.3482587064676617161, 0.3495024875621890459, 0.3507462686567164312, 0.3519900497512437609, 0.3532338308457711462, 0.3544776119402985315, 0.3557213930348258613, 0.3569651741293532465, 0.3582089552238805763, 0.3594527363184079616, 0.3606965174129353469, 0.3619402985074626766, 0.3631840796019900619, 0.3644278606965173917, 0.3656716417910447769, 0.3669154228855721622, 0.3681592039800994920, 0.3694029850746268773, 0.3706467661691542070, 0.3718905472636815923, 0.3731343283582089776, 0.3743781094527363074, 0.3756218905472636926, 0.3768656716417910224, 0.3781094527363184077, 0.3793532338308457930, 0.3805970149253731227, 0.3818407960199005080, 0.3830845771144278378, 0.3843283582089552231, 0.3855721393034826083, 0.3868159203980099381, 0.3880597014925373234, 0.3893034825870646531, 0.3905472636815920384, 0.3917910447761194237, 0.3930348258706467535, 0.3942786069651741387, 0.3955223880597014685, 0.3967661691542288538, 0.3980099502487562391, 0.3992537313432835688, 0.4004975124378109541, 0.4017412935323382839, 0.4029850746268656692, 0.4042288557213930544, 0.4054726368159203842, 0.4067164179104477695, 0.4079601990049750992, 0.4092039800995024845, 0.4104477611940298698, 0.4116915422885571996, 0.4129353233830845848, 0.4141791044776119146, 0.4154228855721392999, 0.4166666666666666852, 0.4179104477611940149, 0.4191542288557214002, 0.4203980099502487300, 0.4216417910447761153, 0.4228855721393035005, 0.4241293532338308303, 0.4253731343283582156, 0.4266169154228855454, 0.4278606965174129306, 0.4291044776119403159, 0.4303482587064676457, 0.4315920398009950310, 0.4328358208955223607, 0.4340796019900497460, 0.4353233830845771313, 0.4365671641791044610, 0.4378109452736318463, 0.4390547263681592316, 0.4402985074626865614, 0.4415422885572139466, 0.4427860696517412764, 0.4440298507462686617, 0.4452736318407960470, 0.4465174129353233767, 0.4477611940298507620, 0.4490049751243780918, 0.4502487562189054771, 0.4514925373134328623, 0.4527363184079601921, 0.4539800995024875774, 0.4552238805970149071, 0.4564676616915422924, 0.4577114427860696777, 0.4589552238805970075, 0.4601990049751243927, 0.4614427860696517225, 0.4626865671641791078, 0.4639303482587064931, 0.4651741293532338228, 0.4664179104477612081, 0.4676616915422885379, 0.4689054726368159232, 0.4701492537313433084, 0.4713930348258706382, 0.4726368159203980235, 0.4738805970149253532, 0.4751243781094527385, 0.4763681592039801238, 0.4776119402985074536, 0.4788557213930348389, 0.4800995024875621686, 0.4813432835820895539, 0.4825870646766169392, 0.4838308457711442689, 0.4850746268656716542, 0.4863184079601989840, 0.4875621890547263693, 0.4888059701492537545, 0.4900497512437810843, 0.4912935323383084696, 0.4925373134328357994, 0.4937810945273631846, 0.4950248756218905699, 0.4962686567164178997, 0.4975124378109452850, 0.4987562189054726147, 0.5000000000000000000, 0.5012437810945273853, 0.5024875621890547706, 0.5037313432835820448, 0.5049751243781094301, 0.5062189054726368154, 0.5074626865671642006, 0.5087064676616915859, 0.5099502487562188602, 0.5111940298507462455, 0.5124378109452736307, 0.5136815920398010160, 0.5149253731343284013, 0.5161691542288556755, 0.5174129353233830608, 0.5186567164179104461, 0.5199004975124378314, 0.5211442786069652167, 0.5223880597014924909, 0.5236318407960198762, 0.5248756218905472615, 0.5261194029850746468, 0.5273631840796020320, 0.5286069651741293063, 0.5298507462686566916, 0.5310945273631840768, 0.5323383084577114621, 0.5335820895522388474, 0.5348258706467661217, 0.5360696517412935069, 0.5373134328358208922, 0.5385572139303482775, 0.5398009950248756628, 0.5410447761194029370, 0.5422885572139303223, 0.5435323383084577076, 0.5447761194029850929, 0.5460199004975124781, 0.5472636815920397524, 0.5485074626865671377, 0.5497512437810945229, 0.5509950248756219082, 0.5522388059701492935, 0.5534825870646765678, 0.5547263681592039530, 0.5559701492537313383, 0.5572139303482587236, 0.5584577114427861089, 0.5597014925373133831, 0.5609452736318407684, 0.5621890547263681537, 0.5634328358208955390, 0.5646766169154229242, 0.5659203980099501985, 0.5671641791044775838, 0.5684079601990049690, 0.5696517412935323543, 0.5708955223880597396, 0.5721393034825870139, 0.5733830845771143991, 0.5746268656716417844, 0.5758706467661691697, 0.5771144278606965550, 0.5783582089552238292, 0.5796019900497512145, 0.5808457711442785998, 0.5820895522388059851, 0.5833333333333333703, 0.5845771144278606446, 0.5858208955223880299, 0.5870646766169154152, 0.5883084577114428004, 0.5895522388059701857, 0.5907960199004974600, 0.5920398009950248452, 0.5932835820895522305, 0.5945273631840796158, 0.5957711442786070011, 0.5970149253731342753, 0.5982587064676616606, 0.5995024875621890459, 0.6007462686567164312, 0.6019900497512438164, 0.6032338308457710907, 0.6044776119402984760, 0.6057213930348258613, 0.6069651741293532465, 0.6082089552238806318, 0.6094527363184079061, 0.6106965174129352913, 0.6119402985074626766, 0.6131840796019900619, 0.6144278606965174472, 0.6156716417910447214, 0.6169154228855721067, 0.6181592039800994920, 0.6194029850746268773, 0.6206467661691542625, 0.6218905472636815368, 0.6231343283582089221, 0.6243781094527363074, 0.6256218905472636926, 0.6268656716417910779, 0.6281094527363184632, 0.6293532338308457375, 0.6305970149253731227, 0.6318407960199005080, 0.6330845771144278933, 0.6343283582089552786, 0.6355721393034825528, 0.6368159203980099381, 0.6380597014925373234, 0.6393034825870647087, 0.6405472636815920939, 0.6417910447761193682, 0.6430348258706467535, 0.6442786069651741387, 0.6455223880597015240, 0.6467661691542289093, 0.6480099502487561836, 0.6492537313432835688, 0.6504975124378109541, 0.6517412935323383394, 0.6529850746268657247, 0.6542288557213929989, 0.6554726368159203842, 0.6567164179104477695, 0.6579601990049751548, 0.6592039800995025400, 0.6604477611940298143, 0.6616915422885571996, 0.6629353233830845848, 0.6641791044776119701, 0.6654228855721393554, 0.6666666666666666297, 0.6679104477611940149, 0.6691542288557214002, 0.6703980099502487855, 0.6716417910447761708, 0.6728855721393034450, 0.6741293532338308303, 0.6753731343283582156, 0.6766169154228856009, 0.6778606965174129861, 0.6791044776119402604, 0.6803482587064676457, 0.6815920398009950310, 0.6828358208955224162, 0.6840796019900498015, 0.6853233830845770758, 0.6865671641791044610, 0.6878109452736318463, 0.6890547263681592316, 0.6902985074626866169, 0.6915422885572138911, 0.6927860696517412764, 0.6940298507462686617, 0.6952736318407960470, 0.6965174129353234322, 0.6977611940298507065, 0.6990049751243780918, 0.7002487562189054771, 0.7014925373134328623, 0.7027363184079602476, 0.7039800995024875219, 0.7052238805970149071, 0.7064676616915422924, 0.7077114427860696777, 0.7089552238805970630, 0.7101990049751243372, 0.7114427860696517225, 0.7126865671641791078, 0.7139303482587064931, 0.7151741293532338783, 0.7164179104477611526, 0.7176616915422885379, 0.7189054726368159232, 0.7201492537313433084, 0.7213930348258706937, 0.7226368159203979680, 0.7238805970149253532, 0.7251243781094527385, 0.7263681592039801238, 0.7276119402985075091, 0.7288557213930347833, 0.7300995024875621686, 0.7313432835820895539, 0.7325870646766169392, 0.7338308457711443245, 0.7350746268656715987, 0.7363184079601989840, 0.7375621890547263693, 0.7388059701492537545, 0.7400497512437811398, 0.7412935323383084141, 0.7425373134328357994, 0.7437810945273631846, 0.7450248756218905699, 0.7462686567164179552, 0.7475124378109452294, 0.7487562189054726147, 0.7500000000000000000, 0.7512437810945273853, 0.7524875621890547706, 0.7537313432835820448, 0.7549751243781094301, 0.7562189054726368154, 0.7574626865671642006, 0.7587064676616915859, 0.7599502487562188602, 0.7611940298507462455, 0.7624378109452736307, 0.7636815920398010160, 0.7649253731343284013, 0.7661691542288556755, 0.7674129353233830608, 0.7686567164179104461, 0.7699004975124378314, 0.7711442786069652167, 0.7723880597014924909, 0.7736318407960198762, 0.7748756218905472615, 0.7761194029850746468, 0.7773631840796020320, 0.7786069651741293063, 0.7798507462686566916, 0.7810945273631840768, 0.7823383084577114621, 0.7835820895522388474, 0.7848258706467661217, 0.7860696517412935069, 0.7873134328358208922, 0.7885572139303482775, 0.7898009950248756628, 0.7910447761194029370, 0.7922885572139303223, 0.7935323383084577076, 0.7947761194029850929, 0.7960199004975124781, 0.7972636815920397524, 0.7985074626865671377, 0.7997512437810945229, 0.8009950248756219082, 0.8022388059701492935, 0.8034825870646765678, 0.8047263681592039530, 0.8059701492537313383, 0.8072139303482587236, 0.8084577114427861089, 0.8097014925373133831, 0.8109452736318407684, 0.8121890547263681537, 0.8134328358208955390, 0.8146766169154229242, 0.8159203980099501985, 0.8171641791044775838, 0.8184079601990049690, 0.8196517412935323543, 0.8208955223880597396, 0.8221393034825870139, 0.8233830845771143991, 0.8246268656716417844, 0.8258706467661691697, 0.8271144278606965550, 0.8283582089552238292, 0.8296019900497512145, 0.8308457711442785998, 0.8320895522388059851, 0.8333333333333333703, 0.8345771144278606446, 0.8358208955223880299, 0.8370646766169154152, 0.8383084577114428004, 0.8395522388059701857, 0.8407960199004974600, 0.8420398009950248452, 0.8432835820895522305, 0.8445273631840796158, 0.8457711442786070011, 0.8470149253731342753, 0.8482587064676616606, 0.8495024875621890459, 0.8507462686567164312, 0.8519900497512438164, 0.8532338308457710907, 0.8544776119402984760, 0.8557213930348258613, 0.8569651741293532465, 0.8582089552238806318, 0.8594527363184079061, 0.8606965174129352913, 0.8619402985074626766, 0.8631840796019900619, 0.8644278606965174472, 0.8656716417910447214, 0.8669154228855721067, 0.8681592039800994920, 0.8694029850746268773, 0.8706467661691542625, 0.8718905472636815368, 0.8731343283582089221, 0.8743781094527363074, 0.8756218905472636926, 0.8768656716417910779, 0.8781094527363184632, 0.8793532338308457375, 0.8805970149253731227, 0.8818407960199005080, 0.8830845771144278933, 0.8843283582089552786, 0.8855721393034825528, 0.8868159203980099381, 0.8880597014925373234, 0.8893034825870647087, 0.8905472636815920939, 0.8917910447761193682, 0.8930348258706467535, 0.8942786069651741387, 0.8955223880597015240, 0.8967661691542289093, 0.8980099502487561836, 0.8992537313432835688, 0.9004975124378109541, 0.9017412935323383394, 0.9029850746268657247, 0.9042288557213929989, 0.9054726368159203842, 0.9067164179104477695, 0.9079601990049751548, 0.9092039800995025400, 0.9104477611940298143, 0.9116915422885571996, 0.9129353233830845848, 0.9141791044776119701, 0.9154228855721393554, 0.9166666666666666297, 0.9179104477611940149, 0.9191542288557214002, 0.9203980099502487855, 0.9216417910447761708, 0.9228855721393034450, 0.9241293532338308303, 0.9253731343283582156, 0.9266169154228856009, 0.9278606965174129861, 0.9291044776119402604, 0.9303482587064676457, 0.9315920398009950310, 0.9328358208955224162, 0.9340796019900498015, 0.9353233830845770758, 0.9365671641791044610, 0.9378109452736318463, 0.9390547263681592316, 0.9402985074626866169, 0.9415422885572138911, 0.9427860696517412764, 0.9440298507462686617, 0.9452736318407960470, 0.9465174129353234322, 0.9477611940298507065, 0.9490049751243780918, 0.9502487562189054771, 0.9514925373134328623, 0.9527363184079602476, 0.9539800995024875219, 0.9552238805970149071, 0.9564676616915422924, 0.9577114427860696777, 0.9589552238805970630, 0.9601990049751243372, 0.9614427860696517225, 0.9626865671641791078, 0.9639303482587064931, 0.9651741293532338783, 0.9664179104477611526, 0.9676616915422885379, 0.9689054726368159232, 0.9701492537313433084, 0.9713930348258706937, 0.9726368159203979680, 0.9738805970149253532, 0.9751243781094527385, 0.9763681592039801238, 0.9776119402985075091, 0.9788557213930347833, 0.9800995024875621686, 0.9813432835820895539, 0.9825870646766169392, 0.9838308457711443245, 0.9850746268656715987, 0.9863184079601989840, 0.9875621890547263693, 0.9888059701492537545, 0.9900497512437811398, 0.9912935323383084141, 0.9925373134328357994, 0.9937810945273631846, 0.9950248756218905699 ),
 .UNSPECIFIED. ) 
 GEOMETRIC_REPRESENTATION_ITEM ( )  RATIONAL_B_SPLINE_SURFACE ( (
 ( 1.000000000000000000, 0.8660254037844387076, 1.000000000000000000, 0.8660254037844387076, 1.000000000000000000, 0.8660254037844387076, 1.000000000000000000, 0.8660254037844387076, 1.000000000000000000, 0.8660254037844387076, 1.000000000000000000, 0.8660254037844387076, 1.000000000000000000, 0.8660254037844387076, 1.000000000000000000, 0.8660254037844387076, 1.000000000000000000, 0.8660254037844387076, 1.000000000000000000, 0.8660254037844387076, 1.000000000000000000, 0.8660254037844387076, 1.000000000000000000, 0.8660254037844387076, 1.000000000000000000, 0.8660254037844387076, 1.000000000000000000, 0.8660254037844387076, 1.000000000000000000, 0.8660254037844387076, 1.000000000000000000, 0.8660254037844387076, 1.000000000000000000, 0.8660254037844387076, 1.000000000000000000, 0.8660254037844387076, 1.000000000000000000, 0.8660254037844387076, 1.000000000000000000, 0.8660254037844387076, 1.000000000000000000, 0.8660254037844387076, 1.000000000000000000, 0.8660254037844387076, 1.000000000000000000, 0.8660254037844387076, 1.000000000000000000, 0.8660254037844387076, 1.000000000000000000, 0.8660254037844387076, 1.000000000000000000, 0.8660254037844387076, 1.000000000000000000, 0.8660254037844387076, 1.000000000000000000, 0.8660254037844387076, 1.000000000000000000, 0.8660254037844387076, 1.000000000000000000, 0.8660254037844387076, 1.000000000000000000, 0.8660254037844387076, 1.000000000000000000, 0.8660254037844387076, 1.000000000000000000, 0.8660254037844387076, 1.000000000000000000, 0.8660254037844387076, 1.000000000000000000, 0.8660254037844387076, 1.000000000000000000, 0.8660254037844387076, 1.000000000000000000, 0.8660254037844387076, 1.000000000000000000, 0.8660254037844387076, 1.000000000000000000, 0.8660254037844387076, 1.000000000000000000, 0.8660254037844387076, 1.000000000000000000, 0.8660254037844387076, 1.000000000000000000, 0.8660254037844387076, 1.000000000000000000, 0.8660254037844387076, 1.000000000000000000, 0.8660254037844387076, 1.000000000000000000, 0.8660254037844387076, 1.000000000000000000, 0.8660254037844387076, 1.000000000000000000, 0.8660254037844387076, 1.000000000000000000, 0.8660254037844387076, 1.000000000000000000, 0.8660254037844387076, 1.000000000000000000, 0.8660254037844387076, 1.000000000000000000, 0.8660254037844387076, 1.000000000000000000, 0.8660254037844387076, 1.000000000000000000, 0.8660254037844387076, 1.000000000000000000, 0.8660254037844387076, 1.000000000000000000, 0.8660254037844387076, 1.000000000000000000, 0.8660254037844387076, 1.000000000000000000, 0.8660254037844387076, 1.000000000000000000, 0.8660254037844387076, 1.000000000000000000, 0.8660254037844387076, 1.000000000000000000, 0.8660254037844387076, 1.000000000000000000, 0.8660254037844387076, 1.000000000000000000, 0.8660254037844387076, 1.000000000000000000, 0.8660254037844387076, 1.000000000000000000, 0.8660254037844387076, 1.000000000000000000, 0.8660254037844387076, 1.000000000000000000, 0.8660254037844387076, 1.000000000000000000, 0.8660254037844387076, 1.000000000000000000, 0.8660254037844387076, 1.000000000000000000, 0.8660254037844387076, 1.000000000000000000, 0.8660254037844387076, 1.000000000000000000, 0.8660254037844387076, 1.000000000000000000, 0.8660254037844387076, 1.000000000000000000, 0.8660254037844387076, 1.000000000000000000, 0.8660254037844387076, 1.000000000000000000, 0.8660254037844387076, 1.000000000000000000, 0.8660254037844387076, 1.000000000000000000, 0.8660254037844387076, 1.000000000000000000, 0.8660254037844387076, 1.000000000000000000, 0.8660254037844387076, 1.000000000000000000, 0.8660254037844387076, 1.000000000000000000, 0.8660254037844387076, 1.000000000000000000, 0.8660254037844387076, 1.000000000000000000, 0.8660254037844387076, 1.000000000000000000, 0.8660254037844387076, 1.000000000000000000, 0.8660254037844387076, 1.000000000000000000, 0.8660254037844387076, 1.000000000000000000, 0.8660254037844387076, 1.000000000000000000, 0.8660254037844387076, 1.000000000000000000, 0.8660254037844387076, 1.000000000000000000, 0.8660254037844387076, 1.000000000000000000, 0.8660254037844387076, 1.000000000000000000, 0.8660254037844387076, 1.000000000000000000, 0.8660254037844387076, 1.000000000000000000, 0.8660254037844387076, 1.000000000000000000, 0.8660254037844387076, 1.000000000000000000, 0.8660254037844387076, 1.000000000000000000, 0.8660254037844387076, 1.000000000000000000, 0.8660254037844387076, 1.000000000000000000, 0.8660254037844387076, 1.000000000000000000, 0.8660254037844387076, 1.000000000000000000, 0.8660254037844387076, 1.000000000000000000, 0.8660254037844387076, 1.000000000000000000, 0.8660254037844387076, 1.000000000000000000, 0.8660254037844387076, 1.000000000000000000, 0.8660254037844387076, 1.000000000000000000, 0.8660254037844387076, 1.000000000000000000, 0.8660254037844387076, 1.000000000000000000, 0.8660254037844387076, 1.000000000000000000, 0.8660254037844387076, 1.000000000000000000, 0.8660254037844387076, 1.000000000000000000, 0.8660254037844387076, 1.000000000000000000, 0.8660254037844387076, 1.000000000000000000, 0.8660254037844387076, 1.000000000000000000, 0.8660254037844387076, 1.000000000000000000, 0.8660254037844387076, 1.000000000000000000, 0.8660254037844387076, 1.000000000000000000, 0.8660254037844387076, 1.000000000000000000, 0.8660254037844387076, 1.000000000000000000, 0.8660254037844387076, 1.000000000000000000, 0.8660254037844387076, 1.000000000000000000, 0.8660254037844387076, 1.000000000000000000, 0.8660254037844387076, 1.000000000000000000, 0.8660254037844387076, 1.000000000000000000, 0.8660254037844387076, 1.000000000000000000, 0.8660254037844387076, 1.000000000000000000, 0.8660254037844387076, 1.000000000000000000, 0.8660254037844387076, 1.000000000000000000, 0.8660254037844387076, 1.000000000000000000, 0.8660254037844387076, 1.000000000000000000, 0.8660254037844387076, 1.000000000000000000, 0.8660254037844387076, 1.000000000000000000, 0.8660254037844387076, 1.000000000000000000, 0.8660254037844387076, 1.000000000000000000, 0.8660254037844387076, 1.000000000000000000, 0.8660254037844387076, 1.000000000000000000, 0.8660254037844387076, 1.000000000000000000, 0.8660254037844387076, 1.000000000000000000, 0.8660254037844387076, 1.000000000000000000, 0.8660254037844387076, 1.000000000000000000, 0.8660254037844387076, 1.000000000000000000, 0.8660254037844387076, 1.000000000000000000, 0.8660254037844387076, 1.000000000000000000, 0.8660254037844387076, 1.000000000000000000, 0.8660254037844387076, 1.000000000000000000, 0.8660254037844387076, 1.000000000000000000, 0.8660254037844387076, 1.000000000000000000, 0.8660254037844387076, 1.000000000000000000, 0.8660254037844387076, 1.000000000000000000, 0.8660254037844387076, 1.000000000000000000, 0.8660254037844387076, 1.000000000000000000, 0.8660254037844387076, 1.000000000000000000, 0.8660254037844387076, 1.000000000000000000, 0.8660254037844387076, 1.000000000000000000, 0.8660254037844387076, 1.000000000000000000, 0.8660254037844387076, 1.000000000000000000, 0.8660254037844387076, 1.000000000000000000, 0.8660254037844387076, 1.000000000000000000, 0.8660254037844387076, 1.000000000000000000, 0.8660254037844387076, 1.000000000000000000, 0.8660254037844387076, 1.000000000000000000, 0.8660254037844387076, 1.000000000000000000, 0.8660254037844387076, 1.000000000000000000, 0.8660254037844387076, 1.000000000000000000, 0.8660254037844387076, 1.000000000000000000, 0.8660254037844387076, 1.000000000000000000, 0.8660254037844387076, 1.000000000000000000, 0.8660254037844387076, 1.000000000000000000, 0.8660254037844387076, 1.000000000000000000, 0.8660254037844387076, 1.000000000000000000, 0.8660254037844387076, 1.000000000000000000, 0.8660254037844387076, 1.000000000000000000, 0.8660254037844387076, 1.000000000000000000, 0.8660254037844387076, 1.000000000000000000, 0.8660254037844387076, 1.000000000000000000, 0.8660254037844387076, 1.000000000000000000, 0.8660254037844387076, 1.000000000000000000, 0.8660254037844387076, 1.000000000000000000, 0.8660254037844387076, 1.000000000000000000, 0.8660254037844387076, 1.000000000000000000, 0.8660254037844387076, 1.000000000000000000, 0.8660254037844387076, 1.000000000000000000, 0.8660254037844387076, 1.000000000000000000, 0.8660254037844387076, 1.000000000000000000, 0.8660254037844387076, 1.000000000000000000, 0.8660254037844387076, 1.000000000000000000, 0.8660254037844387076, 1.000000000000000000, 0.8660254037844387076, 1.000000000000000000, 0.8660254037844387076, 1.000000000000000000, 0.8660254037844387076, 1.000000000000000000, 0.8660254037844387076, 1.000000000000000000, 0.8660254037844387076, 1.000000000000000000, 0.8660254037844387076, 1.000000000000000000, 0.8660254037844387076, 1.000000000000000000, 0.8660254037844387076, 1.000000000000000000, 0.8660254037844387076, 1.000000000000000000, 0.8660254037844387076, 1.000000000000000000, 0.8660254037844387076, 1.000000000000000000, 0.8660254037844387076, 1.000000000000000000, 0.8660254037844387076, 1.000000000000000000, 0.8660254037844387076, 1.000000000000000000, 0.8660254037844387076, 1.000000000000000000, 0.8660254037844387076, 1.000000000000000000, 0.8660254037844387076, 1.000000000000000000, 0.8660254037844387076, 1.000000000000000000, 0.8660254037844387076, 1.000000000000000000, 0.8660254037844387076, 1.000000000000000000, 0.8660254037844387076, 1.000000000000000000, 0.8660254037844387076, 1.000000000000000000, 0.8660254037844387076, 1.000000000000000000, 0.8660254037844387076, 1.000000000000000000, 0.8660254037844387076, 1.000000000000000000, 0.8660254037844387076, 1.000000000000000000, 0.8660254037844387076, 1.000000000000000000, 0.8660254037844387076, 1.000000000000000000, 0.8660254037844387076, 1.000000000000000000, 0.8660254037844387076, 1.000000000000000000, 0.8660254037844387076, 1.000000000000000000, 0.8660254037844387076, 1.000000000000000000, 0.8660254037844387076, 1.000000000000000000, 0.8660254037844387076, 1.000000000000000000, 0.8660254037844387076, 1.000000000000000000, 0.8660254037844387076, 1.000000000000000000, 0.8660254037844387076, 1.000000000000000000, 0.8660254037844387076, 1.000000000000000000, 0.8660254037844387076, 1.000000000000000000, 0.8660254037844387076, 1.000000000000000000, 0.8660254037844387076, 1.000000000000000000, 0.8660254037844387076, 1.000000000000000000, 0.8660254037844387076, 1.000000000000000000, 0.8660254037844387076, 1.000000000000000000, 0.8660254037844387076, 1.000000000000000000, 0.8660254037844387076, 1.000000000000000000, 0.8660254037844387076, 1.000000000000000000, 0.8660254037844387076, 1.000000000000000000, 0.8660254037844387076, 1.000000000000000000, 0.8660254037844387076, 1.000000000000000000, 0.8660254037844387076, 1.000000000000000000, 0.8660254037844387076, 1.000000000000000000, 0.8660254037844387076, 1.000000000000000000, 0.8660254037844387076, 1.000000000000000000, 0.8660254037844387076, 1.000000000000000000, 0.8660254037844387076, 1.000000000000000000, 0.8660254037844387076, 1.000000000000000000, 0.8660254037844387076, 1.000000000000000000, 0.8660254037844387076, 1.000000000000000000, 0.8660254037844387076, 1.000000000000000000, 0.8660254037844387076, 1.000000000000000000, 0.8660254037844387076, 1.000000000000000000, 0.8660254037844387076, 1.000000000000000000, 0.8660254037844387076, 1.000000000000000000, 0.8660254037844387076, 1.000000000000000000, 0.8660254037844387076, 1.000000000000000000, 0.8660254037844387076, 1.000000000000000000, 0.8660254037844387076, 1.000000000000000000, 0.8660254037844387076, 1.000000000000000000, 0.8660254037844387076, 1.000000000000000000, 0.8660254037844387076, 1.000000000000000000, 0.8660254037844387076, 1.000000000000000000, 0.8660254037844387076, 1.000000000000000000, 0.8660254037844387076, 1.000000000000000000, 0.8660254037844387076, 1.000000000000000000, 0.8660254037844387076, 1.000000000000000000, 0.8660254037844387076, 1.000000000000000000, 0.8660254037844387076, 1.000000000000000000, 0.8660254037844387076, 1.000000000000000000, 0.8660254037844387076, 1.000000000000000000, 0.8660254037844387076, 1.000000000000000000, 0.8660254037844387076, 1.000000000000000000, 0.8660254037844387076, 1.000000000000000000, 0.8660254037844387076, 1.000000000000000000, 0.8660254037844387076, 1.000000000000000000, 0.8660254037844387076, 1.000000000000000000, 0.8660254037844387076, 1.000000000000000000, 0.8660254037844387076, 1.000000000000000000, 0.8660254037844387076, 1.000000000000000000, 0.8660254037844387076, 1.000000000000000000, 0.8660254037844387076, 1.000000000000000000, 0.8660254037844387076, 1.000000000000000000, 0.8660254037844387076, 1.000000000000000000, 0.8660254037844387076, 1.000000000000000000, 0.8660254037844387076, 1.000000000000000000, 0.8660254037844387076, 1.000000000000000000, 0.8660254037844387076, 1.000000000000000000, 0.8660254037844387076, 1.000000000000000000, 0.8660254037844387076, 1.000000000000000000, 0.8660254037844387076, 1.000000000000000000, 0.8660254037844387076, 1.000000000000000000, 0.8660254037844387076, 1.000000000000000000, 0.8660254037844387076, 1.000000000000000000, 0.8660254037844387076, 1.000000000000000000, 0.8660254037844387076, 1.000000000000000000, 0.8660254037844387076, 1.000000000000000000, 0.8660254037844387076, 1.000000000000000000, 0.8660254037844387076, 1.000000000000000000, 0.8660254037844387076, 1.000000000000000000, 0.8660254037844387076, 1.000000000000000000, 0.8660254037844387076, 1.000000000000000000, 0.8660254037844387076, 1.000000000000000000, 0.8660254037844387076, 1.000000000000000000, 0.8660254037844387076, 1.000000000000000000, 0.8660254037844387076, 1.000000000000000000, 0.8660254037844387076, 1.000000000000000000, 0.8660254037844387076, 1.000000000000000000, 0.8660254037844387076, 1.000000000000000000, 0.8660254037844387076, 1.000000000000000000, 0.8660254037844387076, 1.000000000000000000, 0.8660254037844387076, 1.000000000000000000, 0.8660254037844387076, 1.000000000000000000, 0.8660254037844387076, 1.000000000000000000, 0.8660254037844387076, 1.000000000000000000, 0.8660254037844387076, 1.000000000000000000, 0.8660254037844387076, 1.000000000000000000, 0.8660254037844387076, 1.000000000000000000, 0.8660254037844387076, 1.000000000000000000, 0.8660254037844387076, 1.000000000000000000, 0.8660254037844387076, 1.000000000000000000, 0.8660254037844387076, 1.000000000000000000, 0.8660254037844387076, 1.000000000000000000, 0.8660254037844387076, 1.000000000000000000, 0.8660254037844387076, 1.000000000000000000, 0.8660254037844387076, 1.000000000000000000, 0.8660254037844387076, 1.000000000000000000, 0.8660254037844387076, 1.000000000000000000, 0.8660254037844387076, 1.000000000000000000, 0.8660254037844387076, 1.000000000000000000, 0.8660254037844387076, 1.000000000000000000, 0.8660254037844387076, 1.000000000000000000, 0.8660254037844387076, 1.000000000000000000, 0.8660254037844387076, 1.000000000000000000, 0.8660254037844387076, 1.000000000000000000, 0.8660254037844387076, 1.000000000000000000, 0.8660254037844387076, 1.000000000000000000, 0.8660254037844387076, 1.000000000000000000, 0.8660254037844387076, 1.000000000000000000, 0.8660254037844387076, 1.000000000000000000, 0.8660254037844387076, 1.000000000000000000, 0.8660254037844387076, 1.000000000000000000, 0.8660254037844387076, 1.000000000000000000, 0.8660254037844387076, 1.000000000000000000, 0.8660254037844387076, 1.000000000000000000, 0.8660254037844387076, 1.000000000000000000, 0.8660254037844387076, 1.000000000000000000, 0.8660254037844387076, 1.000000000000000000, 0.8660254037844387076, 1.000000000000000000, 0.8660254037844387076, 1.000000000000000000, 0.8660254037844387076, 1.000000000000000000, 0.8660254037844387076, 1.000000000000000000, 0.8660254037844387076, 1.000000000000000000, 0.8660254037844387076, 1.000000000000000000, 0.8660254037844387076, 1.000000000000000000, 0.8660254037844387076, 1.000000000000000000, 0.8660254037844387076, 1.000000000000000000, 0.8660254037844387076, 1.000000000000000000, 0.8660254037844387076, 1.000000000000000000, 0.8660254037844387076, 1.000000000000000000, 0.8660254037844387076, 1.000000000000000000, 0.8660254037844387076, 1.000000000000000000, 0.8660254037844387076, 1.000000000000000000, 0.8660254037844387076, 1.000000000000000000, 0.8660254037844387076, 1.000000000000000000, 0.8660254037844387076, 1.000000000000000000, 0.8660254037844387076, 1.000000000000000000, 0.8660254037844387076, 1.000000000000000000, 0.8660254037844387076, 1.000000000000000000, 0.8660254037844387076, 1.000000000000000000, 0.8660254037844387076, 1.000000000000000000, 0.8660254037844387076, 1.000000000000000000, 0.8660254037844387076, 1.000000000000000000, 0.8660254037844387076, 1.000000000000000000, 0.8660254037844387076, 1.000000000000000000, 0.8660254037844387076, 1.000000000000000000, 0.8660254037844387076, 1.000000000000000000, 0.8660254037844387076, 1.000000000000000000, 0.8660254037844387076, 1.000000000000000000, 0.8660254037844387076, 1.000000000000000000, 0.8660254037844387076, 1.000000000000000000, 0.8660254037844387076, 1.000000000000000000, 0.8660254037844387076, 1.000000000000000000, 0.8660254037844387076, 1.000000000000000000, 0.8660254037844387076, 1.000000000000000000, 0.8660254037844387076, 1.000000000000000000, 0.8660254037844387076, 1.000000000000000000, 0.8660254037844387076, 1.000000000000000000, 0.8660254037844387076, 1.000000000000000000, 0.8660254037844387076, 1.000000000000000000, 0.8660254037844387076, 1.000000000000000000, 0.8660254037844387076, 1.000000000000000000, 0.8660254037844387076, 1.000000000000000000, 0.8660254037844387076, 1.000000000000000000, 0.8660254037844387076, 1.000000000000000000, 0.8660254037844387076, 1.000000000000000000, 0.8660254037844387076, 1.000000000000000000, 0.8660254037844387076, 1.000000000000000000, 0.8660254037844387076, 1.000000000000000000, 0.8660254037844387076, 1.000000000000000000, 0.8660254037844387076, 1.000000000000000000, 0.8660254037844387076, 1.000000000000000000, 0.8660254037844387076, 1.000000000000000000, 0.8660254037844387076, 1.000000000000000000, 0.8660254037844387076, 1.000000000000000000, 0.8660254037844387076, 1.000000000000000000, 0.8660254037844387076, 1.000000000000000000, 0.8660254037844387076, 1.000000000000000000, 0.8660254037844387076, 1.000000000000000000, 0.8660254037844387076, 1.000000000000000000, 0.8660254037844387076, 1.000000000000000000, 0.8660254037844387076, 1.000000000000000000, 0.8660254037844387076, 1.000000000000000000, 0.8660254037844387076, 1.000000000000000000, 0.8660254037844387076, 1.000000000000000000, 0.8660254037844387076, 1.000000000000000000, 0.8660254037844387076, 1.000000000000000000, 0.8660254037844387076, 1.000000000000000000, 0.8660254037844387076, 1.000000000000000000, 0.8660254037844387076, 1.000000000000000000, 0.8660254037844387076, 1.000000000000000000, 0.8660254037844387076, 1.000000000000000000, 0.8660254037844387076, 1.000000000000000000, 0.8660254037844387076, 1.000000000000000000, 0.8660254037844387076, 1.000000000000000000, 0.8660254037844387076, 1.000000000000000000, 0.8660254037844387076, 1.000000000000000000, 0.8660254037844387076, 1.000000000000000000, 0.8660254037844387076, 1.000000000000000000, 0.8660254037844387076, 1.000000000000000000, 0.8660254037844387076, 1.000000000000000000, 0.8660254037844387076, 1.000000000000000000, 0.8660254037844387076, 1.000000000000000000, 0.8660254037844387076, 1.000000000000000000, 0.8660254037844387076, 1.000000000000000000, 0.8660254037844387076, 1.000000000000000000, 0.8660254037844387076, 1.000000000000000000, 0.8660254037844387076, 1.000000000000000000, 0.8660254037844387076, 1.000000000000000000, 0.8660254037844387076, 1.000000000000000000, 0.8660254037844387076, 1.000000000000000000, 0.8660254037844387076, 1.000000000000000000, 0.8660254037844387076, 1.000000000000000000, 0.8660254037844387076, 1.000000000000000000, 0.8660254037844387076, 1.000000000000000000, 0.8660254037844387076, 1.000000000000000000, 0.8660254037844387076, 1.000000000000000000, 0.8660254037844387076, 1.000000000000000000, 0.8660254037844387076, 1.000000000000000000, 0.8660254037844387076, 1.000000000000000000, 0.8660254037844387076, 1.000000000000000000, 0.8660254037844387076, 1.000000000000000000, 0.8660254037844387076, 1.000000000000000000, 0.8660254037844387076, 1.000000000000000000, 0.8660254037844387076, 1.000000000000000000, 0.8660254037844387076, 1.000000000000000000, 0.8660254037844387076, 1.000000000000000000, 0.8660254037844387076, 1.000000000000000000, 0.8660254037844387076, 1.000000000000000000, 0.8660254037844387076, 1.000000000000000000, 0.8660254037844387076, 1.000000000000000000, 0.8660254037844387076, 1.000000000000000000, 0.8660254037844387076, 1.000000000000000000, 0.8660254037844387076, 1.000000000000000000, 0.8660254037844387076, 1.000000000000000000, 0.8660254037844387076, 1.000000000000000000, 0.8660254037844387076, 1.000000000000000000, 0.8660254037844387076, 1.000000000000000000, 0.8660254037844387076, 1.000000000000000000, 0.8660254037844387076, 1.000000000000000000, 0.8660254037844387076, 1.000000000000000000, 0.8660254037844387076, 1.000000000000000000, 0.8660254037844387076, 1.000000000000000000, 0.8660254037844387076, 1.000000000000000000, 0.8660254037844387076, 1.000000000000000000, 0.8660254037844387076, 1.000000000000000000, 0.8660254037844387076, 1.000000000000000000, 0.8660254037844387076, 1.000000000000000000, 0.8660254037844387076, 1.000000000000000000, 0.8660254037844387076, 1.000000000000000000, 0.8660254037844387076, 1.000000000000000000, 0.8660254037844387076, 1.000000000000000000, 0.8660254037844387076, 1.000000000000000000, 0.8660254037844387076, 1.000000000000000000, 0.8660254037844387076, 1.000000000000000000, 0.8660254037844387076, 1.000000000000000000, 0.8660254037844387076, 1.000000000000000000, 0.8660254037844387076, 1.000000000000000000, 0.8660254037844387076, 1.000000000000000000, 0.8660254037844387076, 1.000000000000000000, 0.8660254037844387076, 1.000000000000000000, 0.8660254037844387076, 1.000000000000000000, 0.8660254037844387076, 1.000000000000000000, 0.8660254037844387076, 1.000000000000000000, 0.8660254037844387076, 1.000000000000000000, 0.8660254037844387076, 1.000000000000000000, 0.8660254037844387076, 1.000000000000000000, 0.8660254037844387076, 1.000000000000000000, 0.8660254037844387076, 1.000000000000000000, 0.8660254037844387076, 1.000000000000000000, 0.8660254037844387076, 1.000000000000000000, 0.8660254037844387076, 1.000000000000000000, 0.8660254037844387076, 1.000000000000000000, 0.8660254037844387076, 1.000000000000000000, 0.8660254037844387076, 1.000000000000000000, 0.8660254037844387076, 1.000000000000000000, 0.8660254037844387076, 1.000000000000000000, 0.8660254037844387076, 1.000000000000000000, 0.8660254037844387076, 1.000000000000000000, 0.8660254037844387076, 1.000000000000000000, 0.8660254037844387076, 1.000000000000000000, 0.8660254037844387076, 1.000000000000000000, 0.8660254037844387076, 1.000000000000000000, 0.8660254037844387076, 1.000000000000000000, 0.8660254037844387076, 1.000000000000000000, 0.8660254037844387076, 1.000000000000000000, 0.8660254037844387076, 1.000000000000000000, 0.8660254037844387076, 1.000000000000000000, 0.8660254037844387076, 1.000000000000000000, 0.8660254037844387076, 1.000000000000000000, 0.8660254037844387076, 1.000000000000000000, 0.8660254037844387076, 1.000000000000000000, 0.8660254037844387076, 1.000000000000000000, 0.8660254037844387076, 1.000000000000000000, 0.8660254037844387076, 1.000000000000000000, 0.8660254037844387076, 1.000000000000000000, 0.8660254037844387076, 1.000000000000000000, 0.8660254037844387076, 1.000000000000000000, 0.8660254037844387076, 1.000000000000000000, 0.8660254037844387076, 1.000000000000000000, 0.8660254037844387076, 1.000000000000000000, 0.8660254037844387076, 1.000000000000000000, 0.8660254037844387076, 1.000000000000000000, 0.8660254037844387076, 1.000000000000000000, 0.8660254037844387076, 1.000000000000000000, 0.8660254037844387076, 1.000000000000000000, 0.8660254037844387076, 1.000000000000000000, 0.8660254037844387076, 1.000000000000000000, 0.8660254037844387076, 1.000000000000000000, 0.8660254037844387076, 1.000000000000000000, 0.8660254037844387076, 1.000000000000000000, 0.8660254037844387076, 1.000000000000000000, 0.8660254037844387076, 1.000000000000000000, 0.8660254037844387076, 1.000000000000000000, 0.8660254037844387076, 1.000000000000000000, 0.8660254037844387076, 1.000000000000000000, 0.8660254037844387076, 1.000000000000000000, 0.8660254037844387076, 1.000000000000000000, 0.8660254037844387076, 1.000000000000000000, 0.8660254037844387076, 1.000000000000000000, 0.8660254037844387076, 1.000000000000000000, 0.8660254037844387076, 1.000000000000000000, 0.8660254037844387076, 1.000000000000000000, 0.8660254037844387076, 1.000000000000000000, 0.8660254037844387076, 1.000000000000000000, 0.8660254037844387076, 1.000000000000000000, 0.8660254037844387076, 1.000000000000000000, 0.8660254037844387076, 1.000000000000000000, 0.8660254037844387076, 1.000000000000000000, 0.8660254037844387076, 1.000000000000000000, 0.8660254037844387076, 1.000000000000000000, 0.8660254037844387076, 1.000000000000000000, 0.8660254037844387076, 1.000000000000000000, 0.8660254037844387076, 1.000000000000000000, 0.8660254037844387076, 1.000000000000000000, 0.8660254037844387076, 1.000000000000000000, 0.8660254037844387076, 1.000000000000000000, 0.8660254037844387076, 1.000000000000000000, 0.8660254037844387076, 1.000000000000000000, 0.8660254037844387076, 1.000000000000000000, 0.8660254037844387076, 1.000000000000000000, 0.8660254037844387076, 1.000000000000000000, 0.8660254037844387076, 1.000000000000000000, 0.8660254037844387076, 1.000000000000000000, 0.8660254037844387076, 1.000000000000000000, 0.8660254037844387076, 1.000000000000000000, 0.8660254037844387076, 1.000000000000000000, 0.8660254037844387076, 1.000000000000000000, 0.8660254037844387076, 1.000000000000000000, 0.8660254037844387076, 1.000000000000000000, 0.8660254037844387076, 1.000000000000000000, 0.8660254037844387076, 1.000000000000000000, 0.8660254037844387076, 1.000000000000000000, 0.8660254037844387076, 1.000000000000000000, 0.8660254037844387076, 1.000000000000000000, 0.8660254037844387076, 1.000000000000000000, 0.8660254037844387076, 1.000000000000000000, 0.8660254037844387076, 1.000000000000000000, 0.8660254037844387076, 1.000000000000000000, 0.8660254037844387076, 1.000000000000000000, 0.8660254037844387076, 1.000000000000000000, 0.8660254037844387076, 1.000000000000000000, 0.8660254037844387076, 1.000000000000000000, 0.8660254037844387076, 1.000000000000000000, 0.8660254037844387076, 1.000000000000000000, 0.8660254037844387076, 1.000000000000000000, 0.8660254037844387076, 1.000000000000000000, 0.8660254037844387076, 1.000000000000000000, 0.8660254037844387076, 1.000000000000000000, 0.8660254037844387076, 1.000000000000000000, 0.8660254037844387076, 1.000000000000000000, 0.8660254037844387076, 1.000000000000000000, 0.8660254037844387076, 1.000000000000000000, 0.8660254037844387076, 1.000000000000000000, 0.8660254037844387076, 1.000000000000000000, 0.8660254037844387076, 1.000000000000000000, 0.8660254037844387076, 1.000000000000000000, 0.8660254037844387076, 1.000000000000000000, 0.8660254037844387076, 1.000000000000000000, 0.8660254037844387076, 1.000000000000000000, 0.8660254037844387076, 1.000000000000000000, 0.8660254037844387076, 1.000000000000000000, 0.8660254037844387076, 1.000000000000000000, 0.8660254037844387076, 1.000000000000000000, 0.8660254037844387076, 1.000000000000000000, 0.8660254037844387076, 1.000000000000000000, 0.8660254037844387076, 1.000000000000000000, 0.8660254037844387076, 1.000000000000000000, 0.8660254037844387076, 1.000000000000000000, 0.8660254037844387076, 1.000000000000000000, 0.8660254037844387076, 1.000000000000000000, 0.8660254037844387076, 1.000000000000000000, 0.8660254037844387076, 1.000000000000000000, 0.8660254037844387076, 1.000000000000000000, 0.8660254037844387076, 1.000000000000000000, 0.8660254037844387076, 1.000000000000000000, 0.8660254037844387076, 1.000000000000000000, 0.8660254037844387076, 1.000000000000000000, 0.8660254037844387076, 1.000000000000000000, 0.8660254037844387076, 1.000000000000000000, 0.8660254037844387076, 1.000000000000000000, 0.8660254037844387076, 1.000000000000000000, 0.8660254037844387076, 1.000000000000000000, 0.8660254037844387076, 1.000000000000000000, 0.8660254037844387076, 1.000000000000000000, 0.8660254037844387076, 1.000000000000000000, 0.8660254037844387076, 1.000000000000000000, 0.8660254037844387076, 1.000000000000000000, 0.8660254037844387076, 1.000000000000000000, 0.8660254037844387076, 1.000000000000000000, 0.8660254037844387076, 1.000000000000000000, 0.8660254037844387076, 1.000000000000000000, 0.8660254037844387076, 1.000000000000000000, 0.8660254037844387076, 1.000000000000000000, 0.8660254037844387076, 1.000000000000000000, 0.8660254037844387076, 1.000000000000000000, 0.8660254037844387076, 1.000000000000000000, 0.8660254037844387076, 1.000000000000000000, 0.8660254037844387076, 1.000000000000000000, 0.8660254037844387076, 1.000000000000000000, 0.8660254037844387076, 1.000000000000000000, 0.8660254037844387076, 1.000000000000000000, 0.8660254037844387076, 1.000000000000000000, 0.8660254037844387076, 1.000000000000000000, 0.8660254037844387076, 1.000000000000000000, 0.8660254037844387076, 1.000000000000000000, 0.8660254037844387076, 1.000000000000000000, 0.8660254037844387076, 1.000000000000000000, 0.8660254037844387076, 1.000000000000000000, 0.8660254037844387076, 1.000000000000000000, 0.8660254037844387076, 1.000000000000000000, 0.8660254037844387076, 1.000000000000000000, 0.8660254037844387076, 1.000000000000000000, 0.8660254037844387076, 1.000000000000000000, 0.8660254037844387076, 1.000000000000000000, 0.8660254037844387076, 1.000000000000000000, 0.8660254037844387076, 1.000000000000000000, 0.8660254037844387076, 1.000000000000000000, 0.8660254037844387076, 1.000000000000000000, 0.8660254037844387076, 1.000000000000000000, 0.8660254037844387076, 1.000000000000000000, 0.8660254037844387076, 1.000000000000000000, 0.8660254037844387076, 1.000000000000000000, 0.8660254037844387076, 1.000000000000000000, 0.8660254037844387076, 1.000000000000000000, 0.8660254037844387076, 1.000000000000000000, 0.8660254037844387076, 1.000000000000000000, 0.8660254037844387076, 1.000000000000000000, 0.8660254037844387076, 1.000000000000000000, 0.8660254037844387076, 1.000000000000000000, 0.8660254037844387076, 1.000000000000000000, 0.8660254037844387076, 1.000000000000000000, 0.8660254037844387076, 1.000000000000000000, 0.8660254037844387076, 1.000000000000000000, 0.8660254037844387076, 1.000000000000000000, 0.8660254037844387076, 1.000000000000000000, 0.8660254037844387076, 1.000000000000000000, 0.8660254037844387076, 1.000000000000000000, 0.8660254037844387076, 1.000000000000000000, 0.8660254037844387076, 1.000000000000000000, 0.8660254037844387076, 1.000000000000000000, 0.8660254037844387076, 1.000000000000000000, 0.8660254037844387076, 1.000000000000000000, 0.8660254037844387076, 1.000000000000000000, 0.8660254037844387076, 1.000000000000000000, 0.8660254037844387076, 1.000000000000000000, 0.8660254037844387076, 1.000000000000000000, 0.8660254037844387076, 1.000000000000000000, 0.8660254037844387076, 1.000000000000000000, 0.8660254037844387076, 1.000000000000000000, 0.8660254037844387076, 1.000000000000000000, 0.8660254037844387076, 1.000000000000000000, 0.8660254037844387076, 1.000000000000000000, 0.8660254037844387076, 1.000000000000000000, 0.8660254037844387076, 1.000000000000000000, 0.8660254037844387076, 1.000000000000000000, 0.8660254037844387076, 1.000000000000000000, 0.8660254037844387076, 1.000000000000000000, 0.8660254037844387076, 1.000000000000000000, 0.8660254037844387076, 1.000000000000000000, 0.8660254037844387076, 1.000000000000000000, 0.8660254037844387076, 1.000000000000000000, 0.8660254037844387076, 1.000000000000000000, 0.8660254037844387076, 1.000000000000000000, 0.8660254037844387076, 1.000000000000000000, 0.8660254037844387076, 1.000000000000000000, 0.8660254037844387076, 1.000000000000000000, 0.8660254037844387076, 1.000000000000000000, 0.8660254037844387076, 1.000000000000000000, 0.8660254037844387076, 1.000000000000000000, 0.8660254037844387076, 1.000000000000000000, 0.8660254037844387076, 1.000000000000000000, 0.8660254037844387076, 1.000000000000000000, 0.8660254037844387076, 1.000000000000000000, 0.8660254037844387076, 1.000000000000000000, 0.8660254037844387076, 1.000000000000000000, 0.8660254037844387076, 1.000000000000000000, 0.8660254037844387076, 1.000000000000000000, 0.8660254037844387076, 1.000000000000000000, 0.8660254037844387076, 1.000000000000000000, 0.8660254037844387076, 1.000000000000000000, 0.8660254037844387076, 1.000000000000000000, 0.8660254037844387076, 1.000000000000000000, 0.8660254037844387076, 1.000000000000000000, 0.8660254037844387076, 1.000000000000000000, 0.8660254037844387076, 1.000000000000000000, 0.8660254037844387076, 1.000000000000000000, 0.8660254037844387076, 1.000000000000000000, 0.8660254037844387076, 1.000000000000000000, 0.8660254037844387076, 1.000000000000000000, 0.8660254037844387076, 1.000000000000000000, 0.8660254037844387076, 1.000000000000000000, 0.8660254037844387076, 1.000000000000000000, 0.8660254037844387076, 1.000000000000000000, 0.8660254037844387076, 1.000000000000000000, 0.8660254037844387076, 1.000000000000000000, 0.8660254037844387076, 1.000000000000000000, 0.8660254037844387076, 1.000000000000000000, 0.8660254037844387076, 1.000000000000000000, 0.8660254037844387076, 1.000000000000000000, 0.8660254037844387076, 1.000000000000000000, 0.8660254037844387076, 1.000000000000000000, 0.8660254037844387076, 1.000000000000000000, 0.8660254037844387076, 1.000000000000000000, 0.8660254037844387076, 1.000000000000000000, 0.8660254037844387076, 1.000000000000000000, 0.8660254037844387076, 1.000000000000000000, 0.8660254037844387076, 1.000000000000000000, 0.8660254037844387076, 1.000000000000000000, 0.8660254037844387076, 1.000000000000000000, 0.8660254037844387076, 1.000000000000000000, 0.8660254037844387076, 1.000000000000000000, 0.8660254037844387076, 1.000000000000000000, 0.8660254037844387076, 1.000000000000000000, 0.8660254037844387076, 1.000000000000000000, 0.8660254037844387076, 1.000000000000000000, 0.8660254037844387076, 1.000000000000000000, 0.8660254037844387076, 1.000000000000000000, 0.8660254037844387076, 1.000000000000000000, 0.8660254037844387076, 1.000000000000000000, 0.8660254037844387076, 1.000000000000000000, 0.8660254037844387076, 1.000000000000000000, 0.8660254037844387076, 1.000000000000000000, 0.8660254037844387076, 1.000000000000000000, 0.8660254037844387076, 1.000000000000000000, 0.8660254037844387076, 1.000000000000000000, 0.8660254037844387076, 1.000000000000000000, 0.8660254037844387076, 1.000000000000000000, 0.8660254037844387076, 1.000000000000000000, 0.8660254037844387076, 1.000000000000000000, 0.8660254037844387076, 1.000000000000000000, 0.8660254037844387076, 1.000000000000000000, 0.8660254037844387076, 1.000000000000000000, 0.8660254037844387076, 1.000000000000000000, 0.8660254037844387076, 1.000000000000000000, 0.8660254037844387076, 1.000000000000000000, 0.8660254037844387076, 1.000000000000000000, 0.8660254037844387076, 1.000000000000000000, 0.8660254037844387076, 1.000000000000000000, 0.8660254037844387076, 1.000000000000000000, 0.8660254037844387076, 1.000000000000000000, 0.8660254037844387076, 1.000000000000000000, 0.8660254037844387076, 1.000000000000000000, 0.8660254037844387076, 1.000000000000000000, 0.8660254037844387076, 1.000000000000000000, 0.8660254037844387076, 1.000000000000000000, 0.8660254037844387076, 1.000000000000000000, 0.8660254037844387076, 1.000000000000000000, 0.8660254037844387076, 1.000000000000000000, 0.8660254037844387076, 1.000000000000000000, 0.8660254037844387076, 1.000000000000000000, 0.8660254037844387076, 1.000000000000000000, 0.8660254037844387076, 1.000000000000000000, 0.8660254037844387076, 1.000000000000000000, 0.8660254037844387076, 1.000000000000000000),
 ( 1.000000000000000000, 0.8660254037844387076, 1.000000000000000000, 0.8660254037844387076, 1.000000000000000000, 0.8660254037844387076, 1.000000000000000000, 0.8660254037844387076, 1.000000000000000000, 0.8660254037844387076, 1.000000000000000000, 0.8660254037844387076, 1.000000000000000000, 0.8660254037844387076, 1.000000000000000000, 0.8660254037844387076, 1.000000000000000000, 0.8660254037844387076, 1.000000000000000000, 0.8660254037844387076, 1.000000000000000000, 0.8660254037844387076, 1.000000000000000000, 0.8660254037844387076, 1.000000000000000000, 0.8660254037844387076, 1.000000000000000000, 0.8660254037844387076, 1.000000000000000000, 0.8660254037844387076, 1.000000000000000000, 0.8660254037844387076, 1.000000000000000000, 0.8660254037844387076, 1.000000000000000000, 0.8660254037844387076, 1.000000000000000000, 0.8660254037844387076, 1.000000000000000000, 0.8660254037844387076, 1.000000000000000000, 0.8660254037844387076, 1.000000000000000000, 0.8660254037844387076, 1.000000000000000000, 0.8660254037844387076, 1.000000000000000000, 0.8660254037844387076, 1.000000000000000000, 0.8660254037844387076, 1.000000000000000000, 0.8660254037844387076, 1.000000000000000000, 0.8660254037844387076, 1.000000000000000000, 0.8660254037844387076, 1.000000000000000000, 0.8660254037844387076, 1.000000000000000000, 0.8660254037844387076, 1.000000000000000000, 0.8660254037844387076, 1.000000000000000000, 0.8660254037844387076, 1.000000000000000000, 0.8660254037844387076, 1.000000000000000000, 0.8660254037844387076, 1.000000000000000000, 0.8660254037844387076, 1.000000000000000000, 0.8660254037844387076, 1.000000000000000000, 0.8660254037844387076, 1.000000000000000000, 0.8660254037844387076, 1.000000000000000000, 0.8660254037844387076, 1.000000000000000000, 0.8660254037844387076, 1.000000000000000000, 0.8660254037844387076, 1.000000000000000000, 0.8660254037844387076, 1.000000000000000000, 0.8660254037844387076, 1.000000000000000000, 0.8660254037844387076, 1.000000000000000000, 0.8660254037844387076, 1.000000000000000000, 0.8660254037844387076, 1.000000000000000000, 0.8660254037844387076, 1.000000000000000000, 0.8660254037844387076, 1.000000000000000000, 0.8660254037844387076, 1.000000000000000000, 0.8660254037844387076, 1.000000000000000000, 0.8660254037844387076, 1.000000000000000000, 0.8660254037844387076, 1.000000000000000000, 0.8660254037844387076, 1.000000000000000000, 0.8660254037844387076, 1.000000000000000000, 0.8660254037844387076, 1.000000000000000000, 0.8660254037844387076, 1.000000000000000000, 0.8660254037844387076, 1.000000000000000000, 0.8660254037844387076, 1.000000000000000000, 0.8660254037844387076, 1.000000000000000000, 0.8660254037844387076, 1.000000000000000000, 0.8660254037844387076, 1.000000000000000000, 0.8660254037844387076, 1.000000000000000000, 0.8660254037844387076, 1.000000000000000000, 0.8660254037844387076, 1.000000000000000000, 0.8660254037844387076, 1.000000000000000000, 0.8660254037844387076, 1.000000000000000000, 0.8660254037844387076, 1.000000000000000000, 0.8660254037844387076, 1.000000000000000000, 0.8660254037844387076, 1.000000000000000000, 0.8660254037844387076, 1.000000000000000000, 0.8660254037844387076, 1.000000000000000000, 0.8660254037844387076, 1.000000000000000000, 0.8660254037844387076, 1.000000000000000000, 0.8660254037844387076, 1.000000000000000000, 0.8660254037844387076, 1.000000000000000000, 0.8660254037844387076, 1.000000000000000000, 0.8660254037844387076, 1.000000000000000000, 0.8660254037844387076, 1.000000000000000000, 0.8660254037844387076, 1.000000000000000000, 0.8660254037844387076, 1.000000000000000000, 0.8660254037844387076, 1.000000000000000000, 0.8660254037844387076, 1.000000000000000000, 0.8660254037844387076, 1.000000000000000000, 0.8660254037844387076, 1.000000000000000000, 0.8660254037844387076, 1.000000000000000000, 0.8660254037844387076, 1.000000000000000000, 0.8660254037844387076, 1.000000000000000000, 0.8660254037844387076, 1.000000000000000000, 0.8660254037844387076, 1.000000000000000000, 0.8660254037844387076, 1.000000000000000000, 0.8660254037844387076, 1.000000000000000000, 0.8660254037844387076, 1.000000000000000000, 0.8660254037844387076, 1.000000000000000000, 0.8660254037844387076, 1.000000000000000000, 0.8660254037844387076, 1.000000000000000000, 0.8660254037844387076, 1.000000000000000000, 0.8660254037844387076, 1.000000000000000000, 0.8660254037844387076, 1.000000000000000000, 0.8660254037844387076, 1.000000000000000000, 0.8660254037844387076, 1.000000000000000000, 0.8660254037844387076, 1.000000000000000000, 0.8660254037844387076, 1.000000000000000000, 0.8660254037844387076, 1.000000000000000000, 0.8660254037844387076, 1.000000000000000000, 0.8660254037844387076, 1.000000000000000000, 0.8660254037844387076, 1.000000000000000000, 0.8660254037844387076, 1.000000000000000000, 0.8660254037844387076, 1.000000000000000000, 0.8660254037844387076, 1.000000000000000000, 0.8660254037844387076, 1.000000000000000000, 0.8660254037844387076, 1.000000000000000000, 0.8660254037844387076, 1.000000000000000000, 0.8660254037844387076, 1.000000000000000000, 0.8660254037844387076, 1.000000000000000000, 0.8660254037844387076, 1.000000000000000000, 0.8660254037844387076, 1.000000000000000000, 0.8660254037844387076, 1.000000000000000000, 0.8660254037844387076, 1.000000000000000000, 0.8660254037844387076, 1.000000000000000000, 0.8660254037844387076, 1.000000000000000000, 0.8660254037844387076, 1.000000000000000000, 0.8660254037844387076, 1.000000000000000000, 0.8660254037844387076, 1.000000000000000000, 0.8660254037844387076, 1.000000000000000000, 0.8660254037844387076, 1.000000000000000000, 0.8660254037844387076, 1.000000000000000000, 0.8660254037844387076, 1.000000000000000000, 0.8660254037844387076, 1.000000000000000000, 0.8660254037844387076, 1.000000000000000000, 0.8660254037844387076, 1.000000000000000000, 0.8660254037844387076, 1.000000000000000000, 0.8660254037844387076, 1.000000000000000000, 0.8660254037844387076, 1.000000000000000000, 0.8660254037844387076, 1.000000000000000000, 0.8660254037844387076, 1.000000000000000000, 0.8660254037844387076, 1.000000000000000000, 0.8660254037844387076, 1.000000000000000000, 0.8660254037844387076, 1.000000000000000000, 0.8660254037844387076, 1.000000000000000000, 0.8660254037844387076, 1.000000000000000000, 0.8660254037844387076, 1.000000000000000000, 0.8660254037844387076, 1.000000000000000000, 0.8660254037844387076, 1.000000000000000000, 0.8660254037844387076, 1.000000000000000000, 0.8660254037844387076, 1.000000000000000000, 0.8660254037844387076, 1.000000000000000000, 0.8660254037844387076, 1.000000000000000000, 0.8660254037844387076, 1.000000000000000000, 0.8660254037844387076, 1.000000000000000000, 0.8660254037844387076, 1.000000000000000000, 0.8660254037844387076, 1.000000000000000000, 0.8660254037844387076, 1.000000000000000000, 0.8660254037844387076, 1.000000000000000000, 0.8660254037844387076, 1.000000000000000000, 0.8660254037844387076, 1.000000000000000000, 0.8660254037844387076, 1.000000000000000000, 0.8660254037844387076, 1.000000000000000000, 0.8660254037844387076, 1.000000000000000000, 0.8660254037844387076, 1.000000000000000000, 0.8660254037844387076, 1.000000000000000000, 0.8660254037844387076, 1.000000000000000000, 0.8660254037844387076, 1.000000000000000000, 0.8660254037844387076, 1.000000000000000000, 0.8660254037844387076, 1.000000000000000000, 0.8660254037844387076, 1.000000000000000000, 0.8660254037844387076, 1.000000000000000000, 0.8660254037844387076, 1.000000000000000000, 0.8660254037844387076, 1.000000000000000000, 0.8660254037844387076, 1.000000000000000000, 0.8660254037844387076, 1.000000000000000000, 0.8660254037844387076, 1.000000000000000000, 0.8660254037844387076, 1.000000000000000000, 0.8660254037844387076, 1.000000000000000000, 0.8660254037844387076, 1.000000000000000000, 0.8660254037844387076, 1.000000000000000000, 0.8660254037844387076, 1.000000000000000000, 0.8660254037844387076, 1.000000000000000000, 0.8660254037844387076, 1.000000000000000000, 0.8660254037844387076, 1.000000000000000000, 0.8660254037844387076, 1.000000000000000000, 0.8660254037844387076, 1.000000000000000000, 0.8660254037844387076, 1.000000000000000000, 0.8660254037844387076, 1.000000000000000000, 0.8660254037844387076, 1.000000000000000000, 0.8660254037844387076, 1.000000000000000000, 0.8660254037844387076, 1.000000000000000000, 0.8660254037844387076, 1.000000000000000000, 0.8660254037844387076, 1.000000000000000000, 0.8660254037844387076, 1.000000000000000000, 0.8660254037844387076, 1.000000000000000000, 0.8660254037844387076, 1.000000000000000000, 0.8660254037844387076, 1.000000000000000000, 0.8660254037844387076, 1.000000000000000000, 0.8660254037844387076, 1.000000000000000000, 0.8660254037844387076, 1.000000000000000000, 0.8660254037844387076, 1.000000000000000000, 0.8660254037844387076, 1.000000000000000000, 0.8660254037844387076, 1.000000000000000000, 0.8660254037844387076, 1.000000000000000000, 0.8660254037844387076, 1.000000000000000000, 0.8660254037844387076, 1.000000000000000000, 0.8660254037844387076, 1.000000000000000000, 0.8660254037844387076, 1.000000000000000000, 0.8660254037844387076, 1.000000000000000000, 0.8660254037844387076, 1.000000000000000000, 0.8660254037844387076, 1.000000000000000000, 0.8660254037844387076, 1.000000000000000000, 0.8660254037844387076, 1.000000000000000000, 0.8660254037844387076, 1.000000000000000000, 0.8660254037844387076, 1.000000000000000000, 0.8660254037844387076, 1.000000000000000000, 0.8660254037844387076, 1.000000000000000000, 0.8660254037844387076, 1.000000000000000000, 0.8660254037844387076, 1.000000000000000000, 0.8660254037844387076, 1.000000000000000000, 0.8660254037844387076, 1.000000000000000000, 0.8660254037844387076, 1.000000000000000000, 0.8660254037844387076, 1.000000000000000000, 0.8660254037844387076, 1.000000000000000000, 0.8660254037844387076, 1.000000000000000000, 0.8660254037844387076, 1.000000000000000000, 0.8660254037844387076, 1.000000000000000000, 0.8660254037844387076, 1.000000000000000000, 0.8660254037844387076, 1.000000000000000000, 0.8660254037844387076, 1.000000000000000000, 0.8660254037844387076, 1.000000000000000000, 0.8660254037844387076, 1.000000000000000000, 0.8660254037844387076, 1.000000000000000000, 0.8660254037844387076, 1.000000000000000000, 0.8660254037844387076, 1.000000000000000000, 0.8660254037844387076, 1.000000000000000000, 0.8660254037844387076, 1.000000000000000000, 0.8660254037844387076, 1.000000000000000000, 0.8660254037844387076, 1.000000000000000000, 0.8660254037844387076, 1.000000000000000000, 0.8660254037844387076, 1.000000000000000000, 0.8660254037844387076, 1.000000000000000000, 0.8660254037844387076, 1.000000000000000000, 0.8660254037844387076, 1.000000000000000000, 0.8660254037844387076, 1.000000000000000000, 0.8660254037844387076, 1.000000000000000000, 0.8660254037844387076, 1.000000000000000000, 0.8660254037844387076, 1.000000000000000000, 0.8660254037844387076, 1.000000000000000000, 0.8660254037844387076, 1.000000000000000000, 0.8660254037844387076, 1.000000000000000000, 0.8660254037844387076, 1.000000000000000000, 0.8660254037844387076, 1.000000000000000000, 0.8660254037844387076, 1.000000000000000000, 0.8660254037844387076, 1.000000000000000000, 0.8660254037844387076, 1.000000000000000000, 0.8660254037844387076, 1.000000000000000000, 0.8660254037844387076, 1.000000000000000000, 0.8660254037844387076, 1.000000000000000000, 0.8660254037844387076, 1.000000000000000000, 0.8660254037844387076, 1.000000000000000000, 0.8660254037844387076, 1.000000000000000000, 0.8660254037844387076, 1.000000000000000000, 0.8660254037844387076, 1.000000000000000000, 0.8660254037844387076, 1.000000000000000000, 0.8660254037844387076, 1.000000000000000000, 0.8660254037844387076, 1.000000000000000000, 0.8660254037844387076, 1.000000000000000000, 0.8660254037844387076, 1.000000000000000000, 0.8660254037844387076, 1.000000000000000000, 0.8660254037844387076, 1.000000000000000000, 0.8660254037844387076, 1.000000000000000000, 0.8660254037844387076, 1.000000000000000000, 0.8660254037844387076, 1.000000000000000000, 0.8660254037844387076, 1.000000000000000000, 0.8660254037844387076, 1.000000000000000000, 0.8660254037844387076, 1.000000000000000000, 0.8660254037844387076, 1.000000000000000000, 0.8660254037844387076, 1.000000000000000000, 0.8660254037844387076, 1.000000000000000000, 0.8660254037844387076, 1.000000000000000000, 0.8660254037844387076, 1.000000000000000000, 0.8660254037844387076, 1.000000000000000000, 0.8660254037844387076, 1.000000000000000000, 0.8660254037844387076, 1.000000000000000000, 0.8660254037844387076, 1.000000000000000000, 0.8660254037844387076, 1.000000000000000000, 0.8660254037844387076, 1.000000000000000000, 0.8660254037844387076, 1.000000000000000000, 0.8660254037844387076, 1.000000000000000000, 0.8660254037844387076, 1.000000000000000000, 0.8660254037844387076, 1.000000000000000000, 0.8660254037844387076, 1.000000000000000000, 0.8660254037844387076, 1.000000000000000000, 0.8660254037844387076, 1.000000000000000000, 0.8660254037844387076, 1.000000000000000000, 0.8660254037844387076, 1.000000000000000000, 0.8660254037844387076, 1.000000000000000000, 0.8660254037844387076, 1.000000000000000000, 0.8660254037844387076, 1.000000000000000000, 0.8660254037844387076, 1.000000000000000000, 0.8660254037844387076, 1.000000000000000000, 0.8660254037844387076, 1.000000000000000000, 0.8660254037844387076, 1.000000000000000000, 0.8660254037844387076, 1.000000000000000000, 0.8660254037844387076, 1.000000000000000000, 0.8660254037844387076, 1.000000000000000000, 0.8660254037844387076, 1.000000000000000000, 0.8660254037844387076, 1.000000000000000000, 0.8660254037844387076, 1.000000000000000000, 0.8660254037844387076, 1.000000000000000000, 0.8660254037844387076, 1.000000000000000000, 0.8660254037844387076, 1.000000000000000000, 0.8660254037844387076, 1.000000000000000000, 0.8660254037844387076, 1.000000000000000000, 0.8660254037844387076, 1.000000000000000000, 0.8660254037844387076, 1.000000000000000000, 0.8660254037844387076, 1.000000000000000000, 0.8660254037844387076, 1.000000000000000000, 0.8660254037844387076, 1.000000000000000000, 0.8660254037844387076, 1.000000000000000000, 0.8660254037844387076, 1.000000000000000000, 0.8660254037844387076, 1.000000000000000000, 0.8660254037844387076, 1.000000000000000000, 0.8660254037844387076, 1.000000000000000000, 0.8660254037844387076, 1.000000000000000000, 0.8660254037844387076, 1.000000000000000000, 0.8660254037844387076, 1.000000000000000000, 0.8660254037844387076, 1.000000000000000000, 0.8660254037844387076, 1.000000000000000000, 0.8660254037844387076, 1.000000000000000000, 0.8660254037844387076, 1.000000000000000000, 0.8660254037844387076, 1.000000000000000000, 0.8660254037844387076, 1.000000000000000000, 0.8660254037844387076, 1.000000000000000000, 0.8660254037844387076, 1.000000000000000000, 0.8660254037844387076, 1.000000000000000000, 0.8660254037844387076, 1.000000000000000000, 0.8660254037844387076, 1.000000000000000000, 0.8660254037844387076, 1.000000000000000000, 0.8660254037844387076, 1.000000000000000000, 0.8660254037844387076, 1.000000000000000000, 0.8660254037844387076, 1.000000000000000000, 0.8660254037844387076, 1.000000000000000000, 0.8660254037844387076, 1.000000000000000000, 0.8660254037844387076, 1.000000000000000000, 0.8660254037844387076, 1.000000000000000000, 0.8660254037844387076, 1.000000000000000000, 0.8660254037844387076, 1.000000000000000000, 0.8660254037844387076, 1.000000000000000000, 0.8660254037844387076, 1.000000000000000000, 0.8660254037844387076, 1.000000000000000000, 0.8660254037844387076, 1.000000000000000000, 0.8660254037844387076, 1.000000000000000000, 0.8660254037844387076, 1.000000000000000000, 0.8660254037844387076, 1.000000000000000000, 0.8660254037844387076, 1.000000000000000000, 0.8660254037844387076, 1.000000000000000000, 0.8660254037844387076, 1.000000000000000000, 0.8660254037844387076, 1.000000000000000000, 0.8660254037844387076, 1.000000000000000000, 0.8660254037844387076, 1.000000000000000000, 0.8660254037844387076, 1.000000000000000000, 0.8660254037844387076, 1.000000000000000000, 0.8660254037844387076, 1.000000000000000000, 0.8660254037844387076, 1.000000000000000000, 0.8660254037844387076, 1.000000000000000000, 0.8660254037844387076, 1.000000000000000000, 0.8660254037844387076, 1.000000000000000000, 0.8660254037844387076, 1.000000000000000000, 0.8660254037844387076, 1.000000000000000000, 0.8660254037844387076, 1.000000000000000000, 0.8660254037844387076, 1.000000000000000000, 0.8660254037844387076, 1.000000000000000000, 0.8660254037844387076, 1.000000000000000000, 0.8660254037844387076, 1.000000000000000000, 0.8660254037844387076, 1.000000000000000000, 0.8660254037844387076, 1.000000000000000000, 0.8660254037844387076, 1.000000000000000000, 0.8660254037844387076, 1.000000000000000000, 0.8660254037844387076, 1.000000000000000000, 0.8660254037844387076, 1.000000000000000000, 0.8660254037844387076, 1.000000000000000000, 0.8660254037844387076, 1.000000000000000000, 0.8660254037844387076, 1.000000000000000000, 0.8660254037844387076, 1.000000000000000000, 0.8660254037844387076, 1.000000000000000000, 0.8660254037844387076, 1.000000000000000000, 0.8660254037844387076, 1.000000000000000000, 0.8660254037844387076, 1.000000000000000000, 0.8660254037844387076, 1.000000000000000000, 0.8660254037844387076, 1.000000000000000000, 0.8660254037844387076, 1.000000000000000000, 0.8660254037844387076, 1.000000000000000000, 0.8660254037844387076, 1.000000000000000000, 0.8660254037844387076, 1.000000000000000000, 0.8660254037844387076, 1.000000000000000000, 0.8660254037844387076, 1.000000000000000000, 0.8660254037844387076, 1.000000000000000000, 0.8660254037844387076, 1.000000000000000000, 0.8660254037844387076, 1.000000000000000000, 0.8660254037844387076, 1.000000000000000000, 0.8660254037844387076, 1.000000000000000000, 0.8660254037844387076, 1.000000000000000000, 0.8660254037844387076, 1.000000000000000000, 0.8660254037844387076, 1.000000000000000000, 0.8660254037844387076, 1.000000000000000000, 0.8660254037844387076, 1.000000000000000000, 0.8660254037844387076, 1.000000000000000000, 0.8660254037844387076, 1.000000000000000000, 0.8660254037844387076, 1.000000000000000000, 0.8660254037844387076, 1.000000000000000000, 0.8660254037844387076, 1.000000000000000000, 0.8660254037844387076, 1.000000000000000000, 0.8660254037844387076, 1.000000000000000000, 0.8660254037844387076, 1.000000000000000000, 0.8660254037844387076, 1.000000000000000000, 0.8660254037844387076, 1.000000000000000000, 0.8660254037844387076, 1.000000000000000000, 0.8660254037844387076, 1.000000000000000000, 0.8660254037844387076, 1.000000000000000000, 0.8660254037844387076, 1.000000000000000000, 0.8660254037844387076, 1.000000000000000000, 0.8660254037844387076, 1.000000000000000000, 0.8660254037844387076, 1.000000000000000000, 0.8660254037844387076, 1.000000000000000000, 0.8660254037844387076, 1.000000000000000000, 0.8660254037844387076, 1.000000000000000000, 0.8660254037844387076, 1.000000000000000000, 0.8660254037844387076, 1.000000000000000000, 0.8660254037844387076, 1.000000000000000000, 0.8660254037844387076, 1.000000000000000000, 0.8660254037844387076, 1.000000000000000000, 0.8660254037844387076, 1.000000000000000000, 0.8660254037844387076, 1.000000000000000000, 0.8660254037844387076, 1.000000000000000000, 0.8660254037844387076, 1.000000000000000000, 0.8660254037844387076, 1.000000000000000000, 0.8660254037844387076, 1.000000000000000000, 0.8660254037844387076, 1.000000000000000000, 0.8660254037844387076, 1.000000000000000000, 0.8660254037844387076, 1.000000000000000000, 0.8660254037844387076, 1.000000000000000000, 0.8660254037844387076, 1.000000000000000000, 0.8660254037844387076, 1.000000000000000000, 0.8660254037844387076, 1.000000000000000000, 0.8660254037844387076, 1.000000000000000000, 0.8660254037844387076, 1.000000000000000000, 0.8660254037844387076, 1.000000000000000000, 0.8660254037844387076, 1.000000000000000000, 0.8660254037844387076, 1.000000000000000000, 0.8660254037844387076, 1.000000000000000000, 0.8660254037844387076, 1.000000000000000000, 0.8660254037844387076, 1.000000000000000000, 0.8660254037844387076, 1.000000000000000000, 0.8660254037844387076, 1.000000000000000000, 0.8660254037844387076, 1.000000000000000000, 0.8660254037844387076, 1.000000000000000000, 0.8660254037844387076, 1.000000000000000000, 0.8660254037844387076, 1.000000000000000000, 0.8660254037844387076, 1.000000000000000000, 0.8660254037844387076, 1.000000000000000000, 0.8660254037844387076, 1.000000000000000000, 0.8660254037844387076, 1.000000000000000000, 0.8660254037844387076, 1.000000000000000000, 0.8660254037844387076, 1.000000000000000000, 0.8660254037844387076, 1.000000000000000000, 0.8660254037844387076, 1.000000000000000000, 0.8660254037844387076, 1.000000000000000000, 0.8660254037844387076, 1.000000000000000000, 0.8660254037844387076, 1.000000000000000000, 0.8660254037844387076, 1.000000000000000000, 0.8660254037844387076, 1.000000000000000000, 0.8660254037844387076, 1.000000000000000000, 0.8660254037844387076, 1.000000000000000000, 0.8660254037844387076, 1.000000000000000000, 0.8660254037844387076, 1.000000000000000000, 0.8660254037844387076, 1.000000000000000000, 0.8660254037844387076, 1.000000000000000000, 0.8660254037844387076, 1.000000000000000000, 0.8660254037844387076, 1.000000000000000000, 0.8660254037844387076, 1.000000000000000000, 0.8660254037844387076, 1.000000000000000000, 0.8660254037844387076, 1.000000000000000000, 0.8660254037844387076, 1.000000000000000000, 0.8660254037844387076, 1.000000000000000000, 0.8660254037844387076, 1.000000000000000000, 0.8660254037844387076, 1.000000000000000000, 0.8660254037844387076, 1.000000000000000000, 0.8660254037844387076, 1.000000000000000000, 0.8660254037844387076, 1.000000000000000000, 0.8660254037844387076, 1.000000000000000000, 0.8660254037844387076, 1.000000000000000000, 0.8660254037844387076, 1.000000000000000000, 0.8660254037844387076, 1.000000000000000000, 0.8660254037844387076, 1.000000000000000000, 0.8660254037844387076, 1.000000000000000000, 0.8660254037844387076, 1.000000000000000000, 0.8660254037844387076, 1.000000000000000000, 0.8660254037844387076, 1.000000000000000000, 0.8660254037844387076, 1.000000000000000000, 0.8660254037844387076, 1.000000000000000000, 0.8660254037844387076, 1.000000000000000000, 0.8660254037844387076, 1.000000000000000000, 0.8660254037844387076, 1.000000000000000000, 0.8660254037844387076, 1.000000000000000000, 0.8660254037844387076, 1.000000000000000000, 0.8660254037844387076, 1.000000000000000000, 0.8660254037844387076, 1.000000000000000000, 0.8660254037844387076, 1.000000000000000000, 0.8660254037844387076, 1.000000000000000000, 0.8660254037844387076, 1.000000000000000000, 0.8660254037844387076, 1.000000000000000000, 0.8660254037844387076, 1.000000000000000000, 0.8660254037844387076, 1.000000000000000000, 0.8660254037844387076, 1.000000000000000000, 0.8660254037844387076, 1.000000000000000000, 0.8660254037844387076, 1.000000000000000000, 0.8660254037844387076, 1.000000000000000000, 0.8660254037844387076, 1.000000000000000000, 0.8660254037844387076, 1.000000000000000000, 0.8660254037844387076, 1.000000000000000000, 0.8660254037844387076, 1.000000000000000000, 0.8660254037844387076, 1.000000000000000000, 0.8660254037844387076, 1.000000000000000000, 0.8660254037844387076, 1.000000000000000000, 0.8660254037844387076, 1.000000000000000000, 0.8660254037844387076, 1.000000000000000000, 0.8660254037844387076, 1.000000000000000000, 0.8660254037844387076, 1.000000000000000000, 0.8660254037844387076, 1.000000000000000000, 0.8660254037844387076, 1.000000000000000000, 0.8660254037844387076, 1.000000000000000000, 0.8660254037844387076, 1.000000000000000000, 0.8660254037844387076, 1.000000000000000000, 0.8660254037844387076, 1.000000000000000000, 0.8660254037844387076, 1.000000000000000000, 0.8660254037844387076, 1.000000000000000000, 0.8660254037844387076, 1.000000000000000000, 0.8660254037844387076, 1.000000000000000000, 0.8660254037844387076, 1.000000000000000000, 0.8660254037844387076, 1.000000000000000000, 0.8660254037844387076, 1.000000000000000000, 0.8660254037844387076, 1.000000000000000000, 0.8660254037844387076, 1.000000000000000000, 0.8660254037844387076, 1.000000000000000000, 0.8660254037844387076, 1.000000000000000000, 0.8660254037844387076, 1.000000000000000000, 0.8660254037844387076, 1.000000000000000000, 0.8660254037844387076, 1.000000000000000000, 0.8660254037844387076, 1.000000000000000000, 0.8660254037844387076, 1.000000000000000000, 0.8660254037844387076, 1.000000000000000000, 0.8660254037844387076, 1.000000000000000000, 0.8660254037844387076, 1.000000000000000000, 0.8660254037844387076, 1.000000000000000000, 0.8660254037844387076, 1.000000000000000000, 0.8660254037844387076, 1.000000000000000000, 0.8660254037844387076, 1.000000000000000000, 0.8660254037844387076, 1.000000000000000000, 0.8660254037844387076, 1.000000000000000000, 0.8660254037844387076, 1.000000000000000000, 0.8660254037844387076, 1.000000000000000000, 0.8660254037844387076, 1.000000000000000000, 0.8660254037844387076, 1.000000000000000000, 0.8660254037844387076, 1.000000000000000000, 0.8660254037844387076, 1.000000000000000000, 0.8660254037844387076, 1.000000000000000000, 0.8660254037844387076, 1.000000000000000000, 0.8660254037844387076, 1.000000000000000000, 0.8660254037844387076, 1.000000000000000000, 0.8660254037844387076, 1.000000000000000000, 0.8660254037844387076, 1.000000000000000000, 0.8660254037844387076, 1.000000000000000000, 0.8660254037844387076, 1.000000000000000000, 0.8660254037844387076, 1.000000000000000000, 0.8660254037844387076, 1.000000000000000000, 0.8660254037844387076, 1.000000000000000000, 0.8660254037844387076, 1.000000000000000000, 0.8660254037844387076, 1.000000000000000000, 0.8660254037844387076, 1.000000000000000000, 0.8660254037844387076, 1.000000000000000000, 0.8660254037844387076, 1.000000000000000000, 0.8660254037844387076, 1.000000000000000000, 0.8660254037844387076, 1.000000000000000000, 0.8660254037844387076, 1.000000000000000000, 0.8660254037844387076, 1.000000000000000000, 0.8660254037844387076, 1.000000000000000000, 0.8660254037844387076, 1.000000000000000000, 0.8660254037844387076, 1.000000000000000000, 0.8660254037844387076, 1.000000000000000000, 0.8660254037844387076, 1.000000000000000000, 0.8660254037844387076, 1.000000000000000000, 0.8660254037844387076, 1.000000000000000000, 0.8660254037844387076, 1.000000000000000000, 0.8660254037844387076, 1.000000000000000000, 0.8660254037844387076, 1.000000000000000000, 0.8660254037844387076, 1.000000000000000000, 0.8660254037844387076, 1.000000000000000000, 0.8660254037844387076, 1.000000000000000000, 0.8660254037844387076, 1.000000000000000000, 0.8660254037844387076, 1.000000000000000000, 0.8660254037844387076, 1.000000000000000000, 0.8660254037844387076, 1.000000000000000000, 0.8660254037844387076, 1.000000000000000000, 0.8660254037844387076, 1.000000000000000000, 0.8660254037844387076, 1.000000000000000000, 0.8660254037844387076, 1.000000000000000000, 0.8660254037844387076, 1.000000000000000000, 0.8660254037844387076, 1.000000000000000000, 0.8660254037844387076, 1.000000000000000000, 0.8660254037844387076, 1.000000000000000000, 0.8660254037844387076, 1.000000000000000000, 0.8660254037844387076, 1.000000000000000000, 0.8660254037844387076, 1.000000000000000000, 0.8660254037844387076, 1.000000000000000000, 0.8660254037844387076, 1.000000000000000000, 0.8660254037844387076, 1.000000000000000000, 0.8660254037844387076, 1.000000000000000000, 0.8660254037844387076, 1.000000000000000000, 0.8660254037844387076, 1.000000000000000000, 0.8660254037844387076, 1.000000000000000000, 0.8660254037844387076, 1.000000000000000000, 0.8660254037844387076, 1.000000000000000000, 0.8660254037844387076, 1.000000000000000000, 0.8660254037844387076, 1.000000000000000000, 0.8660254037844387076, 1.000000000000000000, 0.8660254037844387076, 1.000000000000000000, 0.8660254037844387076, 1.000000000000000000, 0.8660254037844387076, 1.000000000000000000, 0.8660254037844387076, 1.000000000000000000, 0.8660254037844387076, 1.000000000000000000, 0.8660254037844387076, 1.000000000000000000, 0.8660254037844387076, 1.000000000000000000, 0.8660254037844387076, 1.000000000000000000, 0.8660254037844387076, 1.000000000000000000, 0.8660254037844387076, 1.000000000000000000, 0.8660254037844387076, 1.000000000000000000, 0.8660254037844387076, 1.000000000000000000, 0.8660254037844387076, 1.000000000000000000, 0.8660254037844387076, 1.000000000000000000, 0.8660254037844387076, 1.000000000000000000, 0.8660254037844387076, 1.000000000000000000, 0.8660254037844387076, 1.000000000000000000, 0.8660254037844387076, 1.000000000000000000, 0.8660254037844387076, 1.000000000000000000, 0.8660254037844387076, 1.000000000000000000, 0.8660254037844387076, 1.000000000000000000, 0.8660254037844387076, 1.000000000000000000, 0.8660254037844387076, 1.000000000000000000, 0.8660254037844387076, 1.000000000000000000, 0.8660254037844387076, 1.000000000000000000, 0.8660254037844387076, 1.000000000000000000, 0.8660254037844387076, 1.000000000000000000, 0.8660254037844387076, 1.000000000000000000, 0.8660254037844387076, 1.000000000000000000, 0.8660254037844387076, 1.000000000000000000, 0.8660254037844387076, 1.000000000000000000, 0.8660254037844387076, 1.000000000000000000, 0.8660254037844387076, 1.000000000000000000, 0.8660254037844387076, 1.000000000000000000, 0.8660254037844387076, 1.000000000000000000, 0.8660254037844387076, 1.000000000000000000, 0.8660254037844387076, 1.000000000000000000, 0.8660254037844387076, 1.000000000000000000, 0.8660254037844387076, 1.000000000000000000, 0.8660254037844387076, 1.000000000000000000, 0.8660254037844387076, 1.000000000000000000, 0.8660254037844387076, 1.000000000000000000, 0.8660254037844387076, 1.000000000000000000, 0.8660254037844387076, 1.000000000000000000, 0.8660254037844387076, 1.000000000000000000, 0.8660254037844387076, 1.000000000000000000, 0.8660254037844387076, 1.000000000000000000, 0.8660254037844387076, 1.000000000000000000, 0.8660254037844387076, 1.000000000000000000, 0.8660254037844387076, 1.000000000000000000, 0.8660254037844387076, 1.000000000000000000, 0.8660254037844387076, 1.000000000000000000, 0.8660254037844387076, 1.000000000000000000, 0.8660254037844387076, 1.000000000000000000, 0.8660254037844387076, 1.000000000000000000, 0.8660254037844387076, 1.000000000000000000, 0.8660254037844387076, 1.000000000000000000, 0.8660254037844387076, 1.000000000000000000, 0.8660254037844387076, 1.000000000000000000, 0.8660254037844387076, 1.000000000000000000, 0.8660254037844387076, 1.000000000000000000, 0.8660254037844387076, 1.000000000000000000, 0.8660254037844387076, 1.000000000000000000, 0.8660254037844387076, 1.000000000000000000, 0.8660254037844387076, 1.000000000000000000, 0.8660254037844387076, 1.000000000000000000, 0.8660254037844387076, 1.000000000000000000, 0.8660254037844387076, 1.000000000000000000, 0.8660254037844387076, 1.000000000000000000, 0.8660254037844387076, 1.000000000000000000, 0.8660254037844387076, 1.000000000000000000, 0.8660254037844387076, 1.000000000000000000, 0.8660254037844387076, 1.000000000000000000, 0.8660254037844387076, 1.000000000000000000, 0.8660254037844387076, 1.000000000000000000, 0.8660254037844387076, 1.000000000000000000, 0.8660254037844387076, 1.000000000000000000, 0.8660254037844387076, 1.000000000000000000, 0.8660254037844387076, 1.000000000000000000, 0.8660254037844387076, 1.000000000000000000, 0.8660254037844387076, 1.000000000000000000, 0.8660254037844387076, 1.000000000000000000, 0.8660254037844387076, 1.000000000000000000, 0.8660254037844387076, 1.000000000000000000, 0.8660254037844387076, 1.000000000000000000, 0.8660254037844387076, 1.000000000000000000, 0.8660254037844387076, 1.000000000000000000, 0.8660254037844387076, 1.000000000000000000, 0.8660254037844387076, 1.000000000000000000, 0.8660254037844387076, 1.000000000000000000, 0.8660254037844387076, 1.000000000000000000, 0.8660254037844387076, 1.000000000000000000, 0.8660254037844387076, 1.000000000000000000, 0.8660254037844387076, 1.000000000000000000, 0.8660254037844387076, 1.000000000000000000, 0.8660254037844387076, 1.000000000000000000, 0.8660254037844387076, 1.000000000000000000, 0.8660254037844387076, 1.000000000000000000, 0.8660254037844387076, 1.000000000000000000, 0.8660254037844387076, 1.000000000000000000, 0.8660254037844387076, 1.000000000000000000, 0.8660254037844387076, 1.000000000000000000, 0.8660254037844387076, 1.000000000000000000, 0.8660254037844387076, 1.000000000000000000, 0.8660254037844387076, 1.000000000000000000, 0.8660254037844387076, 1.000000000000000000, 0.8660254037844387076, 1.000000000000000000, 0.8660254037844387076, 1.000000000000000000, 0.8660254037844387076, 1.000000000000000000, 0.8660254037844387076, 1.000000000000000000, 0.8660254037844387076, 1.000000000000000000, 0.8660254037844387076, 1.000000000000000000, 0.8660254037844387076, 1.000000000000000000, 0.8660254037844387076, 1.000000000000000000, 0.8660254037844387076, 1.000000000000000000, 0.8660254037844387076, 1.000000000000000000, 0.8660254037844387076, 1.000000000000000000, 0.8660254037844387076, 1.000000000000000000, 0.8660254037844387076, 1.000000000000000000, 0.8660254037844387076, 1.000000000000000000, 0.8660254037844387076, 1.000000000000000000, 0.8660254037844387076, 1.000000000000000000, 0.8660254037844387076, 1.000000000000000000, 0.8660254037844387076, 1.000000000000000000, 0.8660254037844387076, 1.000000000000000000, 0.8660254037844387076, 1.000000000000000000, 0.8660254037844387076, 1.000000000000000000, 0.8660254037844387076, 1.000000000000000000, 0.8660254037844387076, 1.000000000000000000, 0.8660254037844387076, 1.000000000000000000, 0.8660254037844387076, 1.000000000000000000, 0.8660254037844387076, 1.000000000000000000, 0.8660254037844387076, 1.000000000000000000, 0.8660254037844387076, 1.000000000000000000, 0.8660254037844387076, 1.000000000000000000, 0.8660254037844387076, 1.000000000000000000, 0.8660254037844387076, 1.000000000000000000, 0.8660254037844387076, 1.000000000000000000, 0.8660254037844387076, 1.000000000000000000, 0.8660254037844387076, 1.000000000000000000, 0.8660254037844387076, 1.000000000000000000, 0.8660254037844387076, 1.000000000000000000, 0.8660254037844387076, 1.000000000000000000, 0.8660254037844387076, 1.000000000000000000, 0.8660254037844387076, 1.000000000000000000, 0.8660254037844387076, 1.000000000000000000, 0.8660254037844387076, 1.000000000000000000, 0.8660254037844387076, 1.000000000000000000, 0.8660254037844387076, 1.000000000000000000, 0.8660254037844387076, 1.000000000000000000, 0.8660254037844387076, 1.000000000000000000, 0.8660254037844387076, 1.000000000000000000, 0.8660254037844387076, 1.000000000000000000, 0.8660254037844387076, 1.000000000000000000, 0.8660254037844387076, 1.000000000000000000, 0.8660254037844387076, 1.000000000000000000, 0.8660254037844387076, 1.000000000000000000, 0.8660254037844387076, 1.000000000000000000, 0.8660254037844387076, 1.000000000000000000, 0.8660254037844387076, 1.000000000000000000, 0.8660254037844387076, 1.000000000000000000, 0.8660254037844387076, 1.000000000000000000, 0.8660254037844387076, 1.000000000000000000, 0.8660254037844387076, 1.000000000000000000, 0.8660254037844387076, 1.000000000000000000, 0.8660254037844387076, 1.000000000000000000, 0.8660254037844387076, 1.000000000000000000, 0.8660254037844387076, 1.000000000000000000, 0.8660254037844387076, 1.000000000000000000, 0.8660254037844387076, 1.000000000000000000, 0.8660254037844387076, 1.000000000000000000, 0.8660254037844387076, 1.000000000000000000, 0.8660254037844387076, 1.000000000000000000, 0.8660254037844387076, 1.000000000000000000, 0.8660254037844387076, 1.000000000000000000, 0.8660254037844387076, 1.000000000000000000, 0.8660254037844387076, 1.000000000000000000, 0.8660254037844387076, 1.000000000000000000) ) ) 
 REPRESENTATION_ITEM ( '' )  SURFACE ( )  );
#30818 = CARTESIAN_POINT ( 'NONE',  ( -4.999999999999996447, 8.660254037844387298, -79.87500000409677625 ) ) ;
#30819 = CARTESIAN_POINT ( 'NONE',  ( 9.999999999999998224, 0.000000000000000000, -119.0000000000000000 ) ) ;
#30820 = CARTESIAN_POINT ( 'NONE',  ( 5.405949406249999534, 9.363379034771803333, -37.09375000204836681 ) ) ;
#30821 = EDGE_LOOP ( 'NONE', ( #27201, #6775, #8335, #30874 ) ) ;
#30822 = CARTESIAN_POINT ( 'NONE',  ( 10.00000000000000000, 5.773502691896255534, -4.874999999999959144 ) ) ;
#30823 = CARTESIAN_POINT ( 'NONE',  ( -10.81189881249999729, 1.324075727343319199E-15, -30.78125000204837036 ) ) ;
#30824 = CARTESIAN_POINT ( 'NONE',  ( -5.405949406250003975, -9.363379034771801557, -10.84375000204834727 ) ) ;
#30825 = DIRECTION ( 'NONE',  ( 1.000000000000000000, 0.000000000000000000, 0.000000000000000000 ) ) ;
#30826 = CARTESIAN_POINT ( 'NONE',  ( -9.999999999999998224, 5.773502691896259087, -0.2500000040967509385 ) ) ;
#30827 = CARTESIAN_POINT ( 'NONE',  ( 5.405949406249999534, 9.363379034771803333, -131.7812500020483810 ) ) ;
#30828 = CARTESIAN_POINT ( 'NONE',  ( 9.999999999999996447, -5.773502691896262640, -186.6250000000000284 ) ) ;
#30829 = CARTESIAN_POINT ( 'NONE',  ( -4.999999999999996447, 8.660254037844387298, -120.0000000000000000 ) ) ;
#30831 = VERTEX_POINT ( 'NONE', #32650 ) ;
#30830 = CARTESIAN_POINT ( 'NONE',  ( 7.644554776091147741E-16, 12.48450537969573659, -107.6562500020483810 ) ) ;
#30832 = CARTESIAN_POINT ( 'NONE',  ( 7.070501591499376803E-16, 11.54700538379251284, -138.5000000040967905 ) ) ;
#30833 = ORIENTED_EDGE ( 'NONE', *, *, #23858, .F. ) ;
#30834 = ORIENTED_EDGE ( 'NONE', *, *, #10646, .T. ) ;
#30835 = EDGE_CURVE ( 'NONE', #33047, #32122, #26587, .T. ) ;
#30836 = CARTESIAN_POINT ( 'NONE',  ( 10.81189881249999551, -6.242252689847874514, -39.15625000204835260 ) ) ;
#30837 = CALENDAR_DATE ( 2026, 28, 9 ) ;
#30838 = CARTESIAN_POINT ( 'NONE',  ( -10.81189881249999907, -6.242252689847864744, -90.46875000204836681 ) ) ;
#30839 = DIRECTION ( 'NONE',  ( -0.000000000000000000, -0.000000000000000000, -1.000000000000000000 ) ) ;
#30840 = CARTESIAN_POINT ( 'NONE',  ( -9.999999999999996447, 5.773502691896259975, -173.8750000000000000 ) ) ;
#30841 = CARTESIAN_POINT ( 'NONE',  ( 9.999999999999998224, 0.000000000000000000, -105.8750000040967763 ) ) ;
#30842 = CARTESIAN_POINT ( 'NONE',  ( -10.81189881249999729, 6.242252689847871849, -174.9062500020483810 ) ) ;
#30843 = LINE ( 'NONE', #7324, #20506 ) ;
#30844 = CARTESIAN_POINT ( 'NONE',  ( -10.81189881249999729, -6.242252689847864744, -121.9687500020484237 ) ) ;
#30845 = CARTESIAN_POINT ( 'NONE',  ( 5.405949406249999534, 9.363379034771803333, -95.59375000204838102 ) ) ;
#30846 = CARTESIAN_POINT ( 'NONE',  ( -10.81189881249999729, 1.324075727343319199E-15, -0.7812500020483725827 ) ) ;
#30847 = DIRECTION ( 'NONE',  ( 1.000000000000000000, 0.000000000000000000, 0.000000000000000000 ) ) ;
#30848 = CARTESIAN_POINT ( 'NONE',  ( 7.644554776091147741E-16, 12.48450537969573659, -101.6562500020483952 ) ) ;
#30849 = CARTESIAN_POINT ( 'NONE',  ( -9.999999999999998224, 1.224646799147353059E-15, -175.6250000040968189 ) ) ;
#30850 = CARTESIAN_POINT ( 'NONE',  ( 10.81189881249999729, 6.242252689847867408, -104.7187500020483810 ) ) ;
#30851 = CARTESIAN_POINT ( 'NONE',  ( 10.81189881249999729, 0.000000000000000000, -180.0312500020483810 ) ) ;
#30852 = EDGE_CURVE ( 'NONE', #11384, #26823, #12762, .T. ) ;
#30853 = CARTESIAN_POINT ( 'NONE',  ( 10.81189881249999907, 6.242252689847868297, -199.4062500020484094 ) ) ;
#30854 = CARTESIAN_POINT ( 'NONE',  ( -10.81189881249999729, 6.242252689847871849, -48.71875000204834549 ) ) ;
#30855 = ADVANCED_FACE ( 'NONE', ( #10172 ), #29407, .T. ) ;
#30856 = CARTESIAN_POINT ( 'NONE',  ( -10.00000000000000000, -5.773502691896251982, -169.5000000040967620 ) ) ;
#30857 = CARTESIAN_POINT ( 'NONE',  ( -10.81189881249999907, -6.242252689847864744, -14.15625000204836859 ) ) ;
#30858 = CARTESIAN_POINT ( 'NONE',  ( 7.644554776091147741E-16, 12.48450537969573659, -20.46875000204837036 ) ) ;
#30859 = CYLINDRICAL_SURFACE ( 'NONE', #37831, 9.999999999999998224 ) ;
#30860 = CARTESIAN_POINT ( 'NONE',  ( 10.81189881249999907, 6.242252689847868297, -127.2187500020483668 ) ) ;
#30861 = CARTESIAN_POINT ( 'NONE',  ( -4.999999999999996447, 8.660254037844387298, -95.99999999999998579 ) ) ;
#30862 = CARTESIAN_POINT ( 'NONE',  ( -2.293366432827344421E-15, -12.48450537969573659, -30.40625000204835615 ) ) ;
#30863 = CARTESIAN_POINT ( 'NONE',  ( 10.00000000000000000, 5.773502691896255534, -102.7500000040967905 ) ) ;
#30864 = CARTESIAN_POINT ( 'NONE',  ( 4.999999999999992006, -8.660254037844389075, -168.7500000000000000 ) ) ;
#30865 = CARTESIAN_POINT ( 'NONE',  ( -10.00000000000000000, -5.773502691896251982, -62.62499999999997868 ) ) ;
#30866 = CARTESIAN_POINT ( 'NONE',  ( 10.81189881249999729, 0.000000000000000000, -123.0312500020483952 ) ) ;
#30867 = CARTESIAN_POINT ( 'NONE',  ( -2.293366432827344421E-15, -12.48450537969573659, -106.9062500020483810 ) ) ;
#30868 = VERTEX_POINT ( 'NONE', #42126 ) ;
#30869 = CARTESIAN_POINT ( 'NONE',  ( -9.999999999999998224, 1.224646799147353059E-15, -118.2500000000000000 ) ) ;
#30870 = CARTESIAN_POINT ( 'NONE',  ( 9.999999999999996447, -5.773502691896262640, -98.50000000409677625 ) ) ;
#30871 = CARTESIAN_POINT ( 'NONE',  ( -1.040834085586084257E-14, -145.0000000000000000, 22.49999999999999289 ) ) ;
#30872 = CARTESIAN_POINT ( 'NONE',  ( -5.405949406249996869, 9.363379034771805109, -163.0312500020484094 ) ) ;
#30873 = CARTESIAN_POINT ( 'NONE',  ( -5.405949406249996869, 9.363379034771805109, -60.84375000204836681 ) ) ;
#30874 = ORIENTED_EDGE ( 'NONE', *, *, #18202, .F. ) ;
#30875 = CARTESIAN_POINT ( 'NONE',  ( -9.999999999999998224, 1.224646799147353059E-15, -25.24999999999996803 ) ) ;
#30876 = VECTOR ( 'NONE', #12248, 1000.000000000000000 ) ;
#30877 = CARTESIAN_POINT ( 'NONE',  ( 10.81189881249999551, -6.242252689847874514, -34.65625000204836681 ) ) ;
#30878 = CARTESIAN_POINT ( 'NONE',  ( 5.000000000000000000, 8.660254037844385522, -160.7500000000000000 ) ) ;
#30879 = CIRCLE ( 'NONE', #29512, 45.00000000000000711 ) ;
#30880 = CARTESIAN_POINT ( 'NONE',  ( -9.999999999999998224, 1.224646799147353059E-15, -200.0000000000000000 ) ) ;
#30881 = CARTESIAN_POINT ( 'NONE',  ( -5.000000000000003553, -8.660254037844383745, -25.37500000409675849 ) ) ;
#30882 = CARTESIAN_POINT ( 'NONE',  ( -10.81189881249999729, 1.324075727343319199E-15, -131.2812500020483810 ) ) ;
#30883 = CARTESIAN_POINT ( 'NONE',  ( 79.99999999999998579, -40.00000000000001421, -170.0000000000000000 ) ) ;
#30884 = ORIENTED_EDGE ( 'NONE', *, *, #12475, .T. ) ;
#30885 = ADVANCED_FACE ( 'NONE', ( #35677 ), #39105, .T. ) ;
#30887 = ORIENTED_EDGE ( 'NONE', *, *, #11956, .T. ) ;
#30886 = ORIENTED_EDGE ( 'NONE', *, *, #26939, .T. ) ;
#30888 = CARTESIAN_POINT ( 'NONE',  ( -9.999999999999998224, 1.224646799147353059E-15, -46.62500000409677625 ) ) ;
#30889 = CARTESIAN_POINT ( 'NONE',  ( -9.999999999999479527, -5.773502691896549521, -147.0000000040967620 ) ) ;
#30890 = CARTESIAN_POINT ( 'NONE',  ( -5.405949406249996869, 9.363379034771805109, -162.8437500020484094 ) ) ;
#30891 = CARTESIAN_POINT ( 'NONE',  ( -5.405949406249996869, 9.363379034771805109, -194.5312500020484094 ) ) ;
#30892 = CARTESIAN_POINT ( 'NONE',  ( -5.405949406250003975, -9.363379034771801557, -13.84375000204834905 ) ) ;
#30893 = DIRECTION ( 'NONE',  ( -0.6123724356957964687, 0.3535533905932747301, 0.7071067811865454633 ) ) ;
#30894 = AXIS2_PLACEMENT_3D ( 'NONE', #18678, #2714, #32290 ) ;
#30895 = CARTESIAN_POINT ( 'NONE',  ( -10.81189881249999729, -6.242252689847864744, -151.9687500020484094 ) ) ;
#30896 = VECTOR ( 'NONE', #35316, 1000.000000000000000 ) ;
#30897 = CARTESIAN_POINT ( 'NONE',  ( 10.81189881249999907, 6.242252689847868297, -134.7187500020484094 ) ) ;
#30898 =( BOUNDED_CURVE ( )  B_SPLINE_CURVE ( 2, ( #19475, #3090, #19898, #23370, #3509, #3302, #13407 ),
 .UNSPECIFIED., .F., .F. ) 
 B_SPLINE_CURVE_WITH_KNOTS ( ( 3, 2, 2, 3 ),
 ( 0.4925373134328359104, 0.4937810945273632957, 0.4950248756218906809, 0.4962686567164180107 ),
 .UNSPECIFIED. ) 
 CURVE ( )  GEOMETRIC_REPRESENTATION_ITEM ( )  RATIONAL_B_SPLINE_CURVE ( ( 0.9999999999999880096, 0.8660254037844506980, 1.000000000000000000, 0.8660254037844387076, 1.000000000000000000, 0.8660254037844267172, 1.000000000000011990 ) ) 
 REPRESENTATION_ITEM ( '' )  );
#30899 = CARTESIAN_POINT ( 'NONE',  ( -5.405949406249996869, 9.363379034771805109, -109.0312500020483810 ) ) ;
#30900 = CARTESIAN_POINT ( 'NONE',  ( -10.81189881249999729, 1.324075727343319199E-15, -114.5937500020483810 ) ) ;
#30901 = CARTESIAN_POINT ( 'NONE',  ( -10.00000000000000000, -5.773502691896251982, -195.0000000040967905 ) ) ;
#30902 = CARTESIAN_POINT ( 'NONE',  ( -10.81189881249999907, -6.242252689847864744, -126.6562500020483810 ) ) ;
#30903 = CARTESIAN_POINT ( 'NONE',  ( -9.999999999999998224, 5.773502691896259087, -198.2500000040968189 ) ) ;
#30904 = CARTESIAN_POINT ( 'NONE',  ( -10.81189881249999729, 1.324075727343319199E-15, -129.5937500020483810 ) ) ;
#30905 = CARTESIAN_POINT ( 'NONE',  ( 10.00000000000154010, -5.773502691895370020, -54.62499999999992895 ) ) ;
#30906 = PLANE ( 'NONE',  #30303 ) ;
#30907 = CARTESIAN_POINT ( 'NONE',  ( 10.00000000000000000, 5.773502691896255534, -145.8750000000000284 ) ) ;
#30908 = CARTESIAN_POINT ( 'NONE',  ( 9.999999999999998224, 0.000000000000000000, -24.49999999999996447 ) ) ;
#30909 = CARTESIAN_POINT ( 'NONE',  ( -10.81189881249999729, 6.242252689847871849, -75.71875000204838102 ) ) ;
#30910 = CARTESIAN_POINT ( 'NONE',  ( 10.81189881249999551, -6.242252689847874514, -68.96875000204839523 ) ) ;
#30911 = CARTESIAN_POINT ( 'NONE',  ( 4.999999999999992006, -8.660254037844389075, -19.12500000409675494 ) ) ;
#30912 = CARTESIAN_POINT ( 'NONE',  ( -5.405949406250003975, -9.363379034771801557, -32.03125000204837391 ) ) ;
#30913 = CARTESIAN_POINT ( 'NONE',  ( 7.644554776091147741E-16, 12.48450537969573659, -44.46875000204836681 ) ) ;
#30914 = CARTESIAN_POINT ( 'NONE',  ( -9.999999999999998224, 1.224646799147353059E-15, -151.2500000000000000 ) ) ;
#30915 = CARTESIAN_POINT ( 'NONE',  ( -10.81189881249999907, -6.242252689847864744, -157.9687500020484379 ) ) ;
#30916 = CARTESIAN_POINT ( 'NONE',  ( -4.999999999999996447, 8.660254037844387298, -120.0000000000000000 ) ) ;
#30917 = CARTESIAN_POINT ( 'NONE',  ( 7.644554776091147741E-16, 12.48450537969573659, -128.6562500020483810 ) ) ;
#30918 = CARTESIAN_POINT ( 'NONE',  ( 4.366535267995796055, 9.446561771012207842, -179.9999999999999147 ) ) ;
#30919 = CARTESIAN_POINT ( 'NONE',  ( -2.121150477449813534E-15, -11.54700538379251284, -80.37499999999997158 ) ) ;
#30920 = CARTESIAN_POINT ( 'NONE',  ( -5.405949406249996869, 9.363379034771805109, -17.53125000204835970 ) ) ;
#30921 = VERTEX_POINT ( 'NONE', #9544 ) ;
#30922 = CARTESIAN_POINT ( 'NONE',  ( 5.405949406249992428, -9.363379034771808662, -102.2812500020483952 ) ) ;
#30923 = CARTESIAN_POINT ( 'NONE',  ( -5.000000000000003553, -8.660254037844383745, -121.3750000040967905 ) ) ;
#30924 = CARTESIAN_POINT ( 'NONE',  ( 4.999999999999992006, -8.660254037844389075, -179.6250000040968189 ) ) ;
#30925 = CARTESIAN_POINT ( 'NONE',  ( 9.999999999999996447, -5.773502691896262640, -34.00000000409674783 ) ) ;
#30926 = DIRECTION ( 'NONE',  ( 1.000000000000000000, 0.000000000000000000, 0.000000000000000000 ) ) ;
#30927 = CARTESIAN_POINT ( 'NONE',  ( -2.293366432827344421E-15, -12.48450537969573659, -45.40625000204837391 ) ) ;
#30928 = CARTESIAN_POINT ( 'NONE',  ( 9.999999999999998224, 0.000000000000000000, -147.5000000000000000 ) ) ;
#30929 = CARTESIAN_POINT ( 'NONE',  ( 5.405949406249992428, -9.363379034771808662, -153.2812500020484094 ) ) ;
#30930 = CARTESIAN_POINT ( 'NONE',  ( -10.81189881249999729, 6.242252689847871849, -125.2187500020483810 ) ) ;
#30931 = CARTESIAN_POINT ( 'NONE',  ( 7.070501591499376803E-16, 11.54700538379251284, -190.6250000000000284 ) ) ;
#30932 = AXIS2_PLACEMENT_3D ( 'NONE', #31352, #4789, #1782 ) ;
#30933 = ORIENTED_EDGE ( 'NONE', *, *, #20943, .F. ) ;
#30934 = CARTESIAN_POINT ( 'NONE',  ( -10.00000000000102496, 5.773502691895664007, -22.37499999999994671 ) ) ;
#30935 = ORIENTED_EDGE ( 'NONE', *, *, #24533, .T. ) ;
#30936 = ORIENTED_EDGE ( 'NONE', *, *, #18251, .T. ) ;
#30937 = EDGE_CURVE ( 'NONE', #2019, #12962, #17173, .T. ) ;
#30939 = ORIENTED_EDGE ( 'NONE', *, *, #11435, .T. ) ;
#30938 = CARTESIAN_POINT ( 'NONE',  ( -10.81189881249999729, 6.242252689847871849, -108.7187500020483810 ) ) ;
#30940 = EDGE_CURVE ( 'NONE', #7682, #10798, #1278, .T. ) ;
#30941 = EDGE_CURVE ( 'NONE', #33014, #30027, #4938, .T. ) ;
#30942 = LINE ( 'NONE', #20999, #36187 ) ;
#30943 =( BOUNDED_CURVE ( )  B_SPLINE_CURVE ( 2, ( #26065, #36191, #36405, #16530, #13503, #3615, #13711 ),
 .UNSPECIFIED., .F., .F. ) 
 B_SPLINE_CURVE_WITH_KNOTS ( ( 3, 2, 2, 3 ),
 ( 0.4701492537313434195, 0.4713930348258707492, 0.4726368159203981900, 0.4738805970149255198 ),
 .UNSPECIFIED. ) 
 CURVE ( )  GEOMETRIC_REPRESENTATION_ITEM ( )  RATIONAL_B_SPLINE_CURVE ( ( 0.9999999999999880096, 0.8660254037844506980, 1.000000000000000000, 0.8660254037844387076, 1.000000000000000000, 0.8660254037844207220, 1.000000000000017986 ) ) 
 REPRESENTATION_ITEM ( '' )  );
#30944 = CARTESIAN_POINT ( 'NONE',  ( -5.405949406249996869, 9.363379034771805109, -186.8437500020483810 ) ) ;
#30945 = CARTESIAN_POINT ( 'NONE',  ( -5.405949406249996869, 9.363379034771805109, -38.34375000204837391 ) ) ;
#30946 = CARTESIAN_POINT ( 'NONE',  ( 6.419290871637174156, -8.565826599455219181, 3.494387113477268989E-15 ) ) ;
#30947 = CARTESIAN_POINT ( 'NONE',  ( -9.999999999999479527, -5.773502691896549521, -74.62499999999994316 ) ) ;
#30948 = CARTESIAN_POINT ( 'NONE',  ( -10.81189881249999729, 1.324075727343319199E-15, -168.5937500020484094 ) ) ;
#30949 = CARTESIAN_POINT ( 'NONE',  ( -10.81189881249999729, 6.242252689847871849, -162.7187500020483810 ) ) ;
#30950 = APPROVAL ( #12657, 'UNKNOWN' ) ;
#30951 = CARTESIAN_POINT ( 'NONE',  ( 9.999999999999479527, 5.773502691896553074, -178.8749999999999716 ) ) ;
#30952 = CARTESIAN_POINT ( 'NONE',  ( 10.81189881249999551, -6.242252689847874514, -143.9687500020483810 ) ) ;
#30953 = CARTESIAN_POINT ( 'NONE',  ( -2.293366432827344421E-15, -12.48450537969573659, -151.9062500020483810 ) ) ;
#30954 = CARTESIAN_POINT ( 'NONE',  ( -10.81189881249999729, 6.242252689847871849, -155.2187500020483810 ) ) ;
#30955 = CARTESIAN_POINT ( 'NONE',  ( -9.999999999999998224, 1.224646799147353059E-15, -58.24999999999997158 ) ) ;
#30956 =( BOUNDED_CURVE ( )  B_SPLINE_CURVE ( 2, ( #21160, #4343, #41435, #8229, #24428, #14890, #17914 ),
 .UNSPECIFIED., .F., .F. ) 
 B_SPLINE_CURVE_WITH_KNOTS ( ( 3, 2, 2, 3 ),
 ( 0.3917910447761194792, 0.3930348258706468090, 0.3942786069651742498, 0.3955223880597015795 ),
 .UNSPECIFIED. ) 
 CURVE ( )  GEOMETRIC_REPRESENTATION_ITEM ( )  RATIONAL_B_SPLINE_CURVE ( ( 0.9999999999999940048, 0.8660254037844447028, 1.000000000000000000, 0.8660254037844387076, 1.000000000000000000, 0.8660254037844267172, 1.000000000000011990 ) ) 
 REPRESENTATION_ITEM ( '' )  );
#30957 = CARTESIAN_POINT ( 'NONE',  ( -10.00000000000051337, 5.773502691895962435, -102.2500000040967905 ) ) ;
#30958 = CARTESIAN_POINT ( 'NONE',  ( -5.000000000000003553, -8.660254037844383745, -179.5000000000000000 ) ) ;
#30959 = CARTESIAN_POINT ( 'NONE',  ( 10.81189881249999907, 6.242252689847868297, -85.21875000204836681 ) ) ;
#30960 = CARTESIAN_POINT ( 'NONE',  ( 9.999999999999998224, 0.000000000000000000, -135.5000000000000000 ) ) ;
#30961 = CARTESIAN_POINT ( 'NONE',  ( 5.405949406249999534, 9.363379034771803333, -59.78125000204836681 ) ) ;
#30962 = DIRECTION ( 'NONE',  ( 0.000000000000000000, 1.000000000000000000, 0.000000000000000000 ) ) ;
#30963 = CARTESIAN_POINT ( 'NONE',  ( -2.293366432827344421E-15, -12.48450537969573659, -178.7187500020484094 ) ) ;
#30964 = EDGE_CURVE ( 'NONE', #5198, #5513, #1711, .T. ) ;
#30965 = CARTESIAN_POINT ( 'NONE',  ( -2.293366432827344421E-15, -12.48450537969573659, -117.4062500020483952 ) ) ;
#30966 = VECTOR ( 'NONE', #26218, 1000.000000000000000 ) ;
#30967 = CARTESIAN_POINT ( 'NONE',  ( 10.81189881249999729, 0.000000000000000000, -157.5312500020484094 ) ) ;
#30968 = CYLINDRICAL_SURFACE ( 'NONE', #13044, 9.999999999999998224 ) ;
#30969 = CARTESIAN_POINT ( 'NONE',  ( 7.644554776091147741E-16, 12.48450537969573659, -44.65625000204836681 ) ) ;
#30970 = CARTESIAN_POINT ( 'NONE',  ( 9.999999999999998224, 0.000000000000000000, -129.8750000040967905 ) ) ;
#30971 = CARTESIAN_POINT ( 'NONE',  ( -9.999999999999998224, 1.224646799147353059E-15, -107.7499999999999858 ) ) ;
#30972 = VERTEX_POINT ( 'NONE', #16847 ) ;
#30973 = CARTESIAN_POINT ( 'NONE',  ( 10.81189881249999729, 6.242252689847867408, -127.4062500020483810 ) ) ;
#30974 = CARTESIAN_POINT ( 'NONE',  ( -10.00000000000000000, -5.773502691896251982, -147.0000000040967905 ) ) ;
#30975 = CARTESIAN_POINT ( 'NONE',  ( -9.999999999999998224, 1.224646799147353059E-15, -200.0000000000000000 ) ) ;
#30976 = EDGE_CURVE ( 'NONE', #24961, #9954, #21613, .T. ) ;
#30977 = CARTESIAN_POINT ( 'NONE',  ( -2.293366432827344421E-15, -12.48450537969573659, -183.4062500020483810 ) ) ;
#30978 = ORIENTED_EDGE ( 'NONE', *, *, #41370, .F. ) ;
#30979 = CARTESIAN_POINT ( 'NONE',  ( 5.000000000000000000, 8.660254037844385522, -52.74999999999996447 ) ) ;
#30980 = CARTESIAN_POINT ( 'NONE',  ( 5.405949406249999534, 9.363379034771803333, -175.0937500020484094 ) ) ;
#30981 = CARTESIAN_POINT ( 'NONE',  ( -2.121150477449813534E-15, -11.54700538379251284, -55.25000000409678336 ) ) ;
#30982 = EDGE_CURVE ( 'NONE', #17741, #28218, #26027, .T. ) ;
#30983 = CARTESIAN_POINT ( 'NONE',  ( -31.99999999999997158, 3.918869757271527108E-15, -180.0000000000000000 ) ) ;
#30984 = CARTESIAN_POINT ( 'NONE',  ( -9.999999999999998224, 1.224646799147353059E-15, -171.1250000040968189 ) ) ;
#30985 = CARTESIAN_POINT ( 'NONE',  ( 10.81189881249999729, 0.000000000000000000, -64.53125000204836681 ) ) ;
#30986 = CARTESIAN_POINT ( 'NONE',  ( 10.81189881249999551, -6.242252689847874514, -52.65625000204836681 ) ) ;
#30987 = CARTESIAN_POINT ( 'NONE',  ( 10.00000000000000000, 5.773502691896255534, -53.25000000409676915 ) ) ;
#30988 = AXIS2_PLACEMENT_3D ( 'NONE', #23099, #36261, #2827 ) ;
#30989 = CARTESIAN_POINT ( 'NONE',  ( 10.81189881249999729, 0.000000000000000000, -4.343750002048368586 ) ) ;
#30990 = CARTESIAN_POINT ( 'NONE',  ( 10.00000000000154010, -5.773502691895370020, -29.50000000409671586 ) ) ;
#30991 = CARTESIAN_POINT ( 'NONE',  ( -10.81189881249999729, 1.324075727343319199E-15, -177.7812500020484094 ) ) ;
#30992 = CARTESIAN_POINT ( 'NONE',  ( -9.999999999999998224, 1.224646799147353059E-15, -200.0000000000000000 ) ) ;
#30993 = CARTESIAN_POINT ( 'NONE',  ( 9.999999999999966249, 5.773502691896273298, -198.3750000000000284 ) ) ;
#30994 = ADVANCED_FACE ( 'NONE', ( #40741 ), #28035, .T. ) ;
#30995 = CARTESIAN_POINT ( 'NONE',  ( 80.00000000000002842, -20.00000000000001421, -160.0000000000000000 ) ) ;
#30996 = DIRECTION ( 'NONE',  ( -0.000000000000000000, -0.000000000000000000, -1.000000000000000000 ) ) ;
#30998 = ORIENTED_EDGE ( 'NONE', *, *, #25847, .T. ) ;
#30997 = CARTESIAN_POINT ( 'NONE',  ( -10.81189881249999729, 1.324075727343319199E-15, -89.28125000204838102 ) ) ;
#31000 = ORIENTED_EDGE ( 'NONE', *, *, #8579, .F. ) ;
#30999 = CARTESIAN_POINT ( 'NONE',  ( -4.999999999999996447, 8.660254037844387298, -91.87500000409677625 ) ) ;
#31001 = EDGE_LOOP ( 'NONE', ( #14656, #9491, #42149, #23134 ) ) ;
#31002 = EDGE_CURVE ( 'NONE', #19501, #3609, #25781, .T. ) ;
#31003 = CARTESIAN_POINT ( 'NONE',  ( 5.405949406249999534, 9.363379034771803333, -34.09375000204836681 ) ) ;
#31004 = CARTESIAN_POINT ( 'NONE',  ( -10.81189881249999729, 6.242252689847871849, -26.21875000204837391 ) ) ;
#31005 = CARTESIAN_POINT ( 'NONE',  ( 10.81189881249999729, 0.000000000000000000, -13.53125000204835615 ) ) ;
#31006 = CARTESIAN_POINT ( 'NONE',  ( -10.81189881249999729, 1.324075727343319199E-15, -62.09375000204836681 ) ) ;
#31007 = FACE_OUTER_BOUND ( 'NONE', #26873, .T. ) ;
#31008 = CARTESIAN_POINT ( 'NONE',  ( 7.070501591499377789E-16, 11.54700538379251284, -45.12499999999997158 ) ) ;
#31009 = CARTESIAN_POINT ( 'NONE',  ( -2.293366432827344421E-15, -12.48450537969573659, -183.2187500020484094 ) ) ;
#31010 = CARTESIAN_POINT ( 'NONE',  ( -10.81189881249999907, -6.242252689847864744, -162.4687500020483526 ) ) ;
#31011 = CARTESIAN_POINT ( 'NONE',  ( -5.405949406250003975, -9.363379034771801557, -177.3437500020483810 ) ) ;
#31012 = CARTESIAN_POINT ( 'NONE',  ( 9.999999999999998224, 1.224646799147353059E-15, -99.99999999999998579 ) ) ;
#31013 = FACE_OUTER_BOUND ( 'NONE', #17626, .T. ) ;
#31014 = CARTESIAN_POINT ( 'NONE',  ( 0.000000000000000000, 0.000000000000000000, -200.0000000000000000 ) ) ;
#31015 = CYLINDRICAL_SURFACE ( 'NONE', #17743, 9.999999999999998224 ) ;
#31016 = CARTESIAN_POINT ( 'NONE',  ( 10.81189881249999729, 0.000000000000000000, -110.8437500020483810 ) ) ;
#31017 = CARTESIAN_POINT ( 'NONE',  ( -9.999999999999998224, 1.224646799147353059E-15, -191.7500000000000000 ) ) ;
#31018 = CARTESIAN_POINT ( 'NONE',  ( 10.81189881249999729, 0.000000000000000000, -85.53125000204838102 ) ) ;
#31019 = CARTESIAN_POINT ( 'NONE',  ( 10.81189881249999729, 0.000000000000000000, -97.34375000204838102 ) ) ;
#31020 = CARTESIAN_POINT ( 'NONE',  ( 5.405949406249992428, -9.363379034771808662, -60.09375000204835970 ) ) ;
#31021 = CARTESIAN_POINT ( 'NONE',  ( -10.81189881249999907, -6.242252689847864744, -69.65625000204839523 ) ) ;
#31022 = CARTESIAN_POINT ( 'NONE',  ( -9.999999999999998224, 5.773502691896259087, -156.2500000040967905 ) ) ;
#31023 = CARTESIAN_POINT ( 'NONE',  ( 9.999999999999998224, 0.000000000000000000, -134.0000000000000000 ) ) ;
#31024 = EDGE_CURVE ( 'NONE', #40566, #587, #24380, .T. ) ;
#31025 = CARTESIAN_POINT ( 'NONE',  ( -10.81189881249999729, -6.242252689847864744, -149.1562500020484094 ) ) ;
#31026 = CARTESIAN_POINT ( 'NONE',  ( 10.81189881249999907, 6.242252689847868297, -167.9062500020484094 ) ) ;
#31027 = PLANE ( 'NONE',  #2020 ) ;
#31028 = CARTESIAN_POINT ( 'NONE',  ( -9.999999999999998224, 1.224646799147353059E-15, -159.1250000040967905 ) ) ;
#31029 = CARTESIAN_POINT ( 'NONE',  ( -10.81189881249999729, 6.242252689847871849, -101.2187500020483810 ) ) ;
#31030 = CARTESIAN_POINT ( 'NONE',  ( -5.000000000000003553, -8.660254037844383745, -74.49999999999998579 ) ) ;
#31031 = CARTESIAN_POINT ( 'NONE',  ( 10.81189881249999729, 0.000000000000000000, -6.031250002048377468 ) ) ;
#31032 = CARTESIAN_POINT ( 'NONE',  ( 7.070501591499377789E-16, 11.54700538379251284, -83.00000000409677625 ) ) ;
#31033 =( BOUNDED_CURVE ( )  B_SPLINE_CURVE ( 2, ( #36219, #6028, #2791, #29537, #22422, #12682, #6867 ),
 .UNSPECIFIED., .F., .F. ) 
 B_SPLINE_CURVE_WITH_KNOTS ( ( 3, 2, 2, 3 ),
 ( 0.2388059701492538378, 0.2400497512437811953, 0.2412935323383085806, 0.2425373134328359381 ),
 .UNSPECIFIED. ) 
 CURVE ( )  GEOMETRIC_REPRESENTATION_ITEM ( )  RATIONAL_B_SPLINE_CURVE ( ( 0.9999999999999880096, 0.8660254037844506980, 1.000000000000000000, 0.8660254037844387076, 1.000000000000000000, 0.8660254037844267172, 1.000000000000011990 ) ) 
 REPRESENTATION_ITEM ( '' )  );
#31034 = CARTESIAN_POINT ( 'NONE',  ( 9.999999999999998224, 0.000000000000000000, -26.37500000409676204 ) ) ;
#31035 = CARTESIAN_POINT ( 'NONE',  ( -5.405949406249996869, 9.363379034771805109, -100.0312500020483952 ) ) ;
#31036 = CARTESIAN_POINT ( 'NONE',  ( 5.405949406249999534, 9.363379034771803333, -74.78125000204838102 ) ) ;
#31037 = CARTESIAN_POINT ( 'NONE',  ( -9.999999999999998224, 5.773502691896259087, -79.75000000409677625 ) ) ;
#31038 = CARTESIAN_POINT ( 'NONE',  ( -10.00000000000154188, 5.773502691895366468, -19.37499999999993960 ) ) ;
#31039 = CARTESIAN_POINT ( 'NONE',  ( -10.81189881249999907, -6.242252689847864744, -33.46875000204835260 ) ) ;
#31040 = VERTEX_POINT ( 'NONE', #41385 ) ;
#31041 = CARTESIAN_POINT ( 'NONE',  ( 10.81189881249999907, 6.242252689847868297, -199.4062500020484094 ) ) ;
#31042 = AXIS2_PLACEMENT_3D ( 'NONE', #3652, #27368, #26937 ) ;
#31043 = CARTESIAN_POINT ( 'NONE',  ( -10.81189881249999907, -6.242252689847864744, -27.65625000204838457 ) ) ;
#31044 = CARTESIAN_POINT ( 'NONE',  ( -5.405949406249996869, 9.363379034771805109, -11.34375000204834727 ) ) ;
#31045 = CARTESIAN_POINT ( 'NONE',  ( -10.00000000000019185, -5.773502691896140071, -177.0000000040967620 ) ) ;
#31046 = CARTESIAN_POINT ( 'NONE',  ( 7.070501591499377789E-16, 11.54700538379251284, -6.500000004096756712 ) ) ;
#31047 = CARTESIAN_POINT ( 'NONE',  ( 10.81189881249999551, -6.242252689847874514, -127.6562500020483952 ) ) ;
#31048 = CARTESIAN_POINT ( 'NONE',  ( -4.999999999999996447, 8.660254037844387298, -183.0000000000000000 ) ) ;
#31049 = CARTESIAN_POINT ( 'NONE',  ( 9.999999999999998224, 0.000000000000000000, -1.999999999999974021 ) ) ;
#31051 = ORIENTED_EDGE ( 'NONE', *, *, #22754, .F. ) ;
#31050 = CARTESIAN_POINT ( 'NONE',  ( 10.81189881249999907, 6.242252689847868297, -112.4062500020483952 ) ) ;
#31052 = CYLINDRICAL_SURFACE ( 'NONE', #26215, 9.999999999999998224 ) ;
#31053 = VERTEX_POINT ( 'NONE', #4716 ) ;
#31054 = VERTEX_POINT ( 'NONE', #11821 ) ;
#31055 = CARTESIAN_POINT ( 'NONE',  ( -5.405949406250003975, -9.363379034771801557, -38.03125000204838102 ) ) ;
#31056 = PERSON_AND_ORGANIZATION ( #11915, #17965 ) ;
#31057 = CARTESIAN_POINT ( 'NONE',  ( -2.293366432827344421E-15, -12.48450537969573659, -84.21875000204835260 ) ) ;
#31058 = CARTESIAN_POINT ( 'NONE',  ( -9.999999999999998224, 0.000000000000000000, -99.99999999999998579 ) ) ;
#31059 = CARTESIAN_POINT ( 'NONE',  ( 10.00000000000076916, -5.773502691895816774, -108.6249999999999858 ) ) ;
#31060 = CARTESIAN_POINT ( 'NONE',  ( 10.81189881249999907, 6.242252689847868297, -164.9062500020484094 ) ) ;
#31061 = CARTESIAN_POINT ( 'NONE',  ( 9.999999999998456346, 5.773502691897149042, -54.75000000409674783 ) ) ;
#31062 = VECTOR ( 'NONE', #17372, 1000.000000000000000 ) ;
#31063 = EDGE_CURVE ( 'NONE', #15993, #4202, #11125, .T. ) ;
#31064 = CARTESIAN_POINT ( 'NONE',  ( 10.81189881249999729, 0.000000000000000000, -124.3437500020483952 ) ) ;
#31065 = CARTESIAN_POINT ( 'NONE',  ( -10.81189881249999907, -6.242252689847864744, -85.96875000204836681 ) ) ;
#31066 = CARTESIAN_POINT ( 'NONE',  ( 10.81189881249999729, 0.000000000000000000, -1.531250002048373249 ) ) ;
#31067 = CARTESIAN_POINT ( 'NONE',  ( 10.81189881249999551, -6.242252689847874514, -194.9687500020484094 ) ) ;
#31068 = CARTESIAN_POINT ( 'NONE',  ( -5.405949406250003975, -9.363379034771801557, -89.03125000204838102 ) ) ;
#31069 = CARTESIAN_POINT ( 'NONE',  ( -4.999999999999996447, 8.660254037844387298, -177.3750000040967905 ) ) ;
#31070 = CARTESIAN_POINT ( 'NONE',  ( 5.405949406249992428, -9.363379034771808662, -106.5937500020483810 ) ) ;
#31071 = CARTESIAN_POINT ( 'NONE',  ( 5.405949406249999534, 9.363379034771803333, -167.7812500020484094 ) ) ;
#31072 =( BOUNDED_CURVE ( )  B_SPLINE_CURVE ( 2, ( #22288, #15780, #42116, #28343, #21640, #35459, #5884 ),
 .UNSPECIFIED., .F., .F. ) 
 B_SPLINE_CURVE_WITH_KNOTS ( ( 3, 2, 2, 3 ),
 ( 0.1679104477611940427, 0.1691542288557214002, 0.1703980099502487855, 0.1716417910447761430 ),
 .UNSPECIFIED. ) 
 CURVE ( )  GEOMETRIC_REPRESENTATION_ITEM ( )  RATIONAL_B_SPLINE_CURVE ( ( 1.000000000000000000, 0.8660254037844387076, 1.000000000000000000, 0.8660254037844387076, 1.000000000000000000, 0.8660254037844357100, 1.000000000000003109 ) ) 
 REPRESENTATION_ITEM ( '' )  );
#31073 = CARTESIAN_POINT ( 'NONE',  ( 10.00000000000102318, -5.773502691895667560, -1.000000004096722739 ) ) ;
#31074 = CARTESIAN_POINT ( 'NONE',  ( 10.00000000000038369, -5.773502691896038819, -152.5000000040967620 ) ) ;
#31075 = CARTESIAN_POINT ( 'NONE',  ( -10.81189881249999729, 6.242252689847871849, -198.9062500020484094 ) ) ;
#31076 = CARTESIAN_POINT ( 'NONE',  ( -10.81189881249999729, 6.242252689847871849, -54.71875000204838813 ) ) ;
#31077 = CARTESIAN_POINT ( 'NONE',  ( 9.999999999999996447, -5.773502691896262640, -169.0000000040967905 ) ) ;
#31078 = CARTESIAN_POINT ( 'NONE',  ( -5.405949406249996869, 9.363379034771805109, -13.03125000204835615 ) ) ;
#31079 = CARTESIAN_POINT ( 'NONE',  ( -10.81189881249999729, 6.242252689847871849, -20.21875000204836681 ) ) ;
#31080 = CARTESIAN_POINT ( 'NONE',  ( 9.999999999999998224, 0.000000000000000000, -146.0000000000000000 ) ) ;
#31081 = CARTESIAN_POINT ( 'NONE',  ( 10.81189881249999551, -6.242252689847874514, -130.4687500020483810 ) ) ;
#31082 = CARTESIAN_POINT ( 'NONE',  ( 5.000000000000000000, 8.660254037844385522, -94.74999999999998579 ) ) ;
#31083 = CARTESIAN_POINT ( 'NONE',  ( 10.81189881249999907, 6.242252689847868297, -25.40625000204838102 ) ) ;
#31084 = CARTESIAN_POINT ( 'NONE',  ( -9.999999999999998224, 5.773502691896259087, -108.2500000040967763 ) ) ;
#31085 = CARTESIAN_POINT ( 'NONE',  ( -2.121150477449813534E-15, -11.54700538379251284, -26.75000000409677270 ) ) ;
#31086 = CARTESIAN_POINT ( 'NONE',  ( -2.121150477449813534E-15, -11.54700538379251284, -48.87499999999997868 ) ) ;
#31087 = CARTESIAN_POINT ( 'NONE',  ( 5.405949406249999534, 9.363379034771803333, -121.2812500020483952 ) ) ;
#31088 = CARTESIAN_POINT ( 'NONE',  ( -5.405949406250003975, -9.363379034771801557, -101.0312500020483952 ) ) ;
#31089 = EDGE_CURVE ( 'NONE', #17480, #9895, #34516, .T. ) ;
#31090 = ORIENTED_EDGE ( 'NONE', *, *, #8670, .T. ) ;
#31091 = CARTESIAN_POINT ( 'NONE',  ( 9.999999999999998224, 0.000000000000000000, -102.8750000040967763 ) ) ;
#31092 = CARTESIAN_POINT ( 'NONE',  ( -9.999999999999998224, 1.224646799147353059E-15, -200.0000000000000000 ) ) ;
#31093 = CARTESIAN_POINT ( 'NONE',  ( -5.405949406250003975, -9.363379034771801557, -164.0312500020484094 ) ) ;
#31094 = CARTESIAN_POINT ( 'NONE',  ( -10.81189881249999907, -6.242252689847864744, -54.46875000204836681 ) ) ;
#31095 = ORIENTED_EDGE ( 'NONE', *, *, #32284, .F. ) ;
#31096 = CARTESIAN_POINT ( 'NONE',  ( -2.121150477449813534E-15, -11.54700538379251284, -23.37499999999998224 ) ) ;
#31097 = CARTESIAN_POINT ( 'NONE',  ( -10.81189881249999729, -6.242252689847864744, -32.15625000204835970 ) ) ;
#31098 = CARTESIAN_POINT ( 'NONE',  ( 7.070501591499377789E-16, 11.54700538379251284, -159.1250000000000000 ) ) ;
#31099 = CARTESIAN_POINT ( 'NONE',  ( 9.999999999999998224, 0.000000000000000000, -91.99999999999998579 ) ) ;
#31100 = CARTESIAN_POINT ( 'NONE',  ( -10.00000000000000000, -5.773502691896251982, -30.00000000409674783 ) ) ;
#31101 = APPROVAL_PERSON_ORGANIZATION ( #3661, #15389, #29988 ) ;
#31102 = CARTESIAN_POINT ( 'NONE',  ( -2.121150477449813534E-15, -11.54700538379251284, -33.87499999999996447 ) ) ;
#31103 = CARTESIAN_POINT ( 'NONE',  ( 7.644554776091147741E-16, 12.48450537969573659, -133.1562500020483810 ) ) ;
#31104 = CARTESIAN_POINT ( 'NONE',  ( 0.2267623460602178065, 10.23228579648178638, -4.586030929915087727E-15 ) ) ;
#31105 = CARTESIAN_POINT ( 'NONE',  ( 0.000000000000000000, 0.000000000000000000, -99.99999999999998579 ) ) ;
#31106 = ORIENTED_EDGE ( 'NONE', *, *, #10900, .T. ) ;
#31107 = CARTESIAN_POINT ( 'NONE',  ( -5.405949406250003975, -9.363379034771801557, -63.53125000204837391 ) ) ;
#31109 = ORIENTED_EDGE ( 'NONE', *, *, #18814, .F. ) ;
#31108 = VERTEX_POINT ( 'NONE', #29299 ) ;
#31110 = CARTESIAN_POINT ( 'NONE',  ( 9.999999999999998224, 1.224646799147353059E-15, -99.99999999999998579 ) ) ;
#31111 = DIRECTION ( 'NONE',  ( 1.000000000000000000, 0.000000000000000000, 0.000000000000000000 ) ) ;
#31113 = EDGE_CURVE ( 'NONE', #4342, #32177, #566, .T. ) ;
#31112 = CARTESIAN_POINT ( 'NONE',  ( -5.405949406250003975, -9.363379034771801557, -169.8437500020484094 ) ) ;
#31114 = CARTESIAN_POINT ( 'NONE',  ( -5.405949406249996869, 9.363379034771805109, -185.5312500020484094 ) ) ;
#31115 = CARTESIAN_POINT ( 'NONE',  ( 10.81189881249999551, -6.242252689847874514, -13.46875000204836503 ) ) ;
#31116 = FACE_OUTER_BOUND ( 'NONE', #2286, .T. ) ;
#31117 = CARTESIAN_POINT ( 'NONE',  ( -2.293366432827344421E-15, -12.48450537969573659, -151.7187500020483810 ) ) ;
#31118 = CARTESIAN_POINT ( 'NONE',  ( -10.81189881249999907, -6.242252689847864744, -132.4687500020483810 ) ) ;
#31119 = CARTESIAN_POINT ( 'NONE',  ( 10.81189881249999729, 0.000000000000000000, -105.0312500020483810 ) ) ;
#31120 = CARTESIAN_POINT ( 'NONE',  ( -5.405949406249996869, 9.363379034771805109, -119.3437500020483810 ) ) ;
#31121 = CARTESIAN_POINT ( 'NONE',  ( 5.000000000000000000, 8.660254037844385522, -191.1250000040967905 ) ) ;
#31122 = CARTESIAN_POINT ( 'NONE',  ( -10.81189881249999729, 1.324075727343319199E-15, -123.7812500020483952 ) ) ;
#31123 = CARTESIAN_POINT ( 'NONE',  ( -2.293366432827344421E-15, -12.48450537969573659, -1.718750002048355929 ) ) ;
#31124 = CARTESIAN_POINT ( 'NONE',  ( -10.81189881249999729, 1.324075727343319199E-15, -132.5937500020483810 ) ) ;
#31125 = VECTOR ( 'NONE', #15820, 1000.000000000000000 ) ;
#31126 = CARTESIAN_POINT ( 'NONE',  ( -9.999999999999998224, 1.224646799147353059E-15, -163.2500000000000000 ) ) ;
#31127 = FACE_OUTER_BOUND ( 'NONE', #8011, .T. ) ;
#31128 = CARTESIAN_POINT ( 'NONE',  ( 5.000000000000000000, 8.660254037844385522, -145.7500000000000000 ) ) ;
#31129 = CARTESIAN_POINT ( 'NONE',  ( 9.999999999999996447, -5.773502691896262640, -23.12499999999997868 ) ) ;
#31130 = LOCAL_TIME ( 11, 57, 6.000000000000000000, #37732 ) ;
#31131 = CARTESIAN_POINT ( 'NONE',  ( -10.81189881249999729, 6.242252689847871849, -78.71875000204838102 ) ) ;
#31132 = CARTESIAN_POINT ( 'NONE',  ( 7.644554776091147741E-16, 12.48450537969573659, -68.46875000204838102 ) ) ;
#31133 = CARTESIAN_POINT ( 'NONE',  ( 9.999999999999998224, 0.000000000000000000, -18.87500000409675494 ) ) ;
#31134 = CARTESIAN_POINT ( 'NONE',  ( 10.81189881249999551, -6.242252689847874514, -34.65625000204836681 ) ) ;
#31135 = CARTESIAN_POINT ( 'NONE',  ( -10.81189881249999729, 6.242252689847871849, -42.71875000204835970 ) ) ;
#31136 = CARTESIAN_POINT ( 'NONE',  ( 0.000000000000000000, 0.000000000000000000, -200.0000000000000000 ) ) ;
#31137 = CARTESIAN_POINT ( 'NONE',  ( 5.405949406249999534, 9.363379034771803333, -152.5937500020483810 ) ) ;
#31138 = CARTESIAN_POINT ( 'NONE',  ( 7.070501591499377789E-16, 11.54700538379251284, -123.1249999999999858 ) ) ;
#31139 = CARTESIAN_POINT ( 'NONE',  ( 7.644554776091147741E-16, 12.48450537969573659, -131.6562500020483810 ) ) ;
#31140 = CARTESIAN_POINT ( 'NONE',  ( -4.999999999999996447, 8.660254037844387298, -94.49999999999998579 ) ) ;
#31141 = CARTESIAN_POINT ( 'NONE',  ( -10.00000000000000000, -5.773502691896251982, -74.62499999999997158 ) ) ;
#31142 = CARTESIAN_POINT ( 'NONE',  ( 10.81189881249999551, -6.242252689847874514, -7.656250002048368586 ) ) ;
#31143 = ORIENTED_EDGE ( 'NONE', *, *, #29039, .T. ) ;
#31144 = CARTESIAN_POINT ( 'NONE',  ( -2.293366432827344421E-15, -12.48450537969573659, -100.9062500020483952 ) ) ;
#31145 = CARTESIAN_POINT ( 'NONE',  ( -9.999999999999998224, 1.224646799147353059E-15, -124.6250000040967763 ) ) ;
#31146 = CARTESIAN_POINT ( 'NONE',  ( 9.999999999999998224, 0.000000000000000000, -56.37500000409676204 ) ) ;
#31147 = VECTOR ( 'NONE', #6892, 1000.000000000000000 ) ;
#31148 = CARTESIAN_POINT ( 'NONE',  ( -9.999999999999998224, 1.224646799147353059E-15, -33.12500000409676915 ) ) ;
#31149 = EDGE_CURVE ( 'NONE', #40511, #9826, #20212, .T. ) ;
#31150 = CARTESIAN_POINT ( 'NONE',  ( 5.000000000000000000, 8.660254037844385522, -130.7499999999999716 ) ) ;
#31151 = CARTESIAN_POINT ( 'NONE',  ( 10.81189881249999907, 6.242252689847868297, -44.90625000204836681 ) ) ;
#31152 = CARTESIAN_POINT ( 'NONE',  ( -9.999999999998969713, -5.773502691896847949, -40.50000000409674072 ) ) ;
#31153 = CARTESIAN_POINT ( 'NONE',  ( -5.405949406250003975, -9.363379034771801557, -155.0312500020484094 ) ) ;
#31154 = CARTESIAN_POINT ( 'NONE',  ( 7.644554776091147741E-16, 12.48450537969573659, -126.9687500020483668 ) ) ;
#31155 = CARTESIAN_POINT ( 'NONE',  ( 7.070501591499376803E-16, 11.54700538379251284, -3.500000004096760264 ) ) ;
#31156 = ORIENTED_EDGE ( 'NONE', *, *, #35064, .T. ) ;
#31157 = CARTESIAN_POINT ( 'NONE',  ( -9.999999999999998224, 1.224646799147353059E-15, -102.1250000040967905 ) ) ;
#31158 = EDGE_LOOP ( 'NONE', ( #13967, #5130, #13700, #10360 ) ) ;
#31159 = AXIS2_PLACEMENT_3D ( 'NONE', #33591, #11106, #17155 ) ;
#31160 = ORIENTED_EDGE ( 'NONE', *, *, #34683, .T. ) ;
#31161 = ORIENTED_EDGE ( 'NONE', *, *, #26996, .T. ) ;
#31162 =( BOUNDED_CURVE ( )  B_SPLINE_CURVE ( 2, ( #39151, #36338, #36760, #13431, #6770, #35919, #3117 ),
 .UNSPECIFIED., .F., .F. ) 
 B_SPLINE_CURVE_WITH_KNOTS ( ( 3, 2, 2, 3 ),
 ( 0.8395522388059704078, 0.8407960199004976820, 0.8420398009950251783, 0.8432835820895525636 ),
 .UNSPECIFIED. ) 
 CURVE ( )  GEOMETRIC_REPRESENTATION_ITEM ( )  RATIONAL_B_SPLINE_CURVE ( ( 0.9999999999999761302, 0.8660254037844625774, 1.000000000000000000, 0.8660254037844387076, 1.000000000000000000, 0.8660254037844028474, 1.000000000000035971 ) ) 
 REPRESENTATION_ITEM ( '' )  );
#31163 = CARTESIAN_POINT ( 'NONE',  ( 9.999999999999742428, 5.773502691896404748, -189.3749999999999716 ) ) ;
#31164 = CARTESIAN_POINT ( 'NONE',  ( 7.644554776091147741E-16, 12.48450537969573659, -192.9687500020483810 ) ) ;
#31165 = VECTOR ( 'NONE', #2598, 1000.000000000000114 ) ;
#31166 = CARTESIAN_POINT ( 'NONE',  ( 7.644554776091147741E-16, 12.48450537969573659, -36.96875000204835970 ) ) ;
#31167 = CARTESIAN_POINT ( 'NONE',  ( 1.679738968335770632, -10.37593646986413276, 1.566949817559348910E-14 ) ) ;
#31168 = CARTESIAN_POINT ( 'NONE',  ( 5.000000000000000000, 8.660254037844385522, -139.7499999999999716 ) ) ;
#31169 = CARTESIAN_POINT ( 'NONE',  ( 5.405949406249999534, 9.363379034771803333, -170.5937500020484094 ) ) ;
#31170 = CARTESIAN_POINT ( 'NONE',  ( -10.81189881249999729, 1.324075727343319199E-15, -162.5937500020484094 ) ) ;
#31171 = CARTESIAN_POINT ( 'NONE',  ( -79.99999999999992895, 39.99999999999999289, -170.0000000000000000 ) ) ;
#31172 = CARTESIAN_POINT ( 'NONE',  ( -2.293366432827344421E-15, -12.48450537969573659, -141.2187500020483810 ) ) ;
#31173 = CARTESIAN_POINT ( 'NONE',  ( 5.405949406249992428, -9.363379034771808662, -151.7812500020484094 ) ) ;
#31174 = CARTESIAN_POINT ( 'NONE',  ( -5.405949406249996869, 9.363379034771805109, -150.8437500020483810 ) ) ;
#31175 = CARTESIAN_POINT ( 'NONE',  ( -9.999999999999612754, -5.773502691896474914, -155.6249999999999716 ) ) ;
#31176 = FACE_OUTER_BOUND ( 'NONE', #3265, .T. ) ;
#31177 = CARTESIAN_POINT ( 'NONE',  ( 10.00000000000000000, 5.773502691896255534, -172.8750000000000000 ) ) ;
#31178 = CARTESIAN_POINT ( 'NONE',  ( -5.405949406249996869, 9.363379034771805109, -90.84375000204838102 ) ) ;
#31179 = CARTESIAN_POINT ( 'NONE',  ( -6.652853726956784897, 8.522716305231336165, -100.0000000000000142 ) ) ;
#31180 = CARTESIAN_POINT ( 'NONE',  ( -5.405949406250003975, -9.363379034771801557, -62.03125000204837391 ) ) ;
#31181 = CARTESIAN_POINT ( 'NONE',  ( 10.00000000000000000, 5.773502691896255534, -133.8750000000000000 ) ) ;
#31182 = CARTESIAN_POINT ( 'NONE',  ( -5.405949406249996869, 9.363379034771805109, -180.8437500020483810 ) ) ;
#31183 = CARTESIAN_POINT ( 'NONE',  ( -10.81189881249999907, -6.242252689847864744, -111.6562500020483952 ) ) ;
#31184 = CARTESIAN_POINT ( 'NONE',  ( -5.405949406250003975, -9.363379034771801557, -156.5312500020484094 ) ) ;
#31185 = CARTESIAN_POINT ( 'NONE',  ( 0.000000000000000000, 0.000000000000000000, -99.99999999999998579 ) ) ;
#31186 = CARTESIAN_POINT ( 'NONE',  ( -5.405949406250003975, -9.363379034771801557, -41.03125000204838102 ) ) ;
#31187 = CARTESIAN_POINT ( 'NONE',  ( 7.070501591499377789E-16, 11.54700538379251284, -134.0000000040967905 ) ) ;
#31188 = CARTESIAN_POINT ( 'NONE',  ( 10.00000000000000000, 5.773502691896255534, -109.8750000000000000 ) ) ;
#31189 = ORIENTED_EDGE ( 'NONE', *, *, #36252, .F. ) ;
#31190 = CARTESIAN_POINT ( 'NONE',  ( -2.293366432827344421E-15, -12.48450537969573659, -126.4062500020483810 ) ) ;
#31191 = CARTESIAN_POINT ( 'NONE',  ( -9.999999999999998224, 5.773502691896259087, -151.7500000040967620 ) ) ;
#31192 = CARTESIAN_POINT ( 'NONE',  ( -4.999999999999996447, 8.660254037844387298, -67.87500000409677625 ) ) ;
#31193 = CARTESIAN_POINT ( 'NONE',  ( -10.81189881249999729, 6.242252689847871849, -180.9062500020484094 ) ) ;
#31194 = ORIENTED_EDGE ( 'NONE', *, *, #431, .F. ) ;
#31195 = CARTESIAN_POINT ( 'NONE',  ( 10.81189881249999551, -6.242252689847874514, -172.4687500020484094 ) ) ;
#31196 = CARTESIAN_POINT ( 'NONE',  ( 7.070501591499377789E-16, 11.54700538379251284, -54.50000000409677625 ) ) ;
#31197 = EDGE_CURVE ( 'NONE', #4760, #26724, #37875, .T. ) ;
#31198 = CARTESIAN_POINT ( 'NONE',  ( -79.99999999999994316, -20.00000000000000711, -160.0000000000000000 ) ) ;
#31199 = DIRECTION ( 'NONE',  ( -0.000000000000000000, -0.000000000000000000, 1.000000000000000000 ) ) ;
#31200 = EDGE_CURVE ( 'NONE', #28824, #19402, #42268, .T. ) ;
#31201 = CARTESIAN_POINT ( 'NONE',  ( 7.644554776091147741E-16, 12.48450537969573659, -70.15625000204839523 ) ) ;
#31202 = CARTESIAN_POINT ( 'NONE',  ( -10.81189881249999729, -6.242252689847864744, -54.65625000204838813 ) ) ;
#31203 = CARTESIAN_POINT ( 'NONE',  ( -5.000000000000003553, -8.660254037844383745, -44.87500000409677625 ) ) ;
#31204 = CARTESIAN_POINT ( 'NONE',  ( 5.405949406249992428, -9.363379034771808662, -1.593750002048366365 ) ) ;
#31205 = FACE_OUTER_BOUND ( 'NONE', #20949, .T. ) ;
#31206 = CARTESIAN_POINT ( 'NONE',  ( -10.81189881249999729, 1.324075727343319199E-15, -174.7812500020484094 ) ) ;
#31207 = VECTOR ( 'NONE', #3908, 1000.000000000000000 ) ;
#31208 = CARTESIAN_POINT ( 'NONE',  ( -57.00000000000002132, 6.980486755139916067E-15, -240.0000000000000000 ) ) ;
#31209 = DIRECTION ( 'NONE',  ( -0.000000000000000000, 1.000000000000000000, -0.000000000000000000 ) ) ;
#31210 = VERTEX_POINT ( 'NONE', #21973 ) ;
#31211 = CARTESIAN_POINT ( 'NONE',  ( 23.09401076758504345, 1.040834085586084257E-14, 0.000000000000000000 ) ) ;
#31212 = CARTESIAN_POINT ( 'NONE',  ( -9.999999999999998224, 0.000000000000000000, -99.99999999999998579 ) ) ;
#31213 =( BOUNDED_CURVE ( )  B_SPLINE_CURVE ( 2, ( #15775, #41896, #3274, #36074, #38678, #19033, #28554 ),
 .UNSPECIFIED., .F., .F. ) 
 B_SPLINE_CURVE_WITH_KNOTS ( ( 3, 2, 2, 3 ),
 ( 0.3320895522388061516, 0.3333333333333334259, 0.3345771144278607556, 0.3358208955223880854 ),
 .UNSPECIFIED. ) 
 CURVE ( )  GEOMETRIC_REPRESENTATION_ITEM ( )  RATIONAL_B_SPLINE_CURVE ( ( 0.9999999999999820144, 0.8660254037844566932, 1.000000000000000000, 0.8660254037844387076, 1.000000000000000000, 0.8660254037844387076, 1.000000000000000000 ) ) 
 REPRESENTATION_ITEM ( '' )  );
#31214 = FACE_OUTER_BOUND ( 'NONE', #11386, .T. ) ;
#31216 = ORIENTED_EDGE ( 'NONE', *, *, #13341, .F. ) ;
#31215 = CARTESIAN_POINT ( 'NONE',  ( 5.405949406249999534, 9.363379034771803333, -83.78125000204838102 ) ) ;
#31217 = ORIENTED_EDGE ( 'NONE', *, *, #2500, .T. ) ;
#31218 = ORIENTED_EDGE ( 'NONE', *, *, #21729, .F. ) ;
#31219 = CARTESIAN_POINT ( 'NONE',  ( -10.81189881249999729, 1.324075727343319199E-15, -33.59375000204836681 ) ) ;
#31220 = LINE ( 'NONE', #1647, #39677 ) ;
#31221 = CARTESIAN_POINT ( 'NONE',  ( -5.405949406249996869, 9.363379034771805109, -17.53125000204835970 ) ) ;
#31222 =( BOUNDED_CURVE ( )  B_SPLINE_CURVE ( 2, ( #10207, #32893, #33326, #23172, #23393, #6354, #25996 ),
 .UNSPECIFIED., .F., .F. ) 
 B_SPLINE_CURVE_WITH_KNOTS ( ( 3, 2, 2, 3 ),
 ( 0.7350746268656719318, 0.7363184079601993171, 0.7375621890547265913, 0.7388059701492539766 ),
 .UNSPECIFIED. ) 
 CURVE ( )  GEOMETRIC_REPRESENTATION_ITEM ( )  RATIONAL_B_SPLINE_CURVE ( ( 0.9999999999999641398, 0.8660254037844745678, 1.000000000000000000, 0.8660254037844387076, 1.000000000000000000, 0.8660254037844148378, 1.000000000000023981 ) ) 
 REPRESENTATION_ITEM ( '' )  );
#31224 = ORIENTED_EDGE ( 'NONE', *, *, #13771, .F. ) ;
#31223 = CARTESIAN_POINT ( 'NONE',  ( 10.81189881249999729, 0.000000000000000000, -64.34375000204836681 ) ) ;
#31225 = CARTESIAN_POINT ( 'NONE',  ( -9.999999999999998224, 1.224646799147353059E-15, -131.7499999999999716 ) ) ;
#31226 = CARTESIAN_POINT ( 'NONE',  ( 9.999999999999996447, -5.773502691896262640, -36.62499999999996447 ) ) ;
#31227 = EDGE_CURVE ( 'NONE', #23672, #3711, #39218, .T. ) ;
#31228 = CARTESIAN_POINT ( 'NONE',  ( 10.81189881249999551, -6.242252689847874514, -182.9687500020484094 ) ) ;
#31229 = CARTESIAN_POINT ( 'NONE',  ( -2.293366432827344421E-15, -12.48450537969573659, -168.2187500020483810 ) ) ;
#31230 = CARTESIAN_POINT ( 'NONE',  ( -9.999999999999998224, 1.224646799147353059E-15, -200.0000000000000000 ) ) ;
#31231 = CARTESIAN_POINT ( 'NONE',  ( 7.070501591499376803E-16, 11.54700538379251284, -59.00000000409676915 ) ) ;
#31232 = CARTESIAN_POINT ( 'NONE',  ( 7.070501591499376803E-16, 11.54700538379251284, -141.1250000000000000 ) ) ;
#31233 = DIRECTION ( 'NONE',  ( -0.000000000000000000, -0.000000000000000000, 1.000000000000000000 ) ) ;
#31234 = CARTESIAN_POINT ( 'NONE',  ( -5.000000000000003553, -8.660254037844383745, -196.0000000000000000 ) ) ;
#31235 = CARTESIAN_POINT ( 'NONE',  ( 7.644554776091147741E-16, 12.48450537969573659, -113.4687500020483952 ) ) ;
#31236 = CYLINDRICAL_SURFACE ( 'NONE', #25955, 9.999999999999998224 ) ;
#31237 = CARTESIAN_POINT ( 'NONE',  ( -10.81189881249999729, 6.242252689847871849, -80.40625000204839523 ) ) ;
#31238 = CARTESIAN_POINT ( 'NONE',  ( -5.405949406250003975, -9.363379034771801557, -94.84375000204838102 ) ) ;
#31239 = CARTESIAN_POINT ( 'NONE',  ( 10.81189881249999551, -6.242252689847874514, -62.96875000204838102 ) ) ;
#31240 = CARTESIAN_POINT ( 'NONE',  ( 10.81189881249999907, 6.242252689847868297, -67.40625000204839523 ) ) ;
#31241 = CARTESIAN_POINT ( 'NONE',  ( -4.999999999999996447, 8.660254037844387298, -153.3750000040967905 ) ) ;
#31242 = CARTESIAN_POINT ( 'NONE',  ( -5.000000000000003553, -8.660254037844383745, -131.5000000000000000 ) ) ;
#31243 = CARTESIAN_POINT ( 'NONE',  ( -5.405949406249996869, 9.363379034771805109, -152.5312500020484094 ) ) ;
#31244 = CARTESIAN_POINT ( 'NONE',  ( -10.81189881249999729, 6.242252689847871849, -164.4062500020484094 ) ) ;
#31245 = CARTESIAN_POINT ( 'NONE',  ( -9.999999999998969713, -5.773502691896847949, -13.50000000409673540 ) ) ;
#31246 = CARTESIAN_POINT ( 'NONE',  ( -9.999999999999998224, 1.224646799147353059E-15, -172.2500000000000000 ) ) ;
#31247 = CARTESIAN_POINT ( 'NONE',  ( -2.293366432827344421E-15, -12.48450537969573659, -97.71875000204838102 ) ) ;
#31248 = CARTESIAN_POINT ( 'NONE',  ( 5.000000000000000000, 8.660254037844385522, -63.24999999999997158 ) ) ;
#31249 = CARTESIAN_POINT ( 'NONE',  ( 7.070501591499377789E-16, 11.54700538379251284, -72.12499999999995737 ) ) ;
#31250 = CARTESIAN_POINT ( 'NONE',  ( -5.405949406249996869, 9.363379034771805109, -197.3437500020484094 ) ) ;
#31251 = CARTESIAN_POINT ( 'NONE',  ( 9.999999999999996447, -5.773502691896262640, -85.00000000409677625 ) ) ;
#31252 = EDGE_CURVE ( 'NONE', #17462, #17801, #21861, .T. ) ;
#31253 = CARTESIAN_POINT ( 'NONE',  ( -3.767292561726145905, -9.597395893938625022, -179.9999999999999716 ) ) ;
#31254 = CARTESIAN_POINT ( 'NONE',  ( -2.293366432827344421E-15, -12.48450537969573659, -90.40625000204838102 ) ) ;
#31255 = CARTESIAN_POINT ( 'NONE',  ( 7.644554776091147741E-16, 12.48450537969573659, -74.65625000204838102 ) ) ;
#31256 = EDGE_CURVE ( 'NONE', #37987, #587, #9447, .T. ) ;
#31257 = CARTESIAN_POINT ( 'NONE',  ( -2.121150477449813534E-15, -11.54700538379251284, -68.75000000409679046 ) ) ;
#31258 = CARTESIAN_POINT ( 'NONE',  ( 9.999999999999742428, 5.773502691896404748, -135.3750000000000000 ) ) ;
#31259 = CARTESIAN_POINT ( 'NONE',  ( -10.81189881249999907, -6.242252689847864744, -24.46875000204837036 ) ) ;
#31260 = ORIENTED_EDGE ( 'NONE', *, *, #15933, .T. ) ;
#31261 = CARTESIAN_POINT ( 'NONE',  ( -2.121150477449813534E-15, -11.54700538379251284, -2.374999999999946709 ) ) ;
#31262 = ADVANCED_FACE ( 'NONE', ( #18945 ), #12873, .T. ) ;
#31263 = CARTESIAN_POINT ( 'NONE',  ( -10.81189881249999907, -6.242252689847864744, -18.65625000204837747 ) ) ;
#31264 = CARTESIAN_POINT ( 'NONE',  ( -10.81189881249999729, 6.242252689847871849, -14.21875000204836681 ) ) ;
#31265 = CARTESIAN_POINT ( 'NONE',  ( 9.999999999999998224, 0.000000000000000000, -93.87500000409677625 ) ) ;
#31266 = CARTESIAN_POINT ( 'NONE',  ( -5.000000000000003553, -8.660254037844383745, -2.875000004096767370 ) ) ;
#31267 = CARTESIAN_POINT ( 'NONE',  ( -9.999999999999998224, 1.224646799147353059E-15, -200.0000000000000000 ) ) ;
#31268 = CARTESIAN_POINT ( 'NONE',  ( 7.644554776091147741E-16, 12.48450537969573659, -131.6562500020483810 ) ) ;
#31269 = CARTESIAN_POINT ( 'NONE',  ( 10.00000000000000000, 5.773502691896255534, -186.3750000000000284 ) ) ;
#31271 = ORIENTED_EDGE ( 'NONE', *, *, #375, .T. ) ;
#31270 = CARTESIAN_POINT ( 'NONE',  ( -5.405949406249996869, 9.363379034771805109, -106.0312500020483810 ) ) ;
#31272 = FACE_OUTER_BOUND ( 'NONE', #14967, .T. ) ;
#31273 = VERTEX_POINT ( 'NONE', #22613 ) ;
#31274 = VERTEX_POINT ( 'NONE', #32131 ) ;
#31275 = ADVANCED_FACE ( 'NONE', ( #28472 ), #6219, .T. ) ;
#31276 = CARTESIAN_POINT ( 'NONE',  ( 10.81189881249999551, -6.242252689847874514, -40.65625000204835970 ) ) ;
#31277 = APPROVAL_ROLE ( '' ) ;
#31278 = CARTESIAN_POINT ( 'NONE',  ( 5.405949406249999534, 9.363379034771803333, -88.09375000204836681 ) ) ;
#31279 = CYLINDRICAL_SURFACE ( 'NONE', #10482, 9.999999999999998224 ) ;
#31280 = CARTESIAN_POINT ( 'NONE',  ( -2.121150477449813534E-15, -11.54700538379251284, -128.7500000040967905 ) ) ;
#31281 = CARTESIAN_POINT ( 'NONE',  ( 9.999999999999998224, 1.224646799147353059E-15, -99.99999999999998579 ) ) ;
#31282 = CARTESIAN_POINT ( 'NONE',  ( 10.81189881249999907, 6.242252689847868297, -167.9062500020484094 ) ) ;
#31283 = CARTESIAN_POINT ( 'NONE',  ( -5.000000000000003553, -8.660254037844383745, -139.0000000000000000 ) ) ;
#31284 = CARTESIAN_POINT ( 'NONE',  ( 5.405949406249999534, 9.363379034771803333, -121.0937500020483952 ) ) ;
#31285 =( BOUNDED_CURVE ( )  B_SPLINE_CURVE ( 2, ( #18967, #32154, #14652, #27841, #40973, #11417, #24611 ),
 .UNSPECIFIED., .F., .F. ) 
 B_SPLINE_CURVE_WITH_KNOTS ( ( 3, 2, 2, 3 ),
 ( 0.04104477611940302029, 0.04228855721393039169, 0.04353233830845775615, 0.04477611940298512061 ),
 .UNSPECIFIED. ) 
 CURVE ( )  GEOMETRIC_REPRESENTATION_ITEM ( )  RATIONAL_B_SPLINE_CURVE ( ( 0.9999999999999963363, 0.8660254037844424824, 1.000000000000000000, 0.8660254037844387076, 1.000000000000000000, 0.8660254037844334896, 1.000000000000005329 ) ) 
 REPRESENTATION_ITEM ( '' )  );
#31286 = CARTESIAN_POINT ( 'NONE',  ( -10.81189881249999729, 6.242252689847871849, -83.21875000204838102 ) ) ;
#31287 = CARTESIAN_POINT ( 'NONE',  ( 9.999999999999998224, 0.000000000000000000, -200.0000000000000000 ) ) ;
#31288 = CARTESIAN_POINT ( 'NONE',  ( 5.405949406249992428, -9.363379034771808662, -196.5937500020484094 ) ) ;
#31289 = CARTESIAN_POINT ( 'NONE',  ( -5.405949406249996869, 9.363379034771805109, -91.03125000204838102 ) ) ;
#31290 = CARTESIAN_POINT ( 'NONE',  ( -5.000000000000003553, -8.660254037844383745, -176.8750000040967905 ) ) ;
#31291 = CARTESIAN_POINT ( 'NONE',  ( -5.405949406249996869, 9.363379034771805109, -173.5312500020484094 ) ) ;
#31292 = CARTESIAN_POINT ( 'NONE',  ( 9.999999999998969713, 5.773502691896851502, -103.8750000000000000 ) ) ;
#31293 = CARTESIAN_POINT ( 'NONE',  ( 5.405949406249999534, 9.363379034771803333, -178.2812500020484094 ) ) ;
#31294 = CARTESIAN_POINT ( 'NONE',  ( -10.81189881249999729, 6.242252689847871849, -188.4062500020484094 ) ) ;
#31295 = CARTESIAN_POINT ( 'NONE',  ( -10.81189881249999729, 1.324075727343319199E-15, -51.59375000204835260 ) ) ;
#31296 = CARTESIAN_POINT ( 'NONE',  ( 7.070501591499377789E-16, 11.54700538379251284, -161.0000000040967905 ) ) ;
#31297 = CARTESIAN_POINT ( 'NONE',  ( -5.405949406250003975, -9.363379034771801557, -12.53125000204835615 ) ) ;
#31298 = CARTESIAN_POINT ( 'NONE',  ( 10.81189881249999729, 0.000000000000000000, -16.34375000204835260 ) ) ;
#31299 = CARTESIAN_POINT ( 'NONE',  ( 9.999999999998456346, 5.773502691897149042, -54.37499999999994316 ) ) ;
#31300 = CARTESIAN_POINT ( 'NONE',  ( 10.81189881249999907, 6.242252689847868297, -124.2187500020483952 ) ) ;
#31301 = CARTESIAN_POINT ( 'NONE',  ( 5.000000000000000000, 8.660254037844385522, -99.24999999999998579 ) ) ;
#31302 = CARTESIAN_POINT ( 'NONE',  ( -2.293366432827344421E-15, -12.48450537969573659, -22.90625000204837747 ) ) ;
#31303 = CARTESIAN_POINT ( 'NONE',  ( 7.070501591499377789E-16, 11.54700538379251284, -108.5000000040967763 ) ) ;
#31304 = FACE_OUTER_BOUND ( 'NONE', #21268, .T. ) ;
#31305 = CARTESIAN_POINT ( 'NONE',  ( -5.000000000000003553, -8.660254037844383745, -51.99999999999996447 ) ) ;
#31306 = CARTESIAN_POINT ( 'NONE',  ( 7.644554776091147741E-16, 12.48450537969573659, -119.6562500020484094 ) ) ;
#31307 = CARTESIAN_POINT ( 'NONE',  ( -5.405949406249996869, 9.363379034771805109, -100.0312500020483952 ) ) ;
#31308 = VERTEX_POINT ( 'NONE', #32550 ) ;
#31309 = CARTESIAN_POINT ( 'NONE',  ( -4.999999999999996447, 8.660254037844387298, -96.37500000409677625 ) ) ;
#31310 = CARTESIAN_POINT ( 'NONE',  ( 4.999999999999992006, -8.660254037844389075, -113.2499999999999858 ) ) ;
#31311 = CARTESIAN_POINT ( 'NONE',  ( 10.81189881249999551, -6.242252689847874514, -168.1562500020484094 ) ) ;
#31312 = CARTESIAN_POINT ( 'NONE',  ( 7.644554776091147741E-16, 12.48450537969573659, -47.46875000204836681 ) ) ;
#31313 = ORIENTED_EDGE ( 'NONE', *, *, #1914, .F. ) ;
#31314 = CARTESIAN_POINT ( 'NONE',  ( 7.070501591499377789E-16, 11.54700538379251284, -24.12499999999998934 ) ) ;
#31315 = CARTESIAN_POINT ( 'NONE',  ( -10.81189881249999729, 6.242252689847871849, -24.90625000204838813 ) ) ;
#31316 = CARTESIAN_POINT ( 'NONE',  ( -2.121150477449813534E-15, -11.54700538379251284, -164.3750000000000000 ) ) ;
#31317 = CARTESIAN_POINT ( 'NONE',  ( 4.999999999999992006, -8.660254037844389075, -102.7500000000000000 ) ) ;
#31318 = CARTESIAN_POINT ( 'NONE',  ( 4.999999999999992006, -8.660254037844389075, -31.12500000409676559 ) ) ;
#31319 = CYLINDRICAL_SURFACE ( 'NONE', #37350, 9.999999999999998224 ) ;
#31320 = EDGE_CURVE ( 'NONE', #25539, #39040, #2980, .T. ) ;
#31321 = CARTESIAN_POINT ( 'NONE',  ( -5.405949406250003975, -9.363379034771801557, -137.0312500020484094 ) ) ;
#31322 = CARTESIAN_POINT ( 'NONE',  ( -1.040834085586084257E-14, -20.00000000000000355, 32.49999999999999289 ) ) ;
#31323 = CARTESIAN_POINT ( 'NONE',  ( -9.999999999999998224, 1.224646799147353059E-15, -69.12500000409677625 ) ) ;
#31324 = ORIENTED_EDGE ( 'NONE', *, *, #1662, .F. ) ;
#31325 = CARTESIAN_POINT ( 'NONE',  ( 5.405949406249999534, 9.363379034771803333, -61.28125000204837391 ) ) ;
#31326 = PERSON_AND_ORGANIZATION ( #11915, #17965 ) ;
#31328 = VERTEX_POINT ( 'NONE', #12453 ) ;
#31327 = ORIENTED_EDGE ( 'NONE', *, *, #39233, .F. ) ;
#31329 = CARTESIAN_POINT ( 'NONE',  ( -9.999999999999998224, 1.224646799147353059E-15, -181.6250000040967905 ) ) ;
#31330 = CARTESIAN_POINT ( 'NONE',  ( -2.253471898105756789E-15, 15.00000000000011013, 49.99999999999998579 ) ) ;
#31331 =( BOUNDED_CURVE ( )  B_SPLINE_CURVE ( 2, ( #36783, #16910, #27287, #40637, #1181, #7219, #14524 ),
 .UNSPECIFIED., .F., .F. ) 
 B_SPLINE_CURVE_WITH_KNOTS ( ( 3, 2, 2, 3 ),
 ( 0.2611940298507463565, 0.2624378109452737418, 0.2636815920398011270, 0.2649253731343284568 ),
 .UNSPECIFIED. ) 
 CURVE ( )  GEOMETRIC_REPRESENTATION_ITEM ( )  RATIONAL_B_SPLINE_CURVE ( ( 0.9999999999999880096, 0.8660254037844506980, 1.000000000000000000, 0.8660254037844387076, 1.000000000000000000, 0.8660254037844267172, 1.000000000000011990 ) ) 
 REPRESENTATION_ITEM ( '' )  );
#31332 = CARTESIAN_POINT ( 'NONE',  ( -5.405949406249996869, 9.363379034771805109, -159.8437500020484094 ) ) ;
#31333 = CARTESIAN_POINT ( 'NONE',  ( 7.644554776091147741E-16, 12.48450537969573659, -191.6562500020484094 ) ) ;
#31334 = CARTESIAN_POINT ( 'NONE',  ( -10.81189881249999729, 6.242252689847871849, -8.218750002048354375 ) ) ;
#31335 = CARTESIAN_POINT ( 'NONE',  ( -9.999999999999998224, 1.224646799147353059E-15, -129.1250000040967620 ) ) ;
#31336 = CARTESIAN_POINT ( 'NONE',  ( -5.405949406250003975, -9.363379034771801557, -147.3437500020483810 ) ) ;
#31337 = CARTESIAN_POINT ( 'NONE',  ( 10.81189881249999551, -6.242252689847874514, -106.6562500020483952 ) ) ;
#31338 = CARTESIAN_POINT ( 'NONE',  ( 10.81189881249999729, 0.000000000000000000, -107.8437500020483810 ) ) ;
#31339 = CARTESIAN_POINT ( 'NONE',  ( 10.00000000000012257, -5.773502691896187144, -161.1250000000000568 ) ) ;
#31340 = CARTESIAN_POINT ( 'NONE',  ( -10.81189881249999907, -6.242252689847864744, -117.6562500020483952 ) ) ;
#31341 = CARTESIAN_POINT ( 'NONE',  ( 10.81189881249999551, -6.242252689847874514, -1.468750002048354819 ) ) ;
#31342 = CARTESIAN_POINT ( 'NONE',  ( 7.644554776091147741E-16, 12.48450537969573659, -131.4687500020483810 ) ) ;
#31343 = CARTESIAN_POINT ( 'NONE',  ( -10.81189881249999729, -6.242252689847864744, -195.6562500020484094 ) ) ;
#31344 = DIRECTION ( 'NONE',  ( -0.000000000000000000, -0.000000000000000000, 1.000000000000000000 ) ) ;
#31345 = CARTESIAN_POINT ( 'NONE',  ( 10.00000000000000000, 5.773502691896255534, -148.8750000000000000 ) ) ;
#31346 = CARTESIAN_POINT ( 'NONE',  ( -10.00000000000000000, -5.773502691896251982, -16.12499999999997158 ) ) ;
#31347 = CARTESIAN_POINT ( 'NONE',  ( 10.81189881249999551, -6.242252689847874514, -74.96875000204839523 ) ) ;
#31348 = CARTESIAN_POINT ( 'NONE',  ( -10.81189881249999729, 1.324075727343319199E-15, -59.09375000204835970 ) ) ;
#31349 = CARTESIAN_POINT ( 'NONE',  ( -9.999999999999998224, 5.773502691896259087, -190.7500000040968189 ) ) ;
#31350 = CARTESIAN_POINT ( 'NONE',  ( -10.81189881249999729, 1.324075727343319199E-15, -33.78125000204837391 ) ) ;
#31351 = CARTESIAN_POINT ( 'NONE',  ( -10.81189881249999729, 1.324075727343319199E-15, -36.59375000204836681 ) ) ;
#31352 = CARTESIAN_POINT ( 'NONE',  ( 0.000000000000000000, 0.000000000000000000, -99.99999999999998579 ) ) ;
#31353 = CARTESIAN_POINT ( 'NONE',  ( 10.81189881249999907, 6.242252689847868297, -146.7187500020484094 ) ) ;
#31354 = CARTESIAN_POINT ( 'NONE',  ( -10.00000000000000000, -5.773502691896251982, -124.1250000000000000 ) ) ;
#31355 = CARTESIAN_POINT ( 'NONE',  ( -10.00000000000076916, 5.773502691895813221, -136.3749999999999716 ) ) ;
#31356 = CARTESIAN_POINT ( 'NONE',  ( 9.999999999999998224, 0.000000000000000000, -75.49999999999998579 ) ) ;
#31357 = CARTESIAN_POINT ( 'NONE',  ( -5.405949406250003975, -9.363379034771801557, -6.531250002048377468 ) ) ;
#31358 = ORIENTED_EDGE ( 'NONE', *, *, #1117, .F. ) ;
#31359 = DIRECTION ( 'NONE',  ( -0.000000000000000000, -0.000000000000000000, 1.000000000000000000 ) ) ;
#31360 = CARTESIAN_POINT ( 'NONE',  ( -9.999999999999998224, 5.773502691896259087, -127.7500000040967905 ) ) ;
#31361 = CARTESIAN_POINT ( 'NONE',  ( 9.999999999999998224, 0.000000000000000000, -143.3750000040967905 ) ) ;
#31362 = CARTESIAN_POINT ( 'NONE',  ( -10.81189881249999729, 6.242252689847871849, -78.71875000204838102 ) ) ;
#31363 = CARTESIAN_POINT ( 'NONE',  ( 9.999999999999996447, -5.773502691896262640, -37.00000000409676204 ) ) ;
#31364 = CARTESIAN_POINT ( 'NONE',  ( -10.00000000000102496, 5.773502691895664007, -61.37499999999995737 ) ) ;
#31365 = CARTESIAN_POINT ( 'NONE',  ( 10.81189881249999729, 0.000000000000000000, -42.03125000204838102 ) ) ;
#31366 = CYLINDRICAL_SURFACE ( 'NONE', #4871, 9.999999999999998224 ) ;
#31367 = CARTESIAN_POINT ( 'NONE',  ( 10.81189881249999907, 6.242252689847868297, -146.9062500020484094 ) ) ;
#31368 = CARTESIAN_POINT ( 'NONE',  ( -5.405949406250003975, -9.363379034771801557, -123.3437500020483952 ) ) ;
#31369 = CARTESIAN_POINT ( 'NONE',  ( -9.999999999999998224, 1.224646799147353059E-15, -200.0000000000000000 ) ) ;
#31370 = CYLINDRICAL_SURFACE ( 'NONE', #33491, 9.999999999999998224 ) ;
#31371 = ORIENTED_EDGE ( 'NONE', *, *, #19616, .F. ) ;
#31372 = AXIS2_PLACEMENT_3D ( 'NONE', #23865, #30129, #774 ) ;
#31373 = ORIENTED_EDGE ( 'NONE', *, *, #7944, .T. ) ;
#31374 = VERTEX_POINT ( 'NONE', #28681 ) ;
#31375 = EDGE_CURVE ( 'NONE', #468, #13705, #5366, .T. ) ;
#31376 = CARTESIAN_POINT ( 'NONE',  ( -1.040834085586084257E-14, 125.0000000000000000, 22.49999999999999289 ) ) ;
#31377 = CARTESIAN_POINT ( 'NONE',  ( -2.293366432827344421E-15, -12.48450537969573659, -181.7187500020484094 ) ) ;
#31378 = CARTESIAN_POINT ( 'NONE',  ( 7.644554776091147741E-16, 12.48450537969573659, -38.46875000204835260 ) ) ;
#31379 = CARTESIAN_POINT ( 'NONE',  ( 9.999999999999227285, 5.773502691896701400, -110.2500000040967478 ) ) ;
#31380 = CARTESIAN_POINT ( 'NONE',  ( 5.405949406249992428, -9.363379034771808662, -174.0937500020484094 ) ) ;
#31381 = CARTESIAN_POINT ( 'NONE',  ( -2.293366432827344421E-15, -12.48450537969573659, -156.2187500020483810 ) ) ;
#31382 = CARTESIAN_POINT ( 'NONE',  ( 4.999999999999992006, -8.660254037844389075, -76.12500000409677625 ) ) ;
#31383 = CARTESIAN_POINT ( 'NONE',  ( 10.81189881249999907, 6.242252689847868297, -136.2187500020483810 ) ) ;
#31384 = CARTESIAN_POINT ( 'NONE',  ( 10.81189881249999729, 0.000000000000000000, -138.0312500020484094 ) ) ;
#31385 = CARTESIAN_POINT ( 'NONE',  ( -10.81189881249999729, -6.242252689847864744, -157.9687500020484379 ) ) ;
#31386 = DIRECTION ( 'NONE',  ( 0.000000000000000000, 0.7071067811865484609, 0.7071067811865465735 ) ) ;
#31387 = CARTESIAN_POINT ( 'NONE',  ( -9.999999999999996447, 5.773502691896259975, -169.3750000000000000 ) ) ;
#31388 = CARTESIAN_POINT ( 'NONE',  ( 7.070501591499377789E-16, 11.54700538379251284, -169.6250000000000000 ) ) ;
#31389 = CARTESIAN_POINT ( 'NONE',  ( 5.405949406249992428, -9.363379034771808662, -78.09375000204838102 ) ) ;
#31390 = DIRECTION ( 'NONE',  ( 1.000000000000000000, 0.000000000000000000, 0.000000000000000000 ) ) ;
#31391 = CARTESIAN_POINT ( 'NONE',  ( 10.81189881249999551, -6.242252689847874514, -60.15625000204839523 ) ) ;
#31392 = CARTESIAN_POINT ( 'NONE',  ( -9.955545358920547372, 3.667973230269648610, -99.99999999999998579 ) ) ;
#31393 = CARTESIAN_POINT ( 'NONE',  ( 10.81189881249999551, -6.242252689847874514, -169.4687500020483810 ) ) ;
#31394 = CARTESIAN_POINT ( 'NONE',  ( -10.81189881249999729, 6.242252689847871849, -117.9062500020483952 ) ) ;
#31395 = CARTESIAN_POINT ( 'NONE',  ( 5.405949406249999534, 9.363379034771803333, -154.2812500020484094 ) ) ;
#31396 = LINE ( 'NONE', #8304, #24112 ) ;
#31397 = CARTESIAN_POINT ( 'NONE',  ( 10.81189881249999729, 0.000000000000000000, -46.53125000204838813 ) ) ;
#31398 = CARTESIAN_POINT ( 'NONE',  ( 10.00000000000000000, 5.773502691896255534, -128.2500000040967620 ) ) ;
#31399 = CARTESIAN_POINT ( 'NONE',  ( -4.999999999999996447, 8.660254037844387298, -98.99999999999998579 ) ) ;
#31400 = EDGE_LOOP ( 'NONE', ( #27906, #9777, #19119, #8313 ) ) ;
#31401 = AXIS2_PLACEMENT_3D ( 'NONE', #13842, #24236, #34163 ) ;
#31402 = CARTESIAN_POINT ( 'NONE',  ( 5.405949406249992428, -9.363379034771808662, -129.2812500020483810 ) ) ;
#31403 = CARTESIAN_POINT ( 'NONE',  ( -9.999999999999998224, 1.224646799147353059E-15, -147.1250000040967905 ) ) ;
#31404 = CARTESIAN_POINT ( 'NONE',  ( 9.999999999999998224, 0.000000000000000000, -192.8750000040967905 ) ) ;
#31405 = CARTESIAN_POINT ( 'NONE',  ( 10.81189881249999551, -6.242252689847874514, -180.1562500020484379 ) ) ;
#31406 = ORIENTED_EDGE ( 'NONE', *, *, #19513, .F. ) ;
#31407 = CARTESIAN_POINT ( 'NONE',  ( -10.81189881249999729, 6.242252689847871849, -171.7187500020483810 ) ) ;
#31408 = CARTESIAN_POINT ( 'NONE',  ( 4.999999999999992006, -8.660254037844389075, -61.12500000409676204 ) ) ;
#31409 = CARTESIAN_POINT ( 'NONE',  ( -1.040834085586084257E-14, 145.0000000000000000, 22.49999999999999289 ) ) ;
#31410 = CARTESIAN_POINT ( 'NONE',  ( -4.999999999999996447, 8.660254037844387298, -171.3750000040968189 ) ) ;
#31411 = CARTESIAN_POINT ( 'NONE',  ( -2.293366432827344421E-15, -12.48450537969573659, -67.90625000204838102 ) ) ;
#31412 = CARTESIAN_POINT ( 'NONE',  ( -4.999999999999996447, 8.660254037844387298, -43.87500000409677625 ) ) ;
#31413 = CARTESIAN_POINT ( 'NONE',  ( -5.405949406249996869, 9.363379034771805109, -3.843750002048368586 ) ) ;
#31414 = CARTESIAN_POINT ( 'NONE',  ( -10.81189881249999907, -6.242252689847864744, -165.6562500020483810 ) ) ;
#31415 = FACE_OUTER_BOUND ( 'NONE', #12387, .T. ) ;
#31416 = CARTESIAN_POINT ( 'NONE',  ( 9.999999999999998224, 0.000000000000000000, -112.9999999999999858 ) ) ;
#31417 = ORIENTED_EDGE ( 'NONE', *, *, #23199, .F. ) ;
#31418 = CARTESIAN_POINT ( 'NONE',  ( 10.00000000000102318, -5.773502691895667560, -0.6249999999999450440 ) ) ;
#31419 = CARTESIAN_POINT ( 'NONE',  ( -9.999999999999612754, -5.773502691896474914, -154.1249999999999716 ) ) ;
#31420 = CIRCLE ( 'NONE', #23829, 57.00000000000002132 ) ;
#31421 = CARTESIAN_POINT ( 'NONE',  ( -2.121150477449813534E-15, -11.54700538379251284, -163.2500000040968189 ) ) ;
#31423 = ORIENTED_EDGE ( 'NONE', *, *, #28393, .T. ) ;
#31422 = CARTESIAN_POINT ( 'NONE',  ( -5.405949406249996869, 9.363379034771805109, -79.03125000204838102 ) ) ;
#31424 = CARTESIAN_POINT ( 'NONE',  ( 10.81189881249999729, 0.000000000000000000, -199.4375000020484094 ) ) ;
#31426 = ORIENTED_EDGE ( 'NONE', *, *, #27004, .T. ) ;
#31425 = CARTESIAN_POINT ( 'NONE',  ( -9.999999999999998224, 1.224646799147353059E-15, -200.0000000000000000 ) ) ;
#31427 = ORIENTED_EDGE ( 'NONE', *, *, #34897, .T. ) ;
#31428 = CARTESIAN_POINT ( 'NONE',  ( -5.405949406249996869, 9.363379034771805109, -39.84375000204837391 ) ) ;
#31429 = CARTESIAN_POINT ( 'NONE',  ( -2.121150477449813534E-15, -11.54700538379251284, -186.8750000000000000 ) ) ;
#31430 = CARTESIAN_POINT ( 'NONE',  ( -10.81189881249999729, 1.324075727343319199E-15, -15.78125000204835793 ) ) ;
#31432 = ORIENTED_EDGE ( 'NONE', *, *, #26353, .T. ) ;
#31431 = CARTESIAN_POINT ( 'NONE',  ( -10.81189881249999907, -6.242252689847864744, -64.96875000204838102 ) ) ;
#31433 = DIRECTION ( 'NONE',  ( -1.000000000000000000, 0.000000000000000000, 0.000000000000000000 ) ) ;
#31434 = EDGE_CURVE ( 'NONE', #26359, #468, #31846, .T. ) ;
#31435 = CARTESIAN_POINT ( 'NONE',  ( 5.000000000000000000, 8.660254037844385522, -37.74999999999997868 ) ) ;
#31436 = CARTESIAN_POINT ( 'NONE',  ( -10.81189881249999729, 6.242252689847871849, -197.2187500020484379 ) ) ;
#31437 = CARTESIAN_POINT ( 'NONE',  ( 10.81189881249999729, 0.000000000000000000, -175.3437500020483810 ) ) ;
#31438 = CARTESIAN_POINT ( 'NONE',  ( -10.81189881249999907, -6.242252689847864744, -163.9687500020484094 ) ) ;
#31439 = CARTESIAN_POINT ( 'NONE',  ( 7.644554776091147741E-16, 12.48450537969573659, -176.4687500020484094 ) ) ;
#31440 = CARTESIAN_POINT ( 'NONE',  ( 7.071067811865472841, -7.071067811865472841, -200.0000000000000000 ) ) ;
#31441 = CARTESIAN_POINT ( 'NONE',  ( 10.00000000000025402, -5.773502691896113426, -126.6249999999999858 ) ) ;
#31442 = CARTESIAN_POINT ( 'NONE',  ( -9.999999999999998224, 1.224646799147353059E-15, -191.7500000000000000 ) ) ;
#31443 = CARTESIAN_POINT ( 'NONE',  ( -10.81189881249999729, 1.324075727343319199E-15, -111.5937500020483810 ) ) ;
#31444 = LINE ( 'NONE', #15224, #9403 ) ;
#31445 = CARTESIAN_POINT ( 'NONE',  ( -10.81189881249999729, 6.242252689847871849, -84.90625000204838102 ) ) ;
#31446 = CARTESIAN_POINT ( 'NONE',  ( -2.293366432827344421E-15, -12.48450537969573659, -94.71875000204838102 ) ) ;
#31447 = CARTESIAN_POINT ( 'NONE',  ( 10.81189881249999729, 0.000000000000000000, -59.84375000204835970 ) ) ;
#31448 = CARTESIAN_POINT ( 'NONE',  ( -2.293366432827344421E-15, -12.48450537969573659, -67.90625000204838102 ) ) ;
#31449 = CARTESIAN_POINT ( 'NONE',  ( 5.000000000000000000, 8.660254037844385522, -152.1250000040967905 ) ) ;
#31450 = CARTESIAN_POINT ( 'NONE',  ( -5.000000000000003553, -8.660254037844383745, -122.5000000000000000 ) ) ;
#31451 = CARTESIAN_POINT ( 'NONE',  ( -5.405949406250003975, -9.363379034771801557, -147.5312500020483810 ) ) ;
#31452 = CARTESIAN_POINT ( 'NONE',  ( -5.405949406249996869, 9.363379034771805109, -166.0312500020484094 ) ) ;
#31453 = DIRECTION ( 'NONE',  ( -1.000000000000000000, 0.000000000000000000, 0.000000000000000000 ) ) ;
#31454 = CARTESIAN_POINT ( 'NONE',  ( 10.70731569305672615, 1.500182182589836044, 0.000000000000000000 ) ) ;
#31455 = CARTESIAN_POINT ( 'NONE',  ( 5.405949406249999534, 9.363379034771803333, -95.59375000204838102 ) ) ;
#31456 = ORIENTED_EDGE ( 'NONE', *, *, #27172, .F. ) ;
#31457 = CARTESIAN_POINT ( 'NONE',  ( 10.00000000000000000, 5.773502691896255534, -61.87499999999998579 ) ) ;
#31458 = CARTESIAN_POINT ( 'NONE',  ( 5.405949406249992428, -9.363379034771808662, -198.0937500020484094 ) ) ;
#31459 = CARTESIAN_POINT ( 'NONE',  ( -9.999999999999998224, 5.773502691896259087, -85.75000000409676204 ) ) ;
#31460 = CARTESIAN_POINT ( 'NONE',  ( -9.999999999999479527, -5.773502691896549521, -142.5000000040967620 ) ) ;
#31461 = CARTESIAN_POINT ( 'NONE',  ( 7.644554776091147741E-16, 12.48450537969573659, -92.65625000204839523 ) ) ;
#31462 = CARTESIAN_POINT ( 'NONE',  ( 10.81189881249999551, -6.242252689847874514, -76.65625000204838102 ) ) ;
#31463 =( BOUNDED_CURVE ( )  B_SPLINE_CURVE ( 2, ( #40325, #20484, #23738, #27398, #36680, #1290, #40122 ),
 .UNSPECIFIED., .F., .F. ) 
 B_SPLINE_CURVE_WITH_KNOTS ( ( 3, 2, 2, 3 ),
 ( 0.3283582089552238847, 0.3296019900497513255, 0.3308457711442787108, 0.3320895522388061516 ),
 .UNSPECIFIED. ) 
 CURVE ( )  GEOMETRIC_REPRESENTATION_ITEM ( )  RATIONAL_B_SPLINE_CURVE ( ( 1.000000000000000000, 0.8660254037844387076, 1.000000000000000000, 0.8660254037844387076, 1.000000000000000000, 0.8660254037844207220, 1.000000000000017986 ) ) 
 REPRESENTATION_ITEM ( '' )  );
#31464 = CARTESIAN_POINT ( 'NONE',  ( 7.070501591499377789E-16, 11.54700538379251284, -65.00000000409677625 ) ) ;
#31465 = CARTESIAN_POINT ( 'NONE',  ( -9.999999999999998224, 1.224646799147353059E-15, -69.12500000409677625 ) ) ;
#31466 = CARTESIAN_POINT ( 'NONE',  ( -5.405949406250003975, -9.363379034771801557, -24.34375000204835970 ) ) ;
#31467 = ORIENTED_EDGE ( 'NONE', *, *, #13116, .T. ) ;
#31468 = CARTESIAN_POINT ( 'NONE',  ( 7.070501591499377789E-16, 11.54700538379251284, -3.124999999999951150 ) ) ;
#31469 = CARTESIAN_POINT ( 'NONE',  ( -10.81189881249999729, 1.324075727343319199E-15, -21.78125000204836326 ) ) ;
#31470 = CARTESIAN_POINT ( 'NONE',  ( 10.81189881249999729, 6.242252689847867408, -14.71875000204836859 ) ) ;
#31471 = CARTESIAN_POINT ( 'NONE',  ( 5.000000000000000000, 8.660254037844385522, -142.7500000000000000 ) ) ;
#31472 = CARTESIAN_POINT ( 'NONE',  ( -2.293366432827344421E-15, -12.48450537969573659, -139.7187500020483810 ) ) ;
#31473 = CARTESIAN_POINT ( 'NONE',  ( 9.999999999999998224, 0.000000000000000000, -123.5000000000000000 ) ) ;
#31474 = CARTESIAN_POINT ( 'NONE',  ( 10.81189881249999729, 0.000000000000000000, -129.0312500020484094 ) ) ;
#31475 =( BOUNDED_CURVE ( )  B_SPLINE_CURVE ( 2, ( #40865, #8092, #2052, #41521, #31192, #15183, #28379 ),
 .UNSPECIFIED., .F., .F. ) 
 B_SPLINE_CURVE_WITH_KNOTS ( ( 3, 2, 2, 3 ),
 ( 0.6492537313432837909, 0.6504975124378111762, 0.6517412935323385614, 0.6529850746268659467 ),
 .UNSPECIFIED. ) 
 CURVE ( )  GEOMETRIC_REPRESENTATION_ITEM ( )  RATIONAL_B_SPLINE_CURVE ( ( 0.9999999999999761302, 0.8660254037844625774, 1.000000000000000000, 0.8660254037844387076, 1.000000000000000000, 0.8660254037844148378, 1.000000000000023981 ) ) 
 REPRESENTATION_ITEM ( '' )  );
#31476 = CARTESIAN_POINT ( 'NONE',  ( 4.999999999999992006, -8.660254037844389075, -182.2500000000000000 ) ) ;
#31477 = LINE ( 'NONE', #35774, #11721 ) ;
#31479 = ORIENTED_EDGE ( 'NONE', *, *, #25981, .F. ) ;
#31478 = CARTESIAN_POINT ( 'NONE',  ( -5.405949406249996869, 9.363379034771805109, -101.5312500020483952 ) ) ;
#31480 = LINE ( 'NONE', #27591, #27603 ) ;
#31481 = ORIENTED_EDGE ( 'NONE', *, *, #35386, .T. ) ;
#31482 = CIRCLE ( 'NONE', #12747, 45.00000000000000711 ) ;
#31483 = ORIENTED_EDGE ( 'NONE', *, *, #33653, .F. ) ;
#31484 = CARTESIAN_POINT ( 'NONE',  ( -10.81189881249999907, -6.242252689847864744, -38.15625000204835260 ) ) ;
#31485 = APPROVAL_ROLE ( '' ) ;
#31486 = CARTESIAN_POINT ( 'NONE',  ( 10.81189881249999551, -6.242252689847874514, -83.96875000204838102 ) ) ;
#31487 = CARTESIAN_POINT ( 'NONE',  ( 9.999999999999742428, 5.773502691896404748, -128.2500000040967905 ) ) ;
#31488 = EDGE_CURVE ( 'NONE', #17896, #37898, #30455, .T. ) ;
#31489 = CARTESIAN_POINT ( 'NONE',  ( 9.999999999999998224, 1.224646799147353059E-15, -99.99999999999998579 ) ) ;
#31490 = EDGE_CURVE ( 'NONE', #32484, #40773, #16533, .T. ) ;
#31491 = EDGE_CURVE ( 'NONE', #18815, #3542, #30879, .T. ) ;
#31492 = EDGE_CURVE ( 'NONE', #9851, #35407, #7062, .T. ) ;
#31493 = CARTESIAN_POINT ( 'NONE',  ( 0.000000000000000000, 0.000000000000000000, -200.0000000000000000 ) ) ;
#31494 = CARTESIAN_POINT ( 'NONE',  ( -2.293366432827344421E-15, -12.48450537969573659, -168.4062500020483810 ) ) ;
#31495 = CARTESIAN_POINT ( 'NONE',  ( 9.999999999999998224, 0.000000000000000000, -85.99999999999998579 ) ) ;
#31496 = CARTESIAN_POINT ( 'NONE',  ( -10.81189881249999729, 6.242252689847871849, -116.2187500020483810 ) ) ;
#31497 = PRODUCT ( 'BR-597', 'BR-597', '', ( #26417 ) ) ;
#31498 = APPROVAL ( #40517, 'UNSPECIFIED' ) ;
#31499 = CARTESIAN_POINT ( 'NONE',  ( -5.405949406250003975, -9.363379034771801557, -85.84375000204836681 ) ) ;
#31500 = DIRECTION ( 'NONE',  ( 1.000000000000000000, 0.000000000000000000, 0.000000000000000000 ) ) ;
#31501 = CARTESIAN_POINT ( 'NONE',  ( -10.81189881249999729, 1.324075727343319199E-15, -197.0937500020484094 ) ) ;
#31502 = CARTESIAN_POINT ( 'NONE',  ( -10.81189881249999729, 1.324075727343319199E-15, -95.28125000204838102 ) ) ;
#31503 = CARTESIAN_POINT ( 'NONE',  ( -9.999999999999998224, 1.224646799147353059E-15, -178.6250000040968189 ) ) ;
#31504 = CARTESIAN_POINT ( 'NONE',  ( 10.81189881249999729, 0.000000000000000000, -174.0312500020484094 ) ) ;
#31505 = CARTESIAN_POINT ( 'NONE',  ( -5.000000000000003553, -8.660254037844383745, -70.37500000409677625 ) ) ;
#31506 = CARTESIAN_POINT ( 'NONE',  ( -10.81189881249999729, -6.242252689847864744, -177.6562500020484094 ) ) ;
#31507 = CARTESIAN_POINT ( 'NONE',  ( 10.81189881249999907, 6.242252689847868297, -188.9062500020484379 ) ) ;
#31508 = CARTESIAN_POINT ( 'NONE',  ( 5.405949406249992428, -9.363379034771808662, -43.59375000204837391 ) ) ;
#31509 = CARTESIAN_POINT ( 'NONE',  ( -2.121150477449813534E-15, -11.54700538379251284, -167.7500000040968189 ) ) ;
#31510 = CARTESIAN_POINT ( 'NONE',  ( -10.81189881249999907, -6.242252689847864744, -2.156250002048373915 ) ) ;
#31511 = CARTESIAN_POINT ( 'NONE',  ( 5.405949406249992428, -9.363379034771808662, -13.59375000204834905 ) ) ;
#31512 = CARTESIAN_POINT ( 'NONE',  ( -9.999999999999998224, 1.224646799147353059E-15, -61.24999999999997158 ) ) ;
#31513 = CARTESIAN_POINT ( 'NONE',  ( 5.405949406249992428, -9.363379034771808662, -120.0937500020483952 ) ) ;
#31514 = CARTESIAN_POINT ( 'NONE',  ( 9.999999999999996447, -5.773502691896262640, -99.62500000000000000 ) ) ;
#31515 = CARTESIAN_POINT ( 'NONE',  ( -5.405949406249996869, 9.363379034771805109, -22.03125000204836326 ) ) ;
#31516 = CARTESIAN_POINT ( 'NONE',  ( 5.000000000000000000, 8.660254037844385522, -102.6250000040967905 ) ) ;
#31517 = EDGE_CURVE ( 'NONE', #16629, #33917, #34863, .T. ) ;
#31518 = CARTESIAN_POINT ( 'NONE',  ( 7.070501591499376803E-16, 11.54700538379251284, -82.62500000000000000 ) ) ;
#31519 = CARTESIAN_POINT ( 'NONE',  ( -2.121150477449813534E-15, -11.54700538379251284, -54.87499999999997868 ) ) ;
#31520 = CARTESIAN_POINT ( 'NONE',  ( 10.81189881249999729, 0.000000000000000000, -115.5312500020483952 ) ) ;
#31521 = CARTESIAN_POINT ( 'NONE',  ( -5.405949406250003975, -9.363379034771801557, -99.53125000204839523 ) ) ;
#31522 = EDGE_LOOP ( 'NONE', ( #30209, #21423, #20809, #23617 ) ) ;
#31523 = CARTESIAN_POINT ( 'NONE',  ( -4.999999999999996447, 8.660254037844387298, -93.37500000409677625 ) ) ;
#31524 = CARTESIAN_POINT ( 'NONE',  ( 5.000000000000000000, 8.660254037844385522, -91.74999999999998579 ) ) ;
#31525 = CARTESIAN_POINT ( 'NONE',  ( -5.405949406249996869, 9.363379034771805109, -155.5312500020484094 ) ) ;
#31526 = CARTESIAN_POINT ( 'NONE',  ( -5.405949406249996869, 9.363379034771805109, -51.84375000204835260 ) ) ;
#31528 = EDGE_CURVE ( 'NONE', #13549, #39100, #14398, .T. ) ;
#31527 = ORIENTED_EDGE ( 'NONE', *, *, #38238, .T. ) ;
#31529 = CARTESIAN_POINT ( 'NONE',  ( 10.00000000000000000, 5.773502691896255534, -24.37499999999998579 ) ) ;
#31530 = CARTESIAN_POINT ( 'NONE',  ( -5.405949406249996869, 9.363379034771805109, -26.53125000204836681 ) ) ;
#31531 = CARTESIAN_POINT ( 'NONE',  ( -9.999999999999998224, 1.224646799147353059E-15, -160.2500000000000000 ) ) ;
#31532 = CARTESIAN_POINT ( 'NONE',  ( -9.999999999999998224, 5.773502691896259087, -18.25000000409676559 ) ) ;
#31533 = CARTESIAN_POINT ( 'NONE',  ( 9.999999999999998224, 0.000000000000000000, -200.0000000000000000 ) ) ;
#31534 = CARTESIAN_POINT ( 'NONE',  ( -5.405949406250003975, -9.363379034771801557, -132.5312500020484094 ) ) ;
#31535 = CARTESIAN_POINT ( 'NONE',  ( 7.070501591499376803E-16, 11.54700538379251284, -46.62499999999996447 ) ) ;
#31536 = ADVANCED_FACE ( 'NONE', ( #7270 ), #27123, .T. ) ;
#31537 = DIRECTION ( 'NONE',  ( 0.000000000000000000, 0.000000000000000000, 1.000000000000000000 ) ) ;
#31538 = ORIENTED_EDGE ( 'NONE', *, *, #4281, .F. ) ;
#31539 = CARTESIAN_POINT ( 'NONE',  ( -2.293366432827344421E-15, -12.48450537969573659, -60.40625000204839523 ) ) ;
#31540 = COORDINATED_UNIVERSAL_TIME_OFFSET ( 6, 0, .AHEAD. ) ;
#31542 = ORIENTED_EDGE ( 'NONE', *, *, #32567, .T. ) ;
#31541 = ORIENTED_EDGE ( 'NONE', *, *, #38726, .T. ) ;
#31543 =( BOUNDED_CURVE ( )  B_SPLINE_CURVE ( 2, ( #4728, #21561, #31505, #34742, #18742, #11404, #38388 ),
 .UNSPECIFIED., .F., .F. ) 
 B_SPLINE_CURVE_WITH_KNOTS ( ( 3, 2, 2, 3 ),
 ( 0.6380597014925374344, 0.6393034825870648197, 0.6405472636815923160, 0.6417910447761195902 ),
 .UNSPECIFIED. ) 
 CURVE ( )  GEOMETRIC_REPRESENTATION_ITEM ( )  RATIONAL_B_SPLINE_CURVE ( ( 0.9999999999999880096, 0.8660254037844506980, 1.000000000000000000, 0.8660254037844387076, 1.000000000000000000, 0.8660254037844148378, 1.000000000000023981 ) ) 
 REPRESENTATION_ITEM ( '' )  );
#31544 = CARTESIAN_POINT ( 'NONE',  ( -1.040834085586084257E-14, -145.0000000000000000, 22.49999999999999289 ) ) ;
#31545 = CARTESIAN_POINT ( 'NONE',  ( 7.070501591499376803E-16, 11.54700538379251284, -144.5000000040967905 ) ) ;
#31546 = CARTESIAN_POINT ( 'NONE',  ( -5.405949406250003975, -9.363379034771801557, -154.8437500020483810 ) ) ;
#31547 = CARTESIAN_POINT ( 'NONE',  ( -5.405949406249996869, 9.363379034771805109, -187.0312500020484094 ) ) ;
#31548 = CARTESIAN_POINT ( 'NONE',  ( 7.644554776091147741E-16, 12.48450537969573659, -9.968750002048363257 ) ) ;
#31549 = CARTESIAN_POINT ( 'NONE',  ( 10.81189881249999551, -6.242252689847874514, -140.9687500020483810 ) ) ;
#31550 = CARTESIAN_POINT ( 'NONE',  ( -10.81189881249999907, -6.242252689847864744, -96.65625000204839523 ) ) ;
#31551 = CARTESIAN_POINT ( 'NONE',  ( 5.405949406249999534, 9.363379034771803333, -112.0937500020483810 ) ) ;
#31552 = CARTESIAN_POINT ( 'NONE',  ( -10.00000000000015987, 5.773502691896167605, -190.7500000040968757 ) ) ;
#31553 = CARTESIAN_POINT ( 'NONE',  ( 5.405949406249999534, 9.363379034771803333, -118.2812500020483952 ) ) ;
#31554 = CARTESIAN_POINT ( 'NONE',  ( 10.81189881249999551, -6.242252689847874514, -2.968750002048361925 ) ) ;
#31555 = CARTESIAN_POINT ( 'NONE',  ( 5.405949406249992428, -9.363379034771808662, -120.0937500020483952 ) ) ;
#31556 = CARTESIAN_POINT ( 'NONE',  ( 7.644554776091147741E-16, 12.48450537969573659, -194.6562500020484094 ) ) ;
#31557 = DIRECTION ( 'NONE',  ( -1.000000000000000000, 0.000000000000000000, 0.000000000000000000 ) ) ;
#31558 = CARTESIAN_POINT ( 'NONE',  ( 10.00000000000000000, 5.773502691896255534, -144.3750000000000284 ) ) ;
#31559 = CARTESIAN_POINT ( 'NONE',  ( 7.070501591499377789E-16, 11.54700538379251284, -10.62499999999996803 ) ) ;
#31560 = EDGE_CURVE ( 'NONE', #6937, #31960, #39254, .T. ) ;
#31561 = CARTESIAN_POINT ( 'NONE',  ( -2.293366432827344421E-15, -12.48450537969573659, -76.71875000204838102 ) ) ;
#31562 = CARTESIAN_POINT ( 'NONE',  ( 10.81189881249999907, 6.242252689847868297, -58.21875000204836681 ) ) ;
#31563 = CARTESIAN_POINT ( 'NONE',  ( 7.070501591499377789E-16, 11.54700538379251284, -191.0000000040968189 ) ) ;
#31564 = CARTESIAN_POINT ( 'NONE',  ( 10.81189881249999551, -6.242252689847874514, -24.15625000204838102 ) ) ;
#31565 = CARTESIAN_POINT ( 'NONE',  ( 5.405949406249999534, 9.363379034771803333, -38.59375000204837391 ) ) ;
#31566 = CARTESIAN_POINT ( 'NONE',  ( 9.999999999999998224, 0.000000000000000000, -171.8750000040968189 ) ) ;
#31567 = CARTESIAN_POINT ( 'NONE',  ( -10.81189881249999729, 1.324075727343319199E-15, -147.5937500020483810 ) ) ;
#31568 = CARTESIAN_POINT ( 'NONE',  ( 9.999999999999998224, 0.000000000000000000, -122.0000000000000000 ) ) ;
#31569 = LINE ( 'NONE', #41242, #16880 ) ;
#31570 = CARTESIAN_POINT ( 'NONE',  ( -4.999999999999996447, 8.660254037844387298, -74.99999999999998579 ) ) ;
#31571 = CARTESIAN_POINT ( 'NONE',  ( 10.81189881249999907, 6.242252689847868297, -137.9062500020483810 ) ) ;
#31572 = CARTESIAN_POINT ( 'NONE',  ( -10.81189881249999729, 1.324075727343319199E-15, -11.28125000204835438 ) ) ;
#31573 = ORIENTED_EDGE ( 'NONE', *, *, #40425, .F. ) ;
#31574 = CARTESIAN_POINT ( 'NONE',  ( 10.00000000000025402, -5.773502691896113426, -164.1250000000000284 ) ) ;
#31575 = CARTESIAN_POINT ( 'NONE',  ( -5.000000000000003553, -8.660254037844383745, -118.3750000040967905 ) ) ;
#31576 = CARTESIAN_POINT ( 'NONE',  ( -9.999999999999998224, 1.224646799147353059E-15, -140.7500000000000000 ) ) ;
#31577 = CARTESIAN_POINT ( 'NONE',  ( -10.81189881249999729, 6.242252689847871849, -71.21875000204839523 ) ) ;
#31578 = CARTESIAN_POINT ( 'NONE',  ( -10.00000000000000000, -5.773502691896251982, -30.00000000409675494 ) ) ;
#31579 = CARTESIAN_POINT ( 'NONE',  ( 10.00000000000051159, -5.773502691895965988, -2.500000004096743833 ) ) ;
#31580 = CARTESIAN_POINT ( 'NONE',  ( 10.81189881249999729, 0.000000000000000000, -48.03125000204838813 ) ) ;
#31581 = DIRECTION ( 'NONE',  ( 0.000000000000000000, 0.000000000000000000, -1.000000000000000000 ) ) ;
#31582 = CARTESIAN_POINT ( 'NONE',  ( 7.644554776091147741E-16, 12.48450537969573659, -143.6562500020484094 ) ) ;
#31583 = CARTESIAN_POINT ( 'NONE',  ( 5.405949406249999534, 9.363379034771803333, -128.5937500020483810 ) ) ;
#31584 = LINE ( 'NONE', #34820, #15817 ) ;
#31585 = FACE_OUTER_BOUND ( 'NONE', #12133, .T. ) ;
#31586 = ORIENTED_EDGE ( 'NONE', *, *, #40946, .F. ) ;
#31587 =( BOUNDED_CURVE ( )  B_SPLINE_CURVE ( 2, ( #34268, #5328, #8146, #18051, #4684, #18483, #31246 ),
 .UNSPECIFIED., .F., .F. ) 
 B_SPLINE_CURVE_WITH_KNOTS ( ( 3, 2, 2, 3 ),
 ( 0.1343283582089551953, 0.1355721393034825528, 0.1368159203980099381, 0.1380597014925373234 ),
 .UNSPECIFIED. ) 
 CURVE ( )  GEOMETRIC_REPRESENTATION_ITEM ( )  RATIONAL_B_SPLINE_CURVE ( ( 1.000000000000003109, 0.8660254037844358210, 1.000000000000000000, 0.8660254037844387076, 1.000000000000000000, 0.8660254037844387076, 1.000000000000000000 ) ) 
 REPRESENTATION_ITEM ( '' )  );
#31588 = ORIENTED_EDGE ( 'NONE', *, *, #30717, .F. ) ;
#31589 = VECTOR ( 'NONE', #41972, 1000.000000000000000 ) ;
#31590 = ORIENTED_EDGE ( 'NONE', *, *, #14281, .F. ) ;
#31591 = DIRECTION ( 'NONE',  ( -0.000000000000000000, -0.000000000000000000, 1.000000000000000000 ) ) ;
#31592 = CARTESIAN_POINT ( 'NONE',  ( -10.81189881249999907, -6.242252689847864744, -183.4687500020484379 ) ) ;
#31593 = CARTESIAN_POINT ( 'NONE',  ( 5.405949406249999534, 9.363379034771803333, -32.59375000204836681 ) ) ;
#31594 = CARTESIAN_POINT ( 'NONE',  ( -2.121150477449813534E-15, -11.54700538379251284, -41.37499999999997158 ) ) ;
#31595 = CARTESIAN_POINT ( 'NONE',  ( 10.81189881249999551, -6.242252689847874514, -175.4687500020484094 ) ) ;
#31596 = CARTESIAN_POINT ( 'NONE',  ( 10.81189881249999907, 6.242252689847868297, -155.7187500020483810 ) ) ;
#31597 = CYLINDRICAL_SURFACE ( 'NONE', #10712, 9.999999999999998224 ) ;
#31598 = CARTESIAN_POINT ( 'NONE',  ( 7.644554776091147741E-16, 12.48450537969573659, -137.4687500020483810 ) ) ;
#31599 = CARTESIAN_POINT ( 'NONE',  ( -2.293366432827344421E-15, -12.48450537969573659, -144.4062500020484094 ) ) ;
#31600 = CARTESIAN_POINT ( 'NONE',  ( -10.81189881249999729, 1.324075727343319199E-15, -144.5937500020483810 ) ) ;
#31601 = LINE ( 'NONE', #31823, #11593 ) ;
#31602 = CARTESIAN_POINT ( 'NONE',  ( 5.000000000000000000, 8.660254037844385522, -169.7500000000000000 ) ) ;
#31603 = CARTESIAN_POINT ( 'NONE',  ( 5.000000000000000000, 8.660254037844385522, -169.7500000000000000 ) ) ;
#31604 = ADVANCED_FACE ( 'NONE', ( #36828 ), #30374, .T. ) ;
#31605 = CARTESIAN_POINT ( 'NONE',  ( 10.81189881249999729, 0.000000000000000000, -82.34375000204836681 ) ) ;
#31606 = CARTESIAN_POINT ( 'NONE',  ( 0.000000000000000000, 0.000000000000000000, -99.99999999999998579 ) ) ;
#31607 = CARTESIAN_POINT ( 'NONE',  ( 5.405949406249999534, 9.363379034771803333, -56.78125000204836681 ) ) ;
#31608 = CARTESIAN_POINT ( 'NONE',  ( -10.18354000214830002, 2.855663046881824485, -99.99999999999992895 ) ) ;
#31609 = CARTESIAN_POINT ( 'NONE',  ( -5.405949406250003975, -9.363379034771801557, -166.8437500020484094 ) ) ;
#31610 = CARTESIAN_POINT ( 'NONE',  ( -2.293366432827344421E-15, -12.48450537969573659, -114.4062500020483952 ) ) ;
#31611 = CARTESIAN_POINT ( 'NONE',  ( -5.405949406249996869, 9.363379034771805109, -145.0312500020483810 ) ) ;
#31612 = CARTESIAN_POINT ( 'NONE',  ( 5.000000000000000000, 8.660254037844385522, -143.1250000040967905 ) ) ;
#31613 = CARTESIAN_POINT ( 'NONE',  ( 5.405949406249992428, -9.363379034771808662, -43.78125000204838102 ) ) ;
#31614 = CARTESIAN_POINT ( 'NONE',  ( 4.999999999999992006, -8.660254037844389075, -122.6250000040967905 ) ) ;
#31615 = CARTESIAN_POINT ( 'NONE',  ( -10.00000000000000000, -5.773502691896251982, -95.62499999999998579 ) ) ;
#31616 = VERTEX_POINT ( 'NONE', #23250 ) ;
#31617 = CARTESIAN_POINT ( 'NONE',  ( -5.405949406250003975, -9.363379034771801557, -129.5312500020484094 ) ) ;
#31618 = CARTESIAN_POINT ( 'NONE',  ( -5.000000000000003553, -8.660254037844383745, -136.3750000040967905 ) ) ;
#31619 = CARTESIAN_POINT ( 'NONE',  ( -4.999999999999996447, 8.660254037844387298, -192.3750000040967905 ) ) ;
#31620 = CARTESIAN_POINT ( 'NONE',  ( 10.81189881249999907, 6.242252689847868297, -176.9062500020484094 ) ) ;
#31621 = ORIENTED_EDGE ( 'NONE', *, *, #651, .T. ) ;
#31622 = CARTESIAN_POINT ( 'NONE',  ( -10.81189881249999907, -6.242252689847864744, -174.4687500020484094 ) ) ;
#31623 = CARTESIAN_POINT ( 'NONE',  ( 4.999999999999992006, -8.660254037844389075, -47.62500000409677625 ) ) ;
#31624 = AXIS2_PLACEMENT_3D ( 'NONE', #40746, #27606, #31500 ) ;
#31625 = CARTESIAN_POINT ( 'NONE',  ( 0.000000000000000000, 0.000000000000000000, -200.0000000000000000 ) ) ;
#31626 = CARTESIAN_POINT ( 'NONE',  ( 0.000000000000000000, 0.000000000000000000, -180.0000000000000000 ) ) ;
#31627 = CARTESIAN_POINT ( 'NONE',  ( -5.405949406249996869, 9.363379034771805109, -71.53125000204838102 ) ) ;
#31628 = EDGE_CURVE ( 'NONE', #30921, #2425, #40265, .T. ) ;
#31629 = CARTESIAN_POINT ( 'NONE',  ( 9.999999999999996447, -5.773502691896262640, -43.00000000409676915 ) ) ;
#31630 = CARTESIAN_POINT ( 'NONE',  ( 7.644554776091147741E-16, 12.48450537969573659, -3.968750002048354819 ) ) ;
#31631 = DIRECTION ( 'NONE',  ( 1.000000000000000000, 0.000000000000000000, 0.000000000000000000 ) ) ;
#31632 = CARTESIAN_POINT ( 'NONE',  ( 10.81189881249999907, 6.242252689847868297, -170.9062500020484094 ) ) ;
#31633 = DIRECTION ( 'NONE',  ( -0.4999999999999997224, -0.8660254037844388186, 0.000000000000000000 ) ) ;
#31634 = CARTESIAN_POINT ( 'NONE',  ( 5.000000000000000000, 8.660254037844385522, -64.74999999999997158 ) ) ;
#31635 = EDGE_LOOP ( 'NONE', ( #41908, #40459, #28376, #1686 ) ) ;
#31636 = CARTESIAN_POINT ( 'NONE',  ( -9.999999999999998224, 1.224646799147353059E-15, -1.249999999999973355 ) ) ;
#31637 = CARTESIAN_POINT ( 'NONE',  ( 9.999999999999742428, 5.773502691896404748, -123.7500000040967763 ) ) ;
#31639 = ORIENTED_EDGE ( 'NONE', *, *, #34818, .T. ) ;
#31638 = CARTESIAN_POINT ( 'NONE',  ( 5.405949406249992428, -9.363379034771808662, -76.78125000204838102 ) ) ;
#31640 =( LENGTH_UNIT ( ) NAMED_UNIT ( * ) SI_UNIT ( .MILLI., .METRE. ) );
#31642 = EDGE_LOOP ( 'NONE', ( #3581, #14918, #30336, #30186 ) ) ;
#31641 = CARTESIAN_POINT ( 'NONE',  ( -5.000000000000003553, -8.660254037844383745, -188.8750000040967905 ) ) ;
#31643 = VERTEX_POINT ( 'NONE', #3827 ) ;
#31644 = CARTESIAN_POINT ( 'NONE',  ( -5.405949406250003975, -9.363379034771801557, -25.84375000204835970 ) ) ;
#31645 = FACE_OUTER_BOUND ( 'NONE', #27540, .T. ) ;
#31646 = CARTESIAN_POINT ( 'NONE',  ( 10.81189881249999729, 0.000000000000000000, -7.531250002048350822 ) ) ;
#31648 = ORIENTED_EDGE ( 'NONE', *, *, #28081, .F. ) ;
#31647 = CARTESIAN_POINT ( 'NONE',  ( -2.293366432827344421E-15, -12.48450537969573659, -55.71875000204837391 ) ) ;
#31649 = CARTESIAN_POINT ( 'NONE',  ( 7.070501591499377789E-16, 11.54700538379251284, -34.62499999999995737 ) ) ;
#31650 = AXIS2_PLACEMENT_3D ( 'NONE', #17719, #20757, #30702 ) ;
#31651 = CARTESIAN_POINT ( 'NONE',  ( -5.405949406249996869, 9.363379034771805109, -195.8437500020484094 ) ) ;
#31652 = CARTESIAN_POINT ( 'NONE',  ( 10.81189881249999729, 0.000000000000000000, -179.8437500020483810 ) ) ;
#31653 = CARTESIAN_POINT ( 'NONE',  ( -5.405949406250003975, -9.363379034771801557, -159.3437500020484094 ) ) ;
#31655 = EDGE_CURVE ( 'NONE', #16738, #12651, #17817, .T. ) ;
#31654 = CARTESIAN_POINT ( 'NONE',  ( 7.644554776091147741E-16, 12.48450537969573659, -174.9687500020484094 ) ) ;
#31656 = LINE ( 'NONE', #28629, #12965 ) ;
#31657 = CARTESIAN_POINT ( 'NONE',  ( -4.999999999999996447, 8.660254037844387298, -198.0000000000000000 ) ) ;
#31658 = VECTOR ( 'NONE', #3415, 1000.000000000000000 ) ;
#31659 = CARTESIAN_POINT ( 'NONE',  ( 10.81189881249999729, 0.000000000000000000, -106.3437500020483810 ) ) ;
#31660 = CARTESIAN_POINT ( 'NONE',  ( 9.999999999999998224, 0.000000000000000000, -191.3750000040967905 ) ) ;
#31661 = CARTESIAN_POINT ( 'NONE',  ( -10.81189881249999729, 1.324075727343319199E-15, -80.28125000204838102 ) ) ;
#31662 = CARTESIAN_POINT ( 'NONE',  ( -10.81189881249999729, 6.242252689847871849, -93.71875000204838102 ) ) ;
#31663 = CARTESIAN_POINT ( 'NONE',  ( 5.405949406249992428, -9.363379034771808662, -66.28125000204838102 ) ) ;
#31664 = CARTESIAN_POINT ( 'NONE',  ( -10.00000000000000000, -5.773502691896251982, -142.5000000040967905 ) ) ;
#31665 = CARTESIAN_POINT ( 'NONE',  ( 9.999999999999998224, 0.000000000000000000, -126.5000000000000000 ) ) ;
#31666 = ORIENTED_EDGE ( 'NONE', *, *, #1721, .T. ) ;
#31667 = AXIS2_PLACEMENT_3D ( 'NONE', #22727, #35892, #6329 ) ;
#31668 = CARTESIAN_POINT ( 'NONE',  ( 7.644554776091147741E-16, 12.48450537969573659, -149.6562500020484094 ) ) ;
#31669 = CARTESIAN_POINT ( 'NONE',  ( 10.81189881249999907, 6.242252689847868297, -160.4062500020484094 ) ) ;
#31670 = CARTESIAN_POINT ( 'NONE',  ( 4.999999999999992006, -8.660254037844389075, -39.74999999999997868 ) ) ;
#31671 = CYLINDRICAL_SURFACE ( 'NONE', #17137, 9.999999999999998224 ) ;
#31672 = CARTESIAN_POINT ( 'NONE',  ( 5.405949406249999534, 9.363379034771803333, -101.5937500020483810 ) ) ;
#31673 = ORIENTED_EDGE ( 'NONE', *, *, #14492, .T. ) ;
#31674 = CARTESIAN_POINT ( 'NONE',  ( 9.999999999999998224, 0.000000000000000000, -67.99999999999997158 ) ) ;
#31675 = CARTESIAN_POINT ( 'NONE',  ( -5.405949406250003975, -9.363379034771801557, -193.8437500020484094 ) ) ;
#31676 = CARTESIAN_POINT ( 'NONE',  ( -10.00000000000000000, -5.773502691896251982, -79.50000000409679046 ) ) ;
#31677 = FACE_OUTER_BOUND ( 'NONE', #29832, .T. ) ;
#31678 = CARTESIAN_POINT ( 'NONE',  ( 0.000000000000000000, 0.000000000000000000, -200.0000000000000000 ) ) ;
#31679 = CARTESIAN_POINT ( 'NONE',  ( -10.81189881249999729, 6.242252689847871849, -93.90625000204839523 ) ) ;
#31680 = CARTESIAN_POINT ( 'NONE',  ( -10.81189881249999729, 6.242252689847871849, -78.90625000204838102 ) ) ;
#31681 = CARTESIAN_POINT ( 'NONE',  ( -5.000000000000003553, -8.660254037844383745, -65.87500000409676204 ) ) ;
#31682 = CYLINDRICAL_SURFACE ( 'NONE', #36917, 9.999999999999998224 ) ;
#31683 = CARTESIAN_POINT ( 'NONE',  ( 7.644554776091147741E-16, 12.48450537969573659, -23.46875000204837391 ) ) ;
#31684 = ORIENTED_EDGE ( 'NONE', *, *, #25451, .F. ) ;
#31685 = CARTESIAN_POINT ( 'NONE',  ( -10.81189881249999729, 6.242252689847871849, -194.4062500020484094 ) ) ;
#31686 = CARTESIAN_POINT ( 'NONE',  ( 7.644554776091147741E-16, 12.48450537969573659, -22.15625000204837747 ) ) ;
#31687 = EDGE_CURVE ( 'NONE', #39101, #28777, #20850, .T. ) ;
#31688 = CARTESIAN_POINT ( 'NONE',  ( 10.81189881249999729, 6.242252689847867408, -4.218750002048367698 ) ) ;
#31689 = CARTESIAN_POINT ( 'NONE',  ( 4.999999999999992006, -8.660254037844389075, -64.12500000409676204 ) ) ;
#31690 = CARTESIAN_POINT ( 'NONE',  ( -5.405949406249996869, 9.363379034771805109, -144.8437500020483810 ) ) ;
#31691 = CARTESIAN_POINT ( 'NONE',  ( -2.121150477449813534E-15, -11.54700538379251284, -180.8749999999999432 ) ) ;
#31692 = CARTESIAN_POINT ( 'NONE',  ( 9.999999999999994671, -5.773502691896262640, -137.1250000000000000 ) ) ;
#31693 = CARTESIAN_POINT ( 'NONE',  ( 4.999999999999992006, -8.660254037844389075, -171.7500000000000000 ) ) ;
#31694 = CARTESIAN_POINT ( 'NONE',  ( -9.999999999999998224, 1.224646799147353059E-15, -157.6250000040967905 ) ) ;
#31695 = AXIS2_PLACEMENT_3D ( 'NONE', #11749, #8106, #996 ) ;
#31697 = VERTEX_POINT ( 'NONE', #34034 ) ;
#31696 = CARTESIAN_POINT ( 'NONE',  ( 7.644554776091147741E-16, 12.48450537969573659, -100.1562500020483952 ) ) ;
#31698 = CARTESIAN_POINT ( 'NONE',  ( -9.999999999999998224, 1.224646799147353059E-15, -111.1250000040967763 ) ) ;
#31699 = ORIENTED_EDGE ( 'NONE', *, *, #15901, .T. ) ;
#31700 = ORIENTED_EDGE ( 'NONE', *, *, #27310, .F. ) ;
#31701 = CIRCLE ( 'NONE', #39255, 60.00000000000000711 ) ;
#31702 = CARTESIAN_POINT ( 'NONE',  ( -10.81189881249999907, -6.242252689847864744, -29.15625000204835970 ) ) ;
#31703 = PERSON_AND_ORGANIZATION_ROLE ( 'design_supplier' ) ;
#31704 = CARTESIAN_POINT ( 'NONE',  ( 5.405949406249999534, 9.363379034771803333, -91.09375000204838102 ) ) ;
#31705 = CYLINDRICAL_SURFACE ( 'NONE', #37358, 9.999999999999998224 ) ;
#31706 = DIRECTION ( 'NONE',  ( -0.000000000000000000, -0.000000000000000000, -1.000000000000000000 ) ) ;
#31707 =( BOUNDED_CURVE ( )  B_SPLINE_CURVE ( 2, ( #9218, #6204, #2338, #42641, #41797, #12860, #15467 ),
 .UNSPECIFIED., .F., .F. ) 
 B_SPLINE_CURVE_WITH_KNOTS ( ( 3, 2, 2, 3 ),
 ( 0.9850746268656718208, 0.9863184079601992060, 0.9875621890547265913, 0.9888059701492539766 ),
 .UNSPECIFIED. ) 
 CURVE ( )  GEOMETRIC_REPRESENTATION_ITEM ( )  RATIONAL_B_SPLINE_CURVE ( ( 0.9999999999999761302, 0.8660254037844625774, 1.000000000000000000, 0.8660254037844387076, 1.000000000000000000, 0.8660254037844148378, 1.000000000000023981 ) ) 
 REPRESENTATION_ITEM ( '' )  );
#31708 = CARTESIAN_POINT ( 'NONE',  ( 4.999999999999992006, -8.660254037844389075, -127.1250000040967620 ) ) ;
#31709 = CARTESIAN_POINT ( 'NONE',  ( 7.644554776091147741E-16, 12.48450537969573659, -161.6562500020484379 ) ) ;
#31710 = CARTESIAN_POINT ( 'NONE',  ( -5.000000000000003553, -8.660254037844383745, -10.37500000409674605 ) ) ;
#31711 = DIRECTION ( 'NONE',  ( -1.000000000000000000, 0.000000000000000000, 0.000000000000000000 ) ) ;
#31712 = CARTESIAN_POINT ( 'NONE',  ( 10.81189881249999729, 0.000000000000000000, -113.8437500020483810 ) ) ;
#31713 = CARTESIAN_POINT ( 'NONE',  ( -10.81189881249999729, 6.242252689847871849, -86.21875000204838102 ) ) ;
#31714 = CARTESIAN_POINT ( 'NONE',  ( 10.81189881249999551, -6.242252689847874514, -197.9687500020484094 ) ) ;
#31715 = CARTESIAN_POINT ( 'NONE',  ( 10.81189881249999551, -6.242252689847874514, -90.15625000204836681 ) ) ;
#31716 = CARTESIAN_POINT ( 'NONE',  ( 9.999999999999998224, 0.000000000000000000, -179.3750000040967905 ) ) ;
#31717 = CARTESIAN_POINT ( 'NONE',  ( 5.405949406249992428, -9.363379034771808662, -171.2812500020484094 ) ) ;
#31718 =( BOUNDED_CURVE ( )  B_SPLINE_CURVE ( 2, ( #34467, #17388, #7917, #33823, #17819, #37690, #24761 ),
 .UNSPECIFIED., .F., .F. ) 
 B_SPLINE_CURVE_WITH_KNOTS ( ( 3, 2, 2, 3 ),
 ( 0.4738805970149255198, 0.4751243781094529051, 0.4763681592039803459, 0.4776119402985076756 ),
 .UNSPECIFIED. ) 
 CURVE ( )  GEOMETRIC_REPRESENTATION_ITEM ( )  RATIONAL_B_SPLINE_CURVE ( ( 0.9999999999999820144, 0.8660254037844566932, 1.000000000000000000, 0.8660254037844387076, 1.000000000000000000, 0.8660254037844148378, 1.000000000000023981 ) ) 
 REPRESENTATION_ITEM ( '' )  );
#31719 = CARTESIAN_POINT ( 'NONE',  ( 9.999999999999998224, 0.000000000000000000, -150.5000000000000000 ) ) ;
#31720 = CARTESIAN_POINT ( 'NONE',  ( 10.81189881249999551, -6.242252689847874514, -172.6562500020484094 ) ) ;
#31721 = CARTESIAN_POINT ( 'NONE',  ( 10.81189881249999907, 6.242252689847868297, -184.4062500020484094 ) ) ;
#31722 = CARTESIAN_POINT ( 'NONE',  ( -5.405949406250003975, -9.363379034771801557, -43.84375000204837391 ) ) ;
#31723 = VECTOR ( 'NONE', #36442, 1000.000000000000000 ) ;
#31724 = CARTESIAN_POINT ( 'NONE',  ( 7.070501591499377789E-16, 11.54700538379251284, -167.0000000040967905 ) ) ;
#31725 = CARTESIAN_POINT ( 'NONE',  ( -5.405949406249996869, 9.363379034771805109, -2.531250002048373915 ) ) ;
#31726 = CARTESIAN_POINT ( 'NONE',  ( -10.81189881249999729, 6.242252689847871849, -12.71875000204836326 ) ) ;
#31727 = CARTESIAN_POINT ( 'NONE',  ( -9.999999999999998224, 1.224646799147353059E-15, -200.0000000000000000 ) ) ;
#31728 = CARTESIAN_POINT ( 'NONE',  ( -5.405949406249996869, 9.363379034771805109, -119.3437500020483810 ) ) ;
#31729 = CARTESIAN_POINT ( 'NONE',  ( 7.070501591499377789E-16, 11.54700538379251284, -91.62500000000000000 ) ) ;
#31730 = CARTESIAN_POINT ( 'NONE',  ( 10.81189881249999729, 0.000000000000000000, -19.53125000204835970 ) ) ;
#31731 = CARTESIAN_POINT ( 'NONE',  ( -10.00000000000000000, -5.773502691896251982, -108.0000000040967763 ) ) ;
#31732 = DIRECTION ( 'NONE',  ( 1.000000000000000000, 0.000000000000000000, 0.000000000000000000 ) ) ;
#31733 = CARTESIAN_POINT ( 'NONE',  ( -9.999999999999998224, 1.224646799147353059E-15, -55.24999999999996447 ) ) ;
#31734 = CARTESIAN_POINT ( 'NONE',  ( 10.81189881249999729, 0.000000000000000000, -117.0312500020483952 ) ) ;
#31735 = CARTESIAN_POINT ( 'NONE',  ( 7.644554776091147741E-16, 12.48450537969573659, -98.65625000204838102 ) ) ;
#31736 = ORIENTED_EDGE ( 'NONE', *, *, #20349, .T. ) ;
#31737 =( BOUNDED_CURVE ( )  B_SPLINE_CURVE ( 2, ( #9578, #19499, #3114, #29655, #16241, #29442, #13008 ),
 .UNSPECIFIED., .F., .F. ) 
 B_SPLINE_CURVE_WITH_KNOTS ( ( 3, 2, 2, 3 ),
 ( 0.1567164179104477695, 0.1579601990049751270, 0.1592039800995025123, 0.1604477611940298698 ),
 .UNSPECIFIED. ) 
 CURVE ( )  GEOMETRIC_REPRESENTATION_ITEM ( )  RATIONAL_B_SPLINE_CURVE ( ( 1.000000000000000000, 0.8660254037844387076, 1.000000000000000000, 0.8660254037844387076, 1.000000000000000000, 0.8660254037844357100, 1.000000000000003109 ) ) 
 REPRESENTATION_ITEM ( '' )  );
#31738 = CARTESIAN_POINT ( 'NONE',  ( 7.070501591499377789E-16, 11.54700538379251284, -89.00000000409677625 ) ) ;
#31739 = CYLINDRICAL_SURFACE ( 'NONE', #34652, 9.999999999999998224 ) ;
#31740 = CARTESIAN_POINT ( 'NONE',  ( 5.405949406249992428, -9.363379034771808662, -154.7812500020484094 ) ) ;
#31741 = CARTESIAN_POINT ( 'NONE',  ( 5.405949406249999534, 9.363379034771803333, -49.09375000204838102 ) ) ;
#31742 = ORIENTED_EDGE ( 'NONE', *, *, #31227, .T. ) ;
#31743 = CARTESIAN_POINT ( 'NONE',  ( 9.999999999999996447, -5.773502691896262640, -20.12499999999996803 ) ) ;
#31744 = EDGE_CURVE ( 'NONE', #25635, #1542, #37249, .T. ) ;
#31745 = CARTESIAN_POINT ( 'NONE',  ( 10.81189881249999551, -6.242252689847874514, -28.65625000204838813 ) ) ;
#31746 = CARTESIAN_POINT ( 'NONE',  ( 9.999999999999998224, 0.000000000000000000, -155.0000000000000000 ) ) ;
#31747 = CARTESIAN_POINT ( 'NONE',  ( 9.999999999999998224, 0.000000000000000000, -21.87500000409675494 ) ) ;
#31748 = EDGE_CURVE ( 'NONE', #18719, #38940, #28815, .T. ) ;
#31749 = CARTESIAN_POINT ( 'NONE',  ( -9.999999999998969713, -5.773502691896847949, -34.12499999999995026 ) ) ;
#31750 = CARTESIAN_POINT ( 'NONE',  ( 10.81189881249999551, -6.242252689847874514, -124.6562500020483952 ) ) ;
#31751 = CARTESIAN_POINT ( 'NONE',  ( -4.999999999999996447, 8.660254037844387298, -117.3750000040967905 ) ) ;
#31752 = CARTESIAN_POINT ( 'NONE',  ( 23.09401076758504345, 1.040834085586084257E-14, 45.00000000000009237 ) ) ;
#31753 = ORIENTED_EDGE ( 'NONE', *, *, #4039, .F. ) ;
#31754 = CARTESIAN_POINT ( 'NONE',  ( -5.405949406250003975, -9.363379034771801557, -53.03125000204836681 ) ) ;
#31755 = PERSON_AND_ORGANIZATION ( #11915, #17965 ) ;
#31756 = CARTESIAN_POINT ( 'NONE',  ( -10.81189881249999907, -6.242252689847864744, -108.4687500020483810 ) ) ;
#31758 = ORIENTED_EDGE ( 'NONE', *, *, #23406, .F. ) ;
#31757 = ORIENTED_EDGE ( 'NONE', *, *, #21759, .F. ) ;
#31759 = EDGE_CURVE ( 'NONE', #19819, #18647, #35113, .T. ) ;
#31760 = DIRECTION ( 'NONE',  ( -0.000000000000000000, -0.000000000000000000, 1.000000000000000000 ) ) ;
#31761 = LINE ( 'NONE', #15323, #22873 ) ;
#31762 = CARTESIAN_POINT ( 'NONE',  ( -5.405949406249996869, 9.363379034771805109, -158.3437500020483810 ) ) ;
#31763 = CARTESIAN_POINT ( 'NONE',  ( 7.644554776091147741E-16, 12.48450537969573659, -187.1562500020484094 ) ) ;
#31764 = CARTESIAN_POINT ( 'NONE',  ( 5.405949406249992428, -9.363379034771808662, -6.093750002048370362 ) ) ;
#31765 = EDGE_CURVE ( 'NONE', #40867, #13705, #30693, .T. ) ;
#31766 = CARTESIAN_POINT ( 'NONE',  ( -10.81189881249999729, 6.242252689847871849, -138.7187500020483810 ) ) ;
#31767 = CARTESIAN_POINT ( 'NONE',  ( -5.405949406250003975, -9.363379034771801557, -112.8437500020483810 ) ) ;
#31768 = CARTESIAN_POINT ( 'NONE',  ( 9.999999999999998224, 0.000000000000000000, -147.8750000040967905 ) ) ;
#31769 = CARTESIAN_POINT ( 'NONE',  ( 10.81189881249999551, -6.242252689847874514, -115.6562500020483810 ) ) ;
#31770 = CARTESIAN_POINT ( 'NONE',  ( 10.81189881249999907, 6.242252689847868297, -1.218750002048353709 ) ) ;
#31771 = CARTESIAN_POINT ( 'NONE',  ( 10.81189881249999729, 6.242252689847867408, -121.2187500020483952 ) ) ;
#31772 = CARTESIAN_POINT ( 'NONE',  ( -2.293366432827344421E-15, -12.48450537969573659, -193.9062500020484094 ) ) ;
#31773 = CARTESIAN_POINT ( 'NONE',  ( 9.999999999998969713, 5.773502691896851502, -12.37499999999993783 ) ) ;
#31774 = CARTESIAN_POINT ( 'NONE',  ( 5.000000000000000000, 8.660254037844385522, -150.2500000000000000 ) ) ;
#31775 = CARTESIAN_POINT ( 'NONE',  ( -5.000000000000003553, -8.660254037844383745, -11.49999999999995381 ) ) ;
#31776 = CARTESIAN_POINT ( 'NONE',  ( -10.81189881249999729, 1.324075727343319199E-15, -71.09375000204836681 ) ) ;
#31777 = CARTESIAN_POINT ( 'NONE',  ( 5.405949406249999534, 9.363379034771803333, -53.59375000204835970 ) ) ;
#31778 = CARTESIAN_POINT ( 'NONE',  ( -5.000000000000003553, -8.660254037844383745, -184.3750000040967905 ) ) ;
#31779 = CARTESIAN_POINT ( 'NONE',  ( -2.293366432827344421E-15, -12.48450537969573659, -28.90625000204835615 ) ) ;
#31780 = CARTESIAN_POINT ( 'NONE',  ( -2.293366432827344421E-15, -12.48450537969573659, -37.71875000204835970 ) ) ;
#31781 = CARTESIAN_POINT ( 'NONE',  ( 5.000000000000000000, 8.660254037844385522, -32.12500000409676204 ) ) ;
#31782 = CARTESIAN_POINT ( 'NONE',  ( 10.81189881249999729, 0.000000000000000000, -143.8437500020483810 ) ) ;
#31783 = CARTESIAN_POINT ( 'NONE',  ( 5.000000000000000000, 8.660254037844385522, -111.2499999999999858 ) ) ;
#31784 = CARTESIAN_POINT ( 'NONE',  ( -9.999999999999998224, 1.224646799147353059E-15, -170.7500000000000000 ) ) ;
#31785 = CARTESIAN_POINT ( 'NONE',  ( -10.00000000000000000, -5.773502691896251982, -76.12499999999997158 ) ) ;
#31786 = CARTESIAN_POINT ( 'NONE',  ( -2.293366432827344421E-15, -12.48450537969573659, -139.9062500020484094 ) ) ;
#31787 = CARTESIAN_POINT ( 'NONE',  ( -2.293366432827344421E-15, -12.48450537969573659, -9.406250002048377468 ) ) ;
#31788 = EDGE_LOOP ( 'NONE', ( #31736, #19071, #4870, #11486 ) ) ;
#31789 = CARTESIAN_POINT ( 'NONE',  ( 9.999999999999742428, 5.773502691896404748, -121.8750000000000142 ) ) ;
#31790 = CARTESIAN_POINT ( 'NONE',  ( -10.00000000000000000, -5.773502691896251982, -120.0000000040967905 ) ) ;
#31791 = CARTESIAN_POINT ( 'NONE',  ( -5.000000000000005329, -20.00000000000000000, -235.0000000000000000 ) ) ;
#31792 = CARTESIAN_POINT ( 'NONE',  ( 5.405949406249999534, 9.363379034771803333, -71.59375000204836681 ) ) ;
#31793 = CARTESIAN_POINT ( 'NONE',  ( -2.121150477449813534E-15, -11.54700538379251284, -47.37499999999997158 ) ) ;
#31794 = LOCAL_TIME ( 11, 57, 6.000000000000000000, #41211 ) ;
#31795 = CARTESIAN_POINT ( 'NONE',  ( 4.999999999999992006, -8.660254037844389075, -23.62500000409675849 ) ) ;
#31796 = ADVANCED_FACE ( 'NONE', ( #1441 ), #11127, .T. ) ;
#31797 = AXIS2_PLACEMENT_3D ( 'NONE', #8952, #19080, #22115 ) ;
#31798 = CARTESIAN_POINT ( 'NONE',  ( 9.999999999999998224, 0.000000000000000000, -131.0000000000000000 ) ) ;
#31799 = CARTESIAN_POINT ( 'NONE',  ( -10.81189881249999729, 6.242252689847871849, -44.40625000204836681 ) ) ;
#31800 = EDGE_CURVE ( 'NONE', #42167, #35094, #947, .T. ) ;
#31801 = CARTESIAN_POINT ( 'NONE',  ( 0.000000000000000000, 0.000000000000000000, -200.0000000000000000 ) ) ;
#31802 = CARTESIAN_POINT ( 'NONE',  ( -2.293366432827344421E-15, -12.48450537969573659, -145.9062500020484094 ) ) ;
#31803 = EDGE_CURVE ( 'NONE', #15042, #4157, #39507, .T. ) ;
#31804 = CARTESIAN_POINT ( 'NONE',  ( -5.405949406250003975, -9.363379034771801557, -152.0312500020484094 ) ) ;
#31805 = CARTESIAN_POINT ( 'NONE',  ( -10.00000000000051337, 5.773502691895962435, -78.25000000409677625 ) ) ;
#31806 =( BOUNDED_CURVE ( )  B_SPLINE_CURVE ( 2, ( #27397, #30005, #24392, #10976, #27180, #24172, #34092 ),
 .UNSPECIFIED., .F., .F. ) 
 B_SPLINE_CURVE_WITH_KNOTS ( ( 3, 2, 2, 3 ),
 ( 0.4552238805970150737, 0.4564676616915424590, 0.4577114427860698442, 0.4589552238805971740 ),
 .UNSPECIFIED. ) 
 CURVE ( )  GEOMETRIC_REPRESENTATION_ITEM ( )  RATIONAL_B_SPLINE_CURVE ( ( 0.9999999999999820144, 0.8660254037844566932, 1.000000000000000000, 0.8660254037844387076, 1.000000000000000000, 0.8660254037844207220, 1.000000000000017986 ) ) 
 REPRESENTATION_ITEM ( '' )  );
#31807 = CARTESIAN_POINT ( 'NONE',  ( -7.071067811865472841, -7.071067811865472841, -200.0000000000000000 ) ) ;
#31808 = ORIENTED_EDGE ( 'NONE', *, *, #10072, .F. ) ;
#31809 = ORIENTED_EDGE ( 'NONE', *, *, #31252, .T. ) ;
#31810 = ORIENTED_EDGE ( 'NONE', *, *, #19044, .T. ) ;
#31811 = EDGE_CURVE ( 'NONE', #2913, #6874, #2345, .T. ) ;
#31812 = AXIS2_PLACEMENT_3D ( 'NONE', #39982, #36962, #36330 ) ;
#31813 = CARTESIAN_POINT ( 'NONE',  ( 9.999999999999998224, 0.000000000000000000, -6.875000004096742501 ) ) ;
#31814 = CARTESIAN_POINT ( 'NONE',  ( 10.81189881249999551, -6.242252689847874514, -178.4687500020484094 ) ) ;
#31815 = LOCAL_TIME ( 11, 57, 6.000000000000000000, #8395 ) ;
#31816 = CARTESIAN_POINT ( 'NONE',  ( 7.644554776091147741E-16, 12.48450537969573659, -27.96875000204838457 ) ) ;
#31817 = CARTESIAN_POINT ( 'NONE',  ( -5.405949406250003975, -9.363379034771801557, -166.8437500020484094 ) ) ;
#31818 = CARTESIAN_POINT ( 'NONE',  ( 7.644554776091147741E-16, 12.48450537969573659, -149.4687500020484094 ) ) ;
#31819 = CARTESIAN_POINT ( 'NONE',  ( 0.000000000000000000, 0.000000000000000000, -200.0000000000000000 ) ) ;
#31820 = CARTESIAN_POINT ( 'NONE',  ( -10.81189881249999729, 1.324075727343319199E-15, -131.0937500020483810 ) ) ;
#31821 = CARTESIAN_POINT ( 'NONE',  ( -5.405949406250003975, -9.363379034771801557, -138.5312500020484094 ) ) ;
#31822 = CARTESIAN_POINT ( 'NONE',  ( 5.405949406249992428, -9.363379034771808662, -142.5937500020483810 ) ) ;
#31823 = CARTESIAN_POINT ( 'NONE',  ( -9.999999999999998224, 1.224646799147353059E-15, -200.0000000000000000 ) ) ;
#31824 = CARTESIAN_POINT ( 'NONE',  ( 5.000000000000000000, 8.660254037844385522, -171.2500000000000000 ) ) ;
#31825 = CARTESIAN_POINT ( 'NONE',  ( -5.405949406250003975, -9.363379034771801557, -81.34375000204838102 ) ) ;
#31826 = DIRECTION ( 'NONE',  ( 1.000000000000000000, 0.000000000000000000, 0.000000000000000000 ) ) ;
#31827 = CARTESIAN_POINT ( 'NONE',  ( -5.405949406250003975, -9.363379034771801557, -51.53125000204835970 ) ) ;
#31828 = CARTESIAN_POINT ( 'NONE',  ( -9.999999999999998224, 1.224646799147353059E-15, -37.62500000409676915 ) ) ;
#31829 = CARTESIAN_POINT ( 'NONE',  ( 10.81189881249999551, -6.242252689847874514, -167.9687500020483810 ) ) ;
#31830 = CARTESIAN_POINT ( 'NONE',  ( -5.405949406249996869, 9.363379034771805109, -115.0312500020483952 ) ) ;
#31831 = CARTESIAN_POINT ( 'NONE',  ( -10.81189881249999729, 1.324075727343319199E-15, -147.7812500020483810 ) ) ;
#31832 = FACE_OUTER_BOUND ( 'NONE', #22077, .T. ) ;
#31833 = CARTESIAN_POINT ( 'NONE',  ( -10.81189881249999729, 1.324075727343319199E-15, -36.78125000204837391 ) ) ;
#31834 = CARTESIAN_POINT ( 'NONE',  ( -5.000000000000003553, -8.660254037844383745, -124.3750000040967763 ) ) ;
#31835 = CARTESIAN_POINT ( 'NONE',  ( 4.999999999999992006, -8.660254037844389075, -98.24999999999998579 ) ) ;
#31836 = VERTEX_POINT ( 'NONE', #28201 ) ;
#31837 = CARTESIAN_POINT ( 'NONE',  ( 10.81189881249999551, -6.242252689847874514, -127.6562500020483810 ) ) ;
#31838 = CARTESIAN_POINT ( 'NONE',  ( 7.070501591499377789E-16, 11.54700538379251284, -141.5000000040967905 ) ) ;
#31839 = CARTESIAN_POINT ( 'NONE',  ( -4.999999999999996447, 8.660254037844387298, -184.5000000000000000 ) ) ;
#31840 = CARTESIAN_POINT ( 'NONE',  ( 10.81189881249999907, 6.242252689847868297, -181.4062500020484379 ) ) ;
#31841 = ORIENTED_EDGE ( 'NONE', *, *, #25690, .T. ) ;
#31842 = CARTESIAN_POINT ( 'NONE',  ( -9.999999999999998224, 5.773502691896259087, -52.75000000409676915 ) ) ;
#31843 = CARTESIAN_POINT ( 'NONE',  ( 9.999999999999998224, 0.000000000000000000, -87.87500000409677625 ) ) ;
#31844 = CARTESIAN_POINT ( 'NONE',  ( -10.81189881249999729, 1.324075727343319199E-15, -68.28125000204838102 ) ) ;
#31845 = AXIS2_PLACEMENT_3D ( 'NONE', #1284, #20478, #37314 ) ;
#31846 =( BOUNDED_CURVE ( )  B_SPLINE_CURVE ( 2, ( #32969, #23468, #388, #33611, #19996, #599, #19782 ),
 .UNSPECIFIED., .F., .F. ) 
 B_SPLINE_CURVE_WITH_KNOTS ( ( 3, 2, 2, 3 ),
 ( 0.3283582089552238847, 0.3296019900497513255, 0.3308457711442787108, 0.3320895522388061516 ),
 .UNSPECIFIED. ) 
 CURVE ( )  GEOMETRIC_REPRESENTATION_ITEM ( )  RATIONAL_B_SPLINE_CURVE ( ( 1.000000000000000000, 0.8660254037844387076, 1.000000000000000000, 0.8660254037844387076, 1.000000000000000000, 0.8660254037844207220, 1.000000000000017986 ) ) 
 REPRESENTATION_ITEM ( '' )  );
#31847 = CYLINDRICAL_SURFACE ( 'NONE', #36557, 9.999999999999998224 ) ;
#31848 = CARTESIAN_POINT ( 'NONE',  ( 10.81189881249999907, 6.242252689847868297, -167.9062500020484094 ) ) ;
#31849 = CARTESIAN_POINT ( 'NONE',  ( 10.81189881249999729, 0.000000000000000000, -114.0312500020483952 ) ) ;
#31850 = CARTESIAN_POINT ( 'NONE',  ( -5.000000000000003553, -8.660254037844383745, -163.0000000000000000 ) ) ;
#31851 = CARTESIAN_POINT ( 'NONE',  ( -9.999999999999998224, 1.224646799147353059E-15, -56.74999999999996447 ) ) ;
#31852 = ORIENTED_EDGE ( 'NONE', *, *, #11564, .F. ) ;
#31853 = CARTESIAN_POINT ( 'NONE',  ( 9.999999999999998224, 0.000000000000000000, -17.37500000409675138 ) ) ;
#31854 = CARTESIAN_POINT ( 'NONE',  ( 5.000000000000000000, 8.660254037844385522, -173.1250000040968189 ) ) ;
#31855 = CARTESIAN_POINT ( 'NONE',  ( 0.000000000000000000, 0.000000000000000000, -200.0000000000000000 ) ) ;
#31856 = VECTOR ( 'NONE', #11736, 1000.000000000000000 ) ;
#31857 = EDGE_CURVE ( 'NONE', #8912, #6661, #41335, .T. ) ;
#31859 = ORIENTED_EDGE ( 'NONE', *, *, #37405, .F. ) ;
#31858 = CARTESIAN_POINT ( 'NONE',  ( -10.81189881249999729, 1.324075727343319199E-15, -77.28125000204838102 ) ) ;
#31861 = VERTEX_POINT ( 'NONE', #4244 ) ;
#31860 = CARTESIAN_POINT ( 'NONE',  ( 9.999999999999998224, 0.000000000000000000, -39.49999999999997868 ) ) ;
#31862 = ORIENTED_EDGE ( 'NONE', *, *, #6705, .F. ) ;
#31863 = CARTESIAN_POINT ( 'NONE',  ( -10.81189881249999729, 1.324075727343319199E-15, -32.09375000204836681 ) ) ;
#31864 = CARTESIAN_POINT ( 'NONE',  ( 9.999999999999479527, 5.773502691896553074, -77.25000000409676204 ) ) ;
#31865 = CARTESIAN_POINT ( 'NONE',  ( 10.81189881249999551, -6.242252689847874514, -3.156250002048346381 ) ) ;
#31867 = ORIENTED_EDGE ( 'NONE', *, *, #35558, .F. ) ;
#31866 = CARTESIAN_POINT ( 'NONE',  ( -5.405949406250003975, -9.363379034771801557, -58.84375000204835970 ) ) ;
#31868 = DIRECTION ( 'NONE',  ( -0.000000000000000000, -0.000000000000000000, -1.000000000000000000 ) ) ;
#31869 = CARTESIAN_POINT ( 'NONE',  ( -4.999999999999996447, 8.660254037844387298, -40.49999999999997868 ) ) ;
#31870 = CARTESIAN_POINT ( 'NONE',  ( 5.405949406249999534, 9.363379034771803333, -191.5937500020484094 ) ) ;
#31871 = CARTESIAN_POINT ( 'NONE',  ( 10.81189881249999729, 0.000000000000000000, -176.8437500020483810 ) ) ;
#31872 = CARTESIAN_POINT ( 'NONE',  ( -5.405949406249996869, 9.363379034771805109, -161.3437500020484094 ) ) ;
#31873 = CIRCLE ( 'NONE', #1544, 45.00000000000000711 ) ;
#31874 = CARTESIAN_POINT ( 'NONE',  ( -2.293366432827344421E-15, -12.48450537969573659, -168.2187500020483810 ) ) ;
#31875 = CARTESIAN_POINT ( 'NONE',  ( 5.000000000000000000, 8.660254037844385522, -18.62500000409675494 ) ) ;
#31876 = CARTESIAN_POINT ( 'NONE',  ( -5.000000000000003553, -8.660254037844383745, -24.99999999999996803 ) ) ;
#31877 = CARTESIAN_POINT ( 'NONE',  ( 5.000000000000000000, 8.660254037844385522, -196.7500000000000000 ) ) ;
#31878 = CARTESIAN_POINT ( 'NONE',  ( 10.81189881249999729, 0.000000000000000000, -104.8437500020483810 ) ) ;
#31879 = CARTESIAN_POINT ( 'NONE',  ( -4.999999999999996447, 8.660254037844387298, -17.99999999999996092 ) ) ;
#31880 = CARTESIAN_POINT ( 'NONE',  ( -2.293366432827344421E-15, -12.48450537969573659, -70.90625000204839523 ) ) ;
#31881 = CARTESIAN_POINT ( 'NONE',  ( -10.81189881249999729, -6.242252689847864744, -93.46875000204838102 ) ) ;
#31882 = CARTESIAN_POINT ( 'NONE',  ( -10.81189881249999729, 1.324075727343319199E-15, -66.78125000204838102 ) ) ;
#31883 = CARTESIAN_POINT ( 'NONE',  ( -5.000000000000003553, -8.660254037844383745, -142.3750000040967905 ) ) ;
#31884 = CARTESIAN_POINT ( 'NONE',  ( -9.999999999999998224, 5.773502691896259087, -122.8750000000000142 ) ) ;
#31885 = VERTEX_POINT ( 'NONE', #35102 ) ;
#31886 = CARTESIAN_POINT ( 'NONE',  ( -10.81189881249999729, 6.242252689847871849, -152.4062500020483810 ) ) ;
#31887 = CARTESIAN_POINT ( 'NONE',  ( 10.81189881249999551, -6.242252689847874514, -166.6562500020484094 ) ) ;
#31888 = CONICAL_SURFACE ( 'NONE', #2943, 45.00000000000000711, 0.7853981633974459475 ) ;
#31889 = CARTESIAN_POINT ( 'NONE',  ( -2.121150477449813534E-15, -11.54700538379251284, -13.25000000409675849 ) ) ;
#31890 = CARTESIAN_POINT ( 'NONE',  ( -9.999999999999998224, 1.224646799147353059E-15, -169.2500000000000000 ) ) ;
#31891 = CARTESIAN_POINT ( 'NONE',  ( 10.81189881249999551, -6.242252689847874514, -94.46875000204838102 ) ) ;
#31892 = ORIENTED_EDGE ( 'NONE', *, *, #24647, .T. ) ;
#31893 = CARTESIAN_POINT ( 'NONE',  ( -4.999999999999996447, 8.660254037844387298, -68.99999999999997158 ) ) ;
#31894 = CARTESIAN_POINT ( 'NONE',  ( 10.81189881249999907, 6.242252689847868297, -197.7187500020484094 ) ) ;
#31895 = CARTESIAN_POINT ( 'NONE',  ( 7.070501591499377789E-16, 11.54700538379251284, -75.50000000409677625 ) ) ;
#31896 = CARTESIAN_POINT ( 'NONE',  ( -6.910789922881853897, -7.414454835661850041, -179.9999999999999716 ) ) ;
#31897 = CARTESIAN_POINT ( 'NONE',  ( 9.999999999999998224, 0.000000000000000000, -200.0000000000000000 ) ) ;
#31898 = CARTESIAN_POINT ( 'NONE',  ( -10.81189881249999729, 1.324075727343319199E-15, -93.78125000204838102 ) ) ;
#31899 = CARTESIAN_POINT ( 'NONE',  ( -2.293366432827344421E-15, -12.48450537969573659, -66.40625000204839523 ) ) ;
#31900 = CARTESIAN_POINT ( 'NONE',  ( -9.999999999999998224, 1.224646799147353059E-15, -69.12500000409677625 ) ) ;
#31901 = CARTESIAN_POINT ( 'NONE',  ( 10.81189881249999907, 6.242252689847868297, -26.71875000204837391 ) ) ;
#31902 = VERTEX_POINT ( 'NONE', #32289 ) ;
#31903 = CARTESIAN_POINT ( 'NONE',  ( 10.81189881249999551, -6.242252689847874514, -196.6562500020484379 ) ) ;
#31904 = CARTESIAN_POINT ( 'NONE',  ( 10.81189881249999907, 6.242252689847868297, -16.40625000204837036 ) ) ;
#31905 = CARTESIAN_POINT ( 'NONE',  ( -5.405949406249996869, 9.363379034771805109, -5.343750002048369474 ) ) ;
#31906 = FACE_OUTER_BOUND ( 'NONE', #5609, .T. ) ;
#31907 = CARTESIAN_POINT ( 'NONE',  ( -9.999999999999998224, 1.224646799147353059E-15, -191.7500000000000000 ) ) ;
#31908 = CARTESIAN_POINT ( 'NONE',  ( 9.999999999999866773, -5.773502691896336358, -173.1250000000000000 ) ) ;
#31909 = EDGE_CURVE ( 'NONE', #17345, #16464, #15637, .T. ) ;
#31910 = CARTESIAN_POINT ( 'NONE',  ( 5.000000000000000000, 8.660254037844385522, -177.2500000000000284 ) ) ;
#31911 = CARTESIAN_POINT ( 'NONE',  ( 10.00000000000051159, -5.773502691895965988, -36.62499999999995026 ) ) ;
#31913 = VERTEX_POINT ( 'NONE', #34891 ) ;
#31912 = CARTESIAN_POINT ( 'NONE',  ( -10.81189881249999729, 6.242252689847871849, -104.4062500020483810 ) ) ;
#31914 = ORIENTED_EDGE ( 'NONE', *, *, #25479, .T. ) ;
#31915 = ORIENTED_EDGE ( 'NONE', *, *, #20645, .T. ) ;
#31916 = CARTESIAN_POINT ( 'NONE',  ( -10.81189881249999729, 6.242252689847871849, -32.40625000204835970 ) ) ;
#31917 = DATE_AND_TIME ( #9226, #20779 ) ;
#31918 = AXIS2_PLACEMENT_3D ( 'NONE', #21844, #38672, #25731 ) ;
#31919 = CARTESIAN_POINT ( 'NONE',  ( 10.81189881249999729, 0.000000000000000000, -76.34375000204838102 ) ) ;
#31920 = DIRECTION ( 'NONE',  ( 1.000000000000000000, 0.000000000000000000, 0.000000000000000000 ) ) ;
#31921 = EDGE_CURVE ( 'NONE', #29474, #20834, #22559, .T. ) ;
#31922 = CARTESIAN_POINT ( 'NONE',  ( 9.980591063997303891, -1.864246421445880042, -99.99999999999995737 ) ) ;
#31923 = CARTESIAN_POINT ( 'NONE',  ( -99.99999999999994316, -40.00000000000000711, -160.0000000000000000 ) ) ;
#31924 = CARTESIAN_POINT ( 'NONE',  ( -5.405949406250003975, -9.363379034771801557, -165.5312500020484094 ) ) ;
#31925 = CARTESIAN_POINT ( 'NONE',  ( -9.999999999999998224, 5.773502691896259087, -10.75000000409676204 ) ) ;
#31926 = CARTESIAN_POINT ( 'NONE',  ( 10.00000000000003020, -5.773502691896243988, -198.6250000000000284 ) ) ;
#31927 = CARTESIAN_POINT ( 'NONE',  ( -5.405949406250003975, -9.363379034771801557, -130.8437500020484094 ) ) ;
#31928 = CARTESIAN_POINT ( 'NONE',  ( 5.405949406249992428, -9.363379034771808662, -114.0937500020483810 ) ) ;
#31929 = CARTESIAN_POINT ( 'NONE',  ( 10.81189881249999907, 6.242252689847868297, -82.21875000204836681 ) ) ;
#31930 = CARTESIAN_POINT ( 'NONE',  ( -5.405949406250003975, -9.363379034771801557, -190.8437500020484094 ) ) ;
#31931 = CARTESIAN_POINT ( 'NONE',  ( -10.81189881249999907, -6.242252689847864744, -93.65625000204840944 ) ) ;
#31932 = CARTESIAN_POINT ( 'NONE',  ( -2.121150477449813534E-15, -11.54700538379251284, -169.2500000040967620 ) ) ;
#31933 = CARTESIAN_POINT ( 'NONE',  ( -10.81189881249999729, -6.242252689847864744, -170.1562500020484094 ) ) ;
#31934 = CARTESIAN_POINT ( 'NONE',  ( -4.999999999999996447, 8.660254037844387298, -68.99999999999997158 ) ) ;
#31935 = CARTESIAN_POINT ( 'NONE',  ( 10.81189881249999729, 6.242252689847867408, -173.9062500020483810 ) ) ;
#31936 = CARTESIAN_POINT ( 'NONE',  ( -2.293366432827344421E-15, -12.48450537969573659, -186.4062500020484094 ) ) ;
#31937 = CARTESIAN_POINT ( 'NONE',  ( 5.405949406249999534, 9.363379034771803333, -46.09375000204838102 ) ) ;
#31938 = CARTESIAN_POINT ( 'NONE',  ( -9.999999999999998224, 1.224646799147353059E-15, -166.6250000040967905 ) ) ;
#31939 = CARTESIAN_POINT ( 'NONE',  ( 5.405949406249999534, 9.363379034771803333, 0.2187499979516283055 ) ) ;
#31940 = CARTESIAN_POINT ( 'NONE',  ( -10.81189881249999729, 6.242252689847871849, -11.21875000204835970 ) ) ;
#31941 = CARTESIAN_POINT ( 'NONE',  ( 7.644554776091147741E-16, 12.48450537969573659, -123.9687500020483952 ) ) ;
#31942 = CARTESIAN_POINT ( 'NONE',  ( 9.999999999999998224, 0.000000000000000000, -85.99999999999998579 ) ) ;
#31943 = CARTESIAN_POINT ( 'NONE',  ( -10.81189881249999907, -6.242252689847864744, -18.65625000204837747 ) ) ;
#31944 = CARTESIAN_POINT ( 'NONE',  ( 4.999999999999992006, -8.660254037844389075, -98.62500000409677625 ) ) ;
#31945 = CARTESIAN_POINT ( 'NONE',  ( 10.00000000000051159, -5.773502691895965988, -149.5000000040967905 ) ) ;
#31946 = CARTESIAN_POINT ( 'NONE',  ( 5.405949406249999534, 9.363379034771803333, -115.2812500020483952 ) ) ;
#31947 = CARTESIAN_POINT ( 'NONE',  ( 7.644554776091147741E-16, 12.48450537969573659, -101.6562500020483952 ) ) ;
#31948 = ORIENTED_EDGE ( 'NONE', *, *, #13997, .T. ) ;
#31949 = CARTESIAN_POINT ( 'NONE',  ( -2.121150477449813534E-15, -11.54700538379251284, -88.25000000409677625 ) ) ;
#31950 = DIRECTION ( 'NONE',  ( -0.000000000000000000, -0.000000000000000000, 1.000000000000000000 ) ) ;
#31951 = CARTESIAN_POINT ( 'NONE',  ( -5.405949406250003975, -9.363379034771801557, -156.5312500020484094 ) ) ;
#31952 = CARTESIAN_POINT ( 'NONE',  ( 10.81189881249999907, 6.242252689847868297, -50.71875000204837391 ) ) ;
#31953 = ORIENTED_EDGE ( 'NONE', *, *, #27778, .T. ) ;
#31954 = CARTESIAN_POINT ( 'NONE',  ( 10.00000000000000000, 5.773502691896255534, -16.87499999999996803 ) ) ;
#31955 = CARTESIAN_POINT ( 'NONE',  ( -10.81189881249999729, 1.324075727343319199E-15, -26.28125000204836681 ) ) ;
#31956 = CARTESIAN_POINT ( 'NONE',  ( 7.070501591499377789E-16, 11.54700538379251284, -154.6250000000000284 ) ) ;
#31957 = CARTESIAN_POINT ( 'NONE',  ( -10.00000000000000000, -5.773502691896251982, -16.50000000409676559 ) ) ;
#31958 = DIRECTION ( 'NONE',  ( 0.000000000000000000, 0.000000000000000000, -1.000000000000000000 ) ) ;
#31960 = VERTEX_POINT ( 'NONE', #38533 ) ;
#31959 = CARTESIAN_POINT ( 'NONE',  ( -10.81189881249999729, 6.242252689847871849, -129.9062500020483810 ) ) ;
#31961 = CARTESIAN_POINT ( 'NONE',  ( -10.00000000000102496, 5.773502691895664007, -64.75000000409674783 ) ) ;
#31962 = CARTESIAN_POINT ( 'NONE',  ( 9.999999999999998224, 0.000000000000000000, -188.0000000000000000 ) ) ;
#31963 = VERTEX_POINT ( 'NONE', #2713 ) ;
#31964 = SHAPE_REPRESENTATION ( 'thrust bolt', ( #39998 ), #15874 ) ;
#31965 = CARTESIAN_POINT ( 'NONE',  ( -2.293366432827344421E-15, -12.48450537969573659, -55.90625000204837391 ) ) ;
#31966 = APPLICATION_PROTOCOL_DEFINITION ( 'international standard', 'config_control_design', 1994, #20100 ) ;
#31967 = CARTESIAN_POINT ( 'NONE',  ( 10.81189881249999551, -6.242252689847874514, -101.9687500020483810 ) ) ;
#31969 = ORIENTED_EDGE ( 'NONE', *, *, #42334, .T. ) ;
#31968 = ORIENTED_EDGE ( 'NONE', *, *, #39890, .T. ) ;
#31970 = CARTESIAN_POINT ( 'NONE',  ( 4.999999999999992006, -8.660254037844389075, -175.1250000040968189 ) ) ;
#31971 = CARTESIAN_POINT ( 'NONE',  ( 10.81189881249999907, 6.242252689847868297, -158.7187500020483810 ) ) ;
#31972 = CARTESIAN_POINT ( 'NONE',  ( -10.81189881249999729, 6.242252689847871849, -188.4062500020484094 ) ) ;
#31973 = CARTESIAN_POINT ( 'NONE',  ( -5.405949406249996869, 9.363379034771805109, -8.343750002048345493 ) ) ;
#31974 = CARTESIAN_POINT ( 'NONE',  ( 0.000000000000000000, 0.000000000000000000, -200.0000000000000000 ) ) ;
#31975 = EDGE_CURVE ( 'NONE', #39731, #1094, #36233, .T. ) ;
#31976 = CARTESIAN_POINT ( 'NONE',  ( 7.644554776091147741E-16, 12.48450537969573659, -138.9687500020483810 ) ) ;
#31977 = EDGE_CURVE ( 'NONE', #2291, #30470, #18898, .T. ) ;
#31978 = CARTESIAN_POINT ( 'NONE',  ( 10.81189881249999907, 6.242252689847868297, -112.2187500020483810 ) ) ;
#31979 = CARTESIAN_POINT ( 'NONE',  ( 100.0000000000000284, -20.00000000000001066, -160.0000000000000000 ) ) ;
#31980 = CARTESIAN_POINT ( 'NONE',  ( 10.81189881249999907, 6.242252689847868297, -113.9062500020483952 ) ) ;
#31981 = CARTESIAN_POINT ( 'NONE',  ( 10.00000000000000000, 5.773502691896255534, -192.7500000040968189 ) ) ;
#31982 = CARTESIAN_POINT ( 'NONE',  ( -10.81189881249999729, 6.242252689847871849, -120.7187500020483952 ) ) ;
#31983 = CARTESIAN_POINT ( 'NONE',  ( 5.405949406249999534, 9.363379034771803333, -193.2812500020484094 ) ) ;
#31984 = DIRECTION ( 'NONE',  ( 0.000000000000000000, 0.000000000000000000, -1.000000000000000000 ) ) ;
#31985 = CARTESIAN_POINT ( 'NONE',  ( 4.999999999999992006, -8.660254037844389075, -140.2500000000000000 ) ) ;
#31986 = CARTESIAN_POINT ( 'NONE',  ( -9.999999999999998224, 5.773502691896259087, -14.87499999999997335 ) ) ;
#31987 = CARTESIAN_POINT ( 'NONE',  ( -10.81189881249999729, 1.324075727343319199E-15, -66.59375000204836681 ) ) ;
#31988 = CARTESIAN_POINT ( 'NONE',  ( -10.81189881249999907, -6.242252689847864744, -58.96875000204836681 ) ) ;
#31989 = CARTESIAN_POINT ( 'NONE',  ( 9.999999999999998224, 0.000000000000000000, -191.3750000040967905 ) ) ;
#31990 = CARTESIAN_POINT ( 'NONE',  ( 10.81189881249999907, 6.242252689847868297, -23.90625000204838102 ) ) ;
#31991 = CARTESIAN_POINT ( 'NONE',  ( 10.81189881249999907, 6.242252689847868297, -35.71875000204835970 ) ) ;
#31992 = CARTESIAN_POINT ( 'NONE',  ( -10.00000000000051337, 5.773502691895962435, -31.75000000409674072 ) ) ;
#31993 = CARTESIAN_POINT ( 'NONE',  ( 5.405949406249992428, -9.363379034771808662, -148.5937500020483810 ) ) ;
#31994 = CARTESIAN_POINT ( 'NONE',  ( -9.999999999999998224, 5.773502691896259087, -115.3749999999999858 ) ) ;
#31995 = CARTESIAN_POINT ( 'NONE',  ( -10.00000000000051337, 5.773502691895962435, -145.3750000000000000 ) ) ;
#31996 = CARTESIAN_POINT ( 'NONE',  ( -9.999999999999998224, 1.224646799147353059E-15, -79.24999999999998579 ) ) ;
#31997 = CARTESIAN_POINT ( 'NONE',  ( 10.81189881249999729, 0.000000000000000000, -136.5312500020484094 ) ) ;
#31998 = CARTESIAN_POINT ( 'NONE',  ( -10.81189881249999729, 1.324075727343319199E-15, -9.781250002048352599 ) ) ;
#31999 = ORIENTED_EDGE ( 'NONE', *, *, #41978, .F. ) ;
#32000 = CARTESIAN_POINT ( 'NONE',  ( 9.999999999999998224, 0.000000000000000000, -200.0000000000000000 ) ) ;
#32001 = CARTESIAN_POINT ( 'NONE',  ( -10.00000000000000000, -5.773502691896251982, -112.5000000040967905 ) ) ;
#32002 = CARTESIAN_POINT ( 'NONE',  ( 10.00000000000102318, -5.773502691895667560, -38.50000000409673362 ) ) ;
#32003 = CARTESIAN_POINT ( 'NONE',  ( -10.81189881249999907, -6.242252689847864744, -73.96875000204836681 ) ) ;
#32004 = CARTESIAN_POINT ( 'NONE',  ( 5.000000000000000000, 8.660254037844385522, -40.74999999999997868 ) ) ;
#32005 = CARTESIAN_POINT ( 'NONE',  ( 4.999999999999992006, -8.660254037844389075, -26.62500000409676204 ) ) ;
#32006 = CARTESIAN_POINT ( 'NONE',  ( 7.644554776091147741E-16, 12.48450537969573659, -49.15625000204837391 ) ) ;
#32007 = CARTESIAN_POINT ( 'NONE',  ( -35.00000000000000711, 0.000000000000000000, -169.9999999999999716 ) ) ;
#32008 = CARTESIAN_POINT ( 'NONE',  ( -2.293366432827344421E-15, -12.48450537969573659, -34.90625000204835970 ) ) ;
#32009 = CARTESIAN_POINT ( 'NONE',  ( 9.999999999999998224, 0.000000000000000000, -105.4999999999999858 ) ) ;
#32010 = CARTESIAN_POINT ( 'NONE',  ( -10.81189881249999907, -6.242252689847864744, -146.1562500020484094 ) ) ;
#32011 = CARTESIAN_POINT ( 'NONE',  ( 7.644554776091147741E-16, 12.48450537969573659, -151.1562500020484094 ) ) ;
#32012 = CARTESIAN_POINT ( 'NONE',  ( 9.999999999998969713, 5.773502691896851502, -60.37499999999996447 ) ) ;
#32013 = CARTESIAN_POINT ( 'NONE',  ( 0.000000000000000000, 0.000000000000000000, -200.0000000000000000 ) ) ;
#32014 = VERTEX_POINT ( 'NONE', #29045 ) ;
#32015 = ORIENTED_EDGE ( 'NONE', *, *, #37295, .T. ) ;
#32016 = ORIENTED_EDGE ( 'NONE', *, *, #32342, .F. ) ;
#32017 = CYLINDRICAL_SURFACE ( 'NONE', #8636, 9.999999999999998224 ) ;
#32018 = CARTESIAN_POINT ( 'NONE',  ( -2.293366432827344421E-15, -12.48450537969573659, -184.7187500020484094 ) ) ;
#32019 = CARTESIAN_POINT ( 'NONE',  ( 5.405949406249992428, -9.363379034771808662, -30.09375000204836326 ) ) ;
#32020 = CARTESIAN_POINT ( 'NONE',  ( 9.999999999999998224, 0.000000000000000000, -40.99999999999997868 ) ) ;
#32021 = EDGE_CURVE ( 'NONE', #22494, #4750, #5356, .T. ) ;
#32022 = CARTESIAN_POINT ( 'NONE',  ( -10.81189881249999729, -6.242252689847864744, -162.4687500020483526 ) ) ;
#32023 = CARTESIAN_POINT ( 'NONE',  ( 10.81189881249999907, 6.242252689847868297, -154.2187500020483810 ) ) ;
#32024 = LINE ( 'NONE', #38266, #12112 ) ;
#32025 = CARTESIAN_POINT ( 'NONE',  ( -5.405949406249996869, 9.363379034771805109, -131.3437500020484094 ) ) ;
#32026 = CARTESIAN_POINT ( 'NONE',  ( 5.405949406249992428, -9.363379034771808662, -136.7812500020483810 ) ) ;
#32027 = CARTESIAN_POINT ( 'NONE',  ( 5.000000000000000000, 8.660254037844385522, -144.2500000000000000 ) ) ;
#32029 = EDGE_CURVE ( 'NONE', #31210, #28982, #12195, .T. ) ;
#32028 = CARTESIAN_POINT ( 'NONE',  ( 10.81189881249999551, -6.242252689847874514, -146.9687500020484094 ) ) ;
#32030 = CARTESIAN_POINT ( 'NONE',  ( -9.999999999999998224, 1.224646799147353059E-15, -176.7500000000000284 ) ) ;
#32031 = CARTESIAN_POINT ( 'NONE',  ( -4.999999999999996447, 8.660254037844387298, -157.5000000000000000 ) ) ;
#32032 = CARTESIAN_POINT ( 'NONE',  ( -4.999999999999996447, 8.660254037844387298, -171.0000000000000000 ) ) ;
#32033 = CARTESIAN_POINT ( 'NONE',  ( -10.81189881249999907, -6.242252689847864744, -81.46875000204838102 ) ) ;
#32034 = DIRECTION ( 'NONE',  ( -0.000000000000000000, -0.000000000000000000, 1.000000000000000000 ) ) ;
#32035 = CARTESIAN_POINT ( 'NONE',  ( -5.405949406249996869, 9.363379034771805109, -49.03125000204838813 ) ) ;
#32036 = CARTESIAN_POINT ( 'NONE',  ( -8.408428485261246976, 6.678869664728471101, -100.0000000000000000 ) ) ;
#32037 = CARTESIAN_POINT ( 'NONE',  ( -2.293366432827344421E-15, -12.48450537969573659, -171.2187500020484094 ) ) ;
#32038 = CARTESIAN_POINT ( 'NONE',  ( -5.000000000000003553, -8.660254037844383745, -139.0000000000000000 ) ) ;
#32039 = CARTESIAN_POINT ( 'NONE',  ( 5.405949406249999534, 9.363379034771803333, -148.2812500020483810 ) ) ;
#32040 = PRODUCT_RELATED_PRODUCT_CATEGORY ( 'detail', '', ( #21848 ) ) ;
#32041 = CARTESIAN_POINT ( 'NONE',  ( -9.999999999999998224, 1.224646799147353059E-15, -24.12500000409675849 ) ) ;
#32042 = CARTESIAN_POINT ( 'NONE',  ( -5.405949406250003975, -9.363379034771801557, -36.53125000204837391 ) ) ;
#32043 = CARTESIAN_POINT ( 'NONE',  ( 9.999999999999998224, 0.000000000000000000, -123.8750000040967905 ) ) ;
#32044 = CARTESIAN_POINT ( 'NONE',  ( -9.999999999999998224, 5.773502691896259087, -100.3750000000000000 ) ) ;
#32045 = ORIENTED_EDGE ( 'NONE', *, *, #35749, .F. ) ;
#32046 = CARTESIAN_POINT ( 'NONE',  ( -5.405949406249996869, 9.363379034771805109, -121.0312500020483952 ) ) ;
#32047 = CARTESIAN_POINT ( 'NONE',  ( 5.000000000000000000, 8.660254037844385522, -140.1250000040967905 ) ) ;
#32048 = CYLINDRICAL_SURFACE ( 'NONE', #42198, 9.999999999999998224 ) ;
#32049 = CARTESIAN_POINT ( 'NONE',  ( -5.405949406249996869, 9.363379034771805109, -172.0312500020484094 ) ) ;
#32050 = CARTESIAN_POINT ( 'NONE',  ( 9.999999999999998224, 0.000000000000000000, -48.87500000409678336 ) ) ;
#32051 =( BOUNDED_CURVE ( )  B_SPLINE_CURVE ( 2, ( #38684, #28775, #11702, #41903, #9118, #41482, #25110 ),
 .UNSPECIFIED., .F., .F. ) 
 B_SPLINE_CURVE_WITH_KNOTS ( ( 3, 2, 2, 3 ),
 ( 0.7052238805970151292, 0.7064676616915425145, 0.7077114427860698997, 0.7089552238805972850 ),
 .UNSPECIFIED. ) 
 CURVE ( )  GEOMETRIC_REPRESENTATION_ITEM ( )  RATIONAL_B_SPLINE_CURVE ( ( 0.9999999999999761302, 0.8660254037844625774, 1.000000000000000000, 0.8660254037844387076, 1.000000000000000000, 0.8660254037844148378, 1.000000000000023981 ) ) 
 REPRESENTATION_ITEM ( '' )  );
#32052 = CARTESIAN_POINT ( 'NONE',  ( -9.999999999999479527, -5.773502691896549521, -98.62499999999998579 ) ) ;
#32053 = CARTESIAN_POINT ( 'NONE',  ( -10.81189881249999907, -6.242252689847864744, -59.15625000204838102 ) ) ;
#32054 = CARTESIAN_POINT ( 'NONE',  ( 7.644554776091147741E-16, 12.48450537969573659, -167.6562500020483810 ) ) ;
#32055 = EDGE_CURVE ( 'NONE', #26056, #31902, #11988, .T. ) ;
#32056 = CARTESIAN_POINT ( 'NONE',  ( 7.423074889580959734, 12.85714285714296423, 52.14285714285716011 ) ) ;
#32057 = LINE ( 'NONE', #15196, #23416 ) ;
#32058 = EDGE_LOOP ( 'NONE', ( #10532, #484, #27750, #11630 ) ) ;
#32059 = CARTESIAN_POINT ( 'NONE',  ( 9.999999999999998224, 0.000000000000000000, -173.3750000040968189 ) ) ;
#32060 = CARTESIAN_POINT ( 'NONE',  ( 9.999999999999998224, 0.000000000000000000, -162.8750000040967905 ) ) ;
#32062 = ORIENTED_EDGE ( 'NONE', *, *, #26529, .F. ) ;
#32061 = CARTESIAN_POINT ( 'NONE',  ( 10.81189881249999551, -6.242252689847874514, -76.65625000204838102 ) ) ;
#32063 = DIRECTION ( 'NONE',  ( 0.000000000000000000, 0.000000000000000000, 1.000000000000000000 ) ) ;
#32065 = ORIENTED_EDGE ( 'NONE', *, *, #3533, .F. ) ;
#32064 = CARTESIAN_POINT ( 'NONE',  ( 9.999999999999998224, 1.224646799147353059E-15, -99.99999999999998579 ) ) ;
#32066 = ORIENTED_EDGE ( 'NONE', *, *, #19280, .F. ) ;
#32067 = CARTESIAN_POINT ( 'NONE',  ( 5.405949406249999534, 9.363379034771803333, -28.09375000204836326 ) ) ;
#32068 = CARTESIAN_POINT ( 'NONE',  ( 9.999999999999479527, 5.773502691896553074, -74.25000000409676204 ) ) ;
#32069 = CARTESIAN_POINT ( 'NONE',  ( -10.81189881249999729, 1.324075727343319199E-15, -2.281250002048373915 ) ) ;
#32071 = ORIENTED_EDGE ( 'NONE', *, *, #12806, .T. ) ;
#32070 = CARTESIAN_POINT ( 'NONE',  ( -10.81189881249999907, -6.242252689847864744, -57.46875000204835970 ) ) ;
#32072 = CARTESIAN_POINT ( 'NONE',  ( 10.00000000000051159, -5.773502691895965988, -3.624999999999940492 ) ) ;
#32073 = CARTESIAN_POINT ( 'NONE',  ( -9.999999999999998224, 1.224646799147353059E-15, -35.74999999999997868 ) ) ;
#32074 = CARTESIAN_POINT ( 'NONE',  ( -2.293366432827344421E-15, -12.48450537969573659, -189.2187500020484094 ) ) ;
#32075 = CARTESIAN_POINT ( 'NONE',  ( -10.81189881249999729, 6.242252689847871849, -174.7187500020483810 ) ) ;
#32076 = CARTESIAN_POINT ( 'NONE',  ( -5.405949406249996869, 9.363379034771805109, -159.8437500020484094 ) ) ;
#32077 = CARTESIAN_POINT ( 'NONE',  ( 10.81189881249999729, 0.000000000000000000, -173.8437500020484094 ) ) ;
#32078 = CARTESIAN_POINT ( 'NONE',  ( -9.999999999999998224, 1.224646799147353059E-15, -76.24999999999998579 ) ) ;
#32079 = VECTOR ( 'NONE', #12847, 1000.000000000000000 ) ;
#32080 = CARTESIAN_POINT ( 'NONE',  ( -9.999999999999998224, 0.000000000000000000, -99.99999999999998579 ) ) ;
#32081 = CARTESIAN_POINT ( 'NONE',  ( 9.999999999999996447, -5.773502691896262640, -192.6250000000000284 ) ) ;
#32082 = CARTESIAN_POINT ( 'NONE',  ( -10.81189881249999729, 6.242252689847871849, -102.7187500020483810 ) ) ;
#32083 = CARTESIAN_POINT ( 'NONE',  ( -10.00000000000007994, 5.773502691896212013, -196.3750000000000000 ) ) ;
#32084 = CARTESIAN_POINT ( 'NONE',  ( 5.405949406249992428, -9.363379034771808662, -76.78125000204838102 ) ) ;
#32085 = CARTESIAN_POINT ( 'NONE',  ( 10.81189881249999729, 6.242252689847867408, -89.71875000204838102 ) ) ;
#32086 = CARTESIAN_POINT ( 'NONE',  ( 10.81189881249999729, 0.000000000000000000, -58.53125000204836681 ) ) ;
#32087 = CARTESIAN_POINT ( 'NONE',  ( -9.999999999999998224, 1.224646799147353059E-15, -144.1250000040967905 ) ) ;
#32088 = CARTESIAN_POINT ( 'NONE',  ( -4.999999999999996447, 8.660254037844387298, -124.5000000000000000 ) ) ;
#32089 =( BOUNDED_CURVE ( )  B_SPLINE_CURVE ( 2, ( #20208, #33397, #16957, #14569, #37682, #30370, #1224 ),
 .UNSPECIFIED., .F., .F. ) 
 B_SPLINE_CURVE_WITH_KNOTS ( ( 3, 2, 2, 3 ),
 ( 0.8992537313432839019, 0.9004975124378112872, 0.9017412935323385614, 0.9029850746268659467 ),
 .UNSPECIFIED. ) 
 CURVE ( )  GEOMETRIC_REPRESENTATION_ITEM ( )  RATIONAL_B_SPLINE_CURVE ( ( 0.9999999999999641398, 0.8660254037844745678, 1.000000000000000000, 0.8660254037844387076, 1.000000000000000000, 0.8660254037844148378, 1.000000000000023981 ) ) 
 REPRESENTATION_ITEM ( '' )  );
#32090 = EDGE_LOOP ( 'NONE', ( #3183, #10581, #26160, #23925 ) ) ;
#32091 = CARTESIAN_POINT ( 'NONE',  ( 10.81189881249999551, -6.242252689847874514, -142.6562500020484094 ) ) ;
#32092 = CARTESIAN_POINT ( 'NONE',  ( 10.81189881249999729, 0.000000000000000000, -159.0312500020484094 ) ) ;
#32093 = EDGE_CURVE ( 'NONE', #26744, #9407, #8559, .T. ) ;
#32094 = CARTESIAN_POINT ( 'NONE',  ( 5.405949406249999534, 9.363379034771803333, -194.7812500020484094 ) ) ;
#32095 = DIRECTION ( 'NONE',  ( -0.000000000000000000, -0.000000000000000000, 1.000000000000000000 ) ) ;
#32096 = CARTESIAN_POINT ( 'NONE',  ( 5.405949406249999534, 9.363379034771803333, -88.09375000204836681 ) ) ;
#32097 = ORIENTED_EDGE ( 'NONE', *, *, #7449, .F. ) ;
#32098 = CARTESIAN_POINT ( 'NONE',  ( 7.070501591499377789E-16, 11.54700538379251284, -69.12500000000000000 ) ) ;
#32099 = CARTESIAN_POINT ( 'NONE',  ( -10.81189881249999907, -6.242252689847864744, -192.4687500020484094 ) ) ;
#32100 = CARTESIAN_POINT ( 'NONE',  ( -4.999999999999996447, 8.660254037844387298, -70.87500000409677625 ) ) ;
#32101 = CARTESIAN_POINT ( 'NONE',  ( 5.000000000000000000, 8.660254037844385522, -165.2500000000000000 ) ) ;
#32102 = CARTESIAN_POINT ( 'NONE',  ( 9.999999999999998224, 0.000000000000000000, -117.5000000000000000 ) ) ;
#32103 = CARTESIAN_POINT ( 'NONE',  ( 10.81189881249999907, 6.242252689847868297, -88.40625000204839523 ) ) ;
#32104 = AXIS2_PLACEMENT_3D ( 'NONE', #39490, #16375, #31826 ) ;
#32105 = CARTESIAN_POINT ( 'NONE',  ( 10.81189881249999551, -6.242252689847874514, -64.65625000204838102 ) ) ;
#32106 = CARTESIAN_POINT ( 'NONE',  ( 4.999999999999992006, -8.660254037844389075, -65.62500000409676204 ) ) ;
#32107 = CARTESIAN_POINT ( 'NONE',  ( 5.000000000000000000, 8.660254037844385522, -93.62500000409677625 ) ) ;
#32108 = CARTESIAN_POINT ( 'NONE',  ( 7.644554776091147741E-16, 12.48450537969573659, -29.46875000204835260 ) ) ;
#32109 = ORIENTED_EDGE ( 'NONE', *, *, #11683, .F. ) ;
#32110 = CARTESIAN_POINT ( 'NONE',  ( -5.405949406250003975, -9.363379034771801557, -189.5312500020484094 ) ) ;
#32111 = CARTESIAN_POINT ( 'NONE',  ( -5.405949406250003975, -9.363379034771801557, -20.03125000204836326 ) ) ;
#32112 = CARTESIAN_POINT ( 'NONE',  ( -10.81189881249999729, 6.242252689847871849, -5.218750002048341052 ) ) ;
#32113 = CYLINDRICAL_SURFACE ( 'NONE', #3486, 9.999999999999998224 ) ;
#32114 = AXIS2_PLACEMENT_3D ( 'NONE', #17959, #11272, #8059 ) ;
#32115 = CARTESIAN_POINT ( 'NONE',  ( 4.999999999999992006, -8.660254037844389075, -180.7500000000000284 ) ) ;
#32116 = CARTESIAN_POINT ( 'NONE',  ( 9.999999999999998224, 0.000000000000000000, -137.0000000000000000 ) ) ;
#32117 = CARTESIAN_POINT ( 'NONE',  ( -10.00000000000000000, -5.773502691896251982, -172.1250000000000284 ) ) ;
#32118 = CYLINDRICAL_SURFACE ( 'NONE', #28976, 9.999999999999998224 ) ;
#32120 = ORIENTED_EDGE ( 'NONE', *, *, #31490, .T. ) ;
#32119 = CARTESIAN_POINT ( 'NONE',  ( 5.405949406249992428, -9.363379034771808662, -99.28125000204839523 ) ) ;
#32121 = DIRECTION ( 'NONE',  ( 1.000000000000000000, 0.000000000000000000, 0.000000000000000000 ) ) ;
#32122 = VERTEX_POINT ( 'NONE', #15431 ) ;
#32123 = ORIENTED_EDGE ( 'NONE', *, *, #37545, .F. ) ;
#32124 = CARTESIAN_POINT ( 'NONE',  ( 10.81189881249999729, 0.000000000000000000, -27.03125000204836681 ) ) ;
#32125 = CONTEXT_DEPENDENT_SHAPE_REPRESENTATION ( #12980, #34946 ) ;
#32126 = CARTESIAN_POINT ( 'NONE',  ( -10.81189881249999907, -6.242252689847864744, -82.96875000204836681 ) ) ;
#32127 = DIRECTION ( 'NONE',  ( -0.000000000000000000, -0.000000000000000000, -1.000000000000000000 ) ) ;
#32128 = CARTESIAN_POINT ( 'NONE',  ( -10.81189881249999729, 6.242252689847871849, -197.2187500020484379 ) ) ;
#32129 = VECTOR ( 'NONE', #3929, 1000.000000000000000 ) ;
#32130 = VECTOR ( 'NONE', #26468, 1000.000000000000000 ) ;
#32131 = CARTESIAN_POINT ( 'NONE',  ( -9.999999999999998224, 1.224646799147353059E-15, -170.7500000000000000 ) ) ;
#32132 = CARTESIAN_POINT ( 'NONE',  ( -9.999999999999998224, 1.224646799147353059E-15, -30.12500000409676204 ) ) ;
#32133 = CARTESIAN_POINT ( 'NONE',  ( -10.81189881249999907, -6.242252689847864744, -156.6562500020483810 ) ) ;
#32134 = CARTESIAN_POINT ( 'NONE',  ( -9.999999999999998224, 1.224646799147353059E-15, -15.12500000409674961 ) ) ;
#32135 = CARTESIAN_POINT ( 'NONE',  ( -1.040834085586084257E-14, 125.0000000000000000, 22.49999999999999289 ) ) ;
#32136 = CARTESIAN_POINT ( 'NONE',  ( 5.405949406249999534, 9.363379034771803333, -128.5937500020483810 ) ) ;
#32137 = CARTESIAN_POINT ( 'NONE',  ( 10.81189881249999729, 6.242252689847867408, -116.7187500020483810 ) ) ;
#32138 = AXIS2_PLACEMENT_3D ( 'NONE', #29564, #17016, #33018 ) ;
#32139 = CARTESIAN_POINT ( 'NONE',  ( -5.405949406250003975, -9.363379034771801557, -73.84375000204838102 ) ) ;
#32140 = CARTESIAN_POINT ( 'NONE',  ( -10.81189881249999729, 6.242252689847871849, -84.90625000204838102 ) ) ;
#32141 = CARTESIAN_POINT ( 'NONE',  ( 7.070501591499377789E-16, 11.54700538379251284, -170.0000000040967905 ) ) ;
#32142 = CARTESIAN_POINT ( 'NONE',  ( -2.121150477449813534E-15, -11.54700538379251284, -133.2500000040967905 ) ) ;
#32143 = CARTESIAN_POINT ( 'NONE',  ( -2.293366432827344421E-15, -12.48450537969573659, -168.4062500020484379 ) ) ;
#32144 = CARTESIAN_POINT ( 'NONE',  ( -5.405949406249996869, 9.363379034771805109, -188.5312500020484094 ) ) ;
#32145 = CARTESIAN_POINT ( 'NONE',  ( -10.81189881249999729, -6.242252689847864744, -46.96875000204837391 ) ) ;
#32146 = CARTESIAN_POINT ( 'NONE',  ( 5.000000000000000000, 8.660254037844385522, -164.1250000040967905 ) ) ;
#32147 = CARTESIAN_POINT ( 'NONE',  ( -10.81189881249999907, -6.242252689847864744, -5.156250002048356151 ) ) ;
#32148 = CARTESIAN_POINT ( 'NONE',  ( -10.81189881249999907, -6.242252689847864744, -16.96875000204836681 ) ) ;
#32149 = CARTESIAN_POINT ( 'NONE',  ( 7.070501591499376803E-16, 11.54700538379251284, -127.6249999999999858 ) ) ;
#32150 = CARTESIAN_POINT ( 'NONE',  ( 7.644554776091147741E-16, 12.48450537969573659, -117.9687500020483668 ) ) ;
#32151 = CARTESIAN_POINT ( 'NONE',  ( -10.00000000000000000, -5.773502691896251982, -92.62499999999998579 ) ) ;
#32152 = CARTESIAN_POINT ( 'NONE',  ( -10.81189881249999729, 1.324075727343319199E-15, -21.78125000204836326 ) ) ;
#32153 = CARTESIAN_POINT ( 'NONE',  ( -9.999999999999998224, 1.224646799147353059E-15, -97.62500000409677625 ) ) ;
#32154 = CARTESIAN_POINT ( 'NONE',  ( -9.999999999999834799, -5.773502691896343464, -190.5000000040967905 ) ) ;
#32155 = CARTESIAN_POINT ( 'NONE',  ( -5.405949406250003975, -9.363379034771801557, -113.0312500020483952 ) ) ;
#32156 = CARTESIAN_POINT ( 'NONE',  ( 7.644554776091147741E-16, 12.48450537969573659, -94.15625000204839523 ) ) ;
#32157 = ORIENTED_EDGE ( 'NONE', *, *, #38901, .T. ) ;
#32158 = CARTESIAN_POINT ( 'NONE',  ( 9.999999999999996447, -5.773502691896262640, -94.00000000409677625 ) ) ;
#32159 = CARTESIAN_POINT ( 'NONE',  ( 7.070501591499376803E-16, 11.54700538379251284, -4.624999999999958256 ) ) ;
#32160 = CARTESIAN_POINT ( 'NONE',  ( -10.81189881249999907, -6.242252689847864744, -156.6562500020483810 ) ) ;
#32161 = CARTESIAN_POINT ( 'NONE',  ( 10.81189881249999729, 0.000000000000000000, -53.84375000204835970 ) ) ;
#32162 = ORIENTED_EDGE ( 'NONE', *, *, #24644, .F. ) ;
#32163 = CARTESIAN_POINT ( 'NONE',  ( -5.000000000000003553, -8.660254037844383745, -18.99999999999996092 ) ) ;
#32164 = CARTESIAN_POINT ( 'NONE',  ( -10.81189881249999729, 6.242252689847871849, -23.40625000204837747 ) ) ;
#32165 = CARTESIAN_POINT ( 'NONE',  ( -9.999999999999998224, 5.773502691896259087, -154.3749999999999716 ) ) ;
#32166 = CARTESIAN_POINT ( 'NONE',  ( 5.000000000000000000, 8.660254037844385522, -18.62500000409675494 ) ) ;
#32167 = AXIS2_PLACEMENT_3D ( 'NONE', #21111, #7531, #1493 ) ;
#32168 = ADVANCED_FACE ( 'NONE', ( #8766 ), #19107, .F. ) ;
#32169 = CARTESIAN_POINT ( 'NONE',  ( -2.121150477449813534E-15, -11.54700538379251284, -197.3750000000000284 ) ) ;
#32171 = ORIENTED_EDGE ( 'NONE', *, *, #25843, .F. ) ;
#32170 = CARTESIAN_POINT ( 'NONE',  ( -10.81189881249999907, -6.242252689847864744, -125.1562500020483810 ) ) ;
#32172 = DIRECTION ( 'NONE',  ( -1.734723475976806848E-16, 1.000000000000000000, 0.000000000000000000 ) ) ;
#32173 = EDGE_LOOP ( 'NONE', ( #32045, #41549, #7728, #15784 ) ) ;
#32174 = CARTESIAN_POINT ( 'NONE',  ( 7.644554776091147741E-16, 12.48450537969573659, -50.65625000204838102 ) ) ;
#32175 = SHAPE_DEFINITION_REPRESENTATION ( #23885, #36293 ) ;
#32176 = CARTESIAN_POINT ( 'NONE',  ( -2.293366432827344421E-15, -12.48450537969573659, -105.2187500020483952 ) ) ;
#32178 = ORIENTED_EDGE ( 'NONE', *, *, #713, .F. ) ;
#32177 = VERTEX_POINT ( 'NONE', #32499 ) ;
#32179 = FACE_OUTER_BOUND ( 'NONE', #17555, .T. ) ;
#32180 = DIRECTION ( 'NONE',  ( -0.000000000000000000, -0.000000000000000000, 1.000000000000000000 ) ) ;
#32181 = CARTESIAN_POINT ( 'NONE',  ( 5.405949406249992428, -9.363379034771808662, -156.0937500020483810 ) ) ;
#32182 = CARTESIAN_POINT ( 'NONE',  ( -10.81189881249999729, 6.242252689847871849, -182.4062500020483810 ) ) ;
#32183 = CARTESIAN_POINT ( 'NONE',  ( 7.644554776091147741E-16, 12.48450537969573659, -5.468750002048341941 ) ) ;
#32184 = DIRECTION ( 'NONE',  ( -0.000000000000000000, -0.000000000000000000, -1.000000000000000000 ) ) ;
#32185 = EDGE_CURVE ( 'NONE', #28503, #6727, #9750, .T. ) ;
#32186 = CARTESIAN_POINT ( 'NONE',  ( 10.81189881249999729, 0.000000000000000000, -142.3437500020483810 ) ) ;
#32187 = CARTESIAN_POINT ( 'NONE',  ( 7.644554776091147741E-16, 12.48450537969573659, -105.9687500020483668 ) ) ;
#32188 = CARTESIAN_POINT ( 'NONE',  ( -2.121150477449813534E-15, -11.54700538379251284, -143.3750000000000000 ) ) ;
#32189 = CARTESIAN_POINT ( 'NONE',  ( -10.81189881249999729, 1.324075727343319199E-15, -113.2812500020483952 ) ) ;
#32190 = CARTESIAN_POINT ( 'NONE',  ( -10.00000000000000000, -5.773502691896251982, -192.0000000040968189 ) ) ;
#32191 = CARTESIAN_POINT ( 'NONE',  ( -10.81189881249999729, 6.242252689847871849, -119.2187500020483810 ) ) ;
#32192 = CARTESIAN_POINT ( 'NONE',  ( 5.405949406249999534, 9.363379034771803333, -196.2812500020484094 ) ) ;
#32193 = CARTESIAN_POINT ( 'NONE',  ( 5.000000000000000000, 8.660254037844385522, -149.1250000040967905 ) ) ;
#32194 = CARTESIAN_POINT ( 'NONE',  ( -9.999999999999998224, 1.224646799147353059E-15, -136.2499999999999716 ) ) ;
#32195 = CARTESIAN_POINT ( 'NONE',  ( -10.00000000000000000, -5.773502691896251982, -13.12499999999997158 ) ) ;
#32196 = CARTESIAN_POINT ( 'NONE',  ( -10.81189881249999729, -6.242252689847864744, -66.46875000204838102 ) ) ;
#32197 = CARTESIAN_POINT ( 'NONE',  ( -10.81189881249999729, 6.242252689847871849, -59.21875000204837391 ) ) ;
#32198 = CARTESIAN_POINT ( 'NONE',  ( -10.00000000000000000, -5.773502691896251982, -192.0000000040968189 ) ) ;
#32199 = CARTESIAN_POINT ( 'NONE',  ( 5.405949406249999534, 9.363379034771803333, -28.28125000204837036 ) ) ;
#32200 = CARTESIAN_POINT ( 'NONE',  ( 5.405949406249992428, -9.363379034771808662, -37.59375000204837391 ) ) ;
#32201 = CARTESIAN_POINT ( 'NONE',  ( 4.999999999999992006, -8.660254037844389075, -142.1250000040967905 ) ) ;
#32202 = CARTESIAN_POINT ( 'NONE',  ( -5.405949406250003975, -9.363379034771801557, -147.3437500020483810 ) ) ;
#32203 = CARTESIAN_POINT ( 'NONE',  ( 7.070501591499377789E-16, 11.54700538379251284, -112.6249999999999858 ) ) ;
#32204 = DIRECTION ( 'NONE',  ( -0.000000000000000000, -0.000000000000000000, -1.000000000000000000 ) ) ;
#32205 = CARTESIAN_POINT ( 'NONE',  ( -10.00000000000000000, -5.773502691896251982, -70.12500000000000000 ) ) ;
#32206 = CARTESIAN_POINT ( 'NONE',  ( 10.81189881249999729, 0.000000000000000000, -142.5312500020483810 ) ) ;
#32207 = CARTESIAN_POINT ( 'NONE',  ( 10.81189881249999729, 6.242252689847867408, -116.9062500020483952 ) ) ;
#32208 = ORIENTED_EDGE ( 'NONE', *, *, #31921, .F. ) ;
#32209 = CARTESIAN_POINT ( 'NONE',  ( 9.999999999999998224, 0.000000000000000000, -200.0000000000000000 ) ) ;
#32210 = CARTESIAN_POINT ( 'NONE',  ( -9.999999999999998224, 5.773502691896259087, -118.7500000040967905 ) ) ;
#32211 = DIRECTION ( 'NONE',  ( 0.6123724356957960246, 0.3535533905932753962, 0.7071067811865453523 ) ) ;
#32212 = CARTESIAN_POINT ( 'NONE',  ( -10.81189881249999907, -6.242252689847864744, -70.96875000204838102 ) ) ;
#32213 = CARTESIAN_POINT ( 'NONE',  ( 9.999999999999998224, 0.000000000000000000, -42.49999999999998579 ) ) ;
#32214 = CARTESIAN_POINT ( 'NONE',  ( 10.00000000000000000, 5.773502691896255534, -29.25000000409675494 ) ) ;
#32215 = CARTESIAN_POINT ( 'NONE',  ( -5.405949406249996869, 9.363379034771805109, -52.03125000204835970 ) ) ;
#32216 = CARTESIAN_POINT ( 'NONE',  ( 10.00000000000025402, -5.773502691896113426, -157.0000000040968189 ) ) ;
#32217 = CARTESIAN_POINT ( 'NONE',  ( 10.81189881249999729, 0.000000000000000000, -36.03125000204837391 ) ) ;
#32218 =( BOUNDED_CURVE ( )  B_SPLINE_CURVE ( 2, ( #9913, #10917, #9, #26329, #23089, #19206, #30373 ),
 .UNSPECIFIED., .F., .F. ) 
 B_SPLINE_CURVE_WITH_KNOTS ( ( 3, 2, 2, 3 ),
 ( 0.8619402985074630097, 0.8631840796019903950, 0.8644278606965177802, 0.8656716417910450545 ),
 .UNSPECIFIED. ) 
 CURVE ( )  GEOMETRIC_REPRESENTATION_ITEM ( )  RATIONAL_B_SPLINE_CURVE ( ( 0.9999999999999641398, 0.8660254037844745678, 1.000000000000000000, 0.8660254037844387076, 1.000000000000000000, 0.8660254037844028474, 1.000000000000035971 ) ) 
 REPRESENTATION_ITEM ( '' )  );
#32219 = CARTESIAN_POINT ( 'NONE',  ( 7.070501591499376803E-16, 11.54700538379251284, -24.12499999999998224 ) ) ;
#32220 = CARTESIAN_POINT ( 'NONE',  ( -10.81189881249999729, 1.324075727343319199E-15, -143.2812500020483810 ) ) ;
#32221 = CARTESIAN_POINT ( 'NONE',  ( 7.644554776091147741E-16, 12.48450537969573659, -152.6562500020484094 ) ) ;
#32223 = EDGE_CURVE ( 'NONE', #34698, #9647, #31656, .T. ) ;
#32222 = CARTESIAN_POINT ( 'NONE',  ( 5.000000000000000000, 8.660254037844385522, -153.2500000000000000 ) ) ;
#32224 = LINE ( 'NONE', #5885, #10726 ) ;
#32225 = ORIENTED_EDGE ( 'NONE', *, *, #41203, .F. ) ;
#32226 = EDGE_LOOP ( 'NONE', ( #16283, #32267, #31742, #10850 ) ) ;
#32227 = EDGE_LOOP ( 'NONE', ( #28068, #13390, #39468, #25585 ) ) ;
#32228 = DIRECTION ( 'NONE',  ( 1.000000000000000000, 0.000000000000000000, 0.000000000000000000 ) ) ;
#32229 = CARTESIAN_POINT ( 'NONE',  ( -10.81189881249999729, 6.242252689847871849, -183.7187500020484379 ) ) ;
#32230 = CARTESIAN_POINT ( 'NONE',  ( 5.405949406249992428, -9.363379034771808662, -28.59375000204836326 ) ) ;
#32231 = CARTESIAN_POINT ( 'NONE',  ( -9.999999999999998224, 1.224646799147353059E-15, -200.0000000000000000 ) ) ;
#32232 = CARTESIAN_POINT ( 'NONE',  ( -5.405949406249996869, 9.363379034771805109, -165.8437500020484094 ) ) ;
#32233 = CARTESIAN_POINT ( 'NONE',  ( 10.81189881249999729, 0.000000000000000000, -143.8437500020483810 ) ) ;
#32234 = CARTESIAN_POINT ( 'NONE',  ( -9.999999999999998224, 1.224646799147353059E-15, -200.0000000000000000 ) ) ;
#32235 = CARTESIAN_POINT ( 'NONE',  ( 10.81189881249999551, -6.242252689847874514, -134.9687500020483810 ) ) ;
#32236 = CARTESIAN_POINT ( 'NONE',  ( 7.644554776091147741E-16, 12.48450537969573659, -143.6562500020484094 ) ) ;
#32237 = CARTESIAN_POINT ( 'NONE',  ( -5.405949406250003975, -9.363379034771801557, -21.34375000204835615 ) ) ;
#32238 = CARTESIAN_POINT ( 'NONE',  ( 10.81189881249999551, -6.242252689847874514, -143.9687500020484094 ) ) ;
#32239 = CARTESIAN_POINT ( 'NONE',  ( 7.070501591499376803E-16, 11.54700538379251284, -157.6250000000000284 ) ) ;
#32240 = CARTESIAN_POINT ( 'NONE',  ( -4.999999999999996447, 8.660254037844387298, -166.5000000000000000 ) ) ;
#32241 = CARTESIAN_POINT ( 'NONE',  ( 5.405949406249992428, -9.363379034771808662, -84.09375000204836681 ) ) ;
#32242 = CARTESIAN_POINT ( 'NONE',  ( -2.121150477449813534E-15, -11.54700538379251284, -114.8749999999999716 ) ) ;
#32243 = CARTESIAN_POINT ( 'NONE',  ( -10.81189881249999729, 6.242252689847871849, -53.40625000204837391 ) ) ;
#32244 = CARTESIAN_POINT ( 'NONE',  ( 10.81189881249999551, -6.242252689847874514, -64.46875000204838102 ) ) ;
#32245 = CARTESIAN_POINT ( 'NONE',  ( -5.000000000000003553, -8.660254037844383745, -175.0000000000000284 ) ) ;
#32246 = CARTESIAN_POINT ( 'NONE',  ( 10.81189881249999729, 0.000000000000000000, -169.3437500020484094 ) ) ;
#32247 = CARTESIAN_POINT ( 'NONE',  ( -10.00000000000000000, -5.773502691896251982, -134.6250000000000000 ) ) ;
#32248 = CARTESIAN_POINT ( 'NONE',  ( -2.293366432827344421E-15, -12.48450537969573659, -142.9062500020484094 ) ) ;
#32249 = FACE_OUTER_BOUND ( 'NONE', #40645, .T. ) ;
#32250 = CARTESIAN_POINT ( 'NONE',  ( 4.999999999999992006, -8.660254037844389075, -125.6250000040967620 ) ) ;
#32251 = CARTESIAN_POINT ( 'NONE',  ( -5.000000000000003553, -8.660254037844383745, -89.49999999999998579 ) ) ;
#32252 = ORIENTED_EDGE ( 'NONE', *, *, #14608, .T. ) ;
#32253 = CARTESIAN_POINT ( 'NONE',  ( -10.81189881249999729, 1.324075727343319199E-15, -119.2812500020483952 ) ) ;
#32254 = CARTESIAN_POINT ( 'NONE',  ( -5.000000000000003553, -8.660254037844383745, -137.8750000040967905 ) ) ;
#32255 = CARTESIAN_POINT ( 'NONE',  ( 10.00000000000154010, -5.773502691895370020, -22.00000000409673007 ) ) ;
#32256 = CARTESIAN_POINT ( 'NONE',  ( 10.81189881249999551, -6.242252689847874514, -171.1562500020484094 ) ) ;
#32257 = CARTESIAN_POINT ( 'NONE',  ( -5.000000000000003553, -8.660254037844383745, -52.37500000409675494 ) ) ;
#32258 = CARTESIAN_POINT ( 'NONE',  ( -2.121150477449813534E-15, -11.54700538379251284, -98.37500000000000000 ) ) ;
#32259 = CARTESIAN_POINT ( 'NONE',  ( -2.293366432827344421E-15, -12.48450537969573659, -61.90625000204838813 ) ) ;
#32260 = CARTESIAN_POINT ( 'NONE',  ( -4.999999999999996447, 8.660254037844387298, -9.375000004096744277 ) ) ;
#32261 = CARTESIAN_POINT ( 'NONE',  ( 7.644554776091147741E-16, 12.48450537969573659, -166.1562500020483810 ) ) ;
#32262 = EDGE_CURVE ( 'NONE', #26141, #32541, #18585, .T. ) ;
#32263 = CARTESIAN_POINT ( 'NONE',  ( -10.00000000000051337, 5.773502691895962435, -7.374999999999958256 ) ) ;
#32265 = EDGE_CURVE ( 'NONE', #21453, #32177, #13031, .T. ) ;
#32264 = CARTESIAN_POINT ( 'NONE',  ( -9.999999999998969713, -5.773502691896847949, -56.62499999999995737 ) ) ;
#32266 = VECTOR ( 'NONE', #10918, 1000.000000000000000 ) ;
#32267 = ORIENTED_EDGE ( 'NONE', *, *, #9949, .T. ) ;
#32268 = ADVANCED_FACE ( 'NONE', ( #10439 ), #16263, .T. ) ;
#32269 = CARTESIAN_POINT ( 'NONE',  ( -9.999999999999998224, 1.224646799147353059E-15, -79.24999999999998579 ) ) ;
#32270 = EDGE_CURVE ( 'NONE', #34935, #19531, #26770, .T. ) ;
#32271 = CARTESIAN_POINT ( 'NONE',  ( 7.070501591499376803E-16, 11.54700538379251284, -137.0000000040967905 ) ) ;
#32273 = ORIENTED_EDGE ( 'NONE', *, *, #22707, .F. ) ;
#32272 = CARTESIAN_POINT ( 'NONE',  ( 10.81189881249999729, 0.000000000000000000, -76.53125000204838102 ) ) ;
#32275 = EDGE_LOOP ( 'NONE', ( #473, #268 ) ) ;
#32274 = CARTESIAN_POINT ( 'NONE',  ( -4.999999999999996447, 8.660254037844387298, -29.99999999999997158 ) ) ;
#32276 = ORIENTED_EDGE ( 'NONE', *, *, #39156, .T. ) ;
#32277 = CARTESIAN_POINT ( 'NONE',  ( 10.81189881249999551, -6.242252689847874514, -32.96875000204834549 ) ) ;
#32278 = CARTESIAN_POINT ( 'NONE',  ( 10.00000000000076916, -5.773502691895816774, -106.0000000040967763 ) ) ;
#32279 = CARTESIAN_POINT ( 'NONE',  ( -10.81189881249999907, -6.242252689847864744, -8.156250002048370362 ) ) ;
#32281 = ORIENTED_EDGE ( 'NONE', *, *, #28864, .T. ) ;
#32280 = CARTESIAN_POINT ( 'NONE',  ( 10.81189881249999551, -6.242252689847874514, -52.46875000204837391 ) ) ;
#32282 = DIRECTION ( 'NONE',  ( -1.000000000000000000, 0.000000000000000000, 0.000000000000000000 ) ) ;
#32283 = CARTESIAN_POINT ( 'NONE',  ( -2.121150477449813534E-15, -11.54700538379251284, -27.87499999999998224 ) ) ;
#32284 = EDGE_CURVE ( 'NONE', #11758, #21425, #16904, .T. ) ;
#32285 = CARTESIAN_POINT ( 'NONE',  ( -10.81189881249999729, 1.324075727343319199E-15, -189.5937500020483810 ) ) ;
#32286 = CARTESIAN_POINT ( 'NONE',  ( 5.405949406249999534, 9.363379034771803333, -178.0937500020484094 ) ) ;
#32287 = CARTESIAN_POINT ( 'NONE',  ( -10.81189881249999729, 1.324075727343319199E-15, -156.5937500020483810 ) ) ;
#32288 = CARTESIAN_POINT ( 'NONE',  ( -10.81189881249999729, 1.324075727343319199E-15, -173.0937500020484094 ) ) ;
#32289 = CARTESIAN_POINT ( 'NONE',  ( 9.999999999999998224, 0.000000000000000000, -168.5000000000000000 ) ) ;
#32290 = DIRECTION ( 'NONE',  ( -1.000000000000000000, 0.000000000000000000, 0.000000000000000000 ) ) ;
#32291 = EDGE_CURVE ( 'NONE', #2592, #7682, #33224, .T. ) ;
#32292 = CARTESIAN_POINT ( 'NONE',  ( -2.121150477449813534E-15, -11.54700538379251284, -183.8750000000000284 ) ) ;
#32293 = CARTESIAN_POINT ( 'NONE',  ( -5.405949406249996869, 9.363379034771805109, -107.3437500020483810 ) ) ;
#32294 = CARTESIAN_POINT ( 'NONE',  ( 9.999999999999998224, 0.000000000000000000, -197.0000000000000000 ) ) ;
#32295 = CARTESIAN_POINT ( 'NONE',  ( -10.81189881249999729, 6.242252689847871849, -77.40625000204838102 ) ) ;
#32296 = CARTESIAN_POINT ( 'NONE',  ( 10.81189881249999729, 0.000000000000000000, -6.031250002048377468 ) ) ;
#32297 = CARTESIAN_POINT ( 'NONE',  ( -10.81189881249999729, 6.242252689847871849, -80.21875000204838102 ) ) ;
#32298 = ADVANCED_FACE ( 'NONE', ( #40008 ), #36355, .F. ) ;
#32299 = AXIS2_PLACEMENT_3D ( 'NONE', #2034, #38061, #15799 ) ;
#32300 =( BOUNDED_CURVE ( )  B_SPLINE_CURVE ( 2, ( #37842, #38854, #31168, #4821, #22247, #15742, #19000 ),
 .UNSPECIFIED., .F., .F. ) 
 B_SPLINE_CURVE_WITH_KNOTS ( ( 3, 2, 2, 3 ),
 ( 0.2985074626865671932, 0.2997512437810946340, 0.3009950248756220192, 0.3022388059701494045 ),
 .UNSPECIFIED. ) 
 CURVE ( )  GEOMETRIC_REPRESENTATION_ITEM ( )  RATIONAL_B_SPLINE_CURVE ( ( 0.9999999999999940048, 0.8660254037844447028, 1.000000000000000000, 0.8660254037844387076, 1.000000000000000000, 0.8660254037844207220, 1.000000000000017986 ) ) 
 REPRESENTATION_ITEM ( '' )  );
#32301 = CARTESIAN_POINT ( 'NONE',  ( 7.644554776091147741E-16, 12.48450537969573659, -61.15625000204838102 ) ) ;
#32302 = CARTESIAN_POINT ( 'NONE',  ( 5.000000000000000000, 8.660254037844385522, -146.1250000040967905 ) ) ;
#32303 = CARTESIAN_POINT ( 'NONE',  ( -5.000000000000003553, -8.660254037844383745, -125.5000000000000000 ) ) ;
#32304 = VERTEX_POINT ( 'NONE', #19519 ) ;
#32305 = CARTESIAN_POINT ( 'NONE',  ( 7.644554776091147741E-16, 12.48450537969573659, -140.6562500020484094 ) ) ;
#32306 = CARTESIAN_POINT ( 'NONE',  ( 10.81189881249999729, 0.000000000000000000, -156.0312500020484094 ) ) ;
#32307 = CARTESIAN_POINT ( 'NONE',  ( 7.644554776091147741E-16, 12.48450537969573659, -193.1562500020484094 ) ) ;
#32308 = CARTESIAN_POINT ( 'NONE',  ( 9.999999999999998224, 0.000000000000000000, -51.49999999999996447 ) ) ;
#32309 = CARTESIAN_POINT ( 'NONE',  ( -10.81189881249999907, -6.242252689847864744, -88.96875000204836681 ) ) ;
#32310 = ORIENTED_EDGE ( 'NONE', *, *, #30576, .F. ) ;
#32311 = CARTESIAN_POINT ( 'NONE',  ( 9.999999999999996447, -5.773502691896262640, -63.62499999999999289 ) ) ;
#32312 = CARTESIAN_POINT ( 'NONE',  ( -10.81189881249999729, 6.242252689847871849, -191.2187500020484663 ) ) ;
#32313 = CARTESIAN_POINT ( 'NONE',  ( 9.999999999999996447, -5.773502691896262640, -74.50000000409677625 ) ) ;
#32314 = LINE ( 'NONE', #42416, #32079 ) ;
#32315 = CARTESIAN_POINT ( 'NONE',  ( 9.999999999999998224, 0.000000000000000000, -123.5000000000000000 ) ) ;
#32316 = CARTESIAN_POINT ( 'NONE',  ( 5.405949406249992428, -9.363379034771808662, -87.28125000204838102 ) ) ;
#32317 = CARTESIAN_POINT ( 'NONE',  ( 10.81189881249999729, 6.242252689847867408, -67.40625000204839523 ) ) ;
#32318 = CARTESIAN_POINT ( 'NONE',  ( 4.999999999999992006, -8.660254037844389075, -61.12500000409676204 ) ) ;
#32319 = CARTESIAN_POINT ( 'NONE',  ( 10.81189881249999907, 6.242252689847868297, -14.71875000204836326 ) ) ;
#32320 = ORIENTED_EDGE ( 'NONE', *, *, #34357, .F. ) ;
#32321 = CARTESIAN_POINT ( 'NONE',  ( -2.293366432827344421E-15, -12.48450537969573659, -192.4062500020484094 ) ) ;
#32322 = CARTESIAN_POINT ( 'NONE',  ( 10.81189881249999551, -6.242252689847874514, -9.156250002048365033 ) ) ;
#32323 = CARTESIAN_POINT ( 'NONE',  ( -2.293366432827344421E-15, -12.48450537969573659, -7.718750002048352599 ) ) ;
#32324 = CARTESIAN_POINT ( 'NONE',  ( -9.999999999999998224, 1.224646799147353059E-15, -136.6250000040967620 ) ) ;
#32325 = CARTESIAN_POINT ( 'NONE',  ( -10.00000000000000000, -5.773502691896251982, -4.096750716442443263E-09 ) ) ;
#32326 = CARTESIAN_POINT ( 'NONE',  ( -9.999999999999998224, 1.224646799147353059E-15, -133.2499999999999716 ) ) ;
#32327 = EDGE_CURVE ( 'NONE', #28547, #41040, #37617, .T. ) ;
#32328 = CARTESIAN_POINT ( 'NONE',  ( -5.000000000000003553, -8.660254037844383745, -178.0000000000000000 ) ) ;
#32329 = CARTESIAN_POINT ( 'NONE',  ( -10.00000000000051337, 5.773502691895962435, -97.37499999999998579 ) ) ;
#32330 = EDGE_CURVE ( 'NONE', #15832, #5830, #18837, .T. ) ;
#32332 = ORIENTED_EDGE ( 'NONE', *, *, #26453, .T. ) ;
#32331 = CARTESIAN_POINT ( 'NONE',  ( -10.81189881249999729, 1.324075727343319199E-15, -102.7812500020483952 ) ) ;
#32333 = CARTESIAN_POINT ( 'NONE',  ( -5.000000000000003553, -8.660254037844383745, -179.8750000040967905 ) ) ;
#32334 = VECTOR ( 'NONE', #26604, 1000.000000000000000 ) ;
#32335 = EDGE_LOOP ( 'NONE', ( #1863, #6623, #9537, #6938 ) ) ;
#32336 = VERTEX_POINT ( 'NONE', #12824 ) ;
#32337 = CARTESIAN_POINT ( 'NONE',  ( -10.81189881249999907, -6.242252689847864744, -27.65625000204838457 ) ) ;
#32338 = CALENDAR_DATE ( 2026, 28, 9 ) ;
#32339 = CARTESIAN_POINT ( 'NONE',  ( 7.644554776091147741E-16, 12.48450537969573659, -78.96875000204839523 ) ) ;
#32340 = FACE_OUTER_BOUND ( 'NONE', #17002, .T. ) ;
#32341 = CARTESIAN_POINT ( 'NONE',  ( 22.00000000000000711, 2.694222958124177598E-15, -99.99999999999998579 ) ) ;
#32342 = EDGE_CURVE ( 'NONE', #22977, #29817, #14134, .T. ) ;
#32343 =( BOUNDED_CURVE ( )  B_SPLINE_CURVE ( 2, ( #23556, #7143, #46, #20296, #10792, #13170, #27204 ),
 .UNSPECIFIED., .F., .F. ) 
 B_SPLINE_CURVE_WITH_KNOTS ( ( 3, 2, 2, 3 ),
 ( 0.4328358208955225273, 0.4340796019900499125, 0.4353233830845772978, 0.4365671641791046276 ),
 .UNSPECIFIED. ) 
 CURVE ( )  GEOMETRIC_REPRESENTATION_ITEM ( )  RATIONAL_B_SPLINE_CURVE ( ( 0.9999999999999820144, 0.8660254037844566932, 1.000000000000000000, 0.8660254037844387076, 1.000000000000000000, 0.8660254037844207220, 1.000000000000017986 ) ) 
 REPRESENTATION_ITEM ( '' )  );
#32344 = CARTESIAN_POINT ( 'NONE',  ( 9.999999999999998224, 0.000000000000000000, -129.8750000040967905 ) ) ;
#32345 = LINE ( 'NONE', #4030, #35012 ) ;
#32346 = CARTESIAN_POINT ( 'NONE',  ( 5.405949406249999534, 9.363379034771803333, -158.7812500020484094 ) ) ;
#32347 = CARTESIAN_POINT ( 'NONE',  ( -9.999999999999998224, 1.224646799147353059E-15, -12.12500000409674783 ) ) ;
#32348 = CARTESIAN_POINT ( 'NONE',  ( -5.000000000000003553, -8.660254037844383745, -125.5000000000000000 ) ) ;
#32349 = CARTESIAN_POINT ( 'NONE',  ( 5.405949406249999534, 9.363379034771803333, -127.0937500020483668 ) ) ;
#32350 = CARTESIAN_POINT ( 'NONE',  ( -10.81189881249999729, 1.324075727343319199E-15, -101.2812500020483952 ) ) ;
#32351 = CARTESIAN_POINT ( 'NONE',  ( -10.81189881249999729, 1.324075727343319199E-15, -113.0937500020483810 ) ) ;
#32352 = CARTESIAN_POINT ( 'NONE',  ( -5.405949406249996869, 9.363379034771805109, -77.34375000204838102 ) ) ;
#32353 = CARTESIAN_POINT ( 'NONE',  ( 7.644554776091147741E-16, 12.48450537969573659, -82.15625000204838102 ) ) ;
#32354 = CARTESIAN_POINT ( 'NONE',  ( -5.000000000000003553, -8.660254037844383745, -166.3750000040967905 ) ) ;
#32355 =( BOUNDED_CURVE ( )  B_SPLINE_CURVE ( 2, ( #30819, #4693, #1257, #4914, #27146, #40715, #18062 ),
 .UNSPECIFIED., .F., .F. ) 
 B_SPLINE_CURVE_WITH_KNOTS ( ( 3, 2, 2, 3 ),
 ( 0.4029850746268657802, 0.4042288557213931655, 0.4054726368159204397, 0.4067164179104478250 ),
 .UNSPECIFIED. ) 
 CURVE ( )  GEOMETRIC_REPRESENTATION_ITEM ( )  RATIONAL_B_SPLINE_CURVE ( ( 0.9999999999999880096, 0.8660254037844506980, 1.000000000000000000, 0.8660254037844387076, 1.000000000000000000, 0.8660254037844327124, 1.000000000000005995 ) ) 
 REPRESENTATION_ITEM ( '' )  );
#32356 = FACE_OUTER_BOUND ( 'NONE', #28928, .T. ) ;
#32357 = CARTESIAN_POINT ( 'NONE',  ( -10.81189881249999729, 6.242252689847871849, -167.4062500020484094 ) ) ;
#32358 = CARTESIAN_POINT ( 'NONE',  ( 10.81189881249999907, 6.242252689847868297, -178.4062500020484094 ) ) ;
#32359 = CARTESIAN_POINT ( 'NONE',  ( -2.121150477449813534E-15, -11.54700538379251284, -152.7500000040967620 ) ) ;
#32360 = CARTESIAN_POINT ( 'NONE',  ( 10.81189881249999907, 6.242252689847868297, 0.09374999795163654892 ) ) ;
#32361 = CARTESIAN_POINT ( 'NONE',  ( 10.81189881249999729, 0.000000000000000000, -4.343750002048368586 ) ) ;
#32362 = LINE ( 'NONE', #42252, #6135 ) ;
#32363 = CARTESIAN_POINT ( 'NONE',  ( 7.644554776091147741E-16, 12.48450537969573659, -110.4687500020483668 ) ) ;
#32364 = CARTESIAN_POINT ( 'NONE',  ( -9.999999999999998224, 5.773502691896259087, -89.87499999999998579 ) ) ;
#32365 = CARTESIAN_POINT ( 'NONE',  ( -5.405949406249996869, 9.363379034771805109, -16.03125000204835970 ) ) ;
#32366 = CARTESIAN_POINT ( 'NONE',  ( -10.00000000000000000, -5.773502691896251982, -97.50000000409679046 ) ) ;
#32367 = CARTESIAN_POINT ( 'NONE',  ( -9.999999999999998224, 1.224646799147353059E-15, -171.1250000040968189 ) ) ;
#32368 = CARTESIAN_POINT ( 'NONE',  ( -10.81189881249999729, 6.242252689847871849, -110.4062500020483810 ) ) ;
#32369 = CARTESIAN_POINT ( 'NONE',  ( 10.81189881249999729, 6.242252689847867408, -89.90625000204839523 ) ) ;
#32370 = ORIENTED_EDGE ( 'NONE', *, *, #39145, .T. ) ;
#32371 = CARTESIAN_POINT ( 'NONE',  ( -4.999999999999996447, 8.660254037844387298, -81.37500000409677625 ) ) ;
#32372 = CARTESIAN_POINT ( 'NONE',  ( 0.000000000000000000, 0.000000000000000000, -200.0000000000000000 ) ) ;
#32373 = CARTESIAN_POINT ( 'NONE',  ( -10.81189881249999729, 1.324075727343319199E-15, -39.59375000204837391 ) ) ;
#32374 = ORIENTED_EDGE ( 'NONE', *, *, #25954, .F. ) ;
#32375 = CARTESIAN_POINT ( 'NONE',  ( -9.999999999999998224, 5.773502691896259087, -16.37499999999998224 ) ) ;
#32376 = VECTOR ( 'NONE', #41555, 1000.000000000000000 ) ;
#32377 = CARTESIAN_POINT ( 'NONE',  ( -9.999999999999998224, 1.224646799147353059E-15, -157.2500000000000000 ) ) ;
#32378 = CARTESIAN_POINT ( 'NONE',  ( 7.070501591499377789E-16, 11.54700538379251284, -18.50000000409676559 ) ) ;
#32379 = AXIS2_PLACEMENT_3D ( 'NONE', #7766, #1073, #16806 ) ;
#32380 = CARTESIAN_POINT ( 'NONE',  ( -9.999999999999998224, 5.773502691896259087, -194.8750000000000000 ) ) ;
#32382 = ORIENTED_EDGE ( 'NONE', *, *, #8003, .F. ) ;
#32381 = CARTESIAN_POINT ( 'NONE',  ( -2.293366432827344421E-15, -12.48450537969573659, -129.4062500020483810 ) ) ;
#32383 = CARTESIAN_POINT ( 'NONE',  ( 9.999999999999998224, 0.000000000000000000, -12.49999999999995559 ) ) ;
#32384 = ORIENTED_EDGE ( 'NONE', *, *, #24919, .F. ) ;
#32385 = CARTESIAN_POINT ( 'NONE',  ( -5.405949406250003975, -9.363379034771801557, -57.53125000204836681 ) ) ;
#32386 = PERSON_AND_ORGANIZATION_ROLE ( 'creator' ) ;
#32387 = EDGE_CURVE ( 'NONE', #3006, #6776, #22774, .T. ) ;
#32388 = CARTESIAN_POINT ( 'NONE',  ( -10.81189881249999729, 1.324075727343319199E-15, -102.5937500020483810 ) ) ;
#32390 = VERTEX_POINT ( 'NONE', #29678 ) ;
#32389 = EDGE_LOOP ( 'NONE', ( #10667, #20780, #28382, #11055 ) ) ;
#32391 = CARTESIAN_POINT ( 'NONE',  ( 9.999999999999998224, 0.000000000000000000, -49.99999999999998579 ) ) ;
#32392 = CARTESIAN_POINT ( 'NONE',  ( 5.000000000000000000, 8.660254037844385522, -33.24999999999997158 ) ) ;
#32393 = CARTESIAN_POINT ( 'NONE',  ( -2.293366432827344421E-15, -12.48450537969573659, -181.9062500020483810 ) ) ;
#32394 = CARTESIAN_POINT ( 'NONE',  ( 9.999999999999998224, 1.224646799147353059E-15, -99.99999999999998579 ) ) ;
#32395 = CARTESIAN_POINT ( 'NONE',  ( -23.09401076758503280, 0.000000000000000000, 0.000000000000000000 ) ) ;
#32396 = VECTOR ( 'NONE', #27751, 1000.000000000000114 ) ;
#32397 = CARTESIAN_POINT ( 'NONE',  ( 7.644554776091147741E-16, 12.48450537969573659, -140.4687500020483810 ) ) ;
#32398 = CARTESIAN_POINT ( 'NONE',  ( -10.81189881249999907, -6.242252689847864744, -97.96875000204838102 ) ) ;
#32399 = FACE_OUTER_BOUND ( 'NONE', #24937, .T. ) ;
#32400 = CARTESIAN_POINT ( 'NONE',  ( -10.81189881249999729, 6.242252689847871849, -107.4062500020483810 ) ) ;
#32401 = CARTESIAN_POINT ( 'NONE',  ( 10.00000000000000000, 5.773502691896255534, -191.2500000040968189 ) ) ;
#32403 = EDGE_CURVE ( 'NONE', #2293, #10098, #10017, .T. ) ;
#32402 = CARTESIAN_POINT ( 'NONE',  ( -5.405949406250003975, -9.363379034771801557, -126.3437500020483952 ) ) ;
#32404 = CARTESIAN_POINT ( 'NONE',  ( 10.81189881249999729, 6.242252689847867408, -188.9062500020484094 ) ) ;
#32405 = DIRECTION ( 'NONE',  ( -0.000000000000000000, -0.000000000000000000, 1.000000000000000000 ) ) ;
#32406 = CARTESIAN_POINT ( 'NONE',  ( 9.999999999999996447, -5.773502691896262640, -137.1250000000000000 ) ) ;
#32407 = CARTESIAN_POINT ( 'NONE',  ( 4.999999999999992006, -8.660254037844389075, -0.7499999999999729106 ) ) ;
#32408 = CARTESIAN_POINT ( 'NONE',  ( -2.293366432827344421E-15, -12.48450537969573659, -67.71875000204838102 ) ) ;
#32409 = CARTESIAN_POINT ( 'NONE',  ( 10.81189881249999551, -6.242252689847874514, -46.46875000204837391 ) ) ;
#32410 = CARTESIAN_POINT ( 'NONE',  ( -9.999999999999998224, 5.773502691896259087, -177.2500000040967905 ) ) ;
#32411 = CARTESIAN_POINT ( 'NONE',  ( -10.81189881249999907, -6.242252689847864744, -27.65625000204838457 ) ) ;
#32412 = CARTESIAN_POINT ( 'NONE',  ( 7.644554776091147741E-16, 12.48450537969573659, -32.46875000204835260 ) ) ;
#32413 = CARTESIAN_POINT ( 'NONE',  ( 9.999999999999998224, 0.000000000000000000, -109.9999999999999858 ) ) ;
#32414 = CARTESIAN_POINT ( 'NONE',  ( 7.644554776091147741E-16, 12.48450537969573659, -138.9687500020484094 ) ) ;
#32415 = CARTESIAN_POINT ( 'NONE',  ( -5.000000000000003553, -8.660254037844383745, -110.4999999999999858 ) ) ;
#32416 = CARTESIAN_POINT ( 'NONE',  ( -10.00000000000051337, 5.773502691895962435, -118.7500000040967763 ) ) ;
#32417 = CARTESIAN_POINT ( 'NONE',  ( -10.00000000000000000, -5.773502691896251982, -67.12499999999998579 ) ) ;
#32418 = CARTESIAN_POINT ( 'NONE',  ( -5.405949406249996869, 9.363379034771805109, -142.0312500020483810 ) ) ;
#32419 = CARTESIAN_POINT ( 'NONE',  ( 7.644554776091147741E-16, 12.48450537969573659, -112.1562500020483952 ) ) ;
#32420 = ORIENTED_EDGE ( 'NONE', *, *, #29617, .F. ) ;
#32421 = CARTESIAN_POINT ( 'NONE',  ( 9.999999999999998224, 0.000000000000000000, -120.8750000040967905 ) ) ;
#32422 = CARTESIAN_POINT ( 'NONE',  ( 10.00000000000000000, 5.773502691896255534, -116.2500000040967905 ) ) ;
#32423 = CARTESIAN_POINT ( 'NONE',  ( -5.405949406250003975, -9.363379034771801557, -72.34375000204836681 ) ) ;
#32424 = CARTESIAN_POINT ( 'NONE',  ( 9.999999999999996447, -5.773502691896262640, -42.62499999999997868 ) ) ;
#32425 = CARTESIAN_POINT ( 'NONE',  ( -10.00000000000000000, -5.773502691896251982, -25.50000000409676915 ) ) ;
#32426 = CARTESIAN_POINT ( 'NONE',  ( 10.81189881249999729, 0.000000000000000000, -42.03125000204838102 ) ) ;
#32427 =( BOUNDED_CURVE ( )  B_SPLINE_CURVE ( 2, ( #14431, #40764, #40336, #11206, #20285, #20923, #23967 ),
 .UNSPECIFIED., .F., .F. ) 
 B_SPLINE_CURVE_WITH_KNOTS ( ( 3, 2, 2, 3 ),
 ( 0.4850746268656717652, 0.4863184079601990950, 0.4875621890547264248, 0.4888059701492538101 ),
 .UNSPECIFIED. ) 
 CURVE ( )  GEOMETRIC_REPRESENTATION_ITEM ( )  RATIONAL_B_SPLINE_CURVE ( ( 0.9999999999999880096, 0.8660254037844506980, 1.000000000000000000, 0.8660254037844387076, 1.000000000000000000, 0.8660254037844327124, 1.000000000000005995 ) ) 
 REPRESENTATION_ITEM ( '' )  );
#32428 = DIRECTION ( 'NONE',  ( 1.000000000000000000, 0.000000000000000000, 0.000000000000000000 ) ) ;
#32429 = CARTESIAN_POINT ( 'NONE',  ( 9.999999999999996447, -5.773502691896262640, -44.50000000409676915 ) ) ;
#32430 = CARTESIAN_POINT ( 'NONE',  ( 10.81189881249999907, 6.242252689847868297, -32.90625000204835970 ) ) ;
#32431 = CARTESIAN_POINT ( 'NONE',  ( 9.999999999999998224, 0.000000000000000000, -167.0000000000000000 ) ) ;
#32432 = CARTESIAN_POINT ( 'NONE',  ( 10.81189881249999907, 6.242252689847868297, -133.4062500020483810 ) ) ;
#32433 = VECTOR ( 'NONE', #38792, 1000.000000000000000 ) ;
#32434 = CARTESIAN_POINT ( 'NONE',  ( -10.81189881249999729, 6.242252689847871849, -147.9062500020483810 ) ) ;
#32435 = CARTESIAN_POINT ( 'NONE',  ( 9.999999999998969713, 5.773502691896851502, -51.37499999999997158 ) ) ;
#32436 = VERTEX_POINT ( 'NONE', #3770 ) ;
#32437 = EDGE_CURVE ( 'NONE', #1269, #30921, #23001, .T. ) ;
#32438 = ORIENTED_EDGE ( 'NONE', *, *, #2732, .T. ) ;
#32439 = ORIENTED_EDGE ( 'NONE', *, *, #9016, .F. ) ;
#32440 = CARTESIAN_POINT ( 'NONE',  ( 0.000000000000000000, 0.000000000000000000, -200.0000000000000000 ) ) ;
#32441 = CARTESIAN_POINT ( 'NONE',  ( 5.405949406249992428, -9.363379034771808662, -177.0937500020484094 ) ) ;
#32442 = CARTESIAN_POINT ( 'NONE',  ( -10.81189881249999729, 6.242252689847871849, -33.71875000204835260 ) ) ;
#32443 = CARTESIAN_POINT ( 'NONE',  ( 7.070501591499376803E-16, 11.54700538379251284, -111.5000000040967763 ) ) ;
#32444 = CARTESIAN_POINT ( 'NONE',  ( 10.81189881249999729, 6.242252689847867408, -161.7187500020483810 ) ) ;
#32445 = CARTESIAN_POINT ( 'NONE',  ( 10.81189881249999551, -6.242252689847874514, -146.9687500020484094 ) ) ;
#32446 = EDGE_CURVE ( 'NONE', #14499, #10098, #42017, .T. ) ;
#32447 = CARTESIAN_POINT ( 'NONE',  ( 10.70731569305672615, 1.500182182589836044, 0.000000000000000000 ) ) ;
#32448 = CARTESIAN_POINT ( 'NONE',  ( -5.405949406249996869, 9.363379034771805109, -128.3437500020484094 ) ) ;
#32449 = CARTESIAN_POINT ( 'NONE',  ( 10.81189881249999551, -6.242252689847874514, -135.1562500020484094 ) ) ;
#32450 = CARTESIAN_POINT ( 'NONE',  ( 10.81189881249999907, 6.242252689847868297, -16.21875000204836326 ) ) ;
#32451 = CARTESIAN_POINT ( 'NONE',  ( 5.405949406249992428, -9.363379034771808662, -147.0937500020483810 ) ) ;
#32452 = CARTESIAN_POINT ( 'NONE',  ( 0.000000000000000000, 0.000000000000000000, -200.0000000000000000 ) ) ;
#32453 = CARTESIAN_POINT ( 'NONE',  ( -4.999999999999996447, 8.660254037844387298, -141.3750000040967905 ) ) ;
#32454 = CARTESIAN_POINT ( 'NONE',  ( -10.00000000000000000, -5.773502691896251982, -164.6249999999999716 ) ) ;
#32455 = FACE_OUTER_BOUND ( 'NONE', #18670, .T. ) ;
#32456 = CARTESIAN_POINT ( 'NONE',  ( 7.644554776091147741E-16, 12.48450537969573659, -72.96875000204835260 ) ) ;
#32457 = CARTESIAN_POINT ( 'NONE',  ( 10.81189881249999551, -6.242252689847874514, -52.65625000204837391 ) ) ;
#32458 = CARTESIAN_POINT ( 'NONE',  ( -10.81189881249999729, 6.242252689847871849, -63.71875000204838102 ) ) ;
#32459 = LINE ( 'NONE', #38919, #18541 ) ;
#32460 = CARTESIAN_POINT ( 'NONE',  ( -5.405949406249996869, 9.363379034771805109, -161.3437500020484094 ) ) ;
#32461 = VECTOR ( 'NONE', #33108, 1000.000000000000000 ) ;
#32462 = CARTESIAN_POINT ( 'NONE',  ( 5.000000000000000000, 8.660254037844385522, -133.7499999999999716 ) ) ;
#32463 = CARTESIAN_POINT ( 'NONE',  ( -10.81189881249999729, 6.242252689847871849, -147.9062500020484094 ) ) ;
#32464 = LINE ( 'NONE', #26610, #4112 ) ;
#32465 = CARTESIAN_POINT ( 'NONE',  ( -10.00000000000000000, -5.773502691896251982, -120.0000000040967905 ) ) ;
#32466 = CARTESIAN_POINT ( 'NONE',  ( -5.000000000000003553, -8.660254037844383745, -93.99999999999998579 ) ) ;
#32467 =( BOUNDED_CURVE ( )  B_SPLINE_CURVE ( 2, ( #347, #13469, #26661, #20178, #3788, #36579, #32930 ),
 .UNSPECIFIED., .F., .F. ) 
 B_SPLINE_CURVE_WITH_KNOTS ( ( 3, 2, 2, 3 ),
 ( 0.3694029850746270438, 0.3706467661691543181, 0.3718905472636817033, 0.3731343283582090331 ),
 .UNSPECIFIED. ) 
 CURVE ( )  GEOMETRIC_REPRESENTATION_ITEM ( )  RATIONAL_B_SPLINE_CURVE ( ( 0.9999999999999820144, 0.8660254037844566932, 1.000000000000000000, 0.8660254037844387076, 1.000000000000000000, 0.8660254037844327124, 1.000000000000005995 ) ) 
 REPRESENTATION_ITEM ( '' )  );
#32468 = VERTEX_POINT ( 'NONE', #30955 ) ;
#32469 = CARTESIAN_POINT ( 'NONE',  ( -5.405949406250003975, -9.363379034771801557, -119.0312500020483952 ) ) ;
#32470 = CARTESIAN_POINT ( 'NONE',  ( -10.00000000000000000, -5.773502691896251982, -141.0000000040967905 ) ) ;
#32471 = CARTESIAN_POINT ( 'NONE',  ( -10.00000000000154188, 5.773502691895366468, -52.37499999999992895 ) ) ;
#32472 = CARTESIAN_POINT ( 'NONE',  ( -10.81189881249999907, -6.242252689847864744, -174.6562500020483810 ) ) ;
#32473 = CARTESIAN_POINT ( 'NONE',  ( -10.00000000000000000, -5.773502691896251982, -48.00000000409676204 ) ) ;
#32474 = CARTESIAN_POINT ( 'NONE',  ( 9.999999999999998224, 0.000000000000000000, -97.99999999999998579 ) ) ;
#32475 = CARTESIAN_POINT ( 'NONE',  ( 10.81189881249999729, 0.000000000000000000, -58.53125000204836681 ) ) ;
#32476 = LINE ( 'NONE', #16668, #30395 ) ;
#32477 = CARTESIAN_POINT ( 'NONE',  ( -5.405949406250003975, -9.363379034771801557, -158.0312500020484094 ) ) ;
#32478 = CARTESIAN_POINT ( 'NONE',  ( 5.405949406249999534, 9.363379034771803333, -143.5937500020483810 ) ) ;
#32479 = DIRECTION ( 'NONE',  ( 1.000000000000000000, -0.000000000000000000, -0.000000000000000000 ) ) ;
#32480 = CARTESIAN_POINT ( 'NONE',  ( -4.999999999999996447, 8.660254037844387298, -79.87500000409677625 ) ) ;
#32481 = VERTEX_POINT ( 'NONE', #40214 ) ;
#32482 = CARTESIAN_POINT ( 'NONE',  ( 0.000000000000000000, 0.000000000000000000, -200.0000000000000000 ) ) ;
#32484 = VERTEX_POINT ( 'NONE', #21224 ) ;
#32483 = CARTESIAN_POINT ( 'NONE',  ( 7.644554776091147741E-16, 12.48450537969573659, -67.15625000204838102 ) ) ;
#32485 = PERSON_AND_ORGANIZATION_ROLE ( 'design_supplier' ) ;
#32487 = VERTEX_POINT ( 'NONE', #17761 ) ;
#32486 = CARTESIAN_POINT ( 'NONE',  ( -2.121150477449813534E-15, -11.54700538379251284, -188.7500000040967905 ) ) ;
#32488 = ORIENTED_EDGE ( 'NONE', *, *, #2344, .T. ) ;
#32489 = CARTESIAN_POINT ( 'NONE',  ( -5.405949406249996869, 9.363379034771805109, -29.34375000204836326 ) ) ;
#32490 = DIRECTION ( 'NONE',  ( 0.000000000000000000, 1.000000000000000000, 0.000000000000000000 ) ) ;
#32491 = CARTESIAN_POINT ( 'NONE',  ( 7.644554776091147741E-16, 12.48450537969573659, -194.4687500020484094 ) ) ;
#32492 = CARTESIAN_POINT ( 'NONE',  ( 5.405949406249999534, 9.363379034771803333, -52.09375000204835260 ) ) ;
#32493 = CARTESIAN_POINT ( 'NONE',  ( -9.999999999999479527, -5.773502691896549521, -72.00000000409676204 ) ) ;
#32494 = CARTESIAN_POINT ( 'NONE',  ( 4.999999999999992006, -8.660254037844389075, -27.74999999999996803 ) ) ;
#32495 = CARTESIAN_POINT ( 'NONE',  ( 5.405949406249992428, -9.363379034771808662, -192.0937500020484094 ) ) ;
#32496 = CARTESIAN_POINT ( 'NONE',  ( -2.293366432827344421E-15, -12.48450537969573659, -168.2187500020483810 ) ) ;
#32497 = CARTESIAN_POINT ( 'NONE',  ( 10.81189881249999551, -6.242252689847874514, -154.4687500020484094 ) ) ;
#32498 = CARTESIAN_POINT ( 'NONE',  ( -5.405949406250003975, -9.363379034771801557, -174.3437500020484094 ) ) ;
#32499 = CARTESIAN_POINT ( 'NONE',  ( -7.959047257566134870E-15, -139.9999999999999716, 2.499999999999992006 ) ) ;
#32500 = CARTESIAN_POINT ( 'NONE',  ( 9.999999999999996447, -5.773502691896262640, -189.6250000000000000 ) ) ;
#32501 = CARTESIAN_POINT ( 'NONE',  ( -10.81189881249999729, 1.324075727343319199E-15, -107.0937500020483810 ) ) ;
#32502 = CARTESIAN_POINT ( 'NONE',  ( 7.070501591499376803E-16, 11.54700538379251284, -196.6250000000000284 ) ) ;
#32503 = CARTESIAN_POINT ( 'NONE',  ( -5.405949406250003975, -9.363379034771801557, -77.03125000204838102 ) ) ;
#32504 = LINE ( 'NONE', #29051, #24036 ) ;
#32505 = ADVANCED_FACE ( 'NONE', ( #20793 ), #18510, .T. ) ;
#32506 = CARTESIAN_POINT ( 'NONE',  ( 5.405949406249999534, 9.363379034771803333, -85.09375000204836681 ) ) ;
#32507 = ADVANCED_FACE ( 'NONE', ( #34200 ), #754, .T. ) ;
#32508 = CARTESIAN_POINT ( 'NONE',  ( 5.405949406249992428, -9.363379034771808662, -57.28125000204836681 ) ) ;
#32509 = CARTESIAN_POINT ( 'NONE',  ( 10.00000000000000000, 5.773502691896255534, -149.2500000040968189 ) ) ;
#32510 = CARTESIAN_POINT ( 'NONE',  ( 10.00000000000000000, 5.773502691896255534, -114.3750000000000000 ) ) ;
#32511 = ORIENTED_EDGE ( 'NONE', *, *, #6065, .F. ) ;
#32512 = CARTESIAN_POINT ( 'NONE',  ( 10.81189881249999551, -6.242252689847874514, -144.1562500020484094 ) ) ;
#32513 = CARTESIAN_POINT ( 'NONE',  ( 7.644554776091147741E-16, 12.48450537969573659, -155.6562500020484094 ) ) ;
#32514 = LOCAL_TIME ( 11, 57, 6.000000000000000000, #6887 ) ;
#32515 = CARTESIAN_POINT ( 'NONE',  ( -10.81189881249999729, 1.324075727343319199E-15, -197.2812500020484094 ) ) ;
#32516 = CARTESIAN_POINT ( 'NONE',  ( -5.000000000000003553, -8.660254037844383745, -179.5000000000000000 ) ) ;
#32517 = CARTESIAN_POINT ( 'NONE',  ( 5.405949406249999534, 9.363379034771803333, -89.59375000204838102 ) ) ;
#32518 = ORIENTED_EDGE ( 'NONE', *, *, #13460, .F. ) ;
#32519 = CARTESIAN_POINT ( 'NONE',  ( 5.000000000000000000, 8.660254037844385522, -55.74999999999996447 ) ) ;
#32520 = CARTESIAN_POINT ( 'NONE',  ( 10.81189881249999551, -6.242252689847874514, -191.9687500020484379 ) ) ;
#32521 = CARTESIAN_POINT ( 'NONE',  ( 5.000000000000000000, 8.660254037844385522, -72.62500000409677625 ) ) ;
#32522 = CARTESIAN_POINT ( 'NONE',  ( 0.000000000000000000, -5.321294541346989426, -219.9999999999999716 ) ) ;
#32523 = CARTESIAN_POINT ( 'NONE',  ( 9.999999999999998224, 0.000000000000000000, -159.8750000040967905 ) ) ;
#32524 = CARTESIAN_POINT ( 'NONE',  ( 5.405949406249992428, -9.363379034771808662, -82.78125000204838102 ) ) ;
#32525 = CARTESIAN_POINT ( 'NONE',  ( 5.405949406249992428, -9.363379034771808662, -66.28125000204838102 ) ) ;
#32526 = CARTESIAN_POINT ( 'NONE',  ( 7.070501591499377789E-16, 11.54700538379251284, -60.50000000409677625 ) ) ;
#32527 = CARTESIAN_POINT ( 'NONE',  ( 10.81189881249999907, 6.242252689847868297, -16.21875000204836326 ) ) ;
#32528 = LINE ( 'NONE', #2957, #21413 ) ;
#32529 = CARTESIAN_POINT ( 'NONE',  ( 10.81189881249999729, 0.000000000000000000, -192.0312500020484094 ) ) ;
#32530 = AXIS2_PLACEMENT_3D ( 'NONE', #23990, #14019, #1326 ) ;
#32531 = CARTESIAN_POINT ( 'NONE',  ( 5.405949406249999534, 9.363379034771803333, -11.78125000204835438 ) ) ;
#32532 = CARTESIAN_POINT ( 'NONE',  ( 5.405949406249992428, -9.363379034771808662, -0.09375000204836503315 ) ) ;
#32533 = DIRECTION ( 'NONE',  ( -0.000000000000000000, -0.000000000000000000, 1.000000000000000000 ) ) ;
#32534 = CARTESIAN_POINT ( 'NONE',  ( -9.439719357620422358, -3.412429525893140525, -0.000000000000000000 ) ) ;
#32535 = CARTESIAN_POINT ( 'NONE',  ( 5.000000000000000000, 8.660254037844385522, -159.6250000040967905 ) ) ;
#32536 = CARTESIAN_POINT ( 'NONE',  ( -2.121150477449813534E-15, -11.54700538379251284, -176.3750000000000000 ) ) ;
#32537 = CARTESIAN_POINT ( 'NONE',  ( 10.00000000000000000, 5.773502691896255534, -166.8750000000000000 ) ) ;
#32539 = VERTEX_POINT ( 'NONE', #1387 ) ;
#32538 = CARTESIAN_POINT ( 'NONE',  ( 5.405949406249999534, 9.363379034771803333, -94.28125000204838102 ) ) ;
#32540 = CARTESIAN_POINT ( 'NONE',  ( 4.999999999999992006, -8.660254037844389075, -161.6250000040967905 ) ) ;
#32541 = VERTEX_POINT ( 'NONE', #34622 ) ;
#32542 = ORIENTED_EDGE ( 'NONE', *, *, #27596, .T. ) ;
#32543 = CARTESIAN_POINT ( 'NONE',  ( 10.81189881249999551, -6.242252689847874514, -34.46875000204835260 ) ) ;
#32544 = CARTESIAN_POINT ( 'NONE',  ( -5.405949406250003975, -9.363379034771801557, -30.53125000204837036 ) ) ;
#32545 = DATE_TIME_ROLE ( 'classification_date' ) ;
#32546 = CARTESIAN_POINT ( 'NONE',  ( 7.644554776091147741E-16, 12.48450537969573659, -75.96875000204838102 ) ) ;
#32547 = CARTESIAN_POINT ( 'NONE',  ( 0.000000000000000000, 0.000000000000000000, -180.0000000000000000 ) ) ;
#32548 = CARTESIAN_POINT ( 'NONE',  ( -10.81189881249999729, 1.324075727343319199E-15, -191.0937500020484094 ) ) ;
#32549 =( BOUNDED_CURVE ( )  B_SPLINE_CURVE ( 2, ( #42157, #41946, #11960, #24946, #34650, #21684, #25150 ),
 .UNSPECIFIED., .F., .F. ) 
 B_SPLINE_CURVE_WITH_KNOTS ( ( 3, 2, 2, 3 ),
 ( 0.2500000000000001110, 0.2512437810945274963, 0.2524875621890548261, 0.2537313432835822113 ),
 .UNSPECIFIED. ) 
 CURVE ( )  GEOMETRIC_REPRESENTATION_ITEM ( )  RATIONAL_B_SPLINE_CURVE ( ( 0.9999999999999880096, 0.8660254037844506980, 1.000000000000000000, 0.8660254037844387076, 1.000000000000000000, 0.8660254037844267172, 1.000000000000011990 ) ) 
 REPRESENTATION_ITEM ( '' )  );
#32550 = CARTESIAN_POINT ( 'NONE',  ( 9.999999999999998224, 0.000000000000000000, -159.8750000040967905 ) ) ;
#32551 = DIRECTION ( 'NONE',  ( -0.000000000000000000, -0.000000000000000000, 1.000000000000000000 ) ) ;
#32552 = CARTESIAN_POINT ( 'NONE',  ( -5.405949406250003975, -9.363379034771801557, -155.0312500020484094 ) ) ;
#32553 = CARTESIAN_POINT ( 'NONE',  ( 5.000000000000000000, 8.660254037844385522, -11.12500000409674605 ) ) ;
#32554 = AXIS2_PLACEMENT_3D ( 'NONE', #14114, #18007, #7676 ) ;
#32555 = CARTESIAN_POINT ( 'NONE',  ( 9.999999999999998224, 0.000000000000000000, -50.37500000409675494 ) ) ;
#32556 = CARTESIAN_POINT ( 'NONE',  ( 10.81189881249999729, 0.000000000000000000, -130.3437500020484094 ) ) ;
#32557 = CARTESIAN_POINT ( 'NONE',  ( 10.81189881249999729, 0.000000000000000000, -102.0312500020483952 ) ) ;
#32558 = EDGE_CURVE ( 'NONE', #12272, #25832, #27415, .T. ) ;
#32559 = CARTESIAN_POINT ( 'NONE',  ( 5.405949406249992428, -9.363379034771808662, -108.0937500020483810 ) ) ;
#32560 = CARTESIAN_POINT ( 'NONE',  ( -5.405949406249996869, 9.363379034771805109, -78.84375000204838102 ) ) ;
#32561 = CARTESIAN_POINT ( 'NONE',  ( -10.81189881249999729, 1.324075727343319199E-15, -84.78125000204838102 ) ) ;
#32562 = CARTESIAN_POINT ( 'NONE',  ( 7.070501591499377789E-16, 11.54700538379251284, -171.5000000040967905 ) ) ;
#32563 = EDGE_CURVE ( 'NONE', #1542, #3313, #6729, .T. ) ;
#32564 = CARTESIAN_POINT ( 'NONE',  ( 4.999999999999992006, -8.660254037844389075, -133.1250000040967620 ) ) ;
#32565 = CARTESIAN_POINT ( 'NONE',  ( 10.81189881249999729, 0.000000000000000000, -165.0312500020484094 ) ) ;
#32566 = CARTESIAN_POINT ( 'NONE',  ( -10.81189881249999729, 6.242252689847871849, -177.9062500020484094 ) ) ;
#32567 = EDGE_CURVE ( 'NONE', #15830, #29288, #8127, .T. ) ;
#32568 = CARTESIAN_POINT ( 'NONE',  ( -9.999999999999998224, 5.773502691896259087, -156.2500000040967905 ) ) ;
#32569 = CARTESIAN_POINT ( 'NONE',  ( -9.999999999999998224, 1.224646799147353059E-15, -4.249999999999976019 ) ) ;
#32570 = CARTESIAN_POINT ( 'NONE',  ( -10.81189881249999907, -6.242252689847864744, -7.968750002048358816 ) ) ;
#32571 = CARTESIAN_POINT ( 'NONE',  ( -9.999999999999998224, 1.224646799147353059E-15, -172.2500000000000000 ) ) ;
#32572 = CARTESIAN_POINT ( 'NONE',  ( 10.81189881249999729, 0.000000000000000000, -116.8437500020483810 ) ) ;
#32573 = CARTESIAN_POINT ( 'NONE',  ( 4.999999999999992006, -8.660254037844389075, -89.24999999999998579 ) ) ;
#32574 = CARTESIAN_POINT ( 'NONE',  ( -5.405949406249996869, 9.363379034771805109, -14.53125000204835615 ) ) ;
#32575 = CARTESIAN_POINT ( 'NONE',  ( 5.000000000000000000, 8.660254037844385522, -101.1250000040967905 ) ) ;
#32576 = DIRECTION ( 'NONE',  ( 1.000000000000000000, 0.000000000000000000, 0.000000000000000000 ) ) ;
#32577 = CC_DESIGN_PERSON_AND_ORGANIZATION_ASSIGNMENT ( #6259, #19406, ( #27668 ) ) ;
#32578 = CARTESIAN_POINT ( 'NONE',  ( -5.405949406249996869, 9.363379034771805109, -106.0312500020483810 ) ) ;
#32579 = CARTESIAN_POINT ( 'NONE',  ( -10.81189881249999729, 1.324075727343319199E-15, -89.28125000204838102 ) ) ;
#32580 = ORIENTED_EDGE ( 'NONE', *, *, #21185, .F. ) ;
#32581 = AXIS2_PLACEMENT_3D ( 'NONE', #14184, #17433, #37519 ) ;
#32582 = CARTESIAN_POINT ( 'NONE',  ( -10.00000000000000000, -5.773502691896251982, -85.50000000409677625 ) ) ;
#32583 = CARTESIAN_POINT ( 'NONE',  ( 45.00000000000000711, 5.510910596163090344E-15, -200.0000000000000000 ) ) ;
#32584 = CARTESIAN_POINT ( 'NONE',  ( -10.81189881249999729, 1.324075727343319199E-15, -45.59375000204838102 ) ) ;
#32585 = ORIENTED_EDGE ( 'NONE', *, *, #9473, .T. ) ;
#32586 = CARTESIAN_POINT ( 'NONE',  ( -2.121150477449813534E-15, -11.54700538379251284, -15.87499999999998046 ) ) ;
#32587 = CARTESIAN_POINT ( 'NONE',  ( -9.999999999999998224, 5.773502691896259087, -152.8749999999999716 ) ) ;
#32588 = CARTESIAN_POINT ( 'NONE',  ( 5.000000000000000000, 8.660254037844385522, -15.62500000409675138 ) ) ;
#32589 = VECTOR ( 'NONE', #18761, 1000.000000000000000 ) ;
#32590 = CARTESIAN_POINT ( 'NONE',  ( 9.999999999999998224, 0.000000000000000000, -200.0000000000000000 ) ) ;
#32592 = ORIENTED_EDGE ( 'NONE', *, *, #5401, .T. ) ;
#32591 = CARTESIAN_POINT ( 'NONE',  ( -10.81189881249999729, 6.242252689847871849, -125.4062500020483810 ) ) ;
#32593 = CARTESIAN_POINT ( 'NONE',  ( -4.999999999999996447, 8.660254037844387298, -89.99999999999998579 ) ) ;
#32594 = ORIENTED_EDGE ( 'NONE', *, *, #20835, .F. ) ;
#32595 =( BOUNDED_CURVE ( )  B_SPLINE_CURVE ( 2, ( #30217, #4301, #14192, #30636, #10759, #17652, #29999 ),
 .UNSPECIFIED., .F., .F. ) 
 B_SPLINE_CURVE_WITH_KNOTS ( ( 3, 2, 2, 3 ),
 ( 0.4253731343283583266, 0.4266169154228856564, 0.4278606965174130417, 0.4291044776119404269 ),
 .UNSPECIFIED. ) 
 CURVE ( )  GEOMETRIC_REPRESENTATION_ITEM ( )  RATIONAL_B_SPLINE_CURVE ( ( 0.9999999999999880096, 0.8660254037844506980, 1.000000000000000000, 0.8660254037844387076, 1.000000000000000000, 0.8660254037844267172, 1.000000000000011990 ) ) 
 REPRESENTATION_ITEM ( '' )  );
#32596 = CARTESIAN_POINT ( 'NONE',  ( 5.405949406249999534, 9.363379034771803333, -53.78125000204836681 ) ) ;
#32597 = COORDINATED_UNIVERSAL_TIME_OFFSET ( 6, 0, .AHEAD. ) ;
#32598 = CARTESIAN_POINT ( 'NONE',  ( -5.405949406250003975, -9.363379034771801557, -105.3437500020483810 ) ) ;
#32600 = ORIENTED_EDGE ( 'NONE', *, *, #6144, .T. ) ;
#32599 = VERTEX_POINT ( 'NONE', #27926 ) ;
#32601 = CARTESIAN_POINT ( 'NONE',  ( 0.000000000000000000, 0.000000000000000000, -200.0000000000000000 ) ) ;
#32602 = CARTESIAN_POINT ( 'NONE',  ( -2.121150477449813534E-15, -11.54700538379251284, -125.7500000040967763 ) ) ;
#32603 =( BOUNDED_CURVE ( )  B_SPLINE_CURVE ( 2, ( #417, #16774, #26309, #10100, #6659, #13537, #29542 ),
 .UNSPECIFIED., .F., .F. ) 
 B_SPLINE_CURVE_WITH_KNOTS ( ( 3, 2, 2, 3 ),
 ( 0.7537313432835822669, 0.7549751243781096521, 0.7562189054726369264, 0.7574626865671643117 ),
 .UNSPECIFIED. ) 
 CURVE ( )  GEOMETRIC_REPRESENTATION_ITEM ( )  RATIONAL_B_SPLINE_CURVE ( ( 0.9999999999999761302, 0.8660254037844625774, 1.000000000000000000, 0.8660254037844387076, 1.000000000000000000, 0.8660254037844267172, 1.000000000000011990 ) ) 
 REPRESENTATION_ITEM ( '' )  );
#32604 = CARTESIAN_POINT ( 'NONE',  ( -5.405949406250003975, -9.363379034771801557, -177.5312500020483810 ) ) ;
#32605 = CARTESIAN_POINT ( 'NONE',  ( 10.81189881249999729, 0.000000000000000000, -2.843750002048367698 ) ) ;
#32606 = CARTESIAN_POINT ( 'NONE',  ( 9.999999999999998224, 0.000000000000000000, -155.3750000040967905 ) ) ;
#32607 = CARTESIAN_POINT ( 'NONE',  ( -2.293366432827344421E-15, -12.48450537969573659, -132.2187500020483810 ) ) ;
#32608 = CARTESIAN_POINT ( 'NONE',  ( -10.81189881249999907, -6.242252689847864744, -105.4687500020483668 ) ) ;
#32609 = CARTESIAN_POINT ( 'NONE',  ( -9.999999999999998224, 1.224646799147353059E-15, -148.2500000000000000 ) ) ;
#32610 = CARTESIAN_POINT ( 'NONE',  ( 10.81189881249999551, -6.242252689847874514, -111.1562500020483952 ) ) ;
#32611 = CARTESIAN_POINT ( 'NONE',  ( -4.999999999999996447, 8.660254037844387298, -193.8750000040967905 ) ) ;
#32612 = CARTESIAN_POINT ( 'NONE',  ( -2.293366432827344421E-15, -12.48450537969573659, -114.2187500020483668 ) ) ;
#32613 = CARTESIAN_POINT ( 'NONE',  ( 10.81189881249999551, -6.242252689847874514, -184.6562500020484094 ) ) ;
#32614 = CARTESIAN_POINT ( 'NONE',  ( -4.999999999999996447, 8.660254037844387298, -148.8750000040967905 ) ) ;
#32615 = CARTESIAN_POINT ( 'NONE',  ( -4.999999999999996447, 8.660254037844387298, -136.5000000000000000 ) ) ;
#32616 = CARTESIAN_POINT ( 'NONE',  ( 9.999999999999996447, -5.773502691896262640, -8.124999999999966249 ) ) ;
#32617 = CARTESIAN_POINT ( 'NONE',  ( -5.405949406249996869, 9.363379034771805109, -65.34375000204836681 ) ) ;
#32618 = CARTESIAN_POINT ( 'NONE',  ( -10.81189881249999907, -6.242252689847864744, -49.96875000204835970 ) ) ;
#32619 = CARTESIAN_POINT ( 'NONE',  ( -9.999999999999998224, 5.773502691896259087, -183.2500000040968189 ) ) ;
#32620 = CARTESIAN_POINT ( 'NONE',  ( -5.405949406249996869, 9.363379034771805109, -16.03125000204835970 ) ) ;
#32621 = CARTESIAN_POINT ( 'NONE',  ( -5.405949406249996869, 9.363379034771805109, -29.34375000204836326 ) ) ;
#32622 = CARTESIAN_POINT ( 'NONE',  ( -2.121150477449813534E-15, -11.54700538379251284, -142.2500000040967905 ) ) ;
#32623 = CARTESIAN_POINT ( 'NONE',  ( 10.81189881249999729, 0.000000000000000000, -139.3437500020484094 ) ) ;
#32624 = CARTESIAN_POINT ( 'NONE',  ( -5.000000000000003553, -8.660254037844383745, -113.4999999999999858 ) ) ;
#32625 = CARTESIAN_POINT ( 'NONE',  ( -9.999999999999998224, 1.224646799147353059E-15, -110.7499999999999858 ) ) ;
#32626 = CARTESIAN_POINT ( 'NONE',  ( -5.000000000000003553, -8.660254037844383745, -66.99999999999997158 ) ) ;
#32627 = CARTESIAN_POINT ( 'NONE',  ( 7.644554776091147741E-16, 12.48450537969573659, -133.1562500020483810 ) ) ;
#32628 = CARTESIAN_POINT ( 'NONE',  ( 10.81189881249999729, 0.000000000000000000, -118.5312500020483952 ) ) ;
#32629 = ORIENTED_EDGE ( 'NONE', *, *, #8437, .F. ) ;
#32630 = FACE_OUTER_BOUND ( 'NONE', #23348, .T. ) ;
#32631 = CARTESIAN_POINT ( 'NONE',  ( -9.999999999999998224, 5.773502691896259087, -106.7500000040967620 ) ) ;
#32632 = CARTESIAN_POINT ( 'NONE',  ( -9.999999999999996447, 5.773502691896259975, -169.3750000000000000 ) ) ;
#32633 = CARTESIAN_POINT ( 'NONE',  ( -2.293366432827344421E-15, -12.48450537969573659, -66.21875000204838102 ) ) ;
#32634 = ORIENTED_EDGE ( 'NONE', *, *, #4523, .F. ) ;
#32635 = CARTESIAN_POINT ( 'NONE',  ( -2.121150477449813534E-15, -11.54700538379251284, -44.37499999999997158 ) ) ;
#32636 = EDGE_CURVE ( 'NONE', #35567, #23620, #12519, .T. ) ;
#32637 = CARTESIAN_POINT ( 'NONE',  ( -9.999999999999998224, 5.773502691896259087, -19.75000000409677270 ) ) ;
#32638 = CARTESIAN_POINT ( 'NONE',  ( -10.81189881249999729, -6.242252689847864744, -41.15625000204836681 ) ) ;
#32639 = CARTESIAN_POINT ( 'NONE',  ( 9.999999999999996447, -5.773502691896262640, -47.50000000409676915 ) ) ;
#32640 = CARTESIAN_POINT ( 'NONE',  ( 10.81189881249999551, -6.242252689847874514, -39.15625000204835970 ) ) ;
#32641 = DIRECTION ( 'NONE',  ( 1.000000000000000000, 0.000000000000000000, 0.000000000000000000 ) ) ;
#32642 = CARTESIAN_POINT ( 'NONE',  ( -10.81189881249999729, 6.242252689847871849, -140.4062500020484094 ) ) ;
#32643 = CARTESIAN_POINT ( 'NONE',  ( -10.81189881249999729, 1.324075727343319199E-15, -149.2812500020483810 ) ) ;
#32644 = CARTESIAN_POINT ( 'NONE',  ( -4.999999999999996447, 8.660254037844387298, -150.3750000040967905 ) ) ;
#32645 = ORIENTED_EDGE ( 'NONE', *, *, #11274, .F. ) ;
#32646 = VERTEX_POINT ( 'NONE', #37849 ) ;
#32647 = ORIENTED_EDGE ( 'NONE', *, *, #22279, .T. ) ;
#32648 = CARTESIAN_POINT ( 'NONE',  ( -5.405949406250003975, -9.363379034771801557, -175.8437500020483810 ) ) ;
#32649 = CARTESIAN_POINT ( 'NONE',  ( -5.405949406250003975, -9.363379034771801557, -19.84375000204835615 ) ) ;
#32650 = CARTESIAN_POINT ( 'NONE',  ( -9.999999999999998224, 1.224646799147353059E-15, -113.7499999999999858 ) ) ;
#32651 = CARTESIAN_POINT ( 'NONE',  ( -2.293366432827344421E-15, -12.48450537969573659, -160.7187500020483810 ) ) ;
#32652 = CARTESIAN_POINT ( 'NONE',  ( -10.81189881249999729, 6.242252689847871849, -141.7187500020483810 ) ) ;
#32653 = CARTESIAN_POINT ( 'NONE',  ( 10.00000000000051159, -5.773502691895965988, -119.1249999999999858 ) ) ;
#32654 = CARTESIAN_POINT ( 'NONE',  ( 10.81189881249999729, 0.000000000000000000, -125.8437500020483952 ) ) ;
#32655 = CARTESIAN_POINT ( 'NONE',  ( -10.81189881249999729, 6.242252689847871849, -134.4062500020484094 ) ) ;
#32656 = CARTESIAN_POINT ( 'NONE',  ( 10.81189881249999729, 0.000000000000000000, -14.84375000204835082 ) ) ;
#32657 = CARTESIAN_POINT ( 'NONE',  ( 10.81189881249999551, -6.242252689847874514, -134.9687500020483810 ) ) ;
#32658 = CARTESIAN_POINT ( 'NONE',  ( 10.00000000000025402, -5.773502691896113426, -125.5000000040967763 ) ) ;
#32659 = CARTESIAN_POINT ( 'NONE',  ( -9.999999999999998224, 1.224646799147353059E-15, -103.2500000000000000 ) ) ;
#32660 = CARTESIAN_POINT ( 'NONE',  ( -4.999999999999996447, 8.660254037844387298, -160.5000000000000000 ) ) ;
#32661 = CYLINDRICAL_SURFACE ( 'NONE', #41877, 9.999999999999998224 ) ;
#32662 = CARTESIAN_POINT ( 'NONE',  ( 10.81189881249999907, 6.242252689847868297, -71.71875000204838102 ) ) ;
#32663 = CARTESIAN_POINT ( 'NONE',  ( 5.405949406249999534, 9.363379034771803333, -53.78125000204836681 ) ) ;
#32664 = CARTESIAN_POINT ( 'NONE',  ( -10.81189881249999729, 1.324075727343319199E-15, -50.09375000204835260 ) ) ;
#32665 = CARTESIAN_POINT ( 'NONE',  ( -10.00000000000051337, 5.773502691895962435, -90.25000000409679046 ) ) ;
#32666 = CARTESIAN_POINT ( 'NONE',  ( 5.405949406249999534, 9.363379034771803333, -161.5937500020484094 ) ) ;
#32667 = CARTESIAN_POINT ( 'NONE',  ( -9.999999999999998224, 1.224646799147353059E-15, -139.2499999999999716 ) ) ;
#32668 = CARTESIAN_POINT ( 'NONE',  ( 10.81189881249999729, 0.000000000000000000, -139.5312500020484094 ) ) ;
#32669 =( BOUNDED_CURVE ( )  B_SPLINE_CURVE ( 2, ( #8064, #27486, #11061, #24262, #37409, #27699, #7851 ),
 .UNSPECIFIED., .F., .F. ) 
 B_SPLINE_CURVE_WITH_KNOTS ( ( 3, 2, 2, 3 ),
 ( 0.7798507462686569136, 0.7810945273631842989, 0.7823383084577115731, 0.7835820895522389584 ),
 .UNSPECIFIED. ) 
 CURVE ( )  GEOMETRIC_REPRESENTATION_ITEM ( )  RATIONAL_B_SPLINE_CURVE ( ( 0.9999999999999761302, 0.8660254037844625774, 1.000000000000000000, 0.8660254037844387076, 1.000000000000000000, 0.8660254037844267172, 1.000000000000011990 ) ) 
 REPRESENTATION_ITEM ( '' )  );
#32670 = CARTESIAN_POINT ( 'NONE',  ( -2.121150477449813534E-15, -11.54700538379251284, -98.75000000409677625 ) ) ;
#32671 = CARTESIAN_POINT ( 'NONE',  ( -4.999999999999996447, 8.660254037844387298, -114.3750000040967763 ) ) ;
#32672 = CARTESIAN_POINT ( 'NONE',  ( -2.121150477449813534E-15, -11.54700538379251284, -90.87499999999997158 ) ) ;
#32673 = ORIENTED_EDGE ( 'NONE', *, *, #42320, .F. ) ;
#32674 = CARTESIAN_POINT ( 'NONE',  ( 7.644554776091147741E-16, 12.48450537969573659, -121.1562500020483952 ) ) ;
#32675 = CARTESIAN_POINT ( 'NONE',  ( 9.999999999999998224, 0.000000000000000000, -134.3750000040967905 ) ) ;
#32676 = CARTESIAN_POINT ( 'NONE',  ( -5.000000000000003553, -8.660254037844383745, -22.37500000409675494 ) ) ;
#32677 = CARTESIAN_POINT ( 'NONE',  ( -10.81189881249999729, 6.242252689847871849, -176.4062500020484094 ) ) ;
#32678 = CARTESIAN_POINT ( 'NONE',  ( -4.999999999999996447, 8.660254037844387298, -43.87500000409677625 ) ) ;
#32679 = CARTESIAN_POINT ( 'NONE',  ( 0.000000000000000000, 0.000000000000000000, -200.0000000000000000 ) ) ;
#32680 = CARTESIAN_POINT ( 'NONE',  ( -2.293366432827344421E-15, -12.48450537969573659, -57.40625000204838102 ) ) ;
#32681 = CARTESIAN_POINT ( 'NONE',  ( 9.999999999999612754, 5.773502691896477579, -156.3750000000000000 ) ) ;
#32682 = CARTESIAN_POINT ( 'NONE',  ( -2.293366432827344421E-15, -12.48450537969573659, -163.9062500020483810 ) ) ;
#32683 = CARTESIAN_POINT ( 'NONE',  ( -10.81189881249999729, 1.324075727343319199E-15, -140.0937500020483810 ) ) ;
#32684 = CARTESIAN_POINT ( 'NONE',  ( 5.000000000000000000, 8.660254037844385522, -100.7499999999999858 ) ) ;
#32685 = VERTEX_POINT ( 'NONE', #41500 ) ;
#32686 = DIRECTION ( 'NONE',  ( -0.000000000000000000, -0.000000000000000000, 1.000000000000000000 ) ) ;
#32687 = ADVANCED_FACE ( 'NONE', ( #2665 ), #5904, .T. ) ;
#32689 = ORIENTED_EDGE ( 'NONE', *, *, #9324, .T. ) ;
#32688 = CARTESIAN_POINT ( 'NONE',  ( 10.81189881249999907, 6.242252689847868297, -71.90625000204836681 ) ) ;
#32690 = PERSON_AND_ORGANIZATION ( #11915, #17965 ) ;
#32692 = ORIENTED_EDGE ( 'NONE', *, *, #34286, .F. ) ;
#32691 = CARTESIAN_POINT ( 'NONE',  ( -2.293366432827344421E-15, -12.48450537969573659, -118.7187500020483952 ) ) ;
#32693 = ORIENTED_EDGE ( 'NONE', *, *, #42683, .T. ) ;
#32694 = CARTESIAN_POINT ( 'NONE',  ( -5.405949406250003975, -9.363379034771801557, -24.34375000204835970 ) ) ;
#32695 = CARTESIAN_POINT ( 'NONE',  ( -5.405949406249996869, 9.363379034771805109, -197.3437500020484094 ) ) ;
#32696 = CARTESIAN_POINT ( 'NONE',  ( -5.405949406249996869, 9.363379034771805109, -45.84375000204838102 ) ) ;
#32697 = DIRECTION ( 'NONE',  ( 1.000000000000000000, 0.000000000000000000, 0.000000000000000000 ) ) ;
#32698 = CARTESIAN_POINT ( 'NONE',  ( 7.070501591499377789E-16, 11.54700538379251284, -25.62499999999997868 ) ) ;
#32699 = CARTESIAN_POINT ( 'NONE',  ( -10.81189881249999729, -6.242252689847864744, -187.9687500020484094 ) ) ;
#32700 = CARTESIAN_POINT ( 'NONE',  ( -10.81189881249999729, 1.324075727343319199E-15, -168.5937500020484094 ) ) ;
#32701 = CARTESIAN_POINT ( 'NONE',  ( -5.405949406250003975, -9.363379034771801557, -147.3437500020483810 ) ) ;
#32702 =( BOUNDED_CURVE ( )  B_SPLINE_CURVE ( 2, ( #2997, #38605, #12264, #22209, #29116, #15915, #21993 ),
 .UNSPECIFIED., .F., .F. ) 
 B_SPLINE_CURVE_WITH_KNOTS ( ( 3, 2, 2, 3 ),
 ( 0.1791044776119403437, 0.1803482587064677289, 0.1815920398009950587, 0.1828358208955224162 ),
 .UNSPECIFIED. ) 
 CURVE ( )  GEOMETRIC_REPRESENTATION_ITEM ( )  RATIONAL_B_SPLINE_CURVE ( ( 0.9999999999999940048, 0.8660254037844447028, 1.000000000000000000, 0.8660254037844387076, 1.000000000000000000, 0.8660254037844357100, 1.000000000000003109 ) ) 
 REPRESENTATION_ITEM ( '' )  );
#32703 = CARTESIAN_POINT ( 'NONE',  ( -10.81189881249999729, 1.324075727343319199E-15, -167.0937500020484094 ) ) ;
#32704 = DIRECTION ( 'NONE',  ( -0.000000000000000000, -0.000000000000000000, 1.000000000000000000 ) ) ;
#32705 = CARTESIAN_POINT ( 'NONE',  ( -9.999999999999998224, 1.224646799147353059E-15, -185.7500000000000000 ) ) ;
#32706 = CARTESIAN_POINT ( 'NONE',  ( -5.405949406250003975, -9.363379034771801557, -99.34375000204838102 ) ) ;
#32707 = CARTESIAN_POINT ( 'NONE',  ( 9.999999999999998224, 0.000000000000000000, -108.8750000040967763 ) ) ;
#32708 = CARTESIAN_POINT ( 'NONE',  ( -5.405949406250003975, -9.363379034771801557, -75.53125000204838102 ) ) ;
#32709 = CARTESIAN_POINT ( 'NONE',  ( -9.999999999999998224, 1.224646799147353059E-15, -200.0000000000000000 ) ) ;
#32710 = CARTESIAN_POINT ( 'NONE',  ( -10.81189881249999729, 1.324075727343319199E-15, -183.5937500020483810 ) ) ;
#32711 = CARTESIAN_POINT ( 'NONE',  ( 10.81189881249999729, 6.242252689847867408, -158.9062500020483810 ) ) ;
#32712 = CARTESIAN_POINT ( 'NONE',  ( 7.644554776091147741E-16, 12.48450537969573659, -62.65625000204838813 ) ) ;
#32713 = CARTESIAN_POINT ( 'NONE',  ( 9.999999999999998224, 0.000000000000000000, -134.3750000040967905 ) ) ;
#32714 = CARTESIAN_POINT ( 'NONE',  ( -5.000000000000003553, -8.660254037844383745, -111.9999999999999858 ) ) ;
#32715 = ORIENTED_EDGE ( 'NONE', *, *, #29931, .F. ) ;
#32716 = CARTESIAN_POINT ( 'NONE',  ( -10.81189881249999729, -6.242252689847864744, -140.1562500020484094 ) ) ;
#32717 = CARTESIAN_POINT ( 'NONE',  ( 5.405949406249999534, 9.363379034771803333, -157.2812500020484094 ) ) ;
#32718 = CARTESIAN_POINT ( 'NONE',  ( 7.644554776091147741E-16, 12.48450537969573659, -194.6562500020484094 ) ) ;
#32719 = CARTESIAN_POINT ( 'NONE',  ( 0.000000000000000000, 0.000000000000000000, -99.99999999999998579 ) ) ;
#32720 = CARTESIAN_POINT ( 'NONE',  ( -5.405949406249996869, 9.363379034771805109, -89.34375000204838102 ) ) ;
#32721 = ORIENTED_EDGE ( 'NONE', *, *, #41568, .F. ) ;
#32722 = CARTESIAN_POINT ( 'NONE',  ( 5.000000000000000000, 8.660254037844385522, -54.24999999999996447 ) ) ;
#32723 = CARTESIAN_POINT ( 'NONE',  ( 5.405949406249992428, -9.363379034771808662, -187.5937500020483810 ) ) ;
#32724 = CARTESIAN_POINT ( 'NONE',  ( 9.999999999999996447, -5.773502691896262640, -76.00000000409677625 ) ) ;
#32725 = LINE ( 'NONE', #9625, #22393 ) ;
#32726 = CARTESIAN_POINT ( 'NONE',  ( 4.999999999999992006, -8.660254037844389075, -160.1250000040967905 ) ) ;
#32727 = CARTESIAN_POINT ( 'NONE',  ( 7.644554776091147741E-16, 12.48450537969573659, -83.65625000204838102 ) ) ;
#32728 = CARTESIAN_POINT ( 'NONE',  ( -10.81189881249999729, 1.324075727343319199E-15, -68.28125000204838102 ) ) ;
#32729 = CARTESIAN_POINT ( 'NONE',  ( 4.999999999999992006, -8.660254037844389075, -62.62500000409676204 ) ) ;
#32730 = CARTESIAN_POINT ( 'NONE',  ( -10.81189881249999729, 6.242252689847871849, -20.21875000204836681 ) ) ;
#32731 = DIRECTION ( 'NONE',  ( -0.000000000000000000, -0.000000000000000000, 1.000000000000000000 ) ) ;
#32732 = CARTESIAN_POINT ( 'NONE',  ( -10.81189881249999729, 1.324075727343319199E-15, -185.2812500020484094 ) ) ;
#32733 = CARTESIAN_POINT ( 'NONE',  ( 10.81189881249999729, 0.000000000000000000, -15.03125000204835793 ) ) ;
#32734 = CARTESIAN_POINT ( 'NONE',  ( -9.999999999999998224, 1.224646799147353059E-15, -85.24999999999997158 ) ) ;
#32735 = CARTESIAN_POINT ( 'NONE',  ( 9.999999999999998224, 0.000000000000000000, -149.0000000000000000 ) ) ;
#32736 = CARTESIAN_POINT ( 'NONE',  ( 10.00000000000154010, -5.773502691895370020, -62.50000000409673362 ) ) ;
#32737 = CARTESIAN_POINT ( 'NONE',  ( -5.755749739768639017, 8.223921721521577410, 0.000000000000000000 ) ) ;
#32738 = CARTESIAN_POINT ( 'NONE',  ( 9.999999999999996447, -5.773502691896262640, -167.1250000000000000 ) ) ;
#32739 = DIRECTION ( 'NONE',  ( 1.000000000000000000, 0.000000000000000000, 0.000000000000000000 ) ) ;
#32741 = ORIENTED_EDGE ( 'NONE', *, *, #29386, .F. ) ;
#32740 = CARTESIAN_POINT ( 'NONE',  ( -10.81189881249999729, 1.324075727343319199E-15, -92.28125000204838102 ) ) ;
#32742 = CARTESIAN_POINT ( 'NONE',  ( 10.00000000000012257, -5.773502691896188921, -162.6250000000000568 ) ) ;
#32743 = EDGE_CURVE ( 'NONE', #4341, #18779, #30196, .T. ) ;
#32745 = ORIENTED_EDGE ( 'NONE', *, *, #21998, .F. ) ;
#32744 = CARTESIAN_POINT ( 'NONE',  ( -2.293366432827344421E-15, -12.48450537969573659, -102.2187500020483668 ) ) ;
#32746 = ORIENTED_EDGE ( 'NONE', *, *, #7691, .T. ) ;
#32747 = CARTESIAN_POINT ( 'NONE',  ( -10.81189881249999907, -6.242252689847864744, -33.46875000204834549 ) ) ;
#32748 = AXIS2_PLACEMENT_3D ( 'NONE', #12341, #35466, #9122 ) ;
#32749 = CARTESIAN_POINT ( 'NONE',  ( -2.293366432827344421E-15, -12.48450537969573659, -25.90625000204838813 ) ) ;
#32750 = CARTESIAN_POINT ( 'NONE',  ( 10.81189881249999907, 6.242252689847868297, -82.21875000204836681 ) ) ;
#32751 = DIRECTION ( 'NONE',  ( 1.000000000000000000, 0.000000000000000000, 0.000000000000000000 ) ) ;
#32752 = CARTESIAN_POINT ( 'NONE',  ( -10.81189881249999907, -6.242252689847864744, -192.4687500020484094 ) ) ;
#32753 = CARTESIAN_POINT ( 'NONE',  ( -5.000000000000003553, -8.660254037844383745, -121.3750000040967905 ) ) ;
#32754 = LINE ( 'NONE', #39432, #20520 ) ;
#32755 = CARTESIAN_POINT ( 'NONE',  ( -10.81189881249999729, 6.242252689847871849, -158.4062500020483810 ) ) ;
#32756 = CARTESIAN_POINT ( 'NONE',  ( 4.999999999999992006, -8.660254037844389075, 0.3749999959032357388 ) ) ;
#32757 = CARTESIAN_POINT ( 'NONE',  ( -9.999999999999998224, 1.224646799147353059E-15, -178.2500000000000284 ) ) ;
#32758 = CARTESIAN_POINT ( 'NONE',  ( -10.81189881249999907, -6.242252689847864744, -120.4687500020483810 ) ) ;
#32759 = CARTESIAN_POINT ( 'NONE',  ( 10.81189881249999729, 0.000000000000000000, -97.53125000204839523 ) ) ;
#32760 = CARTESIAN_POINT ( 'NONE',  ( -10.81189881249999729, 6.242252689847871849, -104.2187500020483810 ) ) ;
#32761 = CARTESIAN_POINT ( 'NONE',  ( 10.81189881249999729, 0.000000000000000000, -77.84375000204838102 ) ) ;
#32762 = VECTOR ( 'NONE', #30022, 1000.000000000000000 ) ;
#32763 = CARTESIAN_POINT ( 'NONE',  ( 7.644554776091147741E-16, 12.48450537969573659, -85.15625000204838102 ) ) ;
#32764 = CARTESIAN_POINT ( 'NONE',  ( 5.000000000000000000, 8.660254037844385522, -168.6250000040967905 ) ) ;
#32765 = DIRECTION ( 'NONE',  ( 1.000000000000000000, 0.000000000000000000, 0.000000000000000000 ) ) ;
#32766 = CARTESIAN_POINT ( 'NONE',  ( 5.405949406249999534, 9.363379034771803333, -169.2812500020484094 ) ) ;
#32767 = CARTESIAN_POINT ( 'NONE',  ( 5.405949406249999534, 9.363379034771803333, -176.7812500020484094 ) ) ;
#32768 = CARTESIAN_POINT ( 'NONE',  ( -4.999999999999996447, 8.660254037844387298, -154.8750000040967905 ) ) ;
#32769 = CARTESIAN_POINT ( 'NONE',  ( -9.999999999999998224, 1.224646799147353059E-15, -79.62500000409677625 ) ) ;
#32770 = CARTESIAN_POINT ( 'NONE',  ( 5.405949406249999534, 9.363379034771803333, -4.093750002048368586 ) ) ;
#32771 = CARTESIAN_POINT ( 'NONE',  ( 4.999999999999992006, -8.660254037844389075, -156.7500000000000000 ) ) ;
#32772 = CARTESIAN_POINT ( 'NONE',  ( 5.405949406249992428, -9.363379034771808662, -117.0937500020483810 ) ) ;
#32773 = CARTESIAN_POINT ( 'NONE',  ( 4.999999999999992006, -8.660254037844389075, -84.74999999999997158 ) ) ;
#32774 = CARTESIAN_POINT ( 'NONE',  ( 5.405949406249992428, -9.363379034771808662, -13.78125000204835615 ) ) ;
#32775 = CARTESIAN_POINT ( 'NONE',  ( 7.070501591499377789E-16, 11.54700538379251284, -95.00000000409677625 ) ) ;
#32776 = CYLINDRICAL_SURFACE ( 'NONE', #15504, 9.999999999999998224 ) ;
#32777 = CARTESIAN_POINT ( 'NONE',  ( -10.81189881249999729, 1.324075727343319199E-15, -110.2812500020483810 ) ) ;
#32778 = CARTESIAN_POINT ( 'NONE',  ( 10.81189881249999729, 6.242252689847867408, -88.40625000204836681 ) ) ;
#32779 = ORIENTED_EDGE ( 'NONE', *, *, #26106, .F. ) ;
#32780 = CARTESIAN_POINT ( 'NONE',  ( 4.999999999999992006, -8.660254037844389075, -86.62500000409677625 ) ) ;
#32781 = LINE ( 'NONE', #29760, #18769 ) ;
#32782 = CARTESIAN_POINT ( 'NONE',  ( -10.81189881249999729, 6.242252689847871849, -41.21875000204835970 ) ) ;
#32783 = ORIENTED_EDGE ( 'NONE', *, *, #35462, .F. ) ;
#32784 = CARTESIAN_POINT ( 'NONE',  ( 10.00000000000000000, 5.773502691896255534, -10.87499999999995381 ) ) ;
#32785 = CARTESIAN_POINT ( 'NONE',  ( 9.999999999999996447, -5.773502691896262640, -146.1250000000000000 ) ) ;
#32786 = CARTESIAN_POINT ( 'NONE',  ( -4.999999999999996447, 8.660254037844387298, -10.87500000409674605 ) ) ;
#32787 = CARTESIAN_POINT ( 'NONE',  ( -4.999999999999996447, 8.660254037844387298, -196.5000000000000000 ) ) ;
#32789 = ORIENTED_EDGE ( 'NONE', *, *, #19490, .F. ) ;
#32788 = CARTESIAN_POINT ( 'NONE',  ( -2.293366432827344421E-15, -12.48450537969573659, -114.4062500020483952 ) ) ;
#32790 = CYLINDRICAL_SURFACE ( 'NONE', #17263, 5.500000000000003553 ) ;
#32791 = EDGE_CURVE ( 'NONE', #8276, #13430, #31601, .T. ) ;
#32792 =( BOUNDED_CURVE ( )  B_SPLINE_CURVE ( 2, ( #37019, #7459, #7892, #4645, #11318, #37664, #24085 ),
 .UNSPECIFIED., .F., .F. ) 
 B_SPLINE_CURVE_WITH_KNOTS ( ( 3, 2, 2, 3 ),
 ( 0.2014925373134328901, 0.2027363184079602476, 0.2039800995024875774, 0.2052238805970149627 ),
 .UNSPECIFIED. ) 
 CURVE ( )  GEOMETRIC_REPRESENTATION_ITEM ( )  RATIONAL_B_SPLINE_CURVE ( ( 0.9999999999999940048, 0.8660254037844447028, 1.000000000000000000, 0.8660254037844387076, 1.000000000000000000, 0.8660254037844357100, 1.000000000000002887 ) ) 
 REPRESENTATION_ITEM ( '' )  );
#32793 = ADVANCED_FACE ( 'NONE', ( #38701 ), #42135, .F. ) ;
#32794 = AXIS2_PLACEMENT_3D ( 'NONE', #27435, #1108, #4990 ) ;
#32795 = ORIENTED_EDGE ( 'NONE', *, *, #27856, .T. ) ;
#32796 = EDGE_CURVE ( 'NONE', #17140, #26892, #41921, .T. ) ;
#32797 = CARTESIAN_POINT ( 'NONE',  ( 10.81189881249999729, 0.000000000000000000, -48.03125000204838813 ) ) ;
#32798 = PERSON_AND_ORGANIZATION ( #11915, #17965 ) ;
#32799 = CARTESIAN_POINT ( 'NONE',  ( -10.81189881249999907, -6.242252689847864744, -99.46875000204838102 ) ) ;
#32800 = CARTESIAN_POINT ( 'NONE',  ( -10.81189881249999729, -6.242252689847864744, -123.6562500020484094 ) ) ;
#32801 = VERTEX_POINT ( 'NONE', #28362 ) ;
#32802 = AXIS2_PLACEMENT_3D ( 'NONE', #31105, #20512, #4124 ) ;
#32803 = CARTESIAN_POINT ( 'NONE',  ( 0.000000000000000000, 0.000000000000000000, -99.99999999999998579 ) ) ;
#32804 = APPROVAL ( #21966, 'UNKNOWN' ) ;
#32805 = DIRECTION ( 'NONE',  ( 1.000000000000000000, 0.000000000000000000, 0.000000000000000000 ) ) ;
#32806 = CARTESIAN_POINT ( 'NONE',  ( 10.81189881249999551, -6.242252689847874514, -178.6562500020484094 ) ) ;
#32807 = CARTESIAN_POINT ( 'NONE',  ( 10.81189881249999551, -6.242252689847874514, -1.468750002048354819 ) ) ;
#32808 = FACE_OUTER_BOUND ( 'NONE', #40731, .T. ) ;
#32809 = ADVANCED_FACE ( 'NONE', ( #25125 ), #8717, .T. ) ;
#32810 = CARTESIAN_POINT ( 'NONE',  ( -5.405949406249996869, 9.363379034771805109, -135.8437500020484094 ) ) ;
#32811 = CARTESIAN_POINT ( 'NONE',  ( 5.405949406249992428, -9.363379034771808662, -102.0937500020483810 ) ) ;
#32812 = CARTESIAN_POINT ( 'NONE',  ( 9.999999999999998224, 0.000000000000000000, -116.3750000040967905 ) ) ;
#32813 = CARTESIAN_POINT ( 'NONE',  ( -10.81189881249999729, 6.242252689847871849, -111.9062500020483810 ) ) ;
#32814 = CARTESIAN_POINT ( 'NONE',  ( 4.999999999999992006, -8.660254037844389075, -191.6250000040967905 ) ) ;
#32815 = CARTESIAN_POINT ( 'NONE',  ( 10.81189881249999729, 6.242252689847867408, -118.2187500020483810 ) ) ;
#32816 = CARTESIAN_POINT ( 'NONE',  ( -10.81189881249999729, 6.242252689847871849, -186.9062500020484094 ) ) ;
#32817 = CARTESIAN_POINT ( 'NONE',  ( 7.070501591499376803E-16, 11.54700538379251284, -6.500000004096742501 ) ) ;
#32818 = CARTESIAN_POINT ( 'NONE',  ( -4.999999999999996447, 8.660254037844387298, -141.0000000000000000 ) ) ;
#32819 = CARTESIAN_POINT ( 'NONE',  ( -10.00000000000000000, -5.773502691896251982, -2.624999999999960920 ) ) ;
#32820 = EDGE_CURVE ( 'NONE', #16786, #8228, #15541, .T. ) ;
#32821 = CARTESIAN_POINT ( 'NONE',  ( -5.405949406249996869, 9.363379034771805109, -60.84375000204836681 ) ) ;
#32822 = CARTESIAN_POINT ( 'NONE',  ( -10.81189881249999907, -6.242252689847864744, -52.96875000204838102 ) ) ;
#32823 = CARTESIAN_POINT ( 'NONE',  ( 7.070501591499377789E-16, 11.54700538379251284, -180.5000000040967905 ) ) ;
#32824 = CARTESIAN_POINT ( 'NONE',  ( 5.405949406249992428, -9.363379034771808662, -19.78125000204836326 ) ) ;
#32825 = CARTESIAN_POINT ( 'NONE',  ( -5.405949406249996869, 9.363379034771805109, -32.34375000204836681 ) ) ;
#32826 = CARTESIAN_POINT ( 'NONE',  ( -4.999999999999996447, 8.660254037844387298, -27.37500000409676204 ) ) ;
#32827 = CARTESIAN_POINT ( 'NONE',  ( -10.81189881249999729, 6.242252689847871849, -141.7187500020483810 ) ) ;
#32828 = CARTESIAN_POINT ( 'NONE',  ( -10.00000000000000000, -5.773502691896251982, -106.1249999999999858 ) ) ;
#32829 = CARTESIAN_POINT ( 'NONE',  ( 10.81189881249999551, -6.242252689847874514, -36.15625000204835970 ) ) ;
#32830 = EDGE_CURVE ( 'NONE', #33229, #27592, #19957, .T. ) ;
#32831 = CARTESIAN_POINT ( 'NONE',  ( -4.999999999999996447, 8.660254037844387298, -163.5000000000000000 ) ) ;
#32832 = AXIS2_PLACEMENT_3D ( 'NONE', #14185, #34298, #27168 ) ;
#32833 = CARTESIAN_POINT ( 'NONE',  ( 9.999999999999996447, -5.773502691896262640, -68.12499999999998579 ) ) ;
#32834 = CARTESIAN_POINT ( 'NONE',  ( 5.405949406249992428, -9.363379034771808662, -133.7812500020483810 ) ) ;
#32835 = CARTESIAN_POINT ( 'NONE',  ( -5.405949406250003975, -9.363379034771801557, -114.5312500020483952 ) ) ;
#32836 = ORIENTED_EDGE ( 'NONE', *, *, #9301, .T. ) ;
#32837 = CARTESIAN_POINT ( 'NONE',  ( 7.070501591499376803E-16, 11.54700538379251284, -142.6250000000000000 ) ) ;
#32838 = CARTESIAN_POINT ( 'NONE',  ( 5.000000000000000000, 8.660254037844385522, -111.6250000040967763 ) ) ;
#32839 = CARTESIAN_POINT ( 'NONE',  ( -9.999999999999998224, 1.224646799147353059E-15, -100.6250000040967905 ) ) ;
#32840 = CARTESIAN_POINT ( 'NONE',  ( -5.405949406250003975, -9.363379034771801557, -63.34375000204836681 ) ) ;
#32841 = ORIENTED_EDGE ( 'NONE', *, *, #42516, .T. ) ;
#32842 = CARTESIAN_POINT ( 'NONE',  ( 10.00000000000000000, 5.773502691896255534, -39.37499999999996447 ) ) ;
#32843 = CARTESIAN_POINT ( 'NONE',  ( -9.999999999999998224, 1.224646799147353059E-15, -18.12500000409675138 ) ) ;
#32844 = CARTESIAN_POINT ( 'NONE',  ( 5.405949406249999534, 9.363379034771803333, -44.78125000204838102 ) ) ;
#32845 = EDGE_CURVE ( 'NONE', #15525, #36438, #34610, .T. ) ;
#32846 = CARTESIAN_POINT ( 'NONE',  ( -9.999999999999998224, 1.224646799147353059E-15, -157.6250000040967905 ) ) ;
#32847 = CARTESIAN_POINT ( 'NONE',  ( 4.999999999999992006, -8.660254037844389075, -40.12500000409676915 ) ) ;
#32848 = EDGE_CURVE ( 'NONE', #21106, #37675, #38484, .T. ) ;
#32849 =( BOUNDED_CURVE ( )  B_SPLINE_CURVE ( 2, ( #8506, #21229, #24278, #21660, #4833, #34840, #5264 ),
 .UNSPECIFIED., .F., .F. ) 
 B_SPLINE_CURVE_WITH_KNOTS ( ( 3, 2, 2, 3 ),
 ( 0.5783582089552241623, 0.5796019900497515476, 0.5808457711442788218, 0.5820895522388062071 ),
 .UNSPECIFIED. ) 
 CURVE ( )  GEOMETRIC_REPRESENTATION_ITEM ( )  RATIONAL_B_SPLINE_CURVE ( ( 0.9999999999999641398, 0.8660254037844745678, 1.000000000000000000, 0.8660254037844387076, 1.000000000000000000, 0.8660254037844148378, 1.000000000000023981 ) ) 
 REPRESENTATION_ITEM ( '' )  );
#32850 = CARTESIAN_POINT ( 'NONE',  ( -4.999999999999996447, 8.660254037844387298, -166.5000000000000000 ) ) ;
#32851 = CARTESIAN_POINT ( 'NONE',  ( -10.81189881249999729, 1.324075727343319199E-15, -137.2812500020483810 ) ) ;
#32852 = CARTESIAN_POINT ( 'NONE',  ( 10.81189881249999551, -6.242252689847874514, -144.1562500020484094 ) ) ;
#32853 = EDGE_LOOP ( 'NONE', ( #27864, #32958, #16870, #24522 ) ) ;
#32854 =( BOUNDED_CURVE ( )  B_SPLINE_CURVE ( 2, ( #16582, #33240, #3666, #39899, #6475, #16794, #9494 ),
 .UNSPECIFIED., .F., .F. ) 
 B_SPLINE_CURVE_WITH_KNOTS ( ( 3, 2, 2, 3 ),
 ( 0.3507462686567164867, 0.3519900497512438720, 0.3532338308457712572, 0.3544776119402986980 ),
 .UNSPECIFIED. ) 
 CURVE ( )  GEOMETRIC_REPRESENTATION_ITEM ( )  RATIONAL_B_SPLINE_CURVE ( ( 0.9999999999999940048, 0.8660254037844447028, 1.000000000000000000, 0.8660254037844387076, 1.000000000000000000, 0.8660254037844207220, 1.000000000000017986 ) ) 
 REPRESENTATION_ITEM ( '' )  );
#32855 = EDGE_LOOP ( 'NONE', ( #32208, #34290, #2910, #20149 ) ) ;
#32856 = VERTEX_POINT ( 'NONE', #32030 ) ;
#32857 = CARTESIAN_POINT ( 'NONE',  ( -9.999999999999998224, 1.224646799147353059E-15, -130.2499999999999716 ) ) ;
#32858 = CARTESIAN_POINT ( 'NONE',  ( -5.405949406250003975, -9.363379034771801557, -172.8437500020484094 ) ) ;
#32859 = CARTESIAN_POINT ( 'NONE',  ( -10.81189881249999729, 6.242252689847871849, -26.21875000204837391 ) ) ;
#32860 = CARTESIAN_POINT ( 'NONE',  ( 9.999999999999998224, 0.000000000000000000, -200.0000000000000000 ) ) ;
#32861 = CARTESIAN_POINT ( 'NONE',  ( -10.81189881249999729, 6.242252689847871849, -153.7187500020483810 ) ) ;
#32862 = CARTESIAN_POINT ( 'NONE',  ( -10.81189881249999729, 1.324075727343319199E-15, -143.0937500020483810 ) ) ;
#32863 = CARTESIAN_POINT ( 'NONE',  ( -9.999999999999998224, 1.224646799147353059E-15, -10.24999999999995381 ) ) ;
#32864 = CARTESIAN_POINT ( 'NONE',  ( -2.293366432827344421E-15, -12.48450537969573659, -124.7187500020483668 ) ) ;
#32865 = CARTESIAN_POINT ( 'NONE',  ( 5.405949406249999534, 9.363379034771803333, -136.2812500020483810 ) ) ;
#32866 = CARTESIAN_POINT ( 'NONE',  ( -10.81189881249999729, 1.324075727343319199E-15, -21.59375000204835615 ) ) ;
#32867 = CARTESIAN_POINT ( 'NONE',  ( 5.405949406249999534, 9.363379034771803333, -137.5937500020483810 ) ) ;
#32868 = CYLINDRICAL_SURFACE ( 'NONE', #3326, 9.999999999999998224 ) ;
#32869 = CARTESIAN_POINT ( 'NONE',  ( 9.999999999999998224, 0.000000000000000000, -141.8750000040967905 ) ) ;
#32870 = CARTESIAN_POINT ( 'NONE',  ( 4.999999999999992006, -8.660254037844389075, -164.2500000000000000 ) ) ;
#32871 = CARTESIAN_POINT ( 'NONE',  ( -9.999999999999998224, 1.224646799147353059E-15, -132.1250000040967620 ) ) ;
#32872 = CARTESIAN_POINT ( 'NONE',  ( -2.293366432827344421E-15, -12.48450537969573659, -70.71875000204839523 ) ) ;
#32873 = CARTESIAN_POINT ( 'NONE',  ( 5.405949406249992428, -9.363379034771808662, -42.28125000204838102 ) ) ;
#32874 = CARTESIAN_POINT ( 'NONE',  ( 5.405949406249999534, 9.363379034771803333, -56.59375000204835970 ) ) ;
#32875 = CARTESIAN_POINT ( 'NONE',  ( 42.00000000000004974, 0.000000000000000000, -219.9999999999999716 ) ) ;
#32876 = CARTESIAN_POINT ( 'NONE',  ( 5.405949406249999534, 9.363379034771803333, -160.0937500020484094 ) ) ;
#32877 = CARTESIAN_POINT ( 'NONE',  ( -9.999999999999998224, 5.773502691896259087, -128.8749999999999716 ) ) ;
#32878 = CARTESIAN_POINT ( 'NONE',  ( 5.405949406249999534, 9.363379034771803333, -134.7812500020483810 ) ) ;
#32879 = CYLINDRICAL_SURFACE ( 'NONE', #40323, 9.999999999999998224 ) ;
#32880 = CARTESIAN_POINT ( 'NONE',  ( -2.121150477449813534E-15, -11.54700538379251284, -116.7500000040967905 ) ) ;
#32881 = CARTESIAN_POINT ( 'NONE',  ( 10.00000000000000000, 5.773502691896255534, -93.37499999999997158 ) ) ;
#32882 = VERTEX_POINT ( 'NONE', #9344 ) ;
#32883 = CARTESIAN_POINT ( 'NONE',  ( -5.405949406249996869, 9.363379034771805109, -109.0312500020483810 ) ) ;
#32884 = CARTESIAN_POINT ( 'NONE',  ( 4.999999999999992006, -8.660254037844389075, -134.6250000040967620 ) ) ;
#32885 = CYLINDRICAL_SURFACE ( 'NONE', #11178, 9.999999999999998224 ) ;
#32886 = CARTESIAN_POINT ( 'NONE',  ( 10.81189881249999907, 6.242252689847868297, -173.9062500020484094 ) ) ;
#32887 = CARTESIAN_POINT ( 'NONE',  ( -2.121150477449813534E-15, -11.54700538379251284, -40.25000000409676204 ) ) ;
#32888 = CARTESIAN_POINT ( 'NONE',  ( 4.999999999999992006, -8.660254037844389075, -91.12500000409677625 ) ) ;
#32889 = CARTESIAN_POINT ( 'NONE',  ( -5.405949406249996869, 9.363379034771805109, -58.03125000204836681 ) ) ;
#32890 = CARTESIAN_POINT ( 'NONE',  ( -10.00000000000038547, 5.773502691896036154, -155.8749999999999432 ) ) ;
#32891 = CARTESIAN_POINT ( 'NONE',  ( 10.81189881249999907, 6.242252689847868297, -157.4062500020483810 ) ) ;
#32892 = CARTESIAN_POINT ( 'NONE',  ( 10.81189881249999729, 0.000000000000000000, -146.8437500020483810 ) ) ;
#32893 = CARTESIAN_POINT ( 'NONE',  ( -9.999999999998456346, -5.773502691897145489, -51.00000000409671941 ) ) ;
#32894 = CARTESIAN_POINT ( 'NONE',  ( -9.999999999999998224, 1.224646799147353059E-15, -200.0000000000000000 ) ) ;
#32895 = EDGE_LOOP ( 'NONE', ( #29137, #2637, #17962, #32957 ) ) ;
#32896 = CARTESIAN_POINT ( 'NONE',  ( 31.99999999999997158, 0.000000000000000000, -180.0000000000000000 ) ) ;
#32898 = ORIENTED_EDGE ( 'NONE', *, *, #23304, .T. ) ;
#32897 = CARTESIAN_POINT ( 'NONE',  ( 10.81189881249999729, 0.000000000000000000, -67.53125000204838102 ) ) ;
#32899 = CALENDAR_DATE ( 2026, 28, 9 ) ;
#32901 = VERTEX_POINT ( 'NONE', #2458 ) ;
#32900 = CARTESIAN_POINT ( 'NONE',  ( 7.644554776091147741E-16, 12.48450537969573659, -116.4687500020483952 ) ) ;
#32902 = ORIENTED_EDGE ( 'NONE', *, *, #3448, .F. ) ;
#32903 = CARTESIAN_POINT ( 'NONE',  ( -5.405949406249996869, 9.363379034771805109, -20.34375000204835615 ) ) ;
#32904 = CARTESIAN_POINT ( 'NONE',  ( 5.405949406249992428, -9.363379034771808662, -1.781250002048373471 ) ) ;
#32906 = EDGE_CURVE ( 'NONE', #419, #4342, #28790, .T. ) ;
#32905 = CARTESIAN_POINT ( 'NONE',  ( 10.81189881249999551, -6.242252689847874514, -44.96875000204836681 ) ) ;
#32907 = FACE_OUTER_BOUND ( 'NONE', #29762, .T. ) ;
#32908 = CARTESIAN_POINT ( 'NONE',  ( -5.000000000000003553, -8.660254037844383745, -29.49999999999997158 ) ) ;
#32909 = CARTESIAN_POINT ( 'NONE',  ( -10.81189881249999729, 1.324075727343319199E-15, -177.5937500020484094 ) ) ;
#32910 = CARTESIAN_POINT ( 'NONE',  ( 10.81189881249999551, -6.242252689847874514, -170.9687500020483810 ) ) ;
#32911 =( BOUNDED_CURVE ( )  B_SPLINE_CURVE ( 2, ( #9877, #13092, #23050, #42246, #36207, #18955, #22625 ),
 .UNSPECIFIED., .F., .F. ) 
 B_SPLINE_CURVE_WITH_KNOTS ( ( 3, 2, 2, 3 ),
 ( 0.6604477611940301474, 0.6616915422885575326, 0.6629353233830848069, 0.6641791044776121922 ),
 .UNSPECIFIED. ) 
 CURVE ( )  GEOMETRIC_REPRESENTATION_ITEM ( )  RATIONAL_B_SPLINE_CURVE ( ( 0.9999999999999641398, 0.8660254037844745678, 1.000000000000000000, 0.8660254037844387076, 1.000000000000000000, 0.8660254037844148378, 1.000000000000023981 ) ) 
 REPRESENTATION_ITEM ( '' )  );
#32912 = CARTESIAN_POINT ( 'NONE',  ( -10.81189881249999729, 1.324075727343319199E-15, -149.0937500020483810 ) ) ;
#32913 = CARTESIAN_POINT ( 'NONE',  ( -5.405949406250003975, -9.363379034771801557, -163.8437500020484094 ) ) ;
#32914 = CARTESIAN_POINT ( 'NONE',  ( 5.000000000000000000, 8.660254037844385522, -123.6250000040967905 ) ) ;
#32915 = CARTESIAN_POINT ( 'NONE',  ( 7.070501591499377789E-16, 11.54700538379251284, -189.1250000000000000 ) ) ;
#32916 = CARTESIAN_POINT ( 'NONE',  ( -5.405949406250003975, -9.363379034771801557, -100.8437500020483810 ) ) ;
#32917 = CARTESIAN_POINT ( 'NONE',  ( 10.00000000000000000, 5.773502691896255534, -198.7500000040968189 ) ) ;
#32918 = CARTESIAN_POINT ( 'NONE',  ( 10.81189881249999907, 6.242252689847868297, -62.90625000204838813 ) ) ;
#32919 = CARTESIAN_POINT ( 'NONE',  ( -9.999999999999998224, 1.224646799147353059E-15, -132.1250000040967620 ) ) ;
#32920 = CARTESIAN_POINT ( 'NONE',  ( -2.293366432827344421E-15, -12.48450537969573659, -184.7187500020484094 ) ) ;
#32921 = CARTESIAN_POINT ( 'NONE',  ( -10.81189881249999729, -6.242252689847864744, -164.1562500020483810 ) ) ;
#32922 = CARTESIAN_POINT ( 'NONE',  ( -2.293366432827344421E-15, -12.48450537969573659, -61.90625000204838813 ) ) ;
#32923 = CARTESIAN_POINT ( 'NONE',  ( -9.999999999999998224, 5.773502691896259087, -138.2500000040967905 ) ) ;
#32924 = CARTESIAN_POINT ( 'NONE',  ( -2.121150477449813534E-15, -11.54700538379251284, -116.3749999999999858 ) ) ;
#32925 = ADVANCED_FACE ( 'NONE', ( #29845 ), #32868, .T. ) ;
#32926 = ORIENTED_EDGE ( 'NONE', *, *, #12742, .T. ) ;
#32927 = CARTESIAN_POINT ( 'NONE',  ( 5.405949406249992428, -9.363379034771808662, -142.7812500020483810 ) ) ;
#32928 = CARTESIAN_POINT ( 'NONE',  ( -5.405949406249996869, 9.363379034771805109, -158.5312500020484094 ) ) ;
#32929 = CARTESIAN_POINT ( 'NONE',  ( 7.644554776091147741E-16, 12.48450537969573659, -196.1562500020484379 ) ) ;
#32930 = CARTESIAN_POINT ( 'NONE',  ( 9.999999999999998224, 0.000000000000000000, -125.0000000000000000 ) ) ;
#32931 = CARTESIAN_POINT ( 'NONE',  ( -10.81189881249999729, 1.324075727343319199E-15, -93.59375000204838102 ) ) ;
#32932 = AXIS2_PLACEMENT_3D ( 'NONE', #26491, #33614, #7484 ) ;
#32933 = VERTEX_POINT ( 'NONE', #22726 ) ;
#32934 = CARTESIAN_POINT ( 'NONE',  ( -5.000000000000003553, -8.660254037844383745, -57.99999999999997158 ) ) ;
#32935 = CARTESIAN_POINT ( 'NONE',  ( -10.81189881249999907, -6.242252689847864744, -187.9687500020484094 ) ) ;
#32936 = CARTESIAN_POINT ( 'NONE',  ( 7.070501591499377789E-16, 11.54700538379251284, -63.50000000409679046 ) ) ;
#32937 = VECTOR ( 'NONE', #23897, 1000.000000000000000 ) ;
#32938 = CARTESIAN_POINT ( 'NONE',  ( 7.070501591499376803E-16, 11.54700538379251284, -66.12499999999998579 ) ) ;
#32939 = CARTESIAN_POINT ( 'NONE',  ( -2.121150477449813534E-15, -11.54700538379251284, -144.8750000000000000 ) ) ;
#32940 = CARTESIAN_POINT ( 'NONE',  ( -10.81189881249999907, -6.242252689847864744, -86.15625000204836681 ) ) ;
#32941 = CARTESIAN_POINT ( 'NONE',  ( -10.81189881249999729, -6.242252689847864744, -57.65625000204838102 ) ) ;
#32942 = CARTESIAN_POINT ( 'NONE',  ( -2.121150477449813534E-15, -11.54700538379251284, -58.25000000409676915 ) ) ;
#32943 = CARTESIAN_POINT ( 'NONE',  ( -5.405949406249996869, 9.363379034771805109, -15.84375000204835082 ) ) ;
#32944 = CARTESIAN_POINT ( 'NONE',  ( -9.999999999999998224, 1.224646799147353059E-15, -37.62500000409676915 ) ) ;
#32945 = CARTESIAN_POINT ( 'NONE',  ( -5.405949406249996869, 9.363379034771805109, -187.0312500020484094 ) ) ;
#32946 = CARTESIAN_POINT ( 'NONE',  ( -2.293366432827344421E-15, -12.48450537969573659, -15.40625000204837214 ) ) ;
#32947 = CARTESIAN_POINT ( 'NONE',  ( 7.070501591499376803E-16, 11.54700538379251284, -85.62500000000000000 ) ) ;
#32948 = DIRECTION ( 'NONE',  ( -0.000000000000000000, -0.000000000000000000, 1.000000000000000000 ) ) ;
#32949 = CARTESIAN_POINT ( 'NONE',  ( 9.999999999999998224, 0.000000000000000000, -62.37500000409676204 ) ) ;
#32950 = CARTESIAN_POINT ( 'NONE',  ( -9.999999999999998224, 1.224646799147353059E-15, -135.1250000040967620 ) ) ;
#32951 = CARTESIAN_POINT ( 'NONE',  ( 4.999999999999992006, -8.660254037844389075, -165.7500000000000000 ) ) ;
#32952 = CARTESIAN_POINT ( 'NONE',  ( -9.999999999999227285, -5.773502691896698735, -138.0000000040967620 ) ) ;
#32954 = ORIENTED_EDGE ( 'NONE', *, *, #3225, .T. ) ;
#32953 = CARTESIAN_POINT ( 'NONE',  ( -10.81189881249999729, 6.242252689847871849, -93.90625000204839523 ) ) ;
#32955 = CARTESIAN_POINT ( 'NONE',  ( -5.000000000000003553, -8.660254037844383745, -163.0000000000000000 ) ) ;
#32957 = ORIENTED_EDGE ( 'NONE', *, *, #13792, .F. ) ;
#32956 = CARTESIAN_POINT ( 'NONE',  ( 5.405949406249999534, 9.363379034771803333, -100.0937500020483810 ) ) ;
#32958 = ORIENTED_EDGE ( 'NONE', *, *, #27310, .T. ) ;
#32959 =( BOUNDED_CURVE ( )  B_SPLINE_CURVE ( 2, ( #6794, #16269, #9401, #6171, #19312, #2934, #6382 ),
 .UNSPECIFIED., .F., .F. ) 
 B_SPLINE_CURVE_WITH_KNOTS ( ( 3, 2, 2, 3 ),
 ( 0.5074626865671643117, 0.5087064676616916969, 0.5099502487562189712, 0.5111940298507463565 ),
 .UNSPECIFIED. ) 
 CURVE ( )  GEOMETRIC_REPRESENTATION_ITEM ( )  RATIONAL_B_SPLINE_CURVE ( ( 0.9999999999999880096, 0.8660254037844506980, 1.000000000000000000, 0.8660254037844387076, 1.000000000000000000, 0.8660254037844267172, 1.000000000000011990 ) ) 
 REPRESENTATION_ITEM ( '' )  );
#32960 = ADVANCED_FACE ( 'NONE', ( #6955 ), #20112, .F. ) ;
#32961 = CARTESIAN_POINT ( 'NONE',  ( 10.81189881249999551, -6.242252689847874514, -31.46875000204835260 ) ) ;
#32962 = CARTESIAN_POINT ( 'NONE',  ( 5.405949406249992428, -9.363379034771808662, -22.78125000204836326 ) ) ;
#32963 = CARTESIAN_POINT ( 'NONE',  ( 7.644554776091147741E-16, 12.48450537969573659, -72.96875000204835260 ) ) ;
#32964 = CARTESIAN_POINT ( 'NONE',  ( -9.999999999999998224, 1.224646799147353059E-15, -200.0000000000000000 ) ) ;
#32965 = AXIS2_PLACEMENT_3D ( 'NONE', #29732, #11345, #40903 ) ;
#32966 = AXIS2_PLACEMENT_3D ( 'NONE', #16700, #26021, #20166 ) ;
#32967 = CARTESIAN_POINT ( 'NONE',  ( -5.405949406250003975, -9.363379034771801557, -190.8437500020484094 ) ) ;
#32968 = CARTESIAN_POINT ( 'NONE',  ( -10.81189881249999729, 1.324075727343319199E-15, -149.0937500020483810 ) ) ;
#32969 = CARTESIAN_POINT ( 'NONE',  ( 9.999999999999998224, 0.000000000000000000, -132.8750000040967905 ) ) ;
#32970 = FACE_OUTER_BOUND ( 'NONE', #40050, .T. ) ;
#32971 = CARTESIAN_POINT ( 'NONE',  ( 10.81189881249999729, 0.000000000000000000, -153.0312500020484094 ) ) ;
#32972 = CARTESIAN_POINT ( 'NONE',  ( 9.999999999999996447, -5.773502691896262640, -7.000000004096744277 ) ) ;
#32973 = CARTESIAN_POINT ( 'NONE',  ( -2.121150477449813534E-15, -11.54700538379251284, -80.37499999999997158 ) ) ;
#32974 = CARTESIAN_POINT ( 'NONE',  ( -10.81189881249999729, 6.242252689847871849, -120.7187500020483952 ) ) ;
#32975 = CARTESIAN_POINT ( 'NONE',  ( 10.81189881249999907, 6.242252689847868297, -95.90625000204839523 ) ) ;
#32976 = CARTESIAN_POINT ( 'NONE',  ( -10.81189881249999729, 6.242252689847871849, -107.2187500020483810 ) ) ;
#32977 = CARTESIAN_POINT ( 'NONE',  ( -5.405949406250003975, -9.363379034771801557, -76.84375000204838102 ) ) ;
#32978 = CARTESIAN_POINT ( 'NONE',  ( 5.405949406249999534, 9.363379034771803333, -83.78125000204838102 ) ) ;
#32979 = CARTESIAN_POINT ( 'NONE',  ( -9.999999999999998224, 1.224646799147353059E-15, -163.6250000040967905 ) ) ;
#32980 = CARTESIAN_POINT ( 'NONE',  ( 5.000000000000000000, 8.660254037844385522, -81.62500000409676204 ) ) ;
#32981 = CARTESIAN_POINT ( 'NONE',  ( 5.405949406249992428, -9.363379034771808662, -165.2812500020484094 ) ) ;
#32982 = CARTESIAN_POINT ( 'NONE',  ( -5.405949406249996869, 9.363379034771805109, -182.5312500020484094 ) ) ;
#32983 = CARTESIAN_POINT ( 'NONE',  ( 5.000000000000000000, 8.660254037844385522, -155.1250000040967905 ) ) ;
#32984 = CARTESIAN_POINT ( 'NONE',  ( 7.071067811865472841, 7.071067811865472841, -200.0000000000000000 ) ) ;
#32985 = CARTESIAN_POINT ( 'NONE',  ( 5.405949406249999534, 9.363379034771803333, -7.093750002048371250 ) ) ;
#32986 = CYLINDRICAL_SURFACE ( 'NONE', #15783, 9.999999999999998224 ) ;
#32987 = CARTESIAN_POINT ( 'NONE',  ( 5.405949406249999534, 9.363379034771803333, -115.0937500020483810 ) ) ;
#32988 = EDGE_CURVE ( 'NONE', #6419, #21319, #24409, .T. ) ;
#32989 = CARTESIAN_POINT ( 'NONE',  ( 4.999999999999992006, -8.660254037844389075, -80.24999999999998579 ) ) ;
#32990 = CARTESIAN_POINT ( 'NONE',  ( 10.81189881249999551, -6.242252689847874514, -13.65625000204837036 ) ) ;
#32991 = CARTESIAN_POINT ( 'NONE',  ( -2.121150477449813534E-15, -11.54700538379251284, -86.75000000409677625 ) ) ;
#32992 = LINE ( 'NONE', #42468, #25849 ) ;
#32993 = CARTESIAN_POINT ( 'NONE',  ( -10.81189881249999907, -6.242252689847864744, -105.6562500020483952 ) ) ;
#32994 = CARTESIAN_POINT ( 'NONE',  ( -5.405949406250003975, -9.363379034771801557, -90.53125000204838102 ) ) ;
#32995 = VERTEX_POINT ( 'NONE', #30058 ) ;
#32996 = CARTESIAN_POINT ( 'NONE',  ( 9.999999999999998224, 0.000000000000000000, -86.37500000409677625 ) ) ;
#32997 = FACE_OUTER_BOUND ( 'NONE', #29933, .T. ) ;
#32998 = CARTESIAN_POINT ( 'NONE',  ( 7.644554776091147741E-16, 12.48450537969573659, -39.96875000204835970 ) ) ;
#32999 = VERTEX_POINT ( 'NONE', #42555 ) ;
#33000 = CARTESIAN_POINT ( 'NONE',  ( -10.00000000000000000, -5.773502691896251982, -13.12499999999996625 ) ) ;
#33001 = CARTESIAN_POINT ( 'NONE',  ( -9.999999999999998224, 1.224646799147353059E-15, -145.2500000000000000 ) ) ;
#33002 = FACE_OUTER_BOUND ( 'NONE', #30095, .T. ) ;
#33003 = AXIS2_PLACEMENT_3D ( 'NONE', #10654, #27717, #40423 ) ;
#33004 = CARTESIAN_POINT ( 'NONE',  ( -2.121150477449813534E-15, -11.54700538379251284, -8.750000004096758488 ) ) ;
#33005 = CARTESIAN_POINT ( 'NONE',  ( -5.000000000000003553, -8.660254037844383745, -188.5000000000000000 ) ) ;
#33007 = ORIENTED_EDGE ( 'NONE', *, *, #34654, .F. ) ;
#33006 = CARTESIAN_POINT ( 'NONE',  ( 5.405949406249992428, -9.363379034771808662, -120.2812500020483952 ) ) ;
#33008 = CARTESIAN_POINT ( 'NONE',  ( 0.000000000000000000, 0.000000000000000000, -200.0000000000000000 ) ) ;
#33009 = ORIENTED_EDGE ( 'NONE', *, *, #13755, .F. ) ;
#33010 = CARTESIAN_POINT ( 'NONE',  ( 5.405949406249999534, 9.363379034771803333, -47.78125000204838813 ) ) ;
#33011 = APPROVAL_ROLE ( '' ) ;
#33012 = CARTESIAN_POINT ( 'NONE',  ( 7.644554776091147741E-16, 12.48450537969573659, -96.96875000204838102 ) ) ;
#33013 = CARTESIAN_POINT ( 'NONE',  ( -2.293366432827344421E-15, -12.48450537969573659, -121.9062500020483952 ) ) ;
#33014 = VERTEX_POINT ( 'NONE', #26596 ) ;
#33015 = CARTESIAN_POINT ( 'NONE',  ( 4.999999999999992006, -8.660254037844389075, -85.12500000409677625 ) ) ;
#33016 = PLANE ( 'NONE',  #30467 ) ;
#33017 = CARTESIAN_POINT ( 'NONE',  ( -5.405949406249996869, 9.363379034771805109, -184.0312500020484094 ) ) ;
#33018 = DIRECTION ( 'NONE',  ( 1.000000000000000000, 0.000000000000000000, 0.000000000000000000 ) ) ;
#33019 = CARTESIAN_POINT ( 'NONE',  ( 10.81189881249999729, 0.000000000000000000, -130.3437500020484094 ) ) ;
#33020 = VECTOR ( 'NONE', #537, 1000.000000000000000 ) ;
#33021 = CARTESIAN_POINT ( 'NONE',  ( -2.293366432827344421E-15, -12.48450537969573659, -102.2187500020483952 ) ) ;
#33022 = LINE ( 'NONE', #5848, #2900 ) ;
#33023 = CARTESIAN_POINT ( 'NONE',  ( 5.405949406249992428, -9.363379034771808662, -111.2812500020483810 ) ) ;
#33024 = CARTESIAN_POINT ( 'NONE',  ( 10.00000000000000000, 5.773502691896255534, -182.2500000040968189 ) ) ;
#33025 = CARTESIAN_POINT ( 'NONE',  ( 5.405949406249999534, 9.363379034771803333, -115.0937500020483810 ) ) ;
#33026 = CARTESIAN_POINT ( 'NONE',  ( 10.81189881249999729, 6.242252689847867408, -182.9062500020484094 ) ) ;
#33027 = CARTESIAN_POINT ( 'NONE',  ( -4.999999999999996447, 8.660254037844387298, -6.375000004096770034 ) ) ;
#33028 = CARTESIAN_POINT ( 'NONE',  ( 0.000000000000000000, 0.000000000000000000, -200.0000000000000000 ) ) ;
#33029 = CARTESIAN_POINT ( 'NONE',  ( -5.000000000000003553, -8.660254037844383745, -133.0000000000000000 ) ) ;
#33030 = CARTESIAN_POINT ( 'NONE',  ( 9.999999999999998224, 0.000000000000000000, -6.499999999999977796 ) ) ;
#33031 = CARTESIAN_POINT ( 'NONE',  ( 5.405949406249999534, 9.363379034771803333, -56.59375000204835970 ) ) ;
#33032 = AXIS2_PLACEMENT_3D ( 'NONE', #36632, #614, #4683 ) ;
#33033 = CARTESIAN_POINT ( 'NONE',  ( 5.405949406249999534, 9.363379034771803333, -46.09375000204838102 ) ) ;
#33034 = CARTESIAN_POINT ( 'NONE',  ( 5.000000000000000000, 8.660254037844385522, -180.6250000040967905 ) ) ;
#33035 = CARTESIAN_POINT ( 'NONE',  ( -10.81189881249999729, 6.242252689847871849, -21.90625000204837036 ) ) ;
#33036 = CARTESIAN_POINT ( 'NONE',  ( -10.81189881249999907, -6.242252689847864744, -28.96875000204835260 ) ) ;
#33037 = CARTESIAN_POINT ( 'NONE',  ( 9.999999999999998224, 0.000000000000000000, -149.3750000040967905 ) ) ;
#33038 = CARTESIAN_POINT ( 'NONE',  ( 10.81189881249999907, 6.242252689847868297, -140.7187500020483810 ) ) ;
#33039 = EDGE_CURVE ( 'NONE', #1917, #31885, #17429, .T. ) ;
#33040 = CARTESIAN_POINT ( 'NONE',  ( -4.999999999999996447, 8.660254037844387298, -104.9999999999999858 ) ) ;
#33041 = CARTESIAN_POINT ( 'NONE',  ( 10.81189881249999729, 0.000000000000000000, -36.03125000204837391 ) ) ;
#33042 = DIRECTION ( 'NONE',  ( -0.000000000000000000, -0.000000000000000000, -1.000000000000000000 ) ) ;
#33043 = ADVANCED_FACE ( 'NONE', ( #29626 ), #36097, .T. ) ;
#33044 = CARTESIAN_POINT ( 'NONE',  ( -2.121150477449813534E-15, -11.54700538379251284, -63.87499999999999289 ) ) ;
#33045 = CARTESIAN_POINT ( 'NONE',  ( -5.405949406250003975, -9.363379034771801557, -129.5312500020484094 ) ) ;
#33046 = CARTESIAN_POINT ( 'NONE',  ( -5.405949406249996869, 9.363379034771805109, -113.5312500020483952 ) ) ;
#33047 = VERTEX_POINT ( 'NONE', #26809 ) ;
#33048 = VECTOR ( 'NONE', #7119, 1000.000000000000000 ) ;
#33049 = CARTESIAN_POINT ( 'NONE',  ( -4.999999999999996447, 8.660254037844387298, -142.5000000000000000 ) ) ;
#33050 = CARTESIAN_POINT ( 'NONE',  ( 4.999999999999992006, -8.660254037844389075, -107.6250000040967763 ) ) ;
#33051 = CARTESIAN_POINT ( 'NONE',  ( -5.000000000000003553, -8.660254037844383745, -194.8750000040967905 ) ) ;
#33052 = CARTESIAN_POINT ( 'NONE',  ( 5.405949406249992428, -9.363379034771808662, -63.09375000204836681 ) ) ;
#33053 = ORIENTED_EDGE ( 'NONE', *, *, #27535, .T. ) ;
#33054 = CARTESIAN_POINT ( 'NONE',  ( 7.070501591499377789E-16, 11.54700538379251284, -33.12499999999996447 ) ) ;
#33055 = CARTESIAN_POINT ( 'NONE',  ( -9.999999999999998224, 5.773502691896259087, -18.25000000409676559 ) ) ;
#33056 = CARTESIAN_POINT ( 'NONE',  ( -2.293366432827344421E-15, -12.48450537969573659, -46.90625000204836681 ) ) ;
#33057 = CARTESIAN_POINT ( 'NONE',  ( -2.121150477449813534E-15, -11.54700538379251284, -2.374999999999946709 ) ) ;
#33058 = CARTESIAN_POINT ( 'NONE',  ( -9.999999999999998224, 5.773502691896259087, -34.75000000409674783 ) ) ;
#33059 = CARTESIAN_POINT ( 'NONE',  ( 9.999999999999998224, 0.000000000000000000, -117.8750000040967905 ) ) ;
#33060 = CARTESIAN_POINT ( 'NONE',  ( 10.81189881249999907, 6.242252689847868297, -145.4062500020484094 ) ) ;
#33061 = EDGE_CURVE ( 'NONE', #30831, #16772, #6114, .T. ) ;
#33062 = CYLINDRICAL_SURFACE ( 'NONE', #18994, 9.999999999999998224 ) ;
#33063 = ORIENTED_EDGE ( 'NONE', *, *, #5029, .F. ) ;
#33064 = ORIENTED_EDGE ( 'NONE', *, *, #15100, .F. ) ;
#33065 = VERTEX_POINT ( 'NONE', #10391 ) ;
#33066 = EDGE_CURVE ( 'NONE', #36083, #35300, #20258, .T. ) ;
#33067 = CARTESIAN_POINT ( 'NONE',  ( 9.999999999999998224, 0.000000000000000000, -129.5000000000000000 ) ) ;
#33068 = CARTESIAN_POINT ( 'NONE',  ( -10.81189881249999729, 6.242252689847871849, -171.7187500020483810 ) ) ;
#33069 = CARTESIAN_POINT ( 'NONE',  ( 10.81189881249999907, 6.242252689847868297, -26.71875000204838102 ) ) ;
#33070 = CARTESIAN_POINT ( 'NONE',  ( -9.999999999999998224, 1.224646799147353059E-15, -168.1250000040967905 ) ) ;
#33071 = CARTESIAN_POINT ( 'NONE',  ( -10.81189881249999729, 1.324075727343319199E-15, -158.0937500020483810 ) ) ;
#33072 = CARTESIAN_POINT ( 'NONE',  ( 5.405949406249999534, 9.363379034771803333, -148.0937500020483810 ) ) ;
#33073 = CARTESIAN_POINT ( 'NONE',  ( 9.999999999999998224, 0.000000000000000000, -9.499999999999953815 ) ) ;
#33074 = CARTESIAN_POINT ( 'NONE',  ( 10.81189881249999551, -6.242252689847874514, -124.4687500020483952 ) ) ;
#33075 = CARTESIAN_POINT ( 'NONE',  ( -10.81189881249999729, 6.242252689847871849, -129.9062500020483810 ) ) ;
#33077 = CARTESIAN_POINT ( 'NONE',  ( 10.81189881249999551, -6.242252689847874514, -10.46875000204836503 ) ) ;
#33076 =( BOUNDED_CURVE ( )  B_SPLINE_CURVE ( 2, ( #25636, #38795, #9222, #22390, #15884, #12652, #38999 ),
 .UNSPECIFIED., .F., .F. ) 
 B_SPLINE_CURVE_WITH_KNOTS ( ( 3, 2, 2, 3 ),
 ( 0.8059701492537315604, 0.8072139303482589456, 0.8084577114427863309, 0.8097014925373136052 ),
 .UNSPECIFIED. ) 
 CURVE ( )  GEOMETRIC_REPRESENTATION_ITEM ( )  RATIONAL_B_SPLINE_CURVE ( ( 0.9999999999999761302, 0.8660254037844625774, 1.000000000000000000, 0.8660254037844387076, 1.000000000000000000, 0.8660254037844148378, 1.000000000000023981 ) ) 
 REPRESENTATION_ITEM ( '' )  );
#33078 = CARTESIAN_POINT ( 'NONE',  ( 10.81189881249999729, 6.242252689847867408, -142.2187500020483810 ) ) ;
#33079 = LINE ( 'NONE', #20965, #37111 ) ;
#33080 = CARTESIAN_POINT ( 'NONE',  ( -10.00000000000038547, 5.773502691896036154, -182.8750000000000000 ) ) ;
#33081 = CARTESIAN_POINT ( 'NONE',  ( 9.999999999999998224, 0.000000000000000000, -165.5000000000000000 ) ) ;
#33082 = CARTESIAN_POINT ( 'NONE',  ( 0.000000000000000000, 0.000000000000000000, -99.99999999999998579 ) ) ;
#33083 = CARTESIAN_POINT ( 'NONE',  ( -10.81189881249999729, 1.324075727343319199E-15, -74.09375000204838102 ) ) ;
#33084 = CARTESIAN_POINT ( 'NONE',  ( -10.81189881249999729, 6.242252689847871849, -41.40625000204836681 ) ) ;
#33085 = CARTESIAN_POINT ( 'NONE',  ( 5.405949406249992428, -9.363379034771808662, -52.59375000204835260 ) ) ;
#33086 = DIRECTION ( 'NONE',  ( -0.000000000000000000, -0.000000000000000000, -1.000000000000000000 ) ) ;
#33087 = CARTESIAN_POINT ( 'NONE',  ( -5.405949406249996869, 9.363379034771805109, -162.8437500020484094 ) ) ;
#33088 = ADVANCED_FACE ( 'NONE', ( #9762 ), #16643, .T. ) ;
#33089 = CARTESIAN_POINT ( 'NONE',  ( -9.999999999999998224, 1.224646799147353059E-15, -131.7499999999999716 ) ) ;
#33090 = CARTESIAN_POINT ( 'NONE',  ( -10.81189881249999729, 1.324075727343319199E-15, -141.7812500020483810 ) ) ;
#33091 = CYLINDRICAL_SURFACE ( 'NONE', #2062, 9.999999999999998224 ) ;
#33092 = CARTESIAN_POINT ( 'NONE',  ( -9.999999999999998224, 1.224646799147353059E-15, -115.6250000040967905 ) ) ;
#33093 = CARTESIAN_POINT ( 'NONE',  ( -5.000000000000003553, -8.660254037844383745, -90.99999999999998579 ) ) ;
#33094 = ADVANCED_FACE ( 'NONE', ( #3506 ), #26386, .F. ) ;
#33095 = VERTEX_POINT ( 'NONE', #19895 ) ;
#33096 =( BOUNDED_CURVE ( )  B_SPLINE_CURVE ( 2, ( #17446, #14198, #13984, #34093, #30642, #31074, #27181 ),
 .UNSPECIFIED., .F., .F. ) 
 B_SPLINE_CURVE_WITH_KNOTS ( ( 3, 2, 2, 3 ),
 ( 0.2276119402985075368, 0.2288557213930349221, 0.2300995024875622796, 0.2313432835820896372 ),
 .UNSPECIFIED. ) 
 CURVE ( )  GEOMETRIC_REPRESENTATION_ITEM ( )  RATIONAL_B_SPLINE_CURVE ( ( 0.9999999999999910072, 0.8660254037844477004, 1.000000000000000000, 0.8660254037844387076, 1.000000000000000000, 0.8660254037844297148, 1.000000000000008882 ) ) 
 REPRESENTATION_ITEM ( '' )  );
#33097 = CARTESIAN_POINT ( 'NONE',  ( -10.81189881249999729, 6.242252689847871849, -111.9062500020483810 ) ) ;
#33098 = CARTESIAN_POINT ( 'NONE',  ( 9.999999999999998224, 0.000000000000000000, -128.3750000040967905 ) ) ;
#33099 = CARTESIAN_POINT ( 'NONE',  ( 23.09401076758504345, 1.040834085586084257E-14, 0.000000000000000000 ) ) ;
#33100 = AXIS2_PLACEMENT_3D ( 'NONE', #29979, #10526, #14169 ) ;
#33101 = EDGE_CURVE ( 'NONE', #35132, #36368, #33079, .T. ) ;
#33102 = CARTESIAN_POINT ( 'NONE',  ( -5.405949406250003975, -9.363379034771801557, -162.5312500020484094 ) ) ;
#33103 = CARTESIAN_POINT ( 'NONE',  ( 10.00000000000000000, 5.773502691896255534, -42.75000000409675494 ) ) ;
#33104 = CARTESIAN_POINT ( 'NONE',  ( 9.999999999999998224, 0.000000000000000000, -200.0000000000000000 ) ) ;
#33105 = CC_DESIGN_PERSON_AND_ORGANIZATION_ASSIGNMENT ( #23618, #32485, ( #2849 ) ) ;
#33106 = CARTESIAN_POINT ( 'NONE',  ( -10.81189881249999729, 6.242252689847871849, -53.40625000204837391 ) ) ;
#33107 =( BOUNDED_CURVE ( )  B_SPLINE_CURVE ( 2, ( #40451, #7895, #20397, #27959, #11320, #10895, #13909 ),
 .UNSPECIFIED., .F., .F. ) 
 B_SPLINE_CURVE_WITH_KNOTS ( ( 3, 2, 2, 3 ),
 ( 0.5559701492537315604, 0.5572139303482589456, 0.5584577114427863309, 0.5597014925373136052 ),
 .UNSPECIFIED. ) 
 CURVE ( )  GEOMETRIC_REPRESENTATION_ITEM ( )  RATIONAL_B_SPLINE_CURVE ( ( 0.9999999999999761302, 0.8660254037844625774, 1.000000000000000000, 0.8660254037844387076, 1.000000000000000000, 0.8660254037844148378, 1.000000000000023981 ) ) 
 REPRESENTATION_ITEM ( '' )  );
#33108 = DIRECTION ( 'NONE',  ( -0.000000000000000000, -0.000000000000000000, -1.000000000000000000 ) ) ;
#33109 = CARTESIAN_POINT ( 'NONE',  ( 10.81189881249999551, -6.242252689847874514, -163.6562500020484094 ) ) ;
#33110 = CARTESIAN_POINT ( 'NONE',  ( 5.405949406249999534, 9.363379034771803333, -137.5937500020483810 ) ) ;
#33111 = DIRECTION ( 'NONE',  ( -0.000000000000000000, -0.000000000000000000, 1.000000000000000000 ) ) ;
#33112 = DIRECTION ( 'NONE',  ( -0.000000000000000000, -0.000000000000000000, 1.000000000000000000 ) ) ;
#33113 = VERTEX_POINT ( 'NONE', #7816 ) ;
#33114 = LINE ( 'NONE', #13225, #38992 ) ;
#33115 = EDGE_CURVE ( 'NONE', #14748, #32646, #23249, .T. ) ;
#33117 = ORIENTED_EDGE ( 'NONE', *, *, #31227, .F. ) ;
#33116 = CARTESIAN_POINT ( 'NONE',  ( -5.405949406249996869, 9.363379034771805109, -68.53125000204838102 ) ) ;
#33118 = PERSON_AND_ORGANIZATION ( #11915, #17965 ) ;
#33120 = ORIENTED_EDGE ( 'NONE', *, *, #12971, .F. ) ;
#33119 = CARTESIAN_POINT ( 'NONE',  ( -10.81189881249999907, -6.242252689847864744, -117.4687500020483952 ) ) ;
#33121 = ORIENTED_EDGE ( 'NONE', *, *, #35195, .F. ) ;
#33122 = CARTESIAN_POINT ( 'NONE',  ( -5.405949406249996869, 9.363379034771805109, -23.34375000204835970 ) ) ;
#33123 = CARTESIAN_POINT ( 'NONE',  ( 5.405949406249999534, 9.363379034771803333, 0.2187499979516283055 ) ) ;
#33124 = VECTOR ( 'NONE', #42644, 1000.000000000000000 ) ;
#33125 = CARTESIAN_POINT ( 'NONE',  ( -10.81189881249999729, 6.242252689847871849, -45.71875000204837391 ) ) ;
#33126 = CARTESIAN_POINT ( 'NONE',  ( 4.999999999999992006, -8.660254037844389075, -71.62500000409677625 ) ) ;
#33127 = CARTESIAN_POINT ( 'NONE',  ( 9.999999999999998224, 0.000000000000000000, -28.99999999999997158 ) ) ;
#33128 = CARTESIAN_POINT ( 'NONE',  ( -10.81189881249999729, -6.242252689847864744, -181.9687500020484094 ) ) ;
#33129 = CARTESIAN_POINT ( 'NONE',  ( -10.81189881249999907, -6.242252689847864744, -169.9687500020484094 ) ) ;
#33130 = CARTESIAN_POINT ( 'NONE',  ( 10.81189881249999907, 6.242252689847868297, -149.7187500020483810 ) ) ;
#33131 = CARTESIAN_POINT ( 'NONE',  ( 10.81189881249999551, -6.242252689847874514, -161.9687500020484094 ) ) ;
#33132 = CARTESIAN_POINT ( 'NONE',  ( 9.999999999999998224, 0.000000000000000000, -200.0000000000000000 ) ) ;
#33133 = CARTESIAN_POINT ( 'NONE',  ( 5.000000000000000000, 8.660254037844385522, -188.1250000040967905 ) ) ;
#33134 = CARTESIAN_POINT ( 'NONE',  ( -5.000000000000003553, -8.660254037844383745, -185.5000000000000000 ) ) ;
#33135 = CARTESIAN_POINT ( 'NONE',  ( -10.81189881249999907, -6.242252689847864744, -94.96875000204838102 ) ) ;
#33136 = CARTESIAN_POINT ( 'NONE',  ( -4.999999999999996447, 8.660254037844387298, -138.0000000000000000 ) ) ;
#33137 = CARTESIAN_POINT ( 'NONE',  ( -10.81189881249999907, -6.242252689847864744, -66.65625000204839523 ) ) ;
#33138 = CARTESIAN_POINT ( 'NONE',  ( -9.999999999999742428, -5.773502691896402084, -160.1250000000000284 ) ) ;
#33139 = CARTESIAN_POINT ( 'NONE',  ( 10.81189881249999551, -6.242252689847874514, -185.9687500020484094 ) ) ;
#33140 = CARTESIAN_POINT ( 'NONE',  ( 7.644554776091147741E-16, 12.48450537969573659, -125.6562500020483810 ) ) ;
#33141 = CARTESIAN_POINT ( 'NONE',  ( -5.405949406250003975, -9.363379034771801557, -161.0312500020484094 ) ) ;
#33142 = CARTESIAN_POINT ( 'NONE',  ( 7.644554776091147741E-16, 12.48450537969573659, -53.65625000204838102 ) ) ;
#33143 = CARTESIAN_POINT ( 'NONE',  ( 10.00000000000000000, 5.773502691896255534, -134.2500000040967905 ) ) ;
#33144 = CARTESIAN_POINT ( 'NONE',  ( 7.070501591499377789E-16, 11.54700538379251284, -114.1249999999999858 ) ) ;
#33145 = ORIENTED_EDGE ( 'NONE', *, *, #19044, .F. ) ;
#33146 = CARTESIAN_POINT ( 'NONE',  ( 10.81189881249999729, 0.000000000000000000, -136.5312500020484094 ) ) ;
#33147 = CARTESIAN_POINT ( 'NONE',  ( -2.293366432827344421E-15, -12.48450537969573659, -147.4062500020483810 ) ) ;
#33148 = CARTESIAN_POINT ( 'NONE',  ( 10.81189881249999729, 0.000000000000000000, -186.0312500020484094 ) ) ;
#33149 = CARTESIAN_POINT ( 'NONE',  ( 9.999999999999998224, 0.000000000000000000, -131.3750000040967905 ) ) ;
#33150 = CARTESIAN_POINT ( 'NONE',  ( -2.293366432827344421E-15, -12.48450537969573659, -82.71875000204838102 ) ) ;
#33151 = ORIENTED_EDGE ( 'NONE', *, *, #27689, .T. ) ;
#33152 = CARTESIAN_POINT ( 'NONE',  ( 4.999999999999992006, -8.660254037844389075, -60.74999999999997158 ) ) ;
#33153 = CARTESIAN_POINT ( 'NONE',  ( 5.405949406249992428, -9.363379034771808662, -177.0937500020484094 ) ) ;
#33154 = CARTESIAN_POINT ( 'NONE',  ( 10.00000000000000000, 5.773502691896255534, -65.25000000409677625 ) ) ;
#33155 = CARTESIAN_POINT ( 'NONE',  ( -10.00000000000102496, 5.773502691895664007, -21.25000000409673362 ) ) ;
#33156 = DIRECTION ( 'NONE',  ( -0.000000000000000000, -0.000000000000000000, 1.000000000000000000 ) ) ;
#33157 = CARTESIAN_POINT ( 'NONE',  ( -10.81189881249999907, -6.242252689847864744, -81.65625000204839523 ) ) ;
#33158 = CARTESIAN_POINT ( 'NONE',  ( -5.405949406249996869, 9.363379034771805109, -56.53125000204836681 ) ) ;
#33159 = CARTESIAN_POINT ( 'NONE',  ( 9.999999999999998224, 0.000000000000000000, -63.87500000409676915 ) ) ;
#33160 = CARTESIAN_POINT ( 'NONE',  ( -10.81189881249999729, 6.242252689847871849, -18.71875000204837036 ) ) ;
#33161 = LINE ( 'NONE', #152, #78 ) ;
#33162 = CARTESIAN_POINT ( 'NONE',  ( 5.405949406249999534, 9.363379034771803333, -185.7812500020484094 ) ) ;
#33163 = CC_DESIGN_APPROVAL ( #42283, ( #15921 ) ) ;
#33164 = ADVANCED_FACE ( 'NONE', ( #11243 ), #27451, .T. ) ;
#33165 = CARTESIAN_POINT ( 'NONE',  ( 10.81189881249999729, 0.000000000000000000, -12.03125000204835438 ) ) ;
#33166 = DIRECTION ( 'NONE',  ( 0.000000000000000000, 0.000000000000000000, -1.000000000000000000 ) ) ;
#33167 = CARTESIAN_POINT ( 'NONE',  ( -42.00000000000004974, 5.143516556418889633E-15, -219.9999999999999716 ) ) ;
#33168 = CARTESIAN_POINT ( 'NONE',  ( -9.999999999999998224, 1.224646799147353059E-15, -114.1250000040967763 ) ) ;
#33169 = CARTESIAN_POINT ( 'NONE',  ( 5.500000000000000888, -20.00000000000000000, -232.0000000000000000 ) ) ;
#33170 = CARTESIAN_POINT ( 'NONE',  ( -10.00000000000000000, -5.773502691896251982, -169.1249999999999716 ) ) ;
#33171 = CARTESIAN_POINT ( 'NONE',  ( -2.121150477449813534E-15, -11.54700538379251284, -137.7500000040967905 ) ) ;
#33173 = ORIENTED_EDGE ( 'NONE', *, *, #9863, .T. ) ;
#33172 = CARTESIAN_POINT ( 'NONE',  ( 10.81189881249999551, -6.242252689847874514, -96.15625000204838102 ) ) ;
#33174 = DIRECTION ( 'NONE',  ( -0.000000000000000000, -0.000000000000000000, -1.000000000000000000 ) ) ;
#33176 = VERTEX_POINT ( 'NONE', #17284 ) ;
#33175 = CARTESIAN_POINT ( 'NONE',  ( -2.293366432827344421E-15, -12.48450537969573659, -100.7187500020483952 ) ) ;
#33177 =( BOUNDED_CURVE ( )  B_SPLINE_CURVE ( 2, ( #39633, #12874, #20214, #36829, #6844, #26697, #36410 ),
 .UNSPECIFIED., .F., .F. ) 
 B_SPLINE_CURVE_WITH_KNOTS ( ( 3, 2, 2, 3 ),
 ( 0.4328358208955225273, 0.4340796019900499125, 0.4353233830845772978, 0.4365671641791046276 ),
 .UNSPECIFIED. ) 
 CURVE ( )  GEOMETRIC_REPRESENTATION_ITEM ( )  RATIONAL_B_SPLINE_CURVE ( ( 0.9999999999999820144, 0.8660254037844566932, 1.000000000000000000, 0.8660254037844387076, 1.000000000000000000, 0.8660254037844207220, 1.000000000000017986 ) ) 
 REPRESENTATION_ITEM ( '' )  );
#33178 = ORIENTED_EDGE ( 'NONE', *, *, #8857, .T. ) ;
#33179 = CARTESIAN_POINT ( 'NONE',  ( 5.405949406249992428, -9.363379034771808662, -36.09375000204836681 ) ) ;
#33180 = CARTESIAN_POINT ( 'NONE',  ( -10.81189881249999729, 6.242252689847871849, -18.90625000204837391 ) ) ;
#33181 = SECURITY_CLASSIFICATION_LEVEL ( 'unclassified' ) ;
#33182 = CARTESIAN_POINT ( 'NONE',  ( 5.405949406249992428, -9.363379034771808662, -69.09375000204836681 ) ) ;
#33183 = CARTESIAN_POINT ( 'NONE',  ( 0.000000000000000000, 20.00000000000000000, -235.0000000000000000 ) ) ;
#33184 = CARTESIAN_POINT ( 'NONE',  ( -2.293366432827344421E-15, -12.48450537969573659, -189.2187500020484094 ) ) ;
#33185 = CARTESIAN_POINT ( 'NONE',  ( -10.81189881249999907, -6.242252689847864744, -153.4687500020484094 ) ) ;
#33186 = AXIS2_PLACEMENT_3D ( 'NONE', #32679, #13001, #9784 ) ;
#33187 = CARTESIAN_POINT ( 'NONE',  ( 0.000000000000000000, 0.000000000000000000, -200.0000000000000000 ) ) ;
#33188 = CARTESIAN_POINT ( 'NONE',  ( -4.999999999999996447, 8.660254037844387298, -172.5000000000000284 ) ) ;
#33189 = CARTESIAN_POINT ( 'NONE',  ( -10.81189881249999729, 6.242252689847871849, -147.9062500020483810 ) ) ;
#33190 = CARTESIAN_POINT ( 'NONE',  ( 5.000000000000000000, 8.660254037844385522, -5.125000004096769146 ) ) ;
#33191 = CARTESIAN_POINT ( 'NONE',  ( 9.999999999999479527, 5.773502691896553074, -178.8749999999999716 ) ) ;
#33192 = APPROVAL_PERSON_ORGANIZATION ( #35409, #12231, #22441 ) ;
#33193 = CARTESIAN_POINT ( 'NONE',  ( -5.405949406250003975, -9.363379034771801557, -124.8437500020483810 ) ) ;
#33194 = CARTESIAN_POINT ( 'NONE',  ( -4.999999999999996447, 8.660254037844387298, -14.99999999999995737 ) ) ;
#33195 = CARTESIAN_POINT ( 'NONE',  ( -5.405949406250003975, -9.363379034771801557, -92.03125000204838102 ) ) ;
#33196 = CARTESIAN_POINT ( 'NONE',  ( -2.293366432827344421E-15, -12.48450537969573659, -109.7187500020483668 ) ) ;
#33197 = CARTESIAN_POINT ( 'NONE',  ( -5.405949406250003975, -9.363379034771801557, -70.84375000204836681 ) ) ;
#33198 = CARTESIAN_POINT ( 'NONE',  ( -5.405949406249996869, 9.363379034771805109, -77.53125000204838102 ) ) ;
#33199 = CARTESIAN_POINT ( 'NONE',  ( -2.121150477449813534E-15, -11.54700538379251284, -160.2500000040967620 ) ) ;
#33200 = DIRECTION ( 'NONE',  ( -1.000000000000000000, 0.000000000000000000, 0.000000000000000000 ) ) ;
#33201 = CARTESIAN_POINT ( 'NONE',  ( -2.293366432827344421E-15, -12.48450537969573659, -162.4062500020483810 ) ) ;
#33202 = CARTESIAN_POINT ( 'NONE',  ( -10.81189881249999907, -6.242252689847864744, -168.6562500020483810 ) ) ;
#33203 = VECTOR ( 'NONE', #22714, 1000.000000000000000 ) ;
#33204 = LINE ( 'NONE', #10088, #7040 ) ;
#33205 = CARTESIAN_POINT ( 'NONE',  ( -5.405949406250003975, -9.363379034771801557, -4.843750002048369474 ) ) ;
#33206 = CARTESIAN_POINT ( 'NONE',  ( -4.999999999999996447, 8.660254037844387298, -108.3750000040967763 ) ) ;
#33207 = CARTESIAN_POINT ( 'NONE',  ( 10.81189881249999551, -6.242252689847874514, -104.9687500020483810 ) ) ;
#33208 = CARTESIAN_POINT ( 'NONE',  ( 4.999999999999992006, -8.660254037844389075, -83.24999999999997158 ) ) ;
#33209 = CARTESIAN_POINT ( 'NONE',  ( 10.81189881249999551, -6.242252689847874514, -15.15625000204837036 ) ) ;
#33210 = CARTESIAN_POINT ( 'NONE',  ( -9.999999999999998224, 1.224646799147353059E-15, -91.62500000409677625 ) ) ;
#33211 = CARTESIAN_POINT ( 'NONE',  ( 0.000000000000000000, 0.000000000000000000, -200.0000000000000000 ) ) ;
#33212 = CARTESIAN_POINT ( 'NONE',  ( 5.405949406249999534, 9.363379034771803333, -104.7812500020483810 ) ) ;
#33213 = CARTESIAN_POINT ( 'NONE',  ( 5.405949406249992428, -9.363379034771808662, -82.78125000204838102 ) ) ;
#33214 = ORIENTED_EDGE ( 'NONE', *, *, #3533, .T. ) ;
#33215 = CARTESIAN_POINT ( 'NONE',  ( -5.000000000000003553, -8.660254037844383745, -83.87500000409677625 ) ) ;
#33216 = CARTESIAN_POINT ( 'NONE',  ( 5.000000000000000000, 8.660254037844385522, -134.1250000040967620 ) ) ;
#33217 = CARTESIAN_POINT ( 'NONE',  ( -5.405949406250003975, -9.363379034771801557, -45.34375000204838102 ) ) ;
#33218 = ORIENTED_EDGE ( 'NONE', *, *, #17476, .T. ) ;
#33219 = CARTESIAN_POINT ( 'NONE',  ( -9.999999999999998224, 1.224646799147353059E-15, -8.749999999999952038 ) ) ;
#33220 = CARTESIAN_POINT ( 'NONE',  ( -4.999999999999996447, 8.660254037844387298, -145.5000000000000000 ) ) ;
#33221 = CARTESIAN_POINT ( 'NONE',  ( -9.999999999999479527, -5.773502691896549521, -32.62499999999994316 ) ) ;
#33222 = CARTESIAN_POINT ( 'NONE',  ( 9.999999999999996447, -5.773502691896262640, -16.00000000409676559 ) ) ;
#33223 = AXIS2_PLACEMENT_3D ( 'NONE', #23448, #13065, #16729 ) ;
#33224 =( BOUNDED_CURVE ( )  B_SPLINE_CURVE ( 2, ( #329, #10226, #544, #36145, #17119, #6576, #33554 ),
 .UNSPECIFIED., .F., .F. ) 
 B_SPLINE_CURVE_WITH_KNOTS ( ( 3, 2, 2, 3 ),
 ( 0.4664179104477613191, 0.4676616915422886489, 0.4689054726368160342, 0.4701492537313434195 ),
 .UNSPECIFIED. ) 
 CURVE ( )  GEOMETRIC_REPRESENTATION_ITEM ( )  RATIONAL_B_SPLINE_CURVE ( ( 0.9999999999999880096, 0.8660254037844506980, 1.000000000000000000, 0.8660254037844387076, 1.000000000000000000, 0.8660254037844267172, 1.000000000000011990 ) ) 
 REPRESENTATION_ITEM ( '' )  );
#33225 = LOCAL_TIME ( 11, 57, 6.000000000000000000, #35782 ) ;
#33226 = CARTESIAN_POINT ( 'NONE',  ( -10.00000000000000000, -5.773502691896251982, -193.1250000000000284 ) ) ;
#33227 = LINE ( 'NONE', #36447, #16481 ) ;
#33229 = VERTEX_POINT ( 'NONE', #4568 ) ;
#33228 = CARTESIAN_POINT ( 'NONE',  ( -5.405949406249996869, 9.363379034771805109, -121.0312500020483952 ) ) ;
#33230 = DIRECTION ( 'NONE',  ( 1.000000000000000000, 0.000000000000000000, 0.000000000000000000 ) ) ;
#33231 = EDGE_CURVE ( 'NONE', #37987, #34935, #30489, .T. ) ;
#33232 = ORIENTED_EDGE ( 'NONE', *, *, #12215, .T. ) ;
#33233 = CARTESIAN_POINT ( 'NONE',  ( -10.81189881249999729, 6.242252689847871849, -47.40625000204835970 ) ) ;
#33234 = PERSON_AND_ORGANIZATION ( #11915, #17965 ) ;
#33235 = AXIS2_PLACEMENT_3D ( 'NONE', #9481, #31958, #22650 ) ;
#33236 = CARTESIAN_POINT ( 'NONE',  ( -5.405949406249996869, 9.363379034771805109, -95.34375000204838102 ) ) ;
#33237 = CARTESIAN_POINT ( 'NONE',  ( 10.81189881249999729, 0.000000000000000000, -123.0312500020483952 ) ) ;
#33238 = EDGE_LOOP ( 'NONE', ( #26373, #11276, #31953, #28729 ) ) ;
#33239 = FACE_OUTER_BOUND ( 'NONE', #9437, .T. ) ;
#33240 = CARTESIAN_POINT ( 'NONE',  ( 9.999999999999742428, 5.773502691896404748, -128.2500000040967905 ) ) ;
#33241 = CARTESIAN_POINT ( 'NONE',  ( 5.405949406249992428, -9.363379034771808662, -175.7812500020484094 ) ) ;
#33242 = DIRECTION ( 'NONE',  ( 0.000000000000000000, -0.000000000000000000, -1.000000000000000000 ) ) ;
#33243 = CARTESIAN_POINT ( 'NONE',  ( -10.81189881249999729, 1.324075727343319199E-15, -134.0937500020483810 ) ) ;
#33244 = CARTESIAN_POINT ( 'NONE',  ( -5.405949406249996869, 9.363379034771805109, -98.34375000204838102 ) ) ;
#33245 = CARTESIAN_POINT ( 'NONE',  ( 9.999999999999227285, 5.773502691896701400, -106.8749999999999432 ) ) ;
#33246 = CARTESIAN_POINT ( 'NONE',  ( 10.81189881249999907, 6.242252689847868297, -106.4062500020483952 ) ) ;
#33247 = CARTESIAN_POINT ( 'NONE',  ( 10.00000000000000000, 5.773502691896255534, -185.2500000040967905 ) ) ;
#33248 = CARTESIAN_POINT ( 'NONE',  ( 10.81189881249999729, 0.000000000000000000, -116.8437500020483810 ) ) ;
#33249 = AXIS2_PLACEMENT_3D ( 'NONE', #33814, #27759, #21274 ) ;
#33250 = CARTESIAN_POINT ( 'NONE',  ( -10.81189881249999729, 1.324075727343319199E-15, -185.2812500020484094 ) ) ;
#33251 = CARTESIAN_POINT ( 'NONE',  ( 9.999999999999998224, 0.000000000000000000, -122.0000000000000000 ) ) ;
#33252 = FACE_OUTER_BOUND ( 'NONE', #24207, .T. ) ;
#33253 = CARTESIAN_POINT ( 'NONE',  ( -4.999999999999996447, 8.660254037844387298, -133.5000000000000000 ) ) ;
#33254 = CARTESIAN_POINT ( 'NONE',  ( 9.999999999999998224, 0.000000000000000000, -1.999999999999974021 ) ) ;
#33255 = CARTESIAN_POINT ( 'NONE',  ( -2.293366432827344421E-15, -12.48450537969573659, -58.71875000204836681 ) ) ;
#33256 = CARTESIAN_POINT ( 'NONE',  ( -10.81189881249999729, 6.242252689847871849, -45.71875000204837391 ) ) ;
#33257 = CARTESIAN_POINT ( 'NONE',  ( -5.000000000000003553, -8.660254037844383745, -182.8750000040967905 ) ) ;
#33258 = CARTESIAN_POINT ( 'NONE',  ( -5.405949406250003975, -9.363379034771801557, -15.53125000204835793 ) ) ;
#33259 = CARTESIAN_POINT ( 'NONE',  ( 5.405949406249999534, 9.363379034771803333, -28.09375000204836326 ) ) ;
#33260 = CARTESIAN_POINT ( 'NONE',  ( 4.999999999999992006, -8.660254037844389075, -124.1250000040967905 ) ) ;
#33261 = CARTESIAN_POINT ( 'NONE',  ( -10.81189881249999729, 6.242252689847871849, -137.2187500020483810 ) ) ;
#33262 = CARTESIAN_POINT ( 'NONE',  ( 9.999999999999996447, -5.773502691896262640, -104.1249999999999858 ) ) ;
#33263 = CARTESIAN_POINT ( 'NONE',  ( 10.81189881249999907, 6.242252689847868297, -37.40625000204836681 ) ) ;
#33264 = CARTESIAN_POINT ( 'NONE',  ( -2.121150477449813534E-15, -11.54700538379251284, -114.8749999999999716 ) ) ;
#33265 = CARTESIAN_POINT ( 'NONE',  ( -9.999999999999998224, 5.773502691896259087, -58.37499999999998579 ) ) ;
#33266 = CARTESIAN_POINT ( 'NONE',  ( 10.81189881249999729, 0.000000000000000000, -129.0312500020484094 ) ) ;
#33267 = CARTESIAN_POINT ( 'NONE',  ( -5.405949406250003975, -9.363379034771801557, -105.5312500020483810 ) ) ;
#33268 = VERTEX_POINT ( 'NONE', #40802 ) ;
#33269 = CARTESIAN_POINT ( 'NONE',  ( -2.121150477449813534E-15, -11.54700538379251284, -131.3750000000000000 ) ) ;
#33270 = CARTESIAN_POINT ( 'NONE',  ( -10.00000000000000000, -5.773502691896251982, -106.5000000040967763 ) ) ;
#33271 = CARTESIAN_POINT ( 'NONE',  ( -2.121150477449813534E-15, -11.54700538379251284, -136.2500000040967905 ) ) ;
#33272 = CARTESIAN_POINT ( 'NONE',  ( 5.405949406249999534, 9.363379034771803333, -68.59375000204836681 ) ) ;
#33273 = EDGE_LOOP ( 'NONE', ( #18267, #24254 ) ) ;
#33274 = CARTESIAN_POINT ( 'NONE',  ( -9.999999999999998224, 1.224646799147353059E-15, -31.24999999999997158 ) ) ;
#33275 = VECTOR ( 'NONE', #30509, 1000.000000000000000 ) ;
#33276 = CARTESIAN_POINT ( 'NONE',  ( -5.000000000000003553, -8.660254037844383745, -16.37500000409675138 ) ) ;
#33277 = CARTESIAN_POINT ( 'NONE',  ( -10.81189881249999729, -6.242252689847864744, -47.15625000204836681 ) ) ;
#33278 = DIRECTION ( 'NONE',  ( -0.000000000000000000, -0.000000000000000000, 1.000000000000000000 ) ) ;
#33279 = CARTESIAN_POINT ( 'NONE',  ( -9.999999999999998224, 1.224646799147353059E-15, -34.62500000409676915 ) ) ;
#33280 = LINE ( 'NONE', #31267, #40350 ) ;
#33281 = CARTESIAN_POINT ( 'NONE',  ( 5.405949406249992428, -9.363379034771808662, -141.2812500020483810 ) ) ;
#33282 = CARTESIAN_POINT ( 'NONE',  ( 0.000000000000000000, 0.000000000000000000, -200.0000000000000000 ) ) ;
#33283 = ORIENTED_EDGE ( 'NONE', *, *, #32262, .F. ) ;
#33284 = ORIENTED_EDGE ( 'NONE', *, *, #7477, .F. ) ;
#33285 = EDGE_CURVE ( 'NONE', #17480, #19924, #7876, .T. ) ;
#33286 = VERTEX_POINT ( 'NONE', #24006 ) ;
#33287 = CARTESIAN_POINT ( 'NONE',  ( 9.999999999999998224, 0.000000000000000000, -126.8750000040967905 ) ) ;
#33288 = EDGE_CURVE ( 'NONE', #18350, #15045, #10623, .T. ) ;
#33289 = CARTESIAN_POINT ( 'NONE',  ( -2.121150477449813534E-15, -11.54700538379251284, -121.2500000040967905 ) ) ;
#33290 = CARTESIAN_POINT ( 'NONE',  ( -5.405949406249996869, 9.363379034771805109, -174.8437500020484094 ) ) ;
#33291 = CARTESIAN_POINT ( 'NONE',  ( 5.405949406249999534, 9.363379034771803333, -20.59375000204835615 ) ) ;
#33292 = CARTESIAN_POINT ( 'NONE',  ( -4.999999999999996447, 8.660254037844387298, -144.3750000040967905 ) ) ;
#33293 = DIRECTION ( 'NONE',  ( -0.000000000000000000, -0.000000000000000000, 1.000000000000000000 ) ) ;
#33294 = CARTESIAN_POINT ( 'NONE',  ( -2.293366432827344421E-15, -12.48450537969573659, -156.2187500020483810 ) ) ;
#33295 = CARTESIAN_POINT ( 'NONE',  ( 5.405949406249992428, -9.363379034771808662, -138.0937500020483810 ) ) ;
#33296 = DIRECTION ( 'NONE',  ( -1.000000000000000000, 0.000000000000000000, 0.000000000000000000 ) ) ;
#33297 = CARTESIAN_POINT ( 'NONE',  ( 7.644554776091147741E-16, 12.48450537969573659, -123.9687500020483952 ) ) ;
#33298 = CARTESIAN_POINT ( 'NONE',  ( -2.293366432827344421E-15, -12.48450537969573659, -135.4062500020483810 ) ) ;
#33299 = CARTESIAN_POINT ( 'NONE',  ( -5.405949406249996869, 9.363379034771805109, -14.34375000204834905 ) ) ;
#33300 = CARTESIAN_POINT ( 'NONE',  ( 10.81189881249999551, -6.242252689847874514, -136.4687500020483810 ) ) ;
#33301 = DIRECTION ( 'NONE',  ( 1.734723475976806848E-16, -1.000000000000000000, 0.000000000000000000 ) ) ;
#33302 = CARTESIAN_POINT ( 'NONE',  ( 9.999999999999998224, 0.000000000000000000, -120.5000000000000000 ) ) ;
#33303 = CARTESIAN_POINT ( 'NONE',  ( 10.00000000000000000, 5.773502691896255534, -153.3750000000000000 ) ) ;
#33304 = CARTESIAN_POINT ( 'NONE',  ( -9.999999999999998224, 1.224646799147353059E-15, -67.24999999999997158 ) ) ;
#33305 = CARTESIAN_POINT ( 'NONE',  ( -10.81189881249999729, 1.324075727343319199E-15, -83.09375000204836681 ) ) ;
#33306 = CARTESIAN_POINT ( 'NONE',  ( -10.81189881249999729, 6.242252689847871849, -69.71875000204838102 ) ) ;
#33307 = CARTESIAN_POINT ( 'NONE',  ( 10.81189881249999907, 6.242252689847868297, -43.40625000204837391 ) ) ;
#33308 = CARTESIAN_POINT ( 'NONE',  ( 7.644554776091147741E-16, 12.48450537969573659, -51.96875000204836681 ) ) ;
#33309 = LINE ( 'NONE', #27460, #17813 ) ;
#33310 = CARTESIAN_POINT ( 'NONE',  ( -10.81189881249999729, 1.324075727343319199E-15, -162.5937500020484094 ) ) ;
#33311 = CARTESIAN_POINT ( 'NONE',  ( 10.00000000000000000, 5.773502691896255534, -126.3749999999999858 ) ) ;
#33312 = CARTESIAN_POINT ( 'NONE',  ( -10.81189881249999729, 1.324075727343319199E-15, -135.7812500020483810 ) ) ;
#33313 = DIRECTION ( 'NONE',  ( 1.000000000000000000, 0.000000000000000000, 0.000000000000000000 ) ) ;
#33314 = CARTESIAN_POINT ( 'NONE',  ( -4.999999999999996447, 8.660254037844387298, -79.49999999999998579 ) ) ;
#33315 = ORIENTED_EDGE ( 'NONE', *, *, #7790, .F. ) ;
#33316 = CARTESIAN_POINT ( 'NONE',  ( 7.644554776091147741E-16, 12.48450537969573659, -107.6562500020483810 ) ) ;
#33317 = CARTESIAN_POINT ( 'NONE',  ( -10.00000000000000000, -5.773502691896251982, -135.0000000040967905 ) ) ;
#33318 = DIRECTION ( 'NONE',  ( -0.000000000000000000, -0.000000000000000000, -1.000000000000000000 ) ) ;
#33319 = CARTESIAN_POINT ( 'NONE',  ( 5.405949406249992428, -9.363379034771808662, -168.2812500020484094 ) ) ;
#33320 = CARTESIAN_POINT ( 'NONE',  ( 9.999999999999996447, -5.773502691896262640, -40.00000000409676204 ) ) ;
#33321 = CARTESIAN_POINT ( 'NONE',  ( 0.000000000000000000, 0.000000000000000000, -200.0000000000000000 ) ) ;
#33322 = CARTESIAN_POINT ( 'NONE',  ( 5.405949406249992428, -9.363379034771808662, -54.28125000204836681 ) ) ;
#33323 = CARTESIAN_POINT ( 'NONE',  ( -5.000000000000003553, -8.660254037844383745, -63.99999999999997158 ) ) ;
#33324 = CARTESIAN_POINT ( 'NONE',  ( -5.405949406250003975, -9.363379034771801557, -159.5312500020484094 ) ) ;
#33325 = CARTESIAN_POINT ( 'NONE',  ( 10.81189881249999907, 6.242252689847868297, -136.2187500020483810 ) ) ;
#33326 = CARTESIAN_POINT ( 'NONE',  ( -5.000000000000003553, -8.660254037844383745, -50.87500000409675494 ) ) ;
#33327 = CARTESIAN_POINT ( 'NONE',  ( -9.999999999999998224, 1.224646799147353059E-15, -79.62500000409677625 ) ) ;
#33328 = VERTEX_POINT ( 'NONE', #41011 ) ;
#33329 = DIRECTION ( 'NONE',  ( -0.5000000000000003331, 0.8660254037844383745, 0.000000000000000000 ) ) ;
#33331 = ORIENTED_EDGE ( 'NONE', *, *, #15733, .F. ) ;
#33330 = CARTESIAN_POINT ( 'NONE',  ( -5.405949406250003975, -9.363379034771801557, -66.53125000204838102 ) ) ;
#33332 = CALENDAR_DATE ( 2026, 28, 9 ) ;
#33333 = EDGE_CURVE ( 'NONE', #12734, #982, #20318, .T. ) ;
#33335 = ORIENTED_EDGE ( 'NONE', *, *, #20467, .T. ) ;
#33334 = CARTESIAN_POINT ( 'NONE',  ( 10.81189881249999551, -6.242252689847874514, -119.9687500020483952 ) ) ;
#33336 = EDGE_CURVE ( 'NONE', #31054, #27322, #15038, .T. ) ;
#33337 =( BOUNDED_CURVE ( )  B_SPLINE_CURVE ( 2, ( #1858, #34017, #21045, #31421, #38096, #7680, #4651 ),
 .UNSPECIFIED., .F., .F. ) 
 B_SPLINE_CURVE_WITH_KNOTS ( ( 3, 2, 2, 3 ),
 ( 0.1753731343283582433, 0.1766169154228856009, 0.1778606965174129861, 0.1791044776119403437 ),
 .UNSPECIFIED. ) 
 CURVE ( )  GEOMETRIC_REPRESENTATION_ITEM ( )  RATIONAL_B_SPLINE_CURVE ( ( 0.9999999999999970024, 0.8660254037844417052, 1.000000000000000000, 0.8660254037844387076, 1.000000000000000000, 0.8660254037844327124, 1.000000000000005995 ) ) 
 REPRESENTATION_ITEM ( '' )  );
#33338 = EDGE_CURVE ( 'NONE', #32481, #2493, #17100, .T. ) ;
#33339 = CARTESIAN_POINT ( 'NONE',  ( -2.293366432827344421E-15, -12.48450537969573659, -18.21875000204837036 ) ) ;
#33340 = UNCERTAINTY_MEASURE_WITH_UNIT (LENGTH_MEASURE( 1.000000000000000082E-05 ), #31640, 'distance_accuracy_value', 'NONE');
#33341 = CARTESIAN_POINT ( 'NONE',  ( -2.293366432827344421E-15, -12.48450537969573659, -195.2187500020484094 ) ) ;
#33342 = CARTESIAN_POINT ( 'NONE',  ( -2.293366432827344421E-15, -12.48450537969573659, -51.21875000204836681 ) ) ;
#33343 = CARTESIAN_POINT ( 'NONE',  ( -9.999999999999998224, 1.224646799147353059E-15, -134.7499999999999716 ) ) ;
#33344 = DIRECTION ( 'NONE',  ( -0.000000000000000000, -0.000000000000000000, 1.000000000000000000 ) ) ;
#33345 = CARTESIAN_POINT ( 'NONE',  ( 5.405949406249999534, 9.363379034771803333, -176.5937500020484094 ) ) ;
#33346 = CARTESIAN_POINT ( 'NONE',  ( -10.81189881249999907, -6.242252689847864744, -172.9687500020484094 ) ) ;
#33347 = CC_DESIGN_DATE_AND_TIME_ASSIGNMENT ( #8655, #21808, ( #15921 ) ) ;
#33348 = CARTESIAN_POINT ( 'NONE',  ( -5.405949406250003975, -9.363379034771801557, -153.3437500020483810 ) ) ;
#33349 = CARTESIAN_POINT ( 'NONE',  ( -10.81189881249999729, -6.242252689847864744, -163.9687500020483526 ) ) ;
#33350 = CARTESIAN_POINT ( 'NONE',  ( 9.999999999999998224, 0.000000000000000000, -123.8750000040967905 ) ) ;
#33351 = CARTESIAN_POINT ( 'NONE',  ( 9.999999999999998224, 0.000000000000000000, -126.5000000000000000 ) ) ;
#33352 = CARTESIAN_POINT ( 'NONE',  ( 7.070501591499377789E-16, 11.54700538379251284, -178.6250000000000000 ) ) ;
#33353 = CARTESIAN_POINT ( 'NONE',  ( -10.81189881249999907, -6.242252689847864744, -99.46875000204838102 ) ) ;
#33354 = CARTESIAN_POINT ( 'NONE',  ( 10.00000000000051159, -5.773502691895965988, -101.1249999999999858 ) ) ;
#33355 = CARTESIAN_POINT ( 'NONE',  ( 10.81189881249999551, -6.242252689847874514, -64.65625000204839523 ) ) ;
#33356 = FACE_OUTER_BOUND ( 'NONE', #25002, .T. ) ;
#33357 = CARTESIAN_POINT ( 'NONE',  ( -10.81189881249999729, 6.242252689847871849, -186.7187500020483810 ) ) ;
#33358 = CARTESIAN_POINT ( 'NONE',  ( 10.81189881249999551, -6.242252689847874514, -123.1562500020483952 ) ) ;
#33359 = CARTESIAN_POINT ( 'NONE',  ( -10.81189881249999729, -6.242252689847864744, -159.6562500020484094 ) ) ;
#33360 = CARTESIAN_POINT ( 'NONE',  ( 5.405949406249992428, -9.363379034771808662, -54.28125000204836681 ) ) ;
#33361 = CARTESIAN_POINT ( 'NONE',  ( 4.999999999999992006, -8.660254037844389075, -139.1250000040967905 ) ) ;
#33362 = CARTESIAN_POINT ( 'NONE',  ( 4.999999999999992006, -8.660254037844389075, -119.2500000000000000 ) ) ;
#33363 = ORIENTED_EDGE ( 'NONE', *, *, #29132, .T. ) ;
#33364 = CARTESIAN_POINT ( 'NONE',  ( -5.405949406249996869, 9.363379034771805109, -134.5312500020484094 ) ) ;
#33365 = CARTESIAN_POINT ( 'NONE',  ( -10.81189881249999907, -6.242252689847864744, -146.1562500020484094 ) ) ;
#33366 = EDGE_CURVE ( 'NONE', #21484, #36111, #7618, .T. ) ;
#33367 = CARTESIAN_POINT ( 'NONE',  ( 5.405949406249999534, 9.363379034771803333, -187.2812500020484094 ) ) ;
#33368 = CARTESIAN_POINT ( 'NONE',  ( 0.000000000000000000, -5.321294541346989426, -220.0000000000000000 ) ) ;
#33369 = CARTESIAN_POINT ( 'NONE',  ( 10.81189881249999551, -6.242252689847874514, -80.96875000204838102 ) ) ;
#33370 = VERTEX_POINT ( 'NONE', #37742 ) ;
#33371 = CARTESIAN_POINT ( 'NONE',  ( -10.00000000000000000, -5.773502691896251982, -59.62500000000000000 ) ) ;
#33372 = CARTESIAN_POINT ( 'NONE',  ( 5.405949406249999534, 9.363379034771803333, -184.0937500020483810 ) ) ;
#33373 = CARTESIAN_POINT ( 'NONE',  ( -9.999999999999998224, 5.773502691896259087, -64.75000000409677625 ) ) ;
#33374 = FACE_OUTER_BOUND ( 'NONE', #40398, .T. ) ;
#33375 = DIRECTION ( 'NONE',  ( -1.000000000000000000, 0.000000000000000000, -0.000000000000000000 ) ) ;
#33376 = CARTESIAN_POINT ( 'NONE',  ( -10.81189881249999729, 1.324075727343319199E-15, -80.28125000204838102 ) ) ;
#33377 = CARTESIAN_POINT ( 'NONE',  ( 5.405949406249999534, 9.363379034771803333, -58.28125000204836681 ) ) ;
#33378 = CARTESIAN_POINT ( 'NONE',  ( -2.121150477449813534E-15, -11.54700538379251284, -55.25000000409677625 ) ) ;
#33379 = CARTESIAN_POINT ( 'NONE',  ( 7.644554776091147741E-16, 12.48450537969573659, -8.468750002048359704 ) ) ;
#33380 = FACE_OUTER_BOUND ( 'NONE', #7625, .T. ) ;
#33381 = CARTESIAN_POINT ( 'NONE',  ( -10.81189881249999907, -6.242252689847864744, -185.1562500020484094 ) ) ;
#33382 = CARTESIAN_POINT ( 'NONE',  ( 10.81189881249999729, 0.000000000000000000, -7.531250002048350822 ) ) ;
#33383 = CARTESIAN_POINT ( 'NONE',  ( 9.999999999998969713, 5.773502691896851502, -40.87499999999994316 ) ) ;
#33384 = CARTESIAN_POINT ( 'NONE',  ( 9.999999999999998224, 0.000000000000000000, -117.5000000000000000 ) ) ;
#33385 = CYLINDRICAL_SURFACE ( 'NONE', #33223, 9.999999999999998224 ) ;
#33386 = DIRECTION ( 'NONE',  ( 0.000000000000000000, 1.000000000000000000, 0.000000000000000000 ) ) ;
#33387 = CARTESIAN_POINT ( 'NONE',  ( -9.999999999999998224, 1.224646799147353059E-15, -62.74999999999997158 ) ) ;
#33389 = ORIENTED_EDGE ( 'NONE', *, *, #3031, .F. ) ;
#33388 = CARTESIAN_POINT ( 'NONE',  ( 5.405949406249999534, 9.363379034771803333, -91.28125000204838102 ) ) ;
#33390 = CARTESIAN_POINT ( 'NONE',  ( 4.999999999999992006, -8.660254037844389075, -160.1250000040967905 ) ) ;
#33392 = EDGE_LOOP ( 'NONE', ( #40927, #19984, #31432, #34183 ) ) ;
#33391 = CARTESIAN_POINT ( 'NONE',  ( 7.644554776091147741E-16, 12.48450537969573659, -102.9687500020483668 ) ) ;
#33393 = VERTEX_POINT ( 'NONE', #4945 ) ;
#33394 = CARTESIAN_POINT ( 'NONE',  ( 10.81189881249999551, -6.242252689847874514, -32.96875000204834549 ) ) ;
#33395 = CARTESIAN_POINT ( 'NONE',  ( -5.405949406249996869, 9.363379034771805109, -23.53125000204836681 ) ) ;
#33396 = CARTESIAN_POINT ( 'NONE',  ( -10.81189881249999907, -6.242252689847864744, -69.46875000204838102 ) ) ;
#33397 = CARTESIAN_POINT ( 'NONE',  ( -9.999999999998456346, -5.773502691897145489, -18.00000000409673007 ) ) ;
#33398 = CARTESIAN_POINT ( 'NONE',  ( -4.999999999999996447, 8.660254037844387298, -43.49999999999998579 ) ) ;
#33399 = CARTESIAN_POINT ( 'NONE',  ( 7.644554776091147741E-16, 12.48450537969573659, -194.4687500020484094 ) ) ;
#33400 = CARTESIAN_POINT ( 'NONE',  ( -2.293366432827344421E-15, -12.48450537969573659, -148.7187500020484094 ) ) ;
#33401 = CARTESIAN_POINT ( 'NONE',  ( 9.999999999999998224, 0.000000000000000000, -72.87500000409677625 ) ) ;
#33402 = DIRECTION ( 'NONE',  ( 0.000000000000000000, 0.000000000000000000, 1.000000000000000000 ) ) ;
#33403 = CARTESIAN_POINT ( 'NONE',  ( -10.81189881249999907, -6.242252689847864744, -147.6562500020483810 ) ) ;
#33404 = CARTESIAN_POINT ( 'NONE',  ( 9.999999999999998224, 0.000000000000000000, -0.8750000040967653714 ) ) ;
#33405 = CARTESIAN_POINT ( 'NONE',  ( 10.00000000000102318, -5.773502691895667560, -103.0000000040967194 ) ) ;
#33406 = EDGE_CURVE ( 'NONE', #3605, #26657, #18092, .T. ) ;
#33407 = CARTESIAN_POINT ( 'NONE',  ( 10.81189881249999729, 0.000000000000000000, -119.8437500020483810 ) ) ;
#33408 = CARTESIAN_POINT ( 'NONE',  ( -9.999999999999998224, 1.224646799147353059E-15, -160.6250000040967905 ) ) ;
#33409 = CARTESIAN_POINT ( 'NONE',  ( 10.81189881249999551, -6.242252689847874514, -90.15625000204836681 ) ) ;
#33410 = CARTESIAN_POINT ( 'NONE',  ( 7.644554776091147741E-16, 12.48450537969573659, -110.4687500020483668 ) ) ;
#33411 = CARTESIAN_POINT ( 'NONE',  ( -5.405949406249996869, 9.363379034771805109, -69.84375000204836681 ) ) ;
#33412 = CARTESIAN_POINT ( 'NONE',  ( 5.405949406249992428, -9.363379034771808662, -76.78125000204838102 ) ) ;
#33413 = CARTESIAN_POINT ( 'NONE',  ( -5.000000000000003553, -8.660254037844383745, -161.8750000040967905 ) ) ;
#33414 = CARTESIAN_POINT ( 'NONE',  ( -5.405949406249996869, 9.363379034771805109, -160.0312500020484094 ) ) ;
#33415 = CARTESIAN_POINT ( 'NONE',  ( -5.405949406249996869, 9.363379034771805109, -175.0312500020484094 ) ) ;
#33416 = DIRECTION ( 'NONE',  ( -0.000000000000000000, -0.000000000000000000, -1.000000000000000000 ) ) ;
#33417 = CARTESIAN_POINT ( 'NONE',  ( -2.121150477449813534E-15, -11.54700538379251284, -145.2500000040967905 ) ) ;
#33418 = DIRECTION ( 'NONE',  ( -0.000000000000000000, -0.000000000000000000, -1.000000000000000000 ) ) ;
#33419 = CARTESIAN_POINT ( 'NONE',  ( -2.293366432827344421E-15, -12.48450537969573659, -105.2187500020483952 ) ) ;
#33420 = CARTESIAN_POINT ( 'NONE',  ( -5.000000000000003553, -8.660254037844383745, -83.49999999999997158 ) ) ;
#33421 = CARTESIAN_POINT ( 'NONE',  ( 5.405949406249999534, 9.363379034771803333, -4.281250002048375691 ) ) ;
#33422 = CARTESIAN_POINT ( 'NONE',  ( 5.000000000000000000, 8.660254037844385522, -90.62500000409677625 ) ) ;
#33423 = DIRECTION ( 'NONE',  ( -0.8660254037844388186, 0.4999999999999997224, 0.000000000000000000 ) ) ;
#33424 = CARTESIAN_POINT ( 'NONE',  ( -10.81189881249999729, 1.324075727343319199E-15, -96.78125000204839523 ) ) ;
#33425 = CARTESIAN_POINT ( 'NONE',  ( 10.81189881249999729, 0.000000000000000000, -81.03125000204839523 ) ) ;
#33426 = ORIENTED_EDGE ( 'NONE', *, *, #15257, .F. ) ;
#33427 = CARTESIAN_POINT ( 'NONE',  ( 7.070501591499377789E-16, 11.54700538379251284, -74.00000000409677625 ) ) ;
#33428 = CARTESIAN_POINT ( 'NONE',  ( 9.999999999999998224, 0.000000000000000000, -200.0000000000000000 ) ) ;
#33429 = CARTESIAN_POINT ( 'NONE',  ( -10.81189881249999907, -6.242252689847864744, -31.96875000204834905 ) ) ;
#33430 = VERTEX_POINT ( 'NONE', #1716 ) ;
#33431 = CARTESIAN_POINT ( 'NONE',  ( 10.00000000000000000, 5.773502691896255534, -9.374999999999980460 ) ) ;
#33432 = CARTESIAN_POINT ( 'NONE',  ( 10.81189881249999729, 0.000000000000000000, -39.03125000204838102 ) ) ;
#33433 = CARTESIAN_POINT ( 'NONE',  ( 7.070501591499377789E-16, 11.54700538379251284, -144.1250000000000000 ) ) ;
#33434 = DIRECTION ( 'NONE',  ( -0.000000000000000000, -0.000000000000000000, 1.000000000000000000 ) ) ;
#33435 =( BOUNDED_CURVE ( )  B_SPLINE_CURVE ( 2, ( #35668, #26789, #15992, #51, #29398, #6516, #36295 ),
 .UNSPECIFIED., .F., .F. ) 
 B_SPLINE_CURVE_WITH_KNOTS ( ( 3, 2, 2, 3 ),
 ( 0.3768656716417911334, 0.3781094527363185187, 0.3793532338308459040, 0.3805970149253732338 ),
 .UNSPECIFIED. ) 
 CURVE ( )  GEOMETRIC_REPRESENTATION_ITEM ( )  RATIONAL_B_SPLINE_CURVE ( ( 0.9999999999999880096, 0.8660254037844506980, 1.000000000000000000, 0.8660254037844387076, 1.000000000000000000, 0.8660254037844267172, 1.000000000000011990 ) ) 
 REPRESENTATION_ITEM ( '' )  );
#33436 = CARTESIAN_POINT ( 'NONE',  ( -9.999999999999998224, 1.224646799147353059E-15, -10.62500000409674605 ) ) ;
#33437 = CARTESIAN_POINT ( 'NONE',  ( 9.999999999999996447, -5.773502691896262640, -189.6250000000000000 ) ) ;
#33438 = CARTESIAN_POINT ( 'NONE',  ( -9.999999999999998224, 1.224646799147353059E-15, -200.0000000000000000 ) ) ;
#33440 = ORIENTED_EDGE ( 'NONE', *, *, #38704, .T. ) ;
#33439 = CARTESIAN_POINT ( 'NONE',  ( -2.293366432827344421E-15, -12.48450537969573659, -120.4062500020483952 ) ) ;
#33441 = CARTESIAN_POINT ( 'NONE',  ( 9.999999999998456346, 5.773502691897149042, -23.25000000409674072 ) ) ;
#33442 = ORIENTED_EDGE ( 'NONE', *, *, #34658, .T. ) ;
#33443 = EDGE_LOOP ( 'NONE', ( #18164, #18696, #27432, #17427 ) ) ;
#33444 = CARTESIAN_POINT ( 'NONE',  ( -10.81189881249999729, 1.324075727343319199E-15, -47.28125000204838813 ) ) ;
#33445 = DATE_AND_TIME ( #4078, #32514 ) ;
#33446 = CARTESIAN_POINT ( 'NONE',  ( -2.293366432827344421E-15, -12.48450537969573659, -93.21875000204838102 ) ) ;
#33447 = CARTESIAN_POINT ( 'NONE',  ( -5.405949406250003975, -9.363379034771801557, -125.0312500020483952 ) ) ;
#33448 = EDGE_LOOP ( 'NONE', ( #32281, #12205, #693, #36133 ) ) ;
#33449 = CARTESIAN_POINT ( 'NONE',  ( -5.000000000000003553, -8.660254037844383745, -83.49999999999997158 ) ) ;
#33450 = VECTOR ( 'NONE', #22991, 1000.000000000000000 ) ;
#33451 = CARTESIAN_POINT ( 'NONE',  ( -5.405949406250003975, -9.363379034771801557, -196.8437500020484094 ) ) ;
#33452 = CARTESIAN_POINT ( 'NONE',  ( 10.81189881249999551, -6.242252689847874514, -175.6562500020484094 ) ) ;
#33453 = CARTESIAN_POINT ( 'NONE',  ( 0.000000000000000000, 0.000000000000000000, -169.9999999999999716 ) ) ;
#33454 = CARTESIAN_POINT ( 'NONE',  ( 10.81189881249999729, 6.242252689847867408, -130.2187500020483810 ) ) ;
#33455 = CARTESIAN_POINT ( 'NONE',  ( 10.81189881249999551, -6.242252689847874514, -89.96875000204838102 ) ) ;
#33456 = DIRECTION ( 'NONE',  ( -0.000000000000000000, -0.000000000000000000, 1.000000000000000000 ) ) ;
#33457 = CARTESIAN_POINT ( 'NONE',  ( 5.405949406249999534, 9.363379034771803333, -98.78125000204839523 ) ) ;
#33458 = CARTESIAN_POINT ( 'NONE',  ( -9.999999999999998224, 5.773502691896259087, -187.7500000040967905 ) ) ;
#33459 = CARTESIAN_POINT ( 'NONE',  ( 10.81189881249999729, 0.000000000000000000, -112.3437500020483810 ) ) ;
#33460 = CARTESIAN_POINT ( 'NONE',  ( -2.293366432827344421E-15, -12.48450537969573659, -177.4062500020484379 ) ) ;
#33461 = VECTOR ( 'NONE', #34105, 1000.000000000000000 ) ;
#33462 = CARTESIAN_POINT ( 'NONE',  ( -5.000000000000003553, -8.660254037844383745, -107.4999999999999858 ) ) ;
#33463 = CARTESIAN_POINT ( 'NONE',  ( -2.275517850991317657E-15, -20.00000000000000000, -232.0000000000000000 ) ) ;
#33464 = CARTESIAN_POINT ( 'NONE',  ( 5.405949406249992428, -9.363379034771808662, -196.7812500020484094 ) ) ;
#33465 = CARTESIAN_POINT ( 'NONE',  ( 7.644554776091147741E-16, 12.48450537969573659, -62.46875000204839523 ) ) ;
#33466 = CARTESIAN_POINT ( 'NONE',  ( 5.405949406249999534, 9.363379034771803333, -41.59375000204837391 ) ) ;
#33467 = CARTESIAN_POINT ( 'NONE',  ( 9.999999999999996447, -5.773502691896262640, -175.0000000040968189 ) ) ;
#33468 = CARTESIAN_POINT ( 'NONE',  ( -2.293366432827344421E-15, -12.48450537969573659, -21.40625000204837036 ) ) ;
#33469 = CARTESIAN_POINT ( 'NONE',  ( 10.81189881249999729, 0.000000000000000000, -19.34375000204835260 ) ) ;
#33470 = CARTESIAN_POINT ( 'NONE',  ( 0.000000000000000000, 0.000000000000000000, -200.0000000000000000 ) ) ;
#33471 = CARTESIAN_POINT ( 'NONE',  ( -10.81189881249999907, -6.242252689847864744, -129.4687500020483810 ) ) ;
#33472 = CARTESIAN_POINT ( 'NONE',  ( 10.00000000000000000, 5.773502691896255534, -106.8749999999999716 ) ) ;
#33473 = CARTESIAN_POINT ( 'NONE',  ( -5.405949406249996869, 9.363379034771805109, -25.03125000204836681 ) ) ;
#33474 = CARTESIAN_POINT ( 'NONE',  ( 7.070501591499377789E-16, 11.54700538379251284, -58.62499999999997868 ) ) ;
#33475 = CARTESIAN_POINT ( 'NONE',  ( 10.81189881249999729, 0.000000000000000000, -135.0312500020484094 ) ) ;
#33476 = CARTESIAN_POINT ( 'NONE',  ( -5.405949406250003975, -9.363379034771801557, -108.5312500020483810 ) ) ;
#33477 = ADVANCED_FACE ( 'NONE', ( #34736 ), #5158, .T. ) ;
#33478 = ORIENTED_EDGE ( 'NONE', *, *, #15107, .T. ) ;
#33479 =( BOUNDED_CURVE ( )  B_SPLINE_CURVE ( 2, ( #33343, #36138, #10009, #29883, #39366, #23188, #19937 ),
 .UNSPECIFIED., .F., .F. ) 
 B_SPLINE_CURVE_WITH_KNOTS ( ( 3, 2, 2, 3 ),
 ( 0.3246268656716419510, 0.3258706467661692807, 0.3271144278606965550, 0.3283582089552238847 ),
 .UNSPECIFIED. ) 
 CURVE ( )  GEOMETRIC_REPRESENTATION_ITEM ( )  RATIONAL_B_SPLINE_CURVE ( ( 0.9999999999999820144, 0.8660254037844566932, 1.000000000000000000, 0.8660254037844387076, 1.000000000000000000, 0.8660254037844387076, 1.000000000000000000 ) ) 
 REPRESENTATION_ITEM ( '' )  );
#33480 = CARTESIAN_POINT ( 'NONE',  ( -9.999999999999998224, 1.224646799147353059E-15, -131.7499999999999716 ) ) ;
#33481 = CARTESIAN_POINT ( 'NONE',  ( -9.999999999999998224, 5.773502691896259087, -111.2500000040967763 ) ) ;
#33482 = CARTESIAN_POINT ( 'NONE',  ( -9.999999999999918288, -5.773502691896298167, -195.0000000040968189 ) ) ;
#33483 = CARTESIAN_POINT ( 'NONE',  ( 10.81189881249999551, -6.242252689847874514, -59.96875000204837391 ) ) ;
#33484 = ORIENTED_EDGE ( 'NONE', *, *, #13750, .T. ) ;
#33485 = CARTESIAN_POINT ( 'NONE',  ( 10.00000000000000000, 5.773502691896255534, -30.37499999999995381 ) ) ;
#33486 = CARTESIAN_POINT ( 'NONE',  ( 10.81189881249999551, -6.242252689847874514, -39.15625000204835970 ) ) ;
#33487 = CYLINDRICAL_SURFACE ( 'NONE', #17283, 9.999999999999998224 ) ;
#33488 = CARTESIAN_POINT ( 'NONE',  ( 4.999999999999992006, -8.660254037844389075, -35.62500000409676915 ) ) ;
#33489 = CARTESIAN_POINT ( 'NONE',  ( 9.999999999999998224, 0.000000000000000000, -138.5000000000000000 ) ) ;
#33490 = CARTESIAN_POINT ( 'NONE',  ( 5.405949406249999534, 9.363379034771803333, -139.2812500020483810 ) ) ;
#33491 = AXIS2_PLACEMENT_3D ( 'NONE', #2438, #22289, #19038 ) ;
#33492 = CARTESIAN_POINT ( 'NONE',  ( 5.000000000000000000, 8.660254037844385522, -174.6250000040968189 ) ) ;
#33493 = VERTEX_POINT ( 'NONE', #1930 ) ;
#33494 = ADVANCED_FACE ( 'NONE', ( #26650 ), #26436, .F. ) ;
#33495 = ORIENTED_EDGE ( 'NONE', *, *, #20419, .F. ) ;
#33496 = CARTESIAN_POINT ( 'NONE',  ( -9.999999999999998224, 1.224646799147353059E-15, -107.7499999999999858 ) ) ;
#33497 = CARTESIAN_POINT ( 'NONE',  ( 10.00000000000025402, -5.773502691896113426, -129.6250000000000000 ) ) ;
#33499 = EDGE_CURVE ( 'NONE', #15077, #11765, #13890, .T. ) ;
#33498 = CARTESIAN_POINT ( 'NONE',  ( 10.81189881249999729, 0.000000000000000000, -164.8437500020484094 ) ) ;
#33500 = CARTESIAN_POINT ( 'NONE',  ( 10.81189881249999729, 0.000000000000000000, -195.0312500020484094 ) ) ;
#33501 = CARTESIAN_POINT ( 'NONE',  ( 10.81189881249999729, 0.000000000000000000, -20.84375000204835615 ) ) ;
#33502 = CARTESIAN_POINT ( 'NONE',  ( -9.999999999999998224, 1.224646799147353059E-15, -149.7500000000000000 ) ) ;
#33503 = CARTESIAN_POINT ( 'NONE',  ( 10.81189881249999551, -6.242252689847874514, -155.9687500020484094 ) ) ;
#33504 = CARTESIAN_POINT ( 'NONE',  ( 10.81189881249999729, 0.000000000000000000, -137.8437500020484094 ) ) ;
#33505 = CARTESIAN_POINT ( 'NONE',  ( -9.999999999999998224, 1.224646799147353059E-15, -9.125000004096744277 ) ) ;
#33506 = CARTESIAN_POINT ( 'NONE',  ( 10.81189881249999907, 6.242252689847868297, -119.7187500020483810 ) ) ;
#33507 = CARTESIAN_POINT ( 'NONE',  ( 7.070501591499377789E-16, 11.54700538379251284, -194.0000000040967905 ) ) ;
#33508 = AXIS2_PLACEMENT_3D ( 'NONE', #31544, #15101, #40787 ) ;
#33509 = CARTESIAN_POINT ( 'NONE',  ( 7.644554776091147741E-16, 12.48450537969573659, -124.1562500020483952 ) ) ;
#33510 = CARTESIAN_POINT ( 'NONE',  ( 10.81189881249999729, 0.000000000000000000, -8.843750002048345493 ) ) ;
#33511 = CARTESIAN_POINT ( 'NONE',  ( -10.81189881249999729, 6.242252689847871849, -138.7187500020483810 ) ) ;
#33512 = CARTESIAN_POINT ( 'NONE',  ( 7.070501591499376803E-16, 11.54700538379251284, -63.50000000409679046 ) ) ;
#33513 = CARTESIAN_POINT ( 'NONE',  ( 5.000000000000000000, 8.660254037844385522, -110.1250000040967763 ) ) ;
#33514 = CARTESIAN_POINT ( 'NONE',  ( 9.999999999999998224, 0.000000000000000000, -152.0000000000000000 ) ) ;
#33515 = CARTESIAN_POINT ( 'NONE',  ( -4.999999999999996447, 8.660254037844387298, -19.49999999999996092 ) ) ;
#33516 = CARTESIAN_POINT ( 'NONE',  ( -5.405949406250003975, -9.363379034771801557, -85.84375000204836681 ) ) ;
#33517 = CARTESIAN_POINT ( 'NONE',  ( 5.405949406249999534, 9.363379034771803333, -68.59375000204836681 ) ) ;
#33518 = CARTESIAN_POINT ( 'NONE',  ( -5.405949406249996869, 9.363379034771805109, -41.53125000204838102 ) ) ;
#33519 = CARTESIAN_POINT ( 'NONE',  ( -5.405949406250003975, -9.363379034771801557, -55.84375000204835970 ) ) ;
#33520 = DIRECTION ( 'NONE',  ( -0.000000000000000000, -0.000000000000000000, 1.000000000000000000 ) ) ;
#33521 = CARTESIAN_POINT ( 'NONE',  ( -2.293366432827344421E-15, -12.48450537969573659, -153.2187500020483810 ) ) ;
#33522 = CARTESIAN_POINT ( 'NONE',  ( -10.00000000000000000, -5.773502691896251982, -125.6249999999999858 ) ) ;
#33523 = CARTESIAN_POINT ( 'NONE',  ( 10.81189881249999729, 0.000000000000000000, -141.0312500020483810 ) ) ;
#33524 = CARTESIAN_POINT ( 'NONE',  ( 4.999999999999992006, -8.660254037844389075, -187.1250000040967905 ) ) ;
#33525 = CARTESIAN_POINT ( 'NONE',  ( 10.00000000000000000, 5.773502691896255534, -85.87499999999997158 ) ) ;
#33526 = CARTESIAN_POINT ( 'NONE',  ( -2.293366432827344421E-15, -12.48450537969573659, -18.40625000204837036 ) ) ;
#33527 = EDGE_LOOP ( 'NONE', ( #13973, #21306, #14001, #23612 ) ) ;
#33528 = CARTESIAN_POINT ( 'NONE',  ( -5.405949406250003975, -9.363379034771801557, -113.0312500020483952 ) ) ;
#33529 = CARTESIAN_POINT ( 'NONE',  ( 5.000000000000000000, 8.660254037844385522, -135.6250000040967620 ) ) ;
#33530 = LINE ( 'NONE', #9985, #40806 ) ;
#33531 = CARTESIAN_POINT ( 'NONE',  ( -9.999999999999998224, 1.224646799147353059E-15, -39.12500000409676915 ) ) ;
#33532 = EDGE_CURVE ( 'NONE', #258, #5415, #12273, .T. ) ;
#33533 = CARTESIAN_POINT ( 'NONE',  ( 5.000000000000000000, 8.660254037844385522, -155.1250000040967905 ) ) ;
#33534 = CARTESIAN_POINT ( 'NONE',  ( 5.405949406249992428, -9.363379034771808662, -51.28125000204835970 ) ) ;
#33535 = CARTESIAN_POINT ( 'NONE',  ( -9.999999999999998224, 1.224646799147353059E-15, -100.6250000040967905 ) ) ;
#33536 = CARTESIAN_POINT ( 'NONE',  ( -2.293366432827344421E-15, -12.48450537969573659, -150.4062500020483810 ) ) ;
#33537 = CARTESIAN_POINT ( 'NONE',  ( 10.81189881249999907, 6.242252689847868297, -134.7187500020484094 ) ) ;
#33538 = ORIENTED_EDGE ( 'NONE', *, *, #37259, .T. ) ;
#33539 = CARTESIAN_POINT ( 'NONE',  ( 5.000000000000000000, 8.660254037844385522, -189.6250000040967905 ) ) ;
#33541 = VERTEX_POINT ( 'NONE', #12830 ) ;
#33540 = CARTESIAN_POINT ( 'NONE',  ( 5.405949406249999534, 9.363379034771803333, -65.78125000204838102 ) ) ;
#33542 = MECHANICAL_CONTEXT ( 'NONE', #11857, 'mechanical' ) ;
#33544 = EDGE_LOOP ( 'NONE', ( #40730, #40717 ) ) ;
#33543 = CARTESIAN_POINT ( 'NONE',  ( 10.81189881249999729, 0.000000000000000000, -119.8437500020483810 ) ) ;
#33545 = CARTESIAN_POINT ( 'NONE',  ( 10.81189881249999551, -6.242252689847874514, -19.46875000204837391 ) ) ;
#33546 = CARTESIAN_POINT ( 'NONE',  ( -10.81189881249999729, 6.242252689847871849, -186.7187500020483810 ) ) ;
#33547 = CARTESIAN_POINT ( 'NONE',  ( 7.644554776091147741E-16, 12.48450537969573659, -48.96875000204835970 ) ) ;
#33548 = CARTESIAN_POINT ( 'NONE',  ( 9.999999999999998224, 0.000000000000000000, -62.37500000409676204 ) ) ;
#33549 = CARTESIAN_POINT ( 'NONE',  ( 9.999999999999998224, 0.000000000000000000, -105.8750000040967763 ) ) ;
#33550 = CARTESIAN_POINT ( 'NONE',  ( 10.81189881249999729, 0.000000000000000000, -182.8437500020483810 ) ) ;
#33551 = CARTESIAN_POINT ( 'NONE',  ( 7.644554776091147741E-16, 12.48450537969573659, -162.9687500020483810 ) ) ;
#33552 = CARTESIAN_POINT ( 'NONE',  ( -2.293366432827344421E-15, -12.48450537969573659, -151.7187500020483810 ) ) ;
#33553 = CARTESIAN_POINT ( 'NONE',  ( -10.81189881249999729, -6.242252689847864744, -165.4687500020483526 ) ) ;
#33554 = CARTESIAN_POINT ( 'NONE',  ( 9.999999999999998224, 0.000000000000000000, -104.3750000040967763 ) ) ;
#33555 = CARTESIAN_POINT ( 'NONE',  ( 7.071067811865472841, -7.071067811865472841, -200.0000000000000000 ) ) ;
#33556 = CARTESIAN_POINT ( 'NONE',  ( -9.999999999999998224, 5.773502691896259087, -179.8750000000000000 ) ) ;
#33557 = CARTESIAN_POINT ( 'NONE',  ( -10.81189881249999729, 6.242252689847871849, -89.21875000204836681 ) ) ;
#33558 = DIRECTION ( 'NONE',  ( 1.000000000000000000, 0.000000000000000000, 0.000000000000000000 ) ) ;
#33559 = CARTESIAN_POINT ( 'NONE',  ( 10.81189881249999729, 0.000000000000000000, -67.53125000204838102 ) ) ;
#33560 = CARTESIAN_POINT ( 'NONE',  ( 9.999999999999998224, 0.000000000000000000, -96.87500000409677625 ) ) ;
#33561 = CARTESIAN_POINT ( 'NONE',  ( 7.644554776091147741E-16, 12.48450537969573659, -185.4687500020483810 ) ) ;
#33562 = CARTESIAN_POINT ( 'NONE',  ( 7.644554776091147741E-16, 12.48450537969573659, -124.1562500020483952 ) ) ;
#33563 = CARTESIAN_POINT ( 'NONE',  ( 10.81189881249999729, 6.242252689847867408, -166.4062500020483810 ) ) ;
#33564 = CARTESIAN_POINT ( 'NONE',  ( -10.81189881249999729, 1.324075727343319199E-15, -48.78125000204838813 ) ) ;
#33565 = CARTESIAN_POINT ( 'NONE',  ( 9.999999999999996447, -5.773502691896262640, -139.0000000040967905 ) ) ;
#33566 = CARTESIAN_POINT ( 'NONE',  ( 9.999999999999998224, 0.000000000000000000, -108.4999999999999858 ) ) ;
#33567 = EDGE_LOOP ( 'NONE', ( #5341, #30933, #13165, #15442 ) ) ;
#33568 = CARTESIAN_POINT ( 'NONE',  ( 10.81189881249999551, -6.242252689847874514, -130.6562500020483810 ) ) ;
#33569 = APPROVAL_PERSON_ORGANIZATION ( #16741, #29638, #42651 ) ;
#33570 = CARTESIAN_POINT ( 'NONE',  ( 10.81189881249999907, 6.242252689847868297, -149.9062500020484094 ) ) ;
#33571 = EDGE_CURVE ( 'NONE', #40862, #21406, #32959, .T. ) ;
#33572 = CARTESIAN_POINT ( 'NONE',  ( -2.293366432827344421E-15, -12.48450537969573659, -190.9062500020483810 ) ) ;
#33573 = CARTESIAN_POINT ( 'NONE',  ( 10.81189881249999907, 6.242252689847868297, -80.71875000204838102 ) ) ;
#33574 = ORIENTED_EDGE ( 'NONE', *, *, #9584, .T. ) ;
#33575 = CARTESIAN_POINT ( 'NONE',  ( -9.999999999999998224, 5.773502691896259087, -52.37499999999997868 ) ) ;
#33576 = CARTESIAN_POINT ( 'NONE',  ( 10.81189881249999551, -6.242252689847874514, -182.9687500020484094 ) ) ;
#33577 = CARTESIAN_POINT ( 'NONE',  ( 7.070501591499377789E-16, 11.54700538379251284, -66.50000000409676204 ) ) ;
#33578 = EDGE_CURVE ( 'NONE', #19929, #32999, #19457, .T. ) ;
#33579 = CARTESIAN_POINT ( 'NONE',  ( 4.999999999999992006, -8.660254037844389075, -171.7500000000000000 ) ) ;
#33580 = LINE ( 'NONE', #23438, #9808 ) ;
#33581 = EDGE_CURVE ( 'NONE', #39928, #39100, #32504, .T. ) ;
#33582 = CARTESIAN_POINT ( 'NONE',  ( 7.644554776091147741E-16, 12.48450537969573659, -73.15625000204836681 ) ) ;
#33583 = CARTESIAN_POINT ( 'NONE',  ( 10.81189881249999729, 0.000000000000000000, -58.53125000204836681 ) ) ;
#33584 = CARTESIAN_POINT ( 'NONE',  ( -10.00000000000000000, -5.773502691896251982, -54.00000000409676204 ) ) ;
#33585 = CARTESIAN_POINT ( 'NONE',  ( -5.405949406250003975, -9.363379034771801557, -7.843750002048343717 ) ) ;
#33586 = CARTESIAN_POINT ( 'NONE',  ( -2.121150477449813534E-15, -11.54700538379251284, -35.37499999999996447 ) ) ;
#33587 = CARTESIAN_POINT ( 'NONE',  ( 7.644554776091147741E-16, 12.48450537969573659, -185.6562500020484094 ) ) ;
#33588 = CARTESIAN_POINT ( 'NONE',  ( 7.644554776091147741E-16, 12.48450537969573659, -7.156250002048364145 ) ) ;
#33589 = CARTESIAN_POINT ( 'NONE',  ( -5.000000000000003553, -8.660254037844383745, -73.37500000409677625 ) ) ;
#33590 = DIRECTION ( 'NONE',  ( -1.000000000000000000, 0.000000000000000000, 0.000000000000000000 ) ) ;
#33591 = CARTESIAN_POINT ( 'NONE',  ( 0.000000000000000000, 0.000000000000000000, -99.99999999999998579 ) ) ;
#33592 =( BOUNDED_CURVE ( )  B_SPLINE_CURVE ( 2, ( #40458, #11330, #11538, #7683, #30999, #21049, #20618 ),
 .UNSPECIFIED., .F., .F. ) 
 B_SPLINE_CURVE_WITH_KNOTS ( ( 3, 2, 2, 3 ),
 ( 0.5298507462686568026, 0.5310945273631841879, 0.5323383084577115731, 0.5335820895522389584 ),
 .UNSPECIFIED. ) 
 CURVE ( )  GEOMETRIC_REPRESENTATION_ITEM ( )  RATIONAL_B_SPLINE_CURVE ( ( 0.9999999999999880096, 0.8660254037844506980, 1.000000000000000000, 0.8660254037844387076, 1.000000000000000000, 0.8660254037844267172, 1.000000000000011990 ) ) 
 REPRESENTATION_ITEM ( '' )  );
#33593 = CARTESIAN_POINT ( 'NONE',  ( 4.999999999999992006, -8.660254037844389075, -137.6250000040967620 ) ) ;
#33595 = ORIENTED_EDGE ( 'NONE', *, *, #15405, .F. ) ;
#33594 = CARTESIAN_POINT ( 'NONE',  ( 7.644554776091147741E-16, 12.48450537969573659, -88.15625000204838102 ) ) ;
#33596 = CARTESIAN_POINT ( 'NONE',  ( -9.999999999999612754, -5.773502691896474914, -181.5000000040967620 ) ) ;
#33597 = EDGE_CURVE ( 'NONE', #468, #39036, #696, .T. ) ;
#33599 = VERTEX_POINT ( 'NONE', #19950 ) ;
#33598 = CARTESIAN_POINT ( 'NONE',  ( 9.999999999999998224, 1.224646799147353059E-15, -99.99999999999998579 ) ) ;
#33600 = EDGE_LOOP ( 'NONE', ( #25432, #37818, #11057, #38302 ) ) ;
#33601 = CARTESIAN_POINT ( 'NONE',  ( 10.81189881249999551, -6.242252689847874514, -28.46875000204837036 ) ) ;
#33602 = CARTESIAN_POINT ( 'NONE',  ( 5.405949406249992428, -9.363379034771808662, -19.78125000204836326 ) ) ;
#33603 = PERSON_AND_ORGANIZATION ( #6799, #4602 ) ;
#33604 = CARTESIAN_POINT ( 'NONE',  ( -10.81189881249999729, 1.324075727343319199E-15, -68.09375000204836681 ) ) ;
#33605 = CARTESIAN_POINT ( 'NONE',  ( 4.999999999999992006, -8.660254037844389075, -83.62500000409677625 ) ) ;
#33606 = CARTESIAN_POINT ( 'NONE',  ( -9.999999999999998224, 5.773502691896259087, -47.87499999999996447 ) ) ;
#33607 = ADVANCED_FACE ( 'NONE', ( #3566 ), #36568, .F. ) ;
#33608 = CARTESIAN_POINT ( 'NONE',  ( -5.405949406250003975, -9.363379034771801557, -186.3437500020483810 ) ) ;
#33609 = CARTESIAN_POINT ( 'NONE',  ( 10.81189881249999729, 0.000000000000000000, -148.3437500020483810 ) ) ;
#33610 = CARTESIAN_POINT ( 'NONE',  ( -9.999999999999998224, 1.224646799147353059E-15, -92.74999999999998579 ) ) ;
#33611 = CARTESIAN_POINT ( 'NONE',  ( 7.070501591499376803E-16, 11.54700538379251284, -132.5000000040967905 ) ) ;
#33612 = CARTESIAN_POINT ( 'NONE',  ( 4.999999999999992006, -8.660254037844389075, -143.6250000040967905 ) ) ;
#33613 = CARTESIAN_POINT ( 'NONE',  ( 4.999999999999992006, -8.660254037844389075, -1.125000004096765593 ) ) ;
#33614 = DIRECTION ( 'NONE',  ( -0.000000000000000000, -0.000000000000000000, 1.000000000000000000 ) ) ;
#33615 = CARTESIAN_POINT ( 'NONE',  ( 10.81189881249999729, 0.000000000000000000, -118.3437500020483810 ) ) ;
#33616 = CARTESIAN_POINT ( 'NONE',  ( 10.81189881249999729, 0.000000000000000000, -90.03125000204838102 ) ) ;
#33617 = CARTESIAN_POINT ( 'NONE',  ( 10.81189881249999551, -6.242252689847874514, -101.9687500020483810 ) ) ;
#33618 = CARTESIAN_POINT ( 'NONE',  ( 10.81189881249999907, 6.242252689847868297, -70.21875000204838102 ) ) ;
#33619 = CARTESIAN_POINT ( 'NONE',  ( -10.81189881249999907, -6.242252689847864744, -78.65625000204839523 ) ) ;
#33620 = CARTESIAN_POINT ( 'NONE',  ( -9.999999999999998224, 1.224646799147353059E-15, -162.1250000040967905 ) ) ;
#33621 = CARTESIAN_POINT ( 'NONE',  ( -10.81189881249999729, 6.242252689847871849, -155.4062500020483810 ) ) ;
#33622 = CARTESIAN_POINT ( 'NONE',  ( -10.81189881249999907, -6.242252689847864744, -171.6562500020484094 ) ) ;
#33623 = FACE_OUTER_BOUND ( 'NONE', #33273, .T. ) ;
#33624 = CARTESIAN_POINT ( 'NONE',  ( 5.000000000000000000, 8.660254037844385522, -108.6250000040967763 ) ) ;
#33625 = CARTESIAN_POINT ( 'NONE',  ( -2.293366432827344421E-15, -12.48450537969573659, -102.2187500020483952 ) ) ;
#33626 = DIRECTION ( 'NONE',  ( 0.000000000000000000, 0.000000000000000000, 1.000000000000000000 ) ) ;
#33627 = CARTESIAN_POINT ( 'NONE',  ( 10.00000000000000000, 5.773502691896255534, -70.87499999999998579 ) ) ;
#33628 = CARTESIAN_POINT ( 'NONE',  ( 10.81189881249999551, -6.242252689847874514, -3.156250002048361036 ) ) ;
#33629 = CARTESIAN_POINT ( 'NONE',  ( -4.999999999999996447, 8.660254037844387298, -91.87500000409677625 ) ) ;
#33630 = CARTESIAN_POINT ( 'NONE',  ( -9.999999999999227285, -5.773502691896698735, -133.5000000040967620 ) ) ;
#33631 = CARTESIAN_POINT ( 'NONE',  ( -10.81189881249999907, -6.242252689847864744, -104.1562500020483668 ) ) ;
#33632 = CARTESIAN_POINT ( 'NONE',  ( 5.405949406249992428, -9.363379034771808662, -84.28125000204838102 ) ) ;
#33633 = ADVANCED_FACE ( 'NONE', ( #29896 ), #335, .F. ) ;
#33634 = CARTESIAN_POINT ( 'NONE',  ( 4.999999999999992006, -8.660254037844389075, -73.12500000409677625 ) ) ;
#33635 = CARTESIAN_POINT ( 'NONE',  ( 5.000000000000000000, 8.660254037844385522, -168.2500000000000000 ) ) ;
#33636 = CARTESIAN_POINT ( 'NONE',  ( 10.81189881249999907, 6.242252689847868297, -35.71875000204835970 ) ) ;
#33637 = VERTEX_POINT ( 'NONE', #9607 ) ;
#33638 = CARTESIAN_POINT ( 'NONE',  ( 10.00000000000000000, 5.773502691896255534, -7.874999999999974243 ) ) ;
#33639 = EDGE_CURVE ( 'NONE', #13865, #15207, #22780, .T. ) ;
#33640 = CARTESIAN_POINT ( 'NONE',  ( -5.405949406250003975, -9.363379034771801557, -26.03125000204836681 ) ) ;
#33641 = CARTESIAN_POINT ( 'NONE',  ( -5.000000000000003553, -8.660254037844383745, -143.5000000000000000 ) ) ;
#33642 = CYLINDRICAL_SURFACE ( 'NONE', #13069, 9.999999999999998224 ) ;
#33643 = CARTESIAN_POINT ( 'NONE',  ( -10.00000000000000000, -5.773502691896251982, -3.000000004096753603 ) ) ;
#33644 = CARTESIAN_POINT ( 'NONE',  ( 5.405949406249999534, 9.363379034771803333, -137.7812500020483810 ) ) ;
#33645 = CARTESIAN_POINT ( 'NONE',  ( 10.00000000000000000, 5.773502691896255534, -190.8750000000000000 ) ) ;
#33646 = CARTESIAN_POINT ( 'NONE',  ( -5.000000000000003553, -8.660254037844383745, -184.3750000040967905 ) ) ;
#33648 = ORIENTED_EDGE ( 'NONE', *, *, #13142, .T. ) ;
#33647 = CARTESIAN_POINT ( 'NONE',  ( -5.405949406250003975, -9.363379034771801557, -114.5312500020483952 ) ) ;
#33649 = CARTESIAN_POINT ( 'NONE',  ( -9.999999999999998224, 1.224646799147353059E-15, -166.2500000000000000 ) ) ;
#33650 = AXIS2_PLACEMENT_3D ( 'NONE', #39529, #16419, #28987 ) ;
#33651 = ORIENTED_EDGE ( 'NONE', *, *, #4339, .F. ) ;
#33652 = ORIENTED_EDGE ( 'NONE', *, *, #38642, .F. ) ;
#33653 = EDGE_CURVE ( 'NONE', #19199, #30761, #23887, .T. ) ;
#33654 = CARTESIAN_POINT ( 'NONE',  ( 5.405949406249992428, -9.363379034771808662, -48.28125000204838813 ) ) ;
#33655 = APPROVAL_ROLE ( '' ) ;
#33656 = CARTESIAN_POINT ( 'NONE',  ( 10.81189881249999907, 6.242252689847868297, -98.71875000204838102 ) ) ;
#33657 = CARTESIAN_POINT ( 'NONE',  ( -10.81189881249999729, 1.324075727343319199E-15, -123.7812500020483952 ) ) ;
#33658 = ORIENTED_EDGE ( 'NONE', *, *, #41105, .F. ) ;
#33659 = CARTESIAN_POINT ( 'NONE',  ( -5.000000000000003553, -8.660254037844383745, -133.0000000000000000 ) ) ;
#33660 = CARTESIAN_POINT ( 'NONE',  ( 5.405949406249999534, 9.363379034771803333, -193.0937500020484094 ) ) ;
#33661 = CARTESIAN_POINT ( 'NONE',  ( -2.293366432827344421E-15, -12.48450537969573659, -175.9062500020483810 ) ) ;
#33662 = CARTESIAN_POINT ( 'NONE',  ( -10.00000000000102496, 5.773502691895664007, -54.25000000409675494 ) ) ;
#33663 = CARTESIAN_POINT ( 'NONE',  ( -2.293366432827344421E-15, -12.48450537969573659, -120.2187500020483952 ) ) ;
#33664 = CARTESIAN_POINT ( 'NONE',  ( -2.293366432827344421E-15, -12.48450537969573659, -96.21875000204839523 ) ) ;
#33665 = CARTESIAN_POINT ( 'NONE',  ( -2.293366432827344421E-15, -12.48450537969573659, -198.2187500020484379 ) ) ;
#33666 = CARTESIAN_POINT ( 'NONE',  ( 5.405949406249992428, -9.363379034771808662, -103.7812500020483810 ) ) ;
#33667 = CARTESIAN_POINT ( 'NONE',  ( -9.999999999999998224, 1.224646799147353059E-15, -189.1250000040967905 ) ) ;
#33668 = CARTESIAN_POINT ( 'NONE',  ( -2.293366432827344421E-15, -12.48450537969573659, -106.7187500020483668 ) ) ;
#33669 = CARTESIAN_POINT ( 'NONE',  ( 10.81189881249999551, -6.242252689847874514, -178.6562500020484094 ) ) ;
#33670 = CARTESIAN_POINT ( 'NONE',  ( 9.999999999999998224, 0.000000000000000000, -0.8750000040967653714 ) ) ;
#33671 = CARTESIAN_POINT ( 'NONE',  ( -10.81189881249999729, 6.242252689847871849, -192.9062500020484094 ) ) ;
#33672 = CARTESIAN_POINT ( 'NONE',  ( -5.405949406250003975, -9.363379034771801557, -57.34375000204835970 ) ) ;
#33673 = CARTESIAN_POINT ( 'NONE',  ( 5.405949406249992428, -9.363379034771808662, -39.09375000204837391 ) ) ;
#33674 = CARTESIAN_POINT ( 'NONE',  ( 4.999999999999992006, -8.660254037844389075, -170.6250000040968189 ) ) ;
#33675 = CARTESIAN_POINT ( 'NONE',  ( 10.81189881249999551, -6.242252689847874514, -7.656250002048367698 ) ) ;
#33676 = CARTESIAN_POINT ( 'NONE',  ( 10.81189881249999551, -6.242252689847874514, -23.96875000204837391 ) ) ;
#33677 = CARTESIAN_POINT ( 'NONE',  ( 10.81189881249999907, 6.242252689847868297, -131.7187500020483810 ) ) ;
#33678 = CARTESIAN_POINT ( 'NONE',  ( -10.00000000000000000, -5.773502691896251982, -107.6249999999999858 ) ) ;
#33679 = CARTESIAN_POINT ( 'NONE',  ( -5.405949406250003975, -9.363379034771801557, -30.53125000204837036 ) ) ;
#33680 = AXIS2_PLACEMENT_3D ( 'NONE', #39793, #39373, #122 ) ;
#33681 =( BOUNDED_CURVE ( )  B_SPLINE_CURVE ( 2, ( #32606, #13559, #3030, #16797, #29996, #442, #36042 ),
 .UNSPECIFIED., .F., .F. ) 
 B_SPLINE_CURVE_WITH_KNOTS ( ( 3, 2, 2, 3 ),
 ( 0.2164179104477612636, 0.2176616915422886489, 0.2189054726368160064, 0.2201492537313433639 ),
 .UNSPECIFIED. ) 
 CURVE ( )  GEOMETRIC_REPRESENTATION_ITEM ( )  RATIONAL_B_SPLINE_CURVE ( ( 0.9999999999999910072, 0.8660254037844477004, 1.000000000000000000, 0.8660254037844387076, 1.000000000000000000, 0.8660254037844297148, 1.000000000000008882 ) ) 
 REPRESENTATION_ITEM ( '' )  );
#33682 = DIRECTION ( 'NONE',  ( 0.000000000000000000, 0.000000000000000000, -1.000000000000000000 ) ) ;
#33683 = CARTESIAN_POINT ( 'NONE',  ( -9.999999999999998224, 1.224646799147353059E-15, -62.74999999999997158 ) ) ;
#33684 = CARTESIAN_POINT ( 'NONE',  ( -5.405949406249996869, 9.363379034771805109, -122.5312500020483952 ) ) ;
#33685 = CARTESIAN_POINT ( 'NONE',  ( 10.81189881249999729, 0.000000000000000000, -106.5312500020483810 ) ) ;
#33686 = ORIENTED_EDGE ( 'NONE', *, *, #4762, .F. ) ;
#33687 = CARTESIAN_POINT ( 'NONE',  ( -9.999999999999998224, 1.224646799147353059E-15, -12.12500000409674783 ) ) ;
#33688 = CARTESIAN_POINT ( 'NONE',  ( -9.999999999999998224, 1.224646799147353059E-15, -102.1250000040967905 ) ) ;
#33689 = CARTESIAN_POINT ( 'NONE',  ( 9.999999999999998224, 0.000000000000000000, -135.8750000040967905 ) ) ;
#33690 = CARTESIAN_POINT ( 'NONE',  ( -10.81189881249999907, -6.242252689847864744, -61.96875000204838102 ) ) ;
#33691 = EDGE_LOOP ( 'NONE', ( #25845, #36484, #34214, #25325 ) ) ;
#33692 = CARTESIAN_POINT ( 'NONE',  ( 4.999999999999992006, -8.660254037844389075, -36.74999999999997868 ) ) ;
#33693 = CARTESIAN_POINT ( 'NONE',  ( -2.293366432827344421E-15, -12.48450537969573659, -39.40625000204835260 ) ) ;
#33694 = CARTESIAN_POINT ( 'NONE',  ( 9.999999999999996447, -5.773502691896262640, -25.00000000409677625 ) ) ;
#33695 = CARTESIAN_POINT ( 'NONE',  ( -9.999999999999998224, 1.224646799147353059E-15, -57.12500000409676204 ) ) ;
#33696 = EDGE_CURVE ( 'NONE', #4287, #40862, #1834, .T. ) ;
#33697 = CARTESIAN_POINT ( 'NONE',  ( -2.293366432827344421E-15, -12.48450537969573659, -142.9062500020483810 ) ) ;
#33698 = LINE ( 'NONE', #7147, #41715 ) ;
#33699 = ORIENTED_EDGE ( 'NONE', *, *, #34141, .T. ) ;
#33700 = ORIENTED_EDGE ( 'NONE', *, *, #31560, .T. ) ;
#33701 = AXIS2_PLACEMENT_3D ( 'NONE', #31136, #28112, #25090 ) ;
#33702 = CARTESIAN_POINT ( 'NONE',  ( -2.121150477449813534E-15, -11.54700538379251284, -106.2500000040967905 ) ) ;
#33703 = EDGE_CURVE ( 'NONE', #25373, #13583, #35040, .T. ) ;
#33704 = CARTESIAN_POINT ( 'NONE',  ( -5.000000000000003553, -8.660254037844383745, -55.37500000409675494 ) ) ;
#33705 = CARTESIAN_POINT ( 'NONE',  ( 10.81189881249999907, 6.242252689847868297, -164.7187500020483810 ) ) ;
#33706 = CARTESIAN_POINT ( 'NONE',  ( -10.81189881249999729, 1.324075727343319199E-15, -195.7812500020484094 ) ) ;
#33707 = CARTESIAN_POINT ( 'NONE',  ( 10.81189881249999907, 6.242252689847868297, -17.71875000204836681 ) ) ;
#33708 = FACE_OUTER_BOUND ( 'NONE', #27629, .T. ) ;
#33709 = CARTESIAN_POINT ( 'NONE',  ( 5.405949406249999534, 9.363379034771803333, -145.0937500020483810 ) ) ;
#33710 = CARTESIAN_POINT ( 'NONE',  ( 7.644554776091147741E-16, 12.48450537969573659, -135.9687500020483810 ) ) ;
#33711 = CARTESIAN_POINT ( 'NONE',  ( -10.81189881249999907, -6.242252689847864744, -107.1562500020483952 ) ) ;
#33712 = CARTESIAN_POINT ( 'NONE',  ( -5.405949406250003975, -9.363379034771801557, -114.3437500020483810 ) ) ;
#33713 = CARTESIAN_POINT ( 'NONE',  ( 10.00000000000000000, 5.773502691896255534, -192.7500000040968189 ) ) ;
#33714 = CARTESIAN_POINT ( 'NONE',  ( 5.405949406249992428, -9.363379034771808662, -121.7812500020483952 ) ) ;
#33715 = CARTESIAN_POINT ( 'NONE',  ( 10.81189881249999551, -6.242252689847874514, -8.968750002048359704 ) ) ;
#33716 = CARTESIAN_POINT ( 'NONE',  ( -10.81189881249999729, 6.242252689847871849, -126.7187500020483810 ) ) ;
#33717 = CARTESIAN_POINT ( 'NONE',  ( -9.999999999999872102, -5.773502691896326589, -166.5000000040967905 ) ) ;
#33718 =( BOUNDED_CURVE ( )  B_SPLINE_CURVE ( 2, ( #41659, #15111, #12095, #41445, #25077, #38222, #25288 ),
 .UNSPECIFIED., .F., .F. ) 
 B_SPLINE_CURVE_WITH_KNOTS ( ( 3, 2, 2, 3 ),
 ( 0.05970149253731348721, 0.06094527363184085167, 0.06218905472636821613, 0.06343283582089558059 ),
 .UNSPECIFIED. ) 
 CURVE ( )  GEOMETRIC_REPRESENTATION_ITEM ( )  RATIONAL_B_SPLINE_CURVE ( ( 0.9999999999999940048, 0.8660254037844447028, 1.000000000000000000, 0.8660254037844387076, 1.000000000000000000, 0.8660254037844327124, 1.000000000000005995 ) ) 
 REPRESENTATION_ITEM ( '' )  );
#33719 = AXIS2_PLACEMENT_3D ( 'NONE', #2410, #28311, #18795 ) ;
#33720 = CARTESIAN_POINT ( 'NONE',  ( -9.999999999999998224, 1.224646799147353059E-15, -124.6250000040967763 ) ) ;
#33721 = CARTESIAN_POINT ( 'NONE',  ( 7.070501591499377789E-16, 11.54700538379251284, -154.6250000000000284 ) ) ;
#33722 = CARTESIAN_POINT ( 'NONE',  ( 10.00000000000000000, 5.773502691896255534, -18.37499999999997513 ) ) ;
#33723 = CARTESIAN_POINT ( 'NONE',  ( 5.405949406249992428, -9.363379034771808662, -81.09375000204838102 ) ) ;
#33724 = CARTESIAN_POINT ( 'NONE',  ( -10.81189881249999729, 1.324075727343319199E-15, -63.59375000204836681 ) ) ;
#33725 = CARTESIAN_POINT ( 'NONE',  ( -9.999999999999742428, -5.773502691896402084, -117.0000000040967763 ) ) ;
#33726 = CARTESIAN_POINT ( 'NONE',  ( 7.644554776091147741E-16, 12.48450537969573659, -40.15625000204836681 ) ) ;
#33727 = CARTESIAN_POINT ( 'NONE',  ( 5.405949406249992428, -9.363379034771808662, -46.59375000204838102 ) ) ;
#33728 = CYLINDRICAL_SURFACE ( 'NONE', #10950, 9.999999999999998224 ) ;
#33729 = CARTESIAN_POINT ( 'NONE',  ( -5.405949406250003975, -9.363379034771801557, -156.3437500020483810 ) ) ;
#33730 = CARTESIAN_POINT ( 'NONE',  ( -10.00000000000000000, -5.773502691896251982, -133.1250000000000000 ) ) ;
#33731 = CARTESIAN_POINT ( 'NONE',  ( -5.405949406249996869, 9.363379034771805109, -128.5312500020484094 ) ) ;
#33732 = CARTESIAN_POINT ( 'NONE',  ( 8.154330677275039463, 6.787768574218738138, -180.0000000000000000 ) ) ;
#33733 = CARTESIAN_POINT ( 'NONE',  ( 5.000000000000000000, 8.660254037844385522, -81.24999999999998579 ) ) ;
#33734 = CARTESIAN_POINT ( 'NONE',  ( 7.644554776091147741E-16, 12.48450537969573659, -20.65625000204838457 ) ) ;
#33735 = ORIENTED_EDGE ( 'NONE', *, *, #37813, .T. ) ;
#33736 =( BOUNDED_CURVE ( )  B_SPLINE_CURVE ( 2, ( #37190, #27707, #17330, #17538, #1600, #20790, #27493 ),
 .UNSPECIFIED., .F., .F. ) 
 B_SPLINE_CURVE_WITH_KNOTS ( ( 3, 2, 2, 3 ),
 ( 0.6604477611940301474, 0.6616915422885575326, 0.6629353233830848069, 0.6641791044776121922 ),
 .UNSPECIFIED. ) 
 CURVE ( )  GEOMETRIC_REPRESENTATION_ITEM ( )  RATIONAL_B_SPLINE_CURVE ( ( 0.9999999999999641398, 0.8660254037844745678, 1.000000000000000000, 0.8660254037844387076, 1.000000000000000000, 0.8660254037844148378, 1.000000000000023981 ) ) 
 REPRESENTATION_ITEM ( '' )  );
#33737 = CARTESIAN_POINT ( 'NONE',  ( 10.81189881249999551, -6.242252689847874514, -109.6562500020483810 ) ) ;
#33738 = CARTESIAN_POINT ( 'NONE',  ( -9.999999999999998224, 1.224646799147353059E-15, -121.6250000040967905 ) ) ;
#33739 = CARTESIAN_POINT ( 'NONE',  ( -9.999999999999998224, 1.224646799147353059E-15, -185.7500000000000000 ) ) ;
#33740 = CARTESIAN_POINT ( 'NONE',  ( -4.999999999999996447, 8.660254037844387298, -30.37500000409676204 ) ) ;
#33741 = CARTESIAN_POINT ( 'NONE',  ( -9.999999999999998224, 1.224646799147353059E-15, -9.125000004096744277 ) ) ;
#33742 = CARTESIAN_POINT ( 'NONE',  ( 10.81189881249999907, 6.242252689847868297, -53.90625000204838102 ) ) ;
#33743 = EDGE_CURVE ( 'NONE', #32436, #10245, #31331, .T. ) ;
#33744 = CARTESIAN_POINT ( 'NONE',  ( -9.999999999999227285, -5.773502691896698735, -136.1249999999999716 ) ) ;
#33745 = CARTESIAN_POINT ( 'NONE',  ( 10.81189881249999729, 0.000000000000000000, -156.0312500020484094 ) ) ;
#33746 = CARTESIAN_POINT ( 'NONE',  ( -2.293366432827344421E-15, -12.48450537969573659, -132.2187500020483810 ) ) ;
#33747 = CARTESIAN_POINT ( 'NONE',  ( 9.999999999999479527, 5.773502691896553074, -109.8749999999999716 ) ) ;
#33748 = ORIENTED_EDGE ( 'NONE', *, *, #33039, .T. ) ;
#33749 = CARTESIAN_POINT ( 'NONE',  ( 9.999999999999998224, 0.000000000000000000, -164.3750000040967905 ) ) ;
#33750 = ORIENTED_EDGE ( 'NONE', *, *, #5122, .F. ) ;
#33751 = AXIS2_PLACEMENT_3D ( 'NONE', #29487, #12633, #25620 ) ;
#33752 = ORIENTED_EDGE ( 'NONE', *, *, #35208, .F. ) ;
#33753 = APPROVAL_ROLE ( '' ) ;
#33755 = ORIENTED_EDGE ( 'NONE', *, *, #36279, .F. ) ;
#33754 = CARTESIAN_POINT ( 'NONE',  ( -10.81189881249999729, 6.242252689847871849, -114.7187500020483810 ) ) ;
#33756 = ADVANCED_FACE ( 'NONE', ( #33356 ), #24280, .T. ) ;
#33757 = CARTESIAN_POINT ( 'NONE',  ( 9.999999999999998224, 0.000000000000000000, -129.8750000040967905 ) ) ;
#33758 = CARTESIAN_POINT ( 'NONE',  ( 7.644554776091147741E-16, 12.48450537969573659, -188.4687500020484094 ) ) ;
#33759 = CARTESIAN_POINT ( 'NONE',  ( 5.405949406249992428, -9.363379034771808662, -39.09375000204837391 ) ) ;
#33760 = CARTESIAN_POINT ( 'NONE',  ( 7.070501591499376803E-16, 11.54700538379251284, -62.00000000409677625 ) ) ;
#33761 = CARTESIAN_POINT ( 'NONE',  ( -10.81189881249999729, 6.242252689847871849, -177.7187500020484379 ) ) ;
#33762 = CARTESIAN_POINT ( 'NONE',  ( 5.405949406249999534, 9.363379034771803333, -161.5937500020484094 ) ) ;
#33763 = CARTESIAN_POINT ( 'NONE',  ( -2.293366432827344421E-15, -12.48450537969573659, -138.2187500020483810 ) ) ;
#33764 = CARTESIAN_POINT ( 'NONE',  ( 10.81189881249999729, 0.000000000000000000, -163.3437500020484094 ) ) ;
#33765 = CARTESIAN_POINT ( 'NONE',  ( -4.999999999999996447, 8.660254037844387298, -133.8750000040967905 ) ) ;
#33766 = CARTESIAN_POINT ( 'NONE',  ( -9.999999999999998224, 1.224646799147353059E-15, -35.74999999999997868 ) ) ;
#33767 = CARTESIAN_POINT ( 'NONE',  ( 9.999999999999996447, -5.773502691896262640, -179.1250000000000284 ) ) ;
#33768 = AXIS2_PLACEMENT_3D ( 'NONE', #30357, #16944, #30142 ) ;
#33769 = CARTESIAN_POINT ( 'NONE',  ( 5.405949406249999534, 9.363379034771803333, -89.59375000204838102 ) ) ;
#33770 = PLANE ( 'NONE',  #25864 ) ;
#33771 = CARTESIAN_POINT ( 'NONE',  ( 10.81189881249999551, -6.242252689847874514, -66.15625000204839523 ) ) ;
#33772 = CARTESIAN_POINT ( 'NONE',  ( 9.999999999999998224, 0.000000000000000000, -123.8750000040967905 ) ) ;
#33773 = CARTESIAN_POINT ( 'NONE',  ( -2.293366432827344421E-15, -12.48450537969573659, -175.7187500020483810 ) ) ;
#33774 = CARTESIAN_POINT ( 'NONE',  ( 5.405949406249992428, -9.363379034771808662, -124.7812500020483952 ) ) ;
#33775 = CARTESIAN_POINT ( 'NONE',  ( 5.405949406249999534, 9.363379034771803333, -151.2812500020484094 ) ) ;
#33776 = CARTESIAN_POINT ( 'NONE',  ( -5.405949406250003975, -9.363379034771801557, -51.53125000204835970 ) ) ;
#33777 = CARTESIAN_POINT ( 'NONE',  ( 9.999999999999998224, 0.000000000000000000, -128.3750000040967905 ) ) ;
#33778 = CARTESIAN_POINT ( 'NONE',  ( -4.999999999999996447, 8.660254037844387298, -107.9999999999999858 ) ) ;
#33779 = ORIENTED_EDGE ( 'NONE', *, *, #19100, .T. ) ;
#33780 = CARTESIAN_POINT ( 'NONE',  ( -5.405949406249996869, 9.363379034771805109, -137.5312500020484094 ) ) ;
#33781 = CARTESIAN_POINT ( 'NONE',  ( -9.999999999999998224, 1.224646799147353059E-15, -159.1250000040967905 ) ) ;
#33782 = CARTESIAN_POINT ( 'NONE',  ( 10.81189881249999729, 0.000000000000000000, -151.5312500020484094 ) ) ;
#33783 = CARTESIAN_POINT ( 'NONE',  ( -10.81189881249999907, -6.242252689847864744, -185.1562500020484094 ) ) ;
#33784 = CARTESIAN_POINT ( 'NONE',  ( -2.293366432827344421E-15, -12.48450537969573659, -85.71875000204838102 ) ) ;
#33785 = ORIENTED_EDGE ( 'NONE', *, *, #24077, .F. ) ;
#33786 = CARTESIAN_POINT ( 'NONE',  ( -5.000000000000003553, -8.660254037844383745, -51.99999999999996447 ) ) ;
#33787 = CARTESIAN_POINT ( 'NONE',  ( -5.405949406249996869, 9.363379034771805109, -182.3437500020483810 ) ) ;
#33788 = CARTESIAN_POINT ( 'NONE',  ( -2.121150477449813534E-15, -11.54700538379251284, -67.25000000409676204 ) ) ;
#33789 = LINE ( 'NONE', #13900, #3784 ) ;
#33790 = CARTESIAN_POINT ( 'NONE',  ( -9.999999999999872102, -5.773502691896326589, -158.6250000000000284 ) ) ;
#33791 = CARTESIAN_POINT ( 'NONE',  ( 10.81189881249999729, 0.000000000000000000, -76.53125000204838102 ) ) ;
#33792 = CARTESIAN_POINT ( 'NONE',  ( 5.405949406249999534, 9.363379034771803333, -61.28125000204837391 ) ) ;
#33793 = CARTESIAN_POINT ( 'NONE',  ( -5.000000000000003553, -8.660254037844383745, -52.37500000409675494 ) ) ;
#33794 = CARTESIAN_POINT ( 'NONE',  ( -10.81189881249999729, 1.324075727343319199E-15, -14.09375000204834905 ) ) ;
#33795 = CYLINDRICAL_SURFACE ( 'NONE', #6935, 9.999999999999998224 ) ;
#33796 = CARTESIAN_POINT ( 'NONE',  ( 5.405949406249999534, 9.363379034771803333, -173.7812500020484094 ) ) ;
#33797 = CARTESIAN_POINT ( 'NONE',  ( 5.405949406249992428, -9.363379034771808662, -7.781250002048350822 ) ) ;
#33798 = FACE_OUTER_BOUND ( 'NONE', #4441, .T. ) ;
#33799 = CARTESIAN_POINT ( 'NONE',  ( -9.999999999999868550, 5.773502691896333694, -175.7500000040967905 ) ) ;
#33800 =( BOUNDED_CURVE ( )  B_SPLINE_CURVE ( 2, ( #25618, #3159, #6188, #32938, #35960, #39398, #35548 ),
 .UNSPECIFIED., .F., .F. ) 
 B_SPLINE_CURVE_WITH_KNOTS ( ( 3, 2, 2, 3 ),
 ( 0.6641791044776121922, 0.6654228855721395774, 0.6666666666666668517, 0.6679104477611942370 ),
 .UNSPECIFIED. ) 
 CURVE ( )  GEOMETRIC_REPRESENTATION_ITEM ( )  RATIONAL_B_SPLINE_CURVE ( ( 0.9999999999999761302, 0.8660254037844625774, 1.000000000000000000, 0.8660254037844387076, 1.000000000000000000, 0.8660254037844148378, 1.000000000000023981 ) ) 
 REPRESENTATION_ITEM ( '' )  );
#33801 = LINE ( 'NONE', #23664, #1523 ) ;
#33802 = DIRECTION ( 'NONE',  ( 1.000000000000000000, 0.000000000000000000, 0.000000000000000000 ) ) ;
#33803 = CARTESIAN_POINT ( 'NONE',  ( 10.00000000000012257, -5.773502691896187144, -169.0000000040967620 ) ) ;
#33804 = AXIS2_PLACEMENT_3D ( 'NONE', #42427, #15877, #38991 ) ;
#33806 = ORIENTED_EDGE ( 'NONE', *, *, #23049, .T. ) ;
#33805 = CARTESIAN_POINT ( 'NONE',  ( -10.81189881249999729, 6.242252689847871849, -83.40625000204836681 ) ) ;
#33807 = CARTESIAN_POINT ( 'NONE',  ( -9.999999999999998224, 1.224646799147353059E-15, -24.12500000409675849 ) ) ;
#33809 = VERTEX_POINT ( 'NONE', #13668 ) ;
#33808 = CARTESIAN_POINT ( 'NONE',  ( -9.999999999999479527, -5.773502691896549521, -123.0000000040967763 ) ) ;
#33810 = ORIENTED_EDGE ( 'NONE', *, *, #21970, .T. ) ;
#33811 = CARTESIAN_POINT ( 'NONE',  ( -10.81189881249999907, -6.242252689847864744, -22.96875000204837747 ) ) ;
#33812 = CARTESIAN_POINT ( 'NONE',  ( -10.81189881249999729, 6.242252689847871849, -11.40625000204835438 ) ) ;
#33813 = CARTESIAN_POINT ( 'NONE',  ( 10.81189881249999551, -6.242252689847874514, -67.46875000204838102 ) ) ;
#33814 = CARTESIAN_POINT ( 'NONE',  ( 0.000000000000000000, 0.000000000000000000, -200.0000000000000000 ) ) ;
#33815 = ADVANCED_FACE ( 'NONE', ( #3983 ), #34206, .F. ) ;
#33816 = CARTESIAN_POINT ( 'NONE',  ( 4.999999999999992006, -8.660254037844389075, -44.24999999999998579 ) ) ;
#33817 = CARTESIAN_POINT ( 'NONE',  ( -10.81189881249999907, -6.242252689847864744, -187.9687500020484094 ) ) ;
#33818 = EDGE_CURVE ( 'NONE', #20035, #39731, #13881, .T. ) ;
#33819 = CARTESIAN_POINT ( 'NONE',  ( 10.81189881249999551, -6.242252689847874514, -167.9687500020483810 ) ) ;
#33820 = CARTESIAN_POINT ( 'NONE',  ( 9.999999999999998224, 0.000000000000000000, -200.0000000000000000 ) ) ;
#33821 = CARTESIAN_POINT ( 'NONE',  ( -10.00000000000001421, 5.773502691896249317, -199.3750000000000000 ) ) ;
#33822 = CARTESIAN_POINT ( 'NONE',  ( 9.999999999999479527, 5.773502691896553074, -71.25000000409674783 ) ) ;
#33823 = CARTESIAN_POINT ( 'NONE',  ( -2.121150477449813534E-15, -11.54700538379251284, -104.3749999999999858 ) ) ;
#33824 = CARTESIAN_POINT ( 'NONE',  ( -9.999999999999998224, 1.224646799147353059E-15, -90.12500000409677625 ) ) ;
#33825 = CARTESIAN_POINT ( 'NONE',  ( 10.81189881249999729, 0.000000000000000000, -112.3437500020483810 ) ) ;
#33826 = CARTESIAN_POINT ( 'NONE',  ( 9.999999999999998224, 0.000000000000000000, -109.9999999999999858 ) ) ;
#33827 = CARTESIAN_POINT ( 'NONE',  ( -5.405949406250003975, -9.363379034771801557, -93.53125000204838102 ) ) ;
#33828 = CARTESIAN_POINT ( 'NONE',  ( 7.644554776091147741E-16, 12.48450537969573659, -98.46875000204838102 ) ) ;
#33829 = CARTESIAN_POINT ( 'NONE',  ( 5.405949406249999534, 9.363379034771803333, -67.09375000204836681 ) ) ;
#33830 = CARTESIAN_POINT ( 'NONE',  ( 5.405949406249992428, -9.363379034771808662, -79.78125000204838102 ) ) ;
#33831 = CARTESIAN_POINT ( 'NONE',  ( -10.00000000000000000, -5.773502691896251982, -151.5000000040967905 ) ) ;
#33832 = CARTESIAN_POINT ( 'NONE',  ( -10.81189881249999729, 1.324075727343319199E-15, -161.2812500020484094 ) ) ;
#33833 = CARTESIAN_POINT ( 'NONE',  ( -10.81189881249999729, 6.242252689847871849, -174.9062500020483810 ) ) ;
#33834 = CC_DESIGN_APPROVAL ( #11985, ( #19626 ) ) ;
#33835 = CARTESIAN_POINT ( 'NONE',  ( 10.81189881249999729, 0.000000000000000000, -1.343750002048366143 ) ) ;
#33836 = FACE_OUTER_BOUND ( 'NONE', #28930, .T. ) ;
#33837 = CARTESIAN_POINT ( 'NONE',  ( 7.644554776091147741E-16, 12.48450537969573659, -107.4687500020483668 ) ) ;
#33838 = CARTESIAN_POINT ( 'NONE',  ( -9.999999999999998224, 5.773502691896259087, -70.37499999999998579 ) ) ;
#33839 = CARTESIAN_POINT ( 'NONE',  ( 10.81189881249999729, 0.000000000000000000, -4.531250002048375691 ) ) ;
#33840 = CARTESIAN_POINT ( 'NONE',  ( -4.999999999999996447, 8.660254037844387298, -93.37500000409677625 ) ) ;
#33841 = AXIS2_PLACEMENT_3D ( 'NONE', #40038, #362, #573 ) ;
#33842 = PLANE ( 'NONE',  #12064 ) ;
#33843 = CARTESIAN_POINT ( 'NONE',  ( 10.81189881249999551, -6.242252689847874514, -99.15625000204838102 ) ) ;
#33844 = CARTESIAN_POINT ( 'NONE',  ( 10.81189881249999729, 0.000000000000000000, -85.53125000204838102 ) ) ;
#33845 =( BOUNDED_CURVE ( )  B_SPLINE_CURVE ( 2, ( #10261, #19978, #13695, #17154, #10051, #33799, #23231 ),
 .UNSPECIFIED., .F., .F. ) 
 B_SPLINE_CURVE_WITH_KNOTS ( ( 3, 2, 2, 3 ),
 ( 0.1119402985074627876, 0.1131840796019901035, 0.1144278606965174333, 0.1156716417910447492 ),
 .UNSPECIFIED. ) 
 CURVE ( )  GEOMETRIC_REPRESENTATION_ITEM ( )  RATIONAL_B_SPLINE_CURVE ( ( 0.9999999999999894529, 0.8660254037844491437, 1.000000000000000000, 0.8660254037844387076, 1.000000000000000000, 0.8660254037844417052, 0.9999999999999970024 ) ) 
 REPRESENTATION_ITEM ( '' )  );
#33846 = CARTESIAN_POINT ( 'NONE',  ( -2.121150477449813534E-15, -11.54700538379251284, -76.25000000409677625 ) ) ;
#33847 = DIRECTION ( 'NONE',  ( -0.000000000000000000, -0.000000000000000000, 1.000000000000000000 ) ) ;
#33848 = CARTESIAN_POINT ( 'NONE',  ( -10.81189881249999729, 6.242252689847871849, -32.21875000204835260 ) ) ;
#33849 = VERTEX_POINT ( 'NONE', #37425 ) ;
#33850 = CARTESIAN_POINT ( 'NONE',  ( -9.999999999999998224, 1.224646799147353059E-15, -2.749999999999974687 ) ) ;
#33851 = CARTESIAN_POINT ( 'NONE',  ( 7.644554776091147741E-16, 12.48450537969573659, -25.15625000204837747 ) ) ;
#33852 = CARTESIAN_POINT ( 'NONE',  ( 5.405949406249992428, -9.363379034771808662, -13.59375000204834905 ) ) ;
#33853 = CARTESIAN_POINT ( 'NONE',  ( 9.999999999999742428, 5.773502691896404748, -139.8749999999999716 ) ) ;
#33854 = CARTESIAN_POINT ( 'NONE',  ( 4.999999999999992006, -8.660254037844389075, -5.625000004096769146 ) ) ;
#33855 = CARTESIAN_POINT ( 'NONE',  ( -10.81189881249999907, -6.242252689847864744, -134.1562500020483810 ) ) ;
#33856 = CARTESIAN_POINT ( 'NONE',  ( 4.999999999999992006, -8.660254037844389075, -179.2500000000000284 ) ) ;
#33857 = DIRECTION ( 'NONE',  ( 3.186890520727785033E-16, -0.7071067811865493491, 0.7071067811865456854 ) ) ;
#33859 = VERTEX_POINT ( 'NONE', #14302 ) ;
#33858 = CARTESIAN_POINT ( 'NONE',  ( -5.405949406249996869, 9.363379034771805109, -113.5312500020483952 ) ) ;
#33860 = DIRECTION ( 'NONE',  ( -0.000000000000000000, -0.000000000000000000, -1.000000000000000000 ) ) ;
#33861 = EDGE_LOOP ( 'NONE', ( #34000, #29383, #32954, #42371 ) ) ;
#33862 = ORIENTED_EDGE ( 'NONE', *, *, #645, .F. ) ;
#33863 = CARTESIAN_POINT ( 'NONE',  ( 7.644554776091147741E-16, 12.48450537969573659, -40.15625000204836681 ) ) ;
#33864 = APPROVAL_ROLE ( '' ) ;
#33865 = LOCAL_TIME ( 11, 57, 6.000000000000000000, #42486 ) ;
#33866 = CARTESIAN_POINT ( 'NONE',  ( -5.405949406249996869, 9.363379034771805109, -96.84375000204838102 ) ) ;
#33867 = CARTESIAN_POINT ( 'NONE',  ( 9.999999999999998224, 0.000000000000000000, -200.0000000000000000 ) ) ;
#33868 = EDGE_CURVE ( 'NONE', #23753, #22977, #41759, .T. ) ;
#33869 = CARTESIAN_POINT ( 'NONE',  ( 2.194755657887257350, 10.56074294295119387, -99.99999999999997158 ) ) ;
#33870 = CARTESIAN_POINT ( 'NONE',  ( 7.644554776091147741E-16, 12.48450537969573659, -198.9687500020484094 ) ) ;
#33871 = EDGE_CURVE ( 'NONE', #25200, #22602, #37360, .T. ) ;
#33872 = CARTESIAN_POINT ( 'NONE',  ( -10.81189881249999729, 1.324075727343319199E-15, -174.7812500020484094 ) ) ;
#33873 = CARTESIAN_POINT ( 'NONE',  ( -9.999999999999998224, 1.224646799147353059E-15, -137.7499999999999716 ) ) ;
#33874 = EDGE_CURVE ( 'NONE', #16734, #9326, #39208, .T. ) ;
#33875 = CARTESIAN_POINT ( 'NONE',  ( -5.405949406250003975, -9.363379034771801557, -127.8437500020483952 ) ) ;
#33876 = PRODUCT_DEFINITION_SHAPE ( 'NONE', 'NONE',  #20655 ) ;
#33877 = CC_DESIGN_DATE_AND_TIME_ASSIGNMENT ( #3872, #10115, ( #14057 ) ) ;
#33878 = CARTESIAN_POINT ( 'NONE',  ( -2.293366432827344421E-15, -12.48450537969573659, -94.71875000204838102 ) ) ;
#33879 = CARTESIAN_POINT ( 'NONE',  ( 7.644554776091147741E-16, 12.48450537969573659, -198.9687500020484094 ) ) ;
#33880 = CARTESIAN_POINT ( 'NONE',  ( -10.81189881249999907, -6.242252689847864744, -104.1562500020483668 ) ) ;
#33881 = CARTESIAN_POINT ( 'NONE',  ( -9.999999999999998224, 5.773502691896259087, -184.7500000040968189 ) ) ;
#33882 = CARTESIAN_POINT ( 'NONE',  ( 10.81189881249999551, -6.242252689847874514, -107.9687500020483810 ) ) ;
#33883 = CARTESIAN_POINT ( 'NONE',  ( 5.405949406249999534, 9.363379034771803333, -176.7812500020484094 ) ) ;
#33884 = CARTESIAN_POINT ( 'NONE',  ( -9.999999999999998224, 1.224646799147353059E-15, -179.7500000000000284 ) ) ;
#33885 = CARTESIAN_POINT ( 'NONE',  ( -5.405949406250003975, -9.363379034771801557, -179.0312500020483810 ) ) ;
#33886 = CARTESIAN_POINT ( 'NONE',  ( 5.405949406249992428, -9.363379034771808662, -195.2812500020484094 ) ) ;
#33887 = CARTESIAN_POINT ( 'NONE',  ( -2.293366432827344421E-15, -12.48450537969573659, -49.71875000204835970 ) ) ;
#33888 = CARTESIAN_POINT ( 'NONE',  ( 7.644554776091147741E-16, 12.48450537969573659, -44.46875000204836681 ) ) ;
#33889 = CARTESIAN_POINT ( 'NONE',  ( 7.070501591499377789E-16, 11.54700538379251284, -171.5000000040967905 ) ) ;
#33890 = CARTESIAN_POINT ( 'NONE',  ( 5.405949406249992428, -9.363379034771808662, -13.78125000204835615 ) ) ;
#33891 = CARTESIAN_POINT ( 'NONE',  ( 7.644554776091147741E-16, 12.48450537969573659, -23.46875000204837391 ) ) ;
#33892 = CARTESIAN_POINT ( 'NONE',  ( -2.121150477449813534E-15, -11.54700538379251284, -92.75000000409677625 ) ) ;
#33893 = CARTESIAN_POINT ( 'NONE',  ( 5.405949406249999534, 9.363379034771803333, -131.5937500020483810 ) ) ;
#33894 = CARTESIAN_POINT ( 'NONE',  ( 5.000000000000000000, 8.660254037844385522, -96.24999999999998579 ) ) ;
#33895 = CARTESIAN_POINT ( 'NONE',  ( -10.81189881249999907, -6.242252689847864744, -29.15625000204835970 ) ) ;
#33896 = CARTESIAN_POINT ( 'NONE',  ( -10.00000000000000000, -5.773502691896251982, -112.5000000040967905 ) ) ;
#33897 = CARTESIAN_POINT ( 'NONE',  ( 9.999999999999994671, -5.773502691896262640, -168.6250000000000000 ) ) ;
#33898 = CARTESIAN_POINT ( 'NONE',  ( -2.121150477449813534E-15, -11.54700538379251284, -59.37499999999998579 ) ) ;
#33899 = CARTESIAN_POINT ( 'NONE',  ( 10.81189881249999551, -6.242252689847874514, -126.1562500020483810 ) ) ;
#33900 = CARTESIAN_POINT ( 'NONE',  ( 5.405949406249999534, 9.363379034771803333, -109.2812500020483810 ) ) ;
#33901 = EDGE_LOOP ( 'NONE', ( #41984, #4174, #217, #1974 ) ) ;
#33902 = CIRCLE ( 'NONE', #15265, 20.00000000000000355 ) ;
#33903 = CARTESIAN_POINT ( 'NONE',  ( -9.999999999999998224, 1.224646799147353059E-15, -139.2499999999999716 ) ) ;
#33904 = CARTESIAN_POINT ( 'NONE',  ( 5.000000000000000000, 8.660254037844385522, -96.62500000409677625 ) ) ;
#33905 = CARTESIAN_POINT ( 'NONE',  ( -2.121150477449813534E-15, -11.54700538379251284, -113.3749999999999858 ) ) ;
#33906 = CARTESIAN_POINT ( 'NONE',  ( -5.405949406250003975, -9.363379034771801557, -58.84375000204835970 ) ) ;
#33908 = EDGE_CURVE ( 'NONE', #10539, #24722, #28562, .T. ) ;
#33907 = EDGE_LOOP ( 'NONE', ( #13286, #5832, #31106, #20837 ) ) ;
#33909 = CARTESIAN_POINT ( 'NONE',  ( 5.000000000000000000, 8.660254037844385522, -34.74999999999997868 ) ) ;
#33910 = SECURITY_CLASSIFICATION ( '', '', #28245 ) ;
#33911 = CARTESIAN_POINT ( 'NONE',  ( 5.405949406249999534, 9.363379034771803333, -32.78125000204837391 ) ) ;
#33912 = CARTESIAN_POINT ( 'NONE',  ( 9.999999999999996447, -5.773502691896262640, -161.1250000000000284 ) ) ;
#33913 = CARTESIAN_POINT ( 'NONE',  ( 9.999999999999998224, 0.000000000000000000, -200.0000000000000000 ) ) ;
#33914 = CARTESIAN_POINT ( 'NONE',  ( 7.070501591499377789E-16, 11.54700538379251284, -29.00000000409674783 ) ) ;
#33915 = CARTESIAN_POINT ( 'NONE',  ( -5.405949406250003975, -9.363379034771801557, -135.5312500020484094 ) ) ;
#33916 = VERTEX_POINT ( 'NONE', #31828 ) ;
#33918 = ORIENTED_EDGE ( 'NONE', *, *, #9091, .T. ) ;
#33917 = VERTEX_POINT ( 'NONE', #28583 ) ;
#33919 = CYLINDRICAL_SURFACE ( 'NONE', #39711, 9.999999999999998224 ) ;
#33920 = AXIS2_PLACEMENT_3D ( 'NONE', #41160, #30839, #10751 ) ;
#33921 = DIRECTION ( 'NONE',  ( -0.000000000000000000, -0.000000000000000000, 1.000000000000000000 ) ) ;
#33922 = CARTESIAN_POINT ( 'NONE',  ( 7.644554776091147741E-16, 12.48450537969573659, -164.4687500020483810 ) ) ;
#33923 = CARTESIAN_POINT ( 'NONE',  ( -10.81189881249999907, -6.242252689847864744, -197.1562500020484379 ) ) ;
#33924 = CARTESIAN_POINT ( 'NONE',  ( -10.81189881249999729, 1.324075727343319199E-15, -15.59375000204835082 ) ) ;
#33925 = CYLINDRICAL_SURFACE ( 'NONE', #27423, 9.999999999999998224 ) ;
#33926 = CARTESIAN_POINT ( 'NONE',  ( 7.644554776091147741E-16, 12.48450537969573659, -149.4687500020484663 ) ) ;
#33927 = CARTESIAN_POINT ( 'NONE',  ( -10.81189881249999729, 1.324075727343319199E-15, -134.0937500020483810 ) ) ;
#33928 =( BOUNDED_CURVE ( )  B_SPLINE_CURVE ( 2, ( #36510, #1113, #17699, #30479, #37137, #17274, #23571 ),
 .UNSPECIFIED., .F., .F. ) 
 B_SPLINE_CURVE_WITH_KNOTS ( ( 3, 2, 2, 3 ),
 ( 0.2052238805970149627, 0.2064676616915423202, 0.2077114427860697055, 0.2089552238805970630 ),
 .UNSPECIFIED. ) 
 CURVE ( )  GEOMETRIC_REPRESENTATION_ITEM ( )  RATIONAL_B_SPLINE_CURVE ( ( 0.9999999999999970024, 0.8660254037844417052, 1.000000000000000000, 0.8660254037844387076, 1.000000000000000000, 0.8660254037844327124, 1.000000000000005995 ) ) 
 REPRESENTATION_ITEM ( '' )  );
#33929 = CARTESIAN_POINT ( 'NONE',  ( 5.405949406249992428, -9.363379034771808662, -106.7812500020483810 ) ) ;
#33930 = CARTESIAN_POINT ( 'NONE',  ( 10.81189881249999729, 0.000000000000000000, -116.8437500020483810 ) ) ;
#33931 = CARTESIAN_POINT ( 'NONE',  ( -2.293366432827344421E-15, -12.48450537969573659, -0.2187500020483512386 ) ) ;
#33932 = CARTESIAN_POINT ( 'NONE',  ( 10.81189881249999907, 6.242252689847868297, -124.4062500020483810 ) ) ;
#33933 = CARTESIAN_POINT ( 'NONE',  ( 10.81189881249999907, 6.242252689847868297, -7.218750002048349934 ) ) ;
#33934 = CARTESIAN_POINT ( 'NONE',  ( 5.405949406249992428, -9.363379034771808662, -133.5937500020483810 ) ) ;
#33935 = CARTESIAN_POINT ( 'NONE',  ( -2.275517850991317657E-15, -20.00000000000000000, -232.0000000000000000 ) ) ;
#33936 = CARTESIAN_POINT ( 'NONE',  ( -5.000000000000003553, -8.660254037844383745, -178.3750000040967905 ) ) ;
#33937 = CARTESIAN_POINT ( 'NONE',  ( -9.999999999999998224, 1.224646799147353059E-15, -152.7500000000000000 ) ) ;
#33938 = CARTESIAN_POINT ( 'NONE',  ( -4.999999999999996447, 8.660254037844387298, -17.99999999999996092 ) ) ;
#33939 = AXIS2_PLACEMENT_3D ( 'NONE', #3635, #33416, #19797 ) ;
#33940 = ADVANCED_FACE ( 'NONE', ( #18856 ), #5705, .T. ) ;
#33941 = CARTESIAN_POINT ( 'NONE',  ( 10.81189881249999729, 0.000000000000000000, -76.34375000204838102 ) ) ;
#33942 = CARTESIAN_POINT ( 'NONE',  ( -10.81189881249999907, -6.242252689847864744, -67.96875000204838102 ) ) ;
#33943 = CARTESIAN_POINT ( 'NONE',  ( -2.121150477449813534E-15, -11.54700538379251284, -19.25000000409677625 ) ) ;
#33944 = CARTESIAN_POINT ( 'NONE',  ( -10.81189881249999729, 6.242252689847871849, -35.40625000204836681 ) ) ;
#33945 = CARTESIAN_POINT ( 'NONE',  ( 10.81189881249999729, 0.000000000000000000, -49.34375000204838102 ) ) ;
#33946 = CARTESIAN_POINT ( 'NONE',  ( -9.999999999999998224, 1.224646799147353059E-15, -111.1250000040967763 ) ) ;
#33947 = CARTESIAN_POINT ( 'NONE',  ( 5.405949406249999534, 9.363379034771803333, -157.0937500020483810 ) ) ;
#33948 = CARTESIAN_POINT ( 'NONE',  ( -4.999999999999996447, 8.660254037844387298, -118.5000000000000000 ) ) ;
#33949 = CARTESIAN_POINT ( 'NONE',  ( -5.405949406249996869, 9.363379034771805109, -133.0312500020484094 ) ) ;
#33950 = CARTESIAN_POINT ( 'NONE',  ( -3.091979570676882449, 9.607409082080529572, -180.0000000000000000 ) ) ;
#33951 = CARTESIAN_POINT ( 'NONE',  ( -4.999999999999996447, 8.660254037844387298, -85.49999999999998579 ) ) ;
#33952 = CARTESIAN_POINT ( 'NONE',  ( -10.81189881249999729, 1.324075727343319199E-15, -15.78125000204835793 ) ) ;
#33953 = ORIENTED_EDGE ( 'NONE', *, *, #22229, .F. ) ;
#33954 = CARTESIAN_POINT ( 'NONE',  ( -10.81189881249999729, 1.324075727343319199E-15, -104.2812500020483810 ) ) ;
#33955 = CARTESIAN_POINT ( 'NONE',  ( -10.00000000000000000, -5.773502691896251982, -123.0000000040968047 ) ) ;
#33956 = CARTESIAN_POINT ( 'NONE',  ( 9.999999999998456346, 5.773502691897149042, -9.374999999999944933 ) ) ;
#33957 = CARTESIAN_POINT ( 'NONE',  ( -4.999999999999996447, 8.660254037844387298, -31.87500000409676559 ) ) ;
#33958 = CARTESIAN_POINT ( 'NONE',  ( 0.000000000000000000, 0.000000000000000000, -200.0000000000000000 ) ) ;
#33959 = CARTESIAN_POINT ( 'NONE',  ( -10.81189881249999729, 6.242252689847871849, -51.90625000204837391 ) ) ;
#33960 = AXIS2_PLACEMENT_3D ( 'NONE', #6815, #28861, #29069 ) ;
#33961 = CARTESIAN_POINT ( 'NONE',  ( -9.999999999999479527, -5.773502691896549521, -146.6249999999999716 ) ) ;
#33962 = CARTESIAN_POINT ( 'NONE',  ( -10.81189881249999729, 1.324075727343319199E-15, -149.2812500020483810 ) ) ;
#33963 = CARTESIAN_POINT ( 'NONE',  ( -10.81189881249999729, 6.242252689847871849, -132.7187500020483810 ) ) ;
#33964 = CARTESIAN_POINT ( 'NONE',  ( -4.999999999999996447, 8.660254037844387298, -165.3750000040967905 ) ) ;
#33965 = ORIENTED_EDGE ( 'NONE', *, *, #12507, .T. ) ;
#33966 = CARTESIAN_POINT ( 'NONE',  ( 9.999999999999998224, 0.000000000000000000, -85.99999999999998579 ) ) ;
#33967 = ORIENTED_EDGE ( 'NONE', *, *, #39942, .F. ) ;
#33968 = ORIENTED_EDGE ( 'NONE', *, *, #14322, .T. ) ;
#33970 = VERTEX_POINT ( 'NONE', #2264 ) ;
#33969 = CARTESIAN_POINT ( 'NONE',  ( 5.405949406249999534, 9.363379034771803333, -113.5937500020483810 ) ) ;
#33971 = CARTESIAN_POINT ( 'NONE',  ( -10.00000000000076916, 5.773502691895813221, -129.2500000040967905 ) ) ;
#33972 =( BOUNDED_CURVE ( )  B_SPLINE_CURVE ( 2, ( #15198, #40809, #21180, #13835, #27457, #1131, #37380 ),
 .UNSPECIFIED., .F., .F. ) 
 B_SPLINE_CURVE_WITH_KNOTS ( ( 3, 2, 2, 3 ),
 ( 0.1977611940298507898, 0.1990049751243781750, 0.2002487562189055326, 0.2014925373134328901 ),
 .UNSPECIFIED. ) 
 CURVE ( )  GEOMETRIC_REPRESENTATION_ITEM ( )  RATIONAL_B_SPLINE_CURVE ( ( 0.9999999999999940048, 0.8660254037844447028, 1.000000000000000000, 0.8660254037844387076, 1.000000000000000000, 0.8660254037844327124, 1.000000000000005995 ) ) 
 REPRESENTATION_ITEM ( '' )  );
#33973 = CARTESIAN_POINT ( 'NONE',  ( -5.405949406250003975, -9.363379034771801557, -189.3437500020483810 ) ) ;
#33974 = CARTESIAN_POINT ( 'NONE',  ( 10.81189881249999551, -6.242252689847874514, -41.96875000204835970 ) ) ;
#33975 = CARTESIAN_POINT ( 'NONE',  ( -6.904799017827355279, -7.420746795541425911, 9.002545116942468623E-15 ) ) ;
#33976 = CARTESIAN_POINT ( 'NONE',  ( -10.81189881249999729, 6.242252689847871849, -170.2187500020483810 ) ) ;
#33977 = CARTESIAN_POINT ( 'NONE',  ( 5.405949406249992428, -9.363379034771808662, -163.5937500020484094 ) ) ;
#33978 = CARTESIAN_POINT ( 'NONE',  ( 10.81189881249999729, 0.000000000000000000, -139.3437500020484094 ) ) ;
#33979 = CARTESIAN_POINT ( 'NONE',  ( -5.405949406249996869, 9.363379034771805109, -152.3437500020483810 ) ) ;
#33980 = CARTESIAN_POINT ( 'NONE',  ( -9.999999999999998224, 1.224646799147353059E-15, -43.24999999999998579 ) ) ;
#33981 =( BOUNDED_CURVE ( )  B_SPLINE_CURVE ( 2, ( #24785, #17842, #1470, #40289, #4057, #17199, #30400 ),
 .UNSPECIFIED., .F., .F. ) 
 B_SPLINE_CURVE_WITH_KNOTS ( ( 3, 2, 2, 3 ),
 ( 0.8880597014925376564, 0.8893034825870650417, 0.8905472636815924270, 0.8917910447761197013 ),
 .UNSPECIFIED. ) 
 CURVE ( )  GEOMETRIC_REPRESENTATION_ITEM ( )  RATIONAL_B_SPLINE_CURVE ( ( 0.9999999999999641398, 0.8660254037844745678, 1.000000000000000000, 0.8660254037844387076, 1.000000000000000000, 0.8660254037844028474, 1.000000000000035971 ) ) 
 REPRESENTATION_ITEM ( '' )  );
#33982 = FACE_OUTER_BOUND ( 'NONE', #12480, .T. ) ;
#33983 = CARTESIAN_POINT ( 'NONE',  ( 9.999999999999998224, 0.000000000000000000, -182.0000000000000000 ) ) ;
#33984 = CARTESIAN_POINT ( 'NONE',  ( 10.81189881249999907, 6.242252689847868297, -86.71875000204836681 ) ) ;
#33985 = CARTESIAN_POINT ( 'NONE',  ( -9.999999999999479527, -5.773502691896549521, -113.6249999999999716 ) ) ;
#33986 = CARTESIAN_POINT ( 'NONE',  ( 10.81189881249999729, 0.000000000000000000, -55.53125000204836681 ) ) ;
#33987 = CARTESIAN_POINT ( 'NONE',  ( 7.070501591499376803E-16, 11.54700538379251284, -87.50000000409677625 ) ) ;
#33988 = CARTESIAN_POINT ( 'NONE',  ( -10.81189881249999907, -6.242252689847864744, -177.4687500020484094 ) ) ;
#33989 = CARTESIAN_POINT ( 'NONE',  ( -2.293366432827344421E-15, -12.48450537969573659, -123.4062500020484094 ) ) ;
#33990 = CARTESIAN_POINT ( 'NONE',  ( -10.81189881249999729, 6.242252689847871849, -150.9062500020484094 ) ) ;
#33991 = CARTESIAN_POINT ( 'NONE',  ( -9.999999999999998224, 1.224646799147353059E-15, -115.2499999999999858 ) ) ;
#33992 = CARTESIAN_POINT ( 'NONE',  ( -5.405949406249996869, 9.363379034771805109, -53.53125000204836681 ) ) ;
#33993 = CARTESIAN_POINT ( 'NONE',  ( -2.121150477449813534E-15, -11.54700538379251284, -133.2500000040967905 ) ) ;
#33994 = CARTESIAN_POINT ( 'NONE',  ( 9.999999999999998224, 0.000000000000000000, -103.9999999999999858 ) ) ;
#33995 = ORIENTED_EDGE ( 'NONE', *, *, #34944, .F. ) ;
#33996 = CARTESIAN_POINT ( 'NONE',  ( 10.81189881249999729, 0.000000000000000000, -132.0312500020484094 ) ) ;
#33997 = CARTESIAN_POINT ( 'NONE',  ( -4.999999999999996447, 8.660254037844387298, -147.3750000040967905 ) ) ;
#33998 = CARTESIAN_POINT ( 'NONE',  ( -5.405949406249996869, 9.363379034771805109, -151.0312500020483810 ) ) ;
#33999 = CARTESIAN_POINT ( 'NONE',  ( 5.405949406249999534, 9.363379034771803333, -190.2812500020484094 ) ) ;
#34000 = ORIENTED_EDGE ( 'NONE', *, *, #30774, .F. ) ;
#34001 = CARTESIAN_POINT ( 'NONE',  ( 4.999999999999992006, -8.660254037844389075, -51.74999999999996447 ) ) ;
#34002 = CARTESIAN_POINT ( 'NONE',  ( -10.81189881249999729, 6.242252689847871849, -182.2187500020484379 ) ) ;
#34003 = CARTESIAN_POINT ( 'NONE',  ( -9.999999999999998224, 1.224646799147353059E-15, -57.12500000409676204 ) ) ;
#34004 = CARTESIAN_POINT ( 'NONE',  ( 9.999999999999998224, 0.000000000000000000, -153.5000000000000000 ) ) ;
#34005 = CARTESIAN_POINT ( 'NONE',  ( 10.00000000000012257, -5.773502691896187144, -165.6250000000000000 ) ) ;
#34006 = CARTESIAN_POINT ( 'NONE',  ( 7.644554776091147741E-16, 12.48450537969573659, -77.65625000204838102 ) ) ;
#34007 = CARTESIAN_POINT ( 'NONE',  ( -5.405949406250003975, -9.363379034771801557, -48.53125000204838813 ) ) ;
#34008 = ADVANCED_FACE ( 'NONE', ( #1610 ), #2040, .T. ) ;
#34009 = CARTESIAN_POINT ( 'NONE',  ( -4.999999999999996447, 8.660254037844387298, -49.87500000409675494 ) ) ;
#34010 = CARTESIAN_POINT ( 'NONE',  ( -2.293366432827344421E-15, -12.48450537969573659, -10.71875000204836148 ) ) ;
#34011 = CARTESIAN_POINT ( 'NONE',  ( -9.999999999999998224, 1.224646799147353059E-15, -200.0000000000000000 ) ) ;
#34012 = CARTESIAN_POINT ( 'NONE',  ( -10.81189881249999907, -6.242252689847864744, -176.1562500020483810 ) ) ;
#34013 = CARTESIAN_POINT ( 'NONE',  ( 10.81189881249999551, -6.242252689847874514, -6.156250002048363257 ) ) ;
#34014 = DIRECTION ( 'NONE',  ( -0.000000000000000000, -0.000000000000000000, 1.000000000000000000 ) ) ;
#34015 = CARTESIAN_POINT ( 'NONE',  ( 9.999999999999998224, 0.000000000000000000, -117.5000000000000000 ) ) ;
#34016 = DIRECTION ( 'NONE',  ( 0.000000000000000000, -0.08715574274765837404, -0.9961946980917455452 ) ) ;
#34017 = CARTESIAN_POINT ( 'NONE',  ( -9.999999999999872102, -5.773502691896326589, -163.5000000040967620 ) ) ;
#34019 = ORIENTED_EDGE ( 'NONE', *, *, #3134, .F. ) ;
#34018 = CARTESIAN_POINT ( 'NONE',  ( -5.405949406249996869, 9.363379034771805109, -88.03125000204838102 ) ) ;
#34021 = VERTEX_POINT ( 'NONE', #18201 ) ;
#34020 = CARTESIAN_POINT ( 'NONE',  ( -10.00000000000051337, 5.773502691895962435, -80.87499999999995737 ) ) ;
#34022 = ORIENTED_EDGE ( 'NONE', *, *, #12040, .T. ) ;
#34023 = EDGE_CURVE ( 'NONE', #19597, #1644, #26896, .T. ) ;
#34024 = CARTESIAN_POINT ( 'NONE',  ( 10.81189881249999729, 0.000000000000000000, -38.84375000204837391 ) ) ;
#34025 = CARTESIAN_POINT ( 'NONE',  ( 5.405949406249999534, 9.363379034771803333, -26.59375000204835970 ) ) ;
#34026 = CARTESIAN_POINT ( 'NONE',  ( -10.81189881249999729, 6.242252689847871849, -15.90625000204837391 ) ) ;
#34027 = CARTESIAN_POINT ( 'NONE',  ( 10.81189881249999729, 0.000000000000000000, -65.84375000204836681 ) ) ;
#34028 = CYLINDRICAL_SURFACE ( 'NONE', #38751, 9.999999999999998224 ) ;
#34029 = EDGE_CURVE ( 'NONE', #18647, #2497, #23339, .T. ) ;
#34030 = CARTESIAN_POINT ( 'NONE',  ( -9.999999999999998224, 1.224646799147353059E-15, -44.74999999999998579 ) ) ;
#34031 = CARTESIAN_POINT ( 'NONE',  ( -2.293366432827344421E-15, -12.48450537969573659, -181.7187500020484094 ) ) ;
#34032 = CARTESIAN_POINT ( 'NONE',  ( 10.81189881249999729, 0.000000000000000000, -163.3437500020484094 ) ) ;
#34033 = CARTESIAN_POINT ( 'NONE',  ( -10.81189881249999729, -6.242252689847864744, -174.4687500020483526 ) ) ;
#34034 = CARTESIAN_POINT ( 'NONE',  ( 9.999999999999998224, 0.000000000000000000, -179.3750000040967905 ) ) ;
#34035 = CARTESIAN_POINT ( 'NONE',  ( 9.999999999999998224, 0.000000000000000000, -141.5000000000000000 ) ) ;
#34036 = CARTESIAN_POINT ( 'NONE',  ( 5.000000000000000000, 8.660254037844385522, -126.2499999999999716 ) ) ;
#34037 = DIRECTION ( 'NONE',  ( -0.000000000000000000, -0.000000000000000000, 1.000000000000000000 ) ) ;
#34038 = CARTESIAN_POINT ( 'NONE',  ( -2.293366432827344421E-15, -12.48450537969573659, -112.7187500020483952 ) ) ;
#34039 = DIRECTION ( 'NONE',  ( -0.000000000000000000, -0.000000000000000000, -1.000000000000000000 ) ) ;
#34040 = CARTESIAN_POINT ( 'NONE',  ( -5.405949406250003975, -9.363379034771801557, -89.03125000204838102 ) ) ;
#34041 = CARTESIAN_POINT ( 'NONE',  ( 5.405949406249999534, 9.363379034771803333, -103.0937500020483810 ) ) ;
#34042 = CARTESIAN_POINT ( 'NONE',  ( 10.81189881249999551, -6.242252689847874514, -73.46875000204835260 ) ) ;
#34043 = CARTESIAN_POINT ( 'NONE',  ( 5.405949406249999534, 9.363379034771803333, -77.78125000204838102 ) ) ;
#34044 = CARTESIAN_POINT ( 'NONE',  ( -2.121150477449813534E-15, -11.54700538379251284, -154.2500000040967620 ) ) ;
#34045 = CARTESIAN_POINT ( 'NONE',  ( 4.999999999999992006, -8.660254037844389075, -128.2499999999999716 ) ) ;
#34046 = CARTESIAN_POINT ( 'NONE',  ( -5.405949406250003975, -9.363379034771801557, -161.0312500020484094 ) ) ;
#34047 = CARTESIAN_POINT ( 'NONE',  ( -10.81189881249999907, -6.242252689847864744, -176.1562500020483810 ) ) ;
#34048 = CARTESIAN_POINT ( 'NONE',  ( -10.00000000000038547, 5.773502691896036154, -153.2500000040967905 ) ) ;
#34049 = CARTESIAN_POINT ( 'NONE',  ( -9.999999999999998224, 1.224646799147353059E-15, -20.74999999999996447 ) ) ;
#34050 = CARTESIAN_POINT ( 'NONE',  ( -5.405949406249996869, 9.363379034771805109, -107.3437500020483810 ) ) ;
#34051 = CARTESIAN_POINT ( 'NONE',  ( 9.999999999999998224, 0.000000000000000000, -63.49999999999997158 ) ) ;
#34052 = CARTESIAN_POINT ( 'NONE',  ( -2.121150477449813534E-15, -11.54700538379251284, -74.37499999999995737 ) ) ;
#34053 = CARTESIAN_POINT ( 'NONE',  ( 5.405949406249999534, 9.363379034771803333, -1.281250002048373027 ) ) ;
#34054 = CARTESIAN_POINT ( 'NONE',  ( -2.121150477449813534E-15, -11.54700538379251284, -83.75000000409677625 ) ) ;
#34055 =( BOUNDED_CURVE ( )  B_SPLINE_CURVE ( 2, ( #24505, #41078, #21033, #11523, #40654, #2058, #21248 ),
 .UNSPECIFIED., .F., .F. ) 
 B_SPLINE_CURVE_WITH_KNOTS ( ( 3, 2, 2, 3 ),
 ( 0.8992537313432839019, 0.9004975124378112872, 0.9017412935323385614, 0.9029850746268659467 ),
 .UNSPECIFIED. ) 
 CURVE ( )  GEOMETRIC_REPRESENTATION_ITEM ( )  RATIONAL_B_SPLINE_CURVE ( ( 0.9999999999999641398, 0.8660254037844745678, 1.000000000000000000, 0.8660254037844387076, 1.000000000000000000, 0.8660254037844148378, 1.000000000000023981 ) ) 
 REPRESENTATION_ITEM ( '' )  );
#34056 = CARTESIAN_POINT ( 'NONE',  ( 9.999999999999998224, 0.000000000000000000, -115.9999999999999858 ) ) ;
#34057 = CARTESIAN_POINT ( 'NONE',  ( -5.405949406250003975, -9.363379034771801557, -98.03125000204839523 ) ) ;
#34058 = CARTESIAN_POINT ( 'NONE',  ( -2.293366432827344421E-15, -12.48450537969573659, -87.40625000204838102 ) ) ;
#34059 = CARTESIAN_POINT ( 'NONE',  ( -10.00000000000000000, -5.773502691896251982, -75.00000000409677625 ) ) ;
#34060 = CARTESIAN_POINT ( 'NONE',  ( 4.999999999999992006, -8.660254037844389075, -59.24999999999997158 ) ) ;
#34061 = CARTESIAN_POINT ( 'NONE',  ( -5.405949406250003975, -9.363379034771801557, -31.84375000204836681 ) ) ;
#34062 = ORIENTED_EDGE ( 'NONE', *, *, #26583, .F. ) ;
#34063 = CARTESIAN_POINT ( 'NONE',  ( 10.00000000000000000, 5.773502691896255534, -1.874999999999944711 ) ) ;
#34064 = CARTESIAN_POINT ( 'NONE',  ( -10.81189881249999729, 6.242252689847871849, -27.90625000204838102 ) ) ;
#34065 = EDGE_CURVE ( 'NONE', #41802, #28405, #20586, .T. ) ;
#34066 = CARTESIAN_POINT ( 'NONE',  ( 10.81189881249999729, 6.242252689847867408, -11.71875000204837214 ) ) ;
#34067 = CARTESIAN_POINT ( 'NONE',  ( 10.00000000000051159, -5.773502691895965988, -118.0000000040967763 ) ) ;
#34068 = CARTESIAN_POINT ( 'NONE',  ( 7.070501591499377789E-16, 11.54700538379251284, -3.500000004096753603 ) ) ;
#34069 = CARTESIAN_POINT ( 'NONE',  ( -10.81189881249999907, -6.242252689847864744, -128.1562500020483810 ) ) ;
#34070 = CARTESIAN_POINT ( 'NONE',  ( 9.999999999999998224, 0.000000000000000000, -182.0000000000000000 ) ) ;
#34072 = ORIENTED_EDGE ( 'NONE', *, *, #21972, .T. ) ;
#34071 = CARTESIAN_POINT ( 'NONE',  ( 7.644554776091147741E-16, 12.48450537969573659, -109.1562500020483810 ) ) ;
#34073 = CARTESIAN_POINT ( 'NONE',  ( 9.999999999999884537, 5.773502691896319483, -195.3750000000000000 ) ) ;
#34074 = ORIENTED_EDGE ( 'NONE', *, *, #38167, .T. ) ;
#34075 = ORIENTED_EDGE ( 'NONE', *, *, #1421, .T. ) ;
#34076 = CARTESIAN_POINT ( 'NONE',  ( 7.644554776091147741E-16, 12.48450537969573659, -41.65625000204837391 ) ) ;
#34077 = APPROVAL_STATUS ( 'not_yet_approved' ) ;
#34078 = CARTESIAN_POINT ( 'NONE',  ( -2.293366432827344421E-15, -12.48450537969573659, -88.71875000204838102 ) ) ;
#34079 = DIRECTION ( 'NONE',  ( -0.000000000000000000, -0.000000000000000000, 1.000000000000000000 ) ) ;
#34080 = CYLINDRICAL_SURFACE ( 'NONE', #32167, 9.999999999999998224 ) ;
#34081 = CARTESIAN_POINT ( 'NONE',  ( -9.999999999999998224, 1.224646799147353059E-15, -156.1250000040967905 ) ) ;
#34082 = CARTESIAN_POINT ( 'NONE',  ( 7.644554776091147741E-16, 12.48450537969573659, -173.6562500020483810 ) ) ;
#34083 = CARTESIAN_POINT ( 'NONE',  ( -9.999999999999998224, 1.224646799147353059E-15, -139.2499999999999716 ) ) ;
#34084 = CARTESIAN_POINT ( 'NONE',  ( 5.405949406249992428, -9.363379034771808662, -127.5937500020483668 ) ) ;
#34085 = CARTESIAN_POINT ( 'NONE',  ( -5.405949406250003975, -9.363379034771801557, -94.84375000204838102 ) ) ;
#34086 = CARTESIAN_POINT ( 'NONE',  ( -2.293366432827344421E-15, -12.48450537969573659, -1.906250002048373027 ) ) ;
#34087 = CARTESIAN_POINT ( 'NONE',  ( 10.81189881249999729, 0.000000000000000000, -100.5312500020483952 ) ) ;
#34088 = CARTESIAN_POINT ( 'NONE',  ( 4.999999999999992006, -8.660254037844389075, -179.6250000040968189 ) ) ;
#34089 = CARTESIAN_POINT ( 'NONE',  ( -10.81189881249999729, -6.242252689847864744, -105.4687500020483668 ) ) ;
#34090 = CARTESIAN_POINT ( 'NONE',  ( 5.405949406249999534, 9.363379034771803333, -178.2812500020484094 ) ) ;
#34091 =( BOUNDED_CURVE ( )  B_SPLINE_CURVE ( 2, ( #14152, #36213, #33624, #17190, #33206, #39864, #10720 ),
 .UNSPECIFIED., .F., .F. ) 
 B_SPLINE_CURVE_WITH_KNOTS ( ( 3, 2, 2, 3 ),
 ( 0.4477611940298508730, 0.4490049751243782028, 0.4502487562189055881, 0.4514925373134329734 ),
 .UNSPECIFIED. ) 
 CURVE ( )  GEOMETRIC_REPRESENTATION_ITEM ( )  RATIONAL_B_SPLINE_CURVE ( ( 0.9999999999999880096, 0.8660254037844506980, 1.000000000000000000, 0.8660254037844387076, 1.000000000000000000, 0.8660254037844267172, 1.000000000000011990 ) ) 
 REPRESENTATION_ITEM ( '' )  );
#34092 = CARTESIAN_POINT ( 'NONE',  ( -9.999999999999998224, 1.224646799147353059E-15, -107.7499999999999858 ) ) ;
#34093 = CARTESIAN_POINT ( 'NONE',  ( -2.121150477449813534E-15, -11.54700538379251284, -152.7500000040967620 ) ) ;
#34094 = CARTESIAN_POINT ( 'NONE',  ( -2.293366432827344421E-15, -12.48450537969573659, -195.4062500020484094 ) ) ;
#34095 = CARTESIAN_POINT ( 'NONE',  ( 7.644554776091147741E-16, 12.48450537969573659, -48.96875000204835260 ) ) ;
#34096 = CARTESIAN_POINT ( 'NONE',  ( 5.405949406249999534, 9.363379034771803333, -43.09375000204837391 ) ) ;
#34097 = CARTESIAN_POINT ( 'NONE',  ( 4.999999999999992006, -8.660254037844389075, -172.1250000040968189 ) ) ;
#34098 = CARTESIAN_POINT ( 'NONE',  ( -10.81189881249999907, -6.242252689847864744, -6.656250002048364145 ) ) ;
#34099 = CARTESIAN_POINT ( 'NONE',  ( -5.405949406249996869, 9.363379034771805109, -24.84375000204835970 ) ) ;
#34100 = CARTESIAN_POINT ( 'NONE',  ( -2.293366432827344421E-15, -12.48450537969573659, -127.7187500020483668 ) ) ;
#34101 = CARTESIAN_POINT ( 'NONE',  ( -9.999999999999998224, 1.224646799147353059E-15, -97.24999999999998579 ) ) ;
#34102 = CARTESIAN_POINT ( 'NONE',  ( 10.81189881249999729, 0.000000000000000000, -25.53125000204836681 ) ) ;
#34103 = CARTESIAN_POINT ( 'NONE',  ( -9.999999999999998224, 5.773502691896259087, -112.7500000040967763 ) ) ;
#34104 = ADVANCED_BREP_SHAPE_REPRESENTATION ( '', ( #30024, #39998 ), #15874 ) ;
#34105 = DIRECTION ( 'NONE',  ( -0.000000000000000000, -0.000000000000000000, 1.000000000000000000 ) ) ;
#34106 = CARTESIAN_POINT ( 'NONE',  ( 9.999999999999998224, 0.000000000000000000, -58.99999999999997158 ) ) ;
#34107 = CARTESIAN_POINT ( 'NONE',  ( 10.81189881249999907, 6.242252689847868297, -122.9062500020484094 ) ) ;
#34108 = CARTESIAN_POINT ( 'NONE',  ( 10.81189881249999729, 6.242252689847867408, -107.9062500020483952 ) ) ;
#34109 = ORIENTED_EDGE ( 'NONE', *, *, #16142, .F. ) ;
#34110 = CARTESIAN_POINT ( 'NONE',  ( -10.00000000000154188, 5.773502691895366468, -7.750000004096709638 ) ) ;
#34111 = CARTESIAN_POINT ( 'NONE',  ( 4.999999999999992006, -8.660254037844389075, -103.1250000040967763 ) ) ;
#34112 = CARTESIAN_POINT ( 'NONE',  ( 9.999999999999998224, 0.000000000000000000, -150.8750000040967905 ) ) ;
#34113 = CARTESIAN_POINT ( 'NONE',  ( 10.81189881249999907, 6.242252689847868297, -163.4062500020484094 ) ) ;
#34114 = CARTESIAN_POINT ( 'NONE',  ( 10.81189881249999551, -6.242252689847874514, -61.46875000204837391 ) ) ;
#34115 = ORIENTED_EDGE ( 'NONE', *, *, #39913, .T. ) ;
#34116 = CARTESIAN_POINT ( 'NONE',  ( -10.00000000000000000, -5.773502691896251982, -25.12499999999997513 ) ) ;
#34117 = EDGE_CURVE ( 'NONE', #7028, #3605, #19708, .T. ) ;
#34118 = CARTESIAN_POINT ( 'NONE',  ( 7.644554776091147741E-16, 12.48450537969573659, -38.65625000204835260 ) ) ;
#34119 = CARTESIAN_POINT ( 'NONE',  ( -10.00000000000000000, -5.773502691896251982, -163.1250000000000284 ) ) ;
#34120 = EDGE_CURVE ( 'NONE', #30972, #20460, #2672, .T. ) ;
#34121 = DIRECTION ( 'NONE',  ( -0.000000000000000000, -0.000000000000000000, 1.000000000000000000 ) ) ;
#34122 = CARTESIAN_POINT ( 'NONE',  ( 5.000000000000000000, 8.660254037844385522, -32.12500000409676204 ) ) ;
#34123 = EDGE_CURVE ( 'NONE', #23080, #35880, #32459, .T. ) ;
#34124 = EDGE_CURVE ( 'NONE', #26629, #32856, #39330, .T. ) ;
#34125 = CYLINDRICAL_SURFACE ( 'NONE', #15311, 9.999999999999998224 ) ;
#34126 = CARTESIAN_POINT ( 'NONE',  ( 7.644554776091147741E-16, 12.48450537969573659, -137.6562500020483810 ) ) ;
#34127 = CARTESIAN_POINT ( 'NONE',  ( 9.169761814809081812, 5.423027170935617036, 5.369687683974985216E-15 ) ) ;
#34128 = CARTESIAN_POINT ( 'NONE',  ( -9.999999999999998224, 1.224646799147353059E-15, -174.1250000040968189 ) ) ;
#34129 = EDGE_LOOP ( 'NONE', ( #38259, #39476, #6145, #24040 ) ) ;
#34131 = ORIENTED_EDGE ( 'NONE', *, *, #20105, .F. ) ;
#34130 = ORIENTED_EDGE ( 'NONE', *, *, #27009, .T. ) ;
#34132 = EDGE_CURVE ( 'NONE', #28672, #2082, #204, .T. ) ;
#34133 = FACE_OUTER_BOUND ( 'NONE', #24208, .T. ) ;
#34134 = DIRECTION ( 'NONE',  ( 1.000000000000000000, 0.000000000000000000, 0.000000000000000000 ) ) ;
#34135 = CARTESIAN_POINT ( 'NONE',  ( -10.81189881249999907, -6.242252689847864744, -162.4687500020483526 ) ) ;
#34136 = VECTOR ( 'NONE', #19594, 1000.000000000000000 ) ;
#34137 = ADVANCED_FACE ( 'NONE', ( #12573 ), #9559, .F. ) ;
#34138 = CARTESIAN_POINT ( 'NONE',  ( 7.644554776091147741E-16, 12.48450537969573659, -197.6562500020484379 ) ) ;
#34139 = CARTESIAN_POINT ( 'NONE',  ( 7.644554776091147741E-16, 12.48450537969573659, -15.96875000204835615 ) ) ;
#34140 = CYLINDRICAL_SURFACE ( 'NONE', #24688, 9.999999999999998224 ) ;
#34141 = EDGE_CURVE ( 'NONE', #42482, #38638, #29852, .T. ) ;
#34142 = CARTESIAN_POINT ( 'NONE',  ( -2.293366432827344421E-15, -12.48450537969573659, -145.7187500020484094 ) ) ;
#34143 = CARTESIAN_POINT ( 'NONE',  ( 10.81189881249999907, 6.242252689847868297, -136.2187500020483810 ) ) ;
#34144 = CARTESIAN_POINT ( 'NONE',  ( -10.81189881249999729, 6.242252689847871849, -102.9062500020483810 ) ) ;
#34145 = CARTESIAN_POINT ( 'NONE',  ( -5.405949406250003975, -9.363379034771801557, -115.8437500020483810 ) ) ;
#34146 = CARTESIAN_POINT ( 'NONE',  ( -4.999999999999996447, 8.660254037844387298, -195.3750000040967905 ) ) ;
#34147 = CARTESIAN_POINT ( 'NONE',  ( -5.405949406250003975, -9.363379034771801557, -126.5312500020483952 ) ) ;
#34148 = CARTESIAN_POINT ( 'NONE',  ( 5.405949406249999534, 9.363379034771803333, -5.593750002048370362 ) ) ;
#34149 = CARTESIAN_POINT ( 'NONE',  ( 10.81189881249999551, -6.242252689847874514, -131.9687500020483810 ) ) ;
#34150 = CARTESIAN_POINT ( 'NONE',  ( -10.00000000000012434, 5.773502691896184480, -163.3750000000000000 ) ) ;
#34151 = CARTESIAN_POINT ( 'NONE',  ( 9.999999999999998224, 0.000000000000000000, -5.375000004096769146 ) ) ;
#34152 = CARTESIAN_POINT ( 'NONE',  ( -10.00000000000000000, -5.773502691896251982, -154.1250000000000284 ) ) ;
#34153 = CARTESIAN_POINT ( 'NONE',  ( 10.00000000000000000, 5.773502691896255534, -16.87499999999997513 ) ) ;
#34154 = CARTESIAN_POINT ( 'NONE',  ( 7.644554776091147741E-16, 12.48450537969573659, -77.46875000204838102 ) ) ;
#34155 = CARTESIAN_POINT ( 'NONE',  ( 10.81189881249999907, 6.242252689847868297, -68.71875000204838102 ) ) ;
#34156 = DIRECTION ( 'NONE',  ( -0.000000000000000000, -0.000000000000000000, -1.000000000000000000 ) ) ;
#34157 = CARTESIAN_POINT ( 'NONE',  ( 7.644554776091147741E-16, 12.48450537969573659, -32.65625000204835970 ) ) ;
#34158 = CARTESIAN_POINT ( 'NONE',  ( 5.405949406249992428, -9.363379034771808662, -49.59375000204838102 ) ) ;
#34159 = CARTESIAN_POINT ( 'NONE',  ( 5.405949406249992428, -9.363379034771808662, -156.0937500020483810 ) ) ;
#34160 = CARTESIAN_POINT ( 'NONE',  ( 7.070501591499377789E-16, 11.54700538379251284, -121.6249999999999858 ) ) ;
#34161 = CARTESIAN_POINT ( 'NONE',  ( -2.293366432827344421E-15, -12.48450537969573659, -127.9062500020483952 ) ) ;
#34162 = EDGE_CURVE ( 'NONE', #6210, #7311, #3456, .T. ) ;
#34163 = DIRECTION ( 'NONE',  ( 1.000000000000000000, 0.000000000000000000, 0.000000000000000000 ) ) ;
#34164 = AXIS2_PLACEMENT_3D ( 'NONE', #36566, #19948, #23844 ) ;
#34165 = CARTESIAN_POINT ( 'NONE',  ( 9.999999999999998224, 0.000000000000000000, -82.99999999999997158 ) ) ;
#34166 = CARTESIAN_POINT ( 'NONE',  ( -10.81189881249999729, 6.242252689847871849, -14.40625000204836681 ) ) ;
#34167 = ORIENTED_EDGE ( 'NONE', *, *, #7149, .F. ) ;
#34168 = CARTESIAN_POINT ( 'NONE',  ( 5.405949406249999534, 9.363379034771803333, -104.7812500020483810 ) ) ;
#34169 = CARTESIAN_POINT ( 'NONE',  ( 9.999999999999996447, -5.773502691896262640, -127.0000000040967763 ) ) ;
#34170 = CARTESIAN_POINT ( 'NONE',  ( -9.999999999999998224, 1.224646799147353059E-15, -52.62500000409675494 ) ) ;
#34171 = CARTESIAN_POINT ( 'NONE',  ( -9.999999999999998224, 1.224646799147353059E-15, -31.62500000409676559 ) ) ;
#34172 = AXIS2_PLACEMENT_3D ( 'NONE', #42372, #40200, #40831 ) ;
#34173 = DIRECTION ( 'NONE',  ( -0.000000000000000000, -0.000000000000000000, 1.000000000000000000 ) ) ;
#34174 = CARTESIAN_POINT ( 'NONE',  ( 5.405949406249992428, -9.363379034771808662, -48.28125000204838813 ) ) ;
#34175 = EDGE_CURVE ( 'NONE', #18020, #17561, #12023, .T. ) ;
#34176 = CARTESIAN_POINT ( 'NONE',  ( 9.999999999999998224, 0.000000000000000000, -39.87500000409676915 ) ) ;
#34177 = CARTESIAN_POINT ( 'NONE',  ( -10.81189881249999729, 1.324075727343319199E-15, -155.2812500020484094 ) ) ;
#34178 = CARTESIAN_POINT ( 'NONE',  ( -10.81189881249999729, 1.324075727343319199E-15, -126.5937500020483668 ) ) ;
#34179 = CARTESIAN_POINT ( 'NONE',  ( 9.999999999999998224, 0.000000000000000000, -131.3750000040967905 ) ) ;
#34180 = EDGE_LOOP ( 'NONE', ( #16525, #28981, #8224, #19458 ) ) ;
#34181 = CARTESIAN_POINT ( 'NONE',  ( -10.00000000000102496, 5.773502691895664007, -31.37499999999992539 ) ) ;
#34182 = ORIENTED_EDGE ( 'NONE', *, *, #36445, .F. ) ;
#34183 = ORIENTED_EDGE ( 'NONE', *, *, #17359, .F. ) ;
#34185 = VERTEX_POINT ( 'NONE', #19691 ) ;
#34184 = CARTESIAN_POINT ( 'NONE',  ( -5.405949406250003975, -9.363379034771801557, -111.3437500020483810 ) ) ;
#34186 =( BOUNDED_CURVE ( )  B_SPLINE_CURVE ( 2, ( #22595, #42218, #41590, #18715, #12022, #31908, #5778 ),
 .UNSPECIFIED., .F., .F. ) 
 B_SPLINE_CURVE_WITH_KNOTS ( ( 3, 2, 2, 3 ),
 ( 0.1305970149253731227, 0.1318407960199005080, 0.1330845771144278378, 0.1343283582089551953 ),
 .UNSPECIFIED. ) 
 CURVE ( )  GEOMETRIC_REPRESENTATION_ITEM ( )  RATIONAL_B_SPLINE_CURVE ( ( 1.000000000000000000, 0.8660254037844387076, 1.000000000000000000, 0.8660254037844387076, 1.000000000000000000, 0.8660254037844417052, 0.9999999999999970024 ) ) 
 REPRESENTATION_ITEM ( '' )  );
#34187 = VECTOR ( 'NONE', #12141, 1000.000000000000000 ) ;
#34188 = EDGE_CURVE ( 'NONE', #12174, #33849, #16222, .T. ) ;
#34189 = CARTESIAN_POINT ( 'NONE',  ( -5.000000000000003553, -8.660254037844383745, -145.3750000040967905 ) ) ;
#34190 = CARTESIAN_POINT ( 'NONE',  ( 5.405949406249992428, -9.363379034771808662, -186.0937500020483810 ) ) ;
#34191 = CARTESIAN_POINT ( 'NONE',  ( 10.81189881249999551, -6.242252689847874514, -38.96875000204835970 ) ) ;
#34192 = CARTESIAN_POINT ( 'NONE',  ( 5.325955911939489695, -9.231538742169870915, -4.316514933816155950E-15 ) ) ;
#34193 = DIRECTION ( 'NONE',  ( -0.000000000000000000, -0.000000000000000000, 1.000000000000000000 ) ) ;
#34194 = CARTESIAN_POINT ( 'NONE',  ( -10.81189881249999729, 1.324075727343319199E-15, -174.5937500020484094 ) ) ;
#34195 = CARTESIAN_POINT ( 'NONE',  ( -5.405949406249996869, 9.363379034771805109, -164.3437500020484094 ) ) ;
#34196 = CARTESIAN_POINT ( 'NONE',  ( 10.00000000000154010, -5.773502691895370020, -25.00000000409672651 ) ) ;
#34197 = CARTESIAN_POINT ( 'NONE',  ( 10.81189881249999907, 6.242252689847868297, -142.2187500020484094 ) ) ;
#34198 = CARTESIAN_POINT ( 'NONE',  ( -10.81189881249999729, 6.242252689847871849, -150.9062500020484094 ) ) ;
#34199 = CARTESIAN_POINT ( 'NONE',  ( 10.81189881249999729, 0.000000000000000000, -151.3437500020483810 ) ) ;
#34200 = FACE_OUTER_BOUND ( 'NONE', #5355, .T. ) ;
#34201 = CARTESIAN_POINT ( 'NONE',  ( -9.999999999999998224, 1.224646799147353059E-15, -88.24999999999998579 ) ) ;
#34202 = CARTESIAN_POINT ( 'NONE',  ( -10.00000000000000000, -5.773502691896251982, -182.6250000000000284 ) ) ;
#34203 = CARTESIAN_POINT ( 'NONE',  ( 10.81189881249999551, -6.242252689847874514, -88.46875000204836681 ) ) ;
#34204 = CYLINDRICAL_SURFACE ( 'NONE', #30708, 9.999999999999998224 ) ;
#34205 = CARTESIAN_POINT ( 'NONE',  ( -10.81189881249999729, 6.242252689847871849, -62.40625000204838813 ) ) ;
#34206 = CYLINDRICAL_SURFACE ( 'NONE', #35097, 9.999999999999998224 ) ;
#34207 = CARTESIAN_POINT ( 'NONE',  ( -10.81189881249999729, 1.324075727343319199E-15, -179.0937500020484094 ) ) ;
#34208 = CARTESIAN_POINT ( 'NONE',  ( -10.81189881249999907, -6.242252689847864744, -114.6562500020483952 ) ) ;
#34209 = CARTESIAN_POINT ( 'NONE',  ( -2.293366432827344421E-15, -12.48450537969573659, -151.9062500020483810 ) ) ;
#34210 = CARTESIAN_POINT ( 'NONE',  ( 7.070501591499376803E-16, 11.54700538379251284, -115.6249999999999858 ) ) ;
#34211 = CARTESIAN_POINT ( 'NONE',  ( -2.293366432827344421E-15, -12.48450537969573659, -42.40625000204836681 ) ) ;
#34212 = CARTESIAN_POINT ( 'NONE',  ( 10.00000000000000000, 5.773502691896255534, -126.7500000040967905 ) ) ;
#34213 = CARTESIAN_POINT ( 'NONE',  ( 7.070501591499377789E-16, 11.54700538379251284, -109.6249999999999858 ) ) ;
#34214 = ORIENTED_EDGE ( 'NONE', *, *, #20946, .T. ) ;
#34215 = CARTESIAN_POINT ( 'NONE',  ( 10.81189881249999729, 6.242252689847867408, -130.4062500020483810 ) ) ;
#34216 = CARTESIAN_POINT ( 'NONE',  ( 9.999999999999998224, 0.000000000000000000, -144.8750000040967905 ) ) ;
#34217 = CARTESIAN_POINT ( 'NONE',  ( -9.183694056713489507E-15, -20.00000000000000355, 12.49999999999999112 ) ) ;
#34218 = CARTESIAN_POINT ( 'NONE',  ( 7.644554776091147741E-16, 12.48450537969573659, -178.1562500020484094 ) ) ;
#34219 = ORIENTED_EDGE ( 'NONE', *, *, #23075, .F. ) ;
#34220 = CARTESIAN_POINT ( 'NONE',  ( 9.999999999999996447, -5.773502691896262640, -53.12499999999997868 ) ) ;
#34221 = CARTESIAN_POINT ( 'NONE',  ( -10.81189881249999907, -6.242252689847864744, -169.9687500020484094 ) ) ;
#34222 = CARTESIAN_POINT ( 'NONE',  ( 9.999999999999998224, 0.000000000000000000, -57.87500000409676204 ) ) ;
#34223 = DIRECTION ( 'NONE',  ( -0.000000000000000000, -0.000000000000000000, 1.000000000000000000 ) ) ;
#34224 = CARTESIAN_POINT ( 'NONE',  ( -9.999999999999998224, 1.224646799147353059E-15, -200.0000000000000000 ) ) ;
#34225 = CARTESIAN_POINT ( 'NONE',  ( 10.81189881249999551, -6.242252689847874514, -78.15625000204838102 ) ) ;
#34226 = CARTESIAN_POINT ( 'NONE',  ( 7.644554776091147741E-16, 12.48450537969573659, -53.65625000204838102 ) ) ;
#34227 = CARTESIAN_POINT ( 'NONE',  ( -2.121150477449813534E-15, -11.54700538379251284, -52.25000000409676915 ) ) ;
#34228 = CARTESIAN_POINT ( 'NONE',  ( -10.81189881249999907, -6.242252689847864744, -3.468750002048353931 ) ) ;
#34229 = CARTESIAN_POINT ( 'NONE',  ( -9.999999999999998224, 1.224646799147353059E-15, -2.749999999999974687 ) ) ;
#34230 = CARTESIAN_POINT ( 'NONE',  ( -10.81189881249999907, -6.242252689847864744, -179.1562500020484094 ) ) ;
#34231 = CARTESIAN_POINT ( 'NONE',  ( -9.999999999999998224, 1.224646799147353059E-15, -160.6250000040967905 ) ) ;
#34232 = CARTESIAN_POINT ( 'NONE',  ( 9.999999999999998224, 0.000000000000000000, -199.4375000020484094 ) ) ;
#34233 = CARTESIAN_POINT ( 'NONE',  ( -9.999999999999998224, 1.224646799147353059E-15, -103.6250000040967763 ) ) ;
#34234 = DIRECTION ( 'NONE',  ( 0.7071067811865451302, 8.659560562354904508E-17, -0.7071067811865500152 ) ) ;
#34235 =( BOUNDED_CURVE ( )  B_SPLINE_CURVE ( 2, ( #13851, #14056, #3955, #36750, #19916, #27046, #4163 ),
 .UNSPECIFIED., .F., .F. ) 
 B_SPLINE_CURVE_WITH_KNOTS ( ( 3, 2, 2, 3 ),
 ( 0.6977611940298510396, 0.6990049751243784248, 0.7002487562189056991, 0.7014925373134330844 ),
 .UNSPECIFIED. ) 
 CURVE ( )  GEOMETRIC_REPRESENTATION_ITEM ( )  RATIONAL_B_SPLINE_CURVE ( ( 0.9999999999999641398, 0.8660254037844745678, 1.000000000000000000, 0.8660254037844387076, 1.000000000000000000, 0.8660254037844148378, 1.000000000000023981 ) ) 
 REPRESENTATION_ITEM ( '' )  );
#34236 = CARTESIAN_POINT ( 'NONE',  ( -9.999999999999998224, 1.224646799147353059E-15, -39.12500000409676915 ) ) ;
#34237 = EDGE_CURVE ( 'NONE', #30244, #21752, #25766, .T. ) ;
#34239 = EDGE_LOOP ( 'NONE', ( #10636, #18764, #14774, #4601 ) ) ;
#34238 = CARTESIAN_POINT ( 'NONE',  ( -5.405949406249996869, 9.363379034771805109, -82.03125000204839523 ) ) ;
#34241 = ORIENTED_EDGE ( 'NONE', *, *, #8901, .T. ) ;
#34240 = CARTESIAN_POINT ( 'NONE',  ( 0.000000000000000000, 5.321294541346989426, -220.0000000000000000 ) ) ;
#34242 = EDGE_LOOP ( 'NONE', ( #27260, #38831, #23649, #14283 ) ) ;
#34243 = CARTESIAN_POINT ( 'NONE',  ( -2.293366432827344421E-15, -12.48450537969573659, -36.21875000204835970 ) ) ;
#34244 = CARTESIAN_POINT ( 'NONE',  ( 10.81189881249999907, 6.242252689847868297, -25.21875000204837036 ) ) ;
#34245 = CARTESIAN_POINT ( 'NONE',  ( -10.81189881249999729, 1.324075727343319199E-15, -11.28125000204835438 ) ) ;
#34246 =( BOUNDED_CURVE ( )  B_SPLINE_CURVE ( 2, ( #17485, #40572, #11015, #20951, #4345, #40789, #11230 ),
 .UNSPECIFIED., .F., .F. ) 
 B_SPLINE_CURVE_WITH_KNOTS ( ( 3, 2, 2, 3 ),
 ( 0.3246268656716419510, 0.3258706467661692807, 0.3271144278606965550, 0.3283582089552238847 ),
 .UNSPECIFIED. ) 
 CURVE ( )  GEOMETRIC_REPRESENTATION_ITEM ( )  RATIONAL_B_SPLINE_CURVE ( ( 0.9999999999999820144, 0.8660254037844566932, 1.000000000000000000, 0.8660254037844387076, 1.000000000000000000, 0.8660254037844387076, 1.000000000000000000 ) ) 
 REPRESENTATION_ITEM ( '' )  );
#34247 = CARTESIAN_POINT ( 'NONE',  ( -2.293366432827344421E-15, -12.48450537969573659, -66.21875000204836681 ) ) ;
#34248 = CARTESIAN_POINT ( 'NONE',  ( 9.999999999999998224, 0.000000000000000000, -93.49999999999998579 ) ) ;
#34249 = CARTESIAN_POINT ( 'NONE',  ( 10.00000000000000000, 5.773502691896255534, -42.37499999999996447 ) ) ;
#34250 = CARTESIAN_POINT ( 'NONE',  ( 5.405949406249999534, 9.363379034771803333, -188.5937500020483810 ) ) ;
#34251 = CARTESIAN_POINT ( 'NONE',  ( 10.81189881249999729, 0.000000000000000000, -164.8437500020484094 ) ) ;
#34252 = EDGE_CURVE ( 'NONE', #2342, #14232, #42350, .T. ) ;
#34253 = CARTESIAN_POINT ( 'NONE',  ( 0.000000000000000000, 0.000000000000000000, -99.99999999999998579 ) ) ;
#34254 = CARTESIAN_POINT ( 'NONE',  ( -9.999999999999998224, 1.224646799147353059E-15, -200.0000000000000000 ) ) ;
#34255 = CARTESIAN_POINT ( 'NONE',  ( 9.999999999999998224, 0.000000000000000000, -113.3750000040967763 ) ) ;
#34256 = CARTESIAN_POINT ( 'NONE',  ( -9.999999999999479527, -5.773502691896549521, -90.00000000409674783 ) ) ;
#34257 = CARTESIAN_POINT ( 'NONE',  ( 5.405949406249999534, 9.363379034771803333, -115.0937500020483810 ) ) ;
#34258 = CYLINDRICAL_SURFACE ( 'NONE', #22498, 9.999999999999998224 ) ;
#34259 = CARTESIAN_POINT ( 'NONE',  ( -10.81189881249999907, -6.242252689847864744, -78.65625000204839523 ) ) ;
#34260 = CARTESIAN_POINT ( 'NONE',  ( 5.405949406249999534, 9.363379034771803333, -101.5937500020483810 ) ) ;
#34261 = CARTESIAN_POINT ( 'NONE',  ( -5.405949406250003975, -9.363379034771801557, -60.34375000204835970 ) ) ;
#34262 = CARTESIAN_POINT ( 'NONE',  ( 10.81189881249999729, 0.000000000000000000, -72.03125000204838102 ) ) ;
#34263 = CARTESIAN_POINT ( 'NONE',  ( -9.999999999999998224, 1.224646799147353059E-15, -150.1250000040967905 ) ) ;
#34264 = CARTESIAN_POINT ( 'NONE',  ( -9.999999999999998224, 5.773502691896259087, -130.3750000000000000 ) ) ;
#34265 = CARTESIAN_POINT ( 'NONE',  ( -10.81189881249999729, 1.324075727343319199E-15, -152.2812500020484094 ) ) ;
#34266 = CARTESIAN_POINT ( 'NONE',  ( -10.81189881249999729, 1.324075727343319199E-15, -164.2812500020484094 ) ) ;
#34267 = CARTESIAN_POINT ( 'NONE',  ( 4.999999999999992006, -8.660254037844389075, -145.1250000040967905 ) ) ;
#34268 = CARTESIAN_POINT ( 'NONE',  ( 9.999999999999998224, 0.000000000000000000, -173.0000000000000284 ) ) ;
#34269 = CARTESIAN_POINT ( 'NONE',  ( 5.405949406249999534, 9.363379034771803333, -97.09375000204838102 ) ) ;
#34270 = CARTESIAN_POINT ( 'NONE',  ( -9.999999999999998224, 1.224646799147353059E-15, -25.24999999999996803 ) ) ;
#34271 = CARTESIAN_POINT ( 'NONE',  ( 9.999999999999996447, -5.773502691896262640, -69.62499999999998579 ) ) ;
#34272 = CARTESIAN_POINT ( 'NONE',  ( -10.81189881249999729, 1.324075727343319199E-15, -3.781250002048375247 ) ) ;
#34273 = CARTESIAN_POINT ( 'NONE',  ( -2.121150477449813534E-15, -11.54700538379251284, -82.25000000409676204 ) ) ;
#34274 = FACE_OUTER_BOUND ( 'NONE', #10113, .T. ) ;
#34275 = CARTESIAN_POINT ( 'NONE',  ( -5.405949406250003975, -9.363379034771801557, -96.53125000204839523 ) ) ;
#34276 = CARTESIAN_POINT ( 'NONE',  ( -10.81189881249999729, -6.242252689847864744, -72.65625000204836681 ) ) ;
#34277 = CARTESIAN_POINT ( 'NONE',  ( 5.000000000000000000, 8.660254037844385522, -75.62500000409677625 ) ) ;
#34278 = CARTESIAN_POINT ( 'NONE',  ( -9.999999999999998224, 1.224646799147353059E-15, -134.7499999999999716 ) ) ;
#34279 = CARTESIAN_POINT ( 'NONE',  ( 10.81189881249999729, 0.000000000000000000, -34.34375000204836681 ) ) ;
#34280 = ORIENTED_EDGE ( 'NONE', *, *, #32791, .F. ) ;
#34281 = CARTESIAN_POINT ( 'NONE',  ( 10.81189881249999907, 6.242252689847868297, -197.9062500020484379 ) ) ;
#34282 = CARTESIAN_POINT ( 'NONE',  ( 10.81189881249999551, -6.242252689847874514, -28.65625000204838102 ) ) ;
#34283 = CARTESIAN_POINT ( 'NONE',  ( 7.644554776091147741E-16, 12.48450537969573659, -14.46875000204836859 ) ) ;
#34284 = CARTESIAN_POINT ( 'NONE',  ( 5.000000000000000000, 8.660254037844385522, -6.625000004096770923 ) ) ;
#34285 = CARTESIAN_POINT ( 'NONE',  ( -10.81189881249999907, -6.242252689847864744, -126.6562500020483810 ) ) ;
#34286 = EDGE_CURVE ( 'NONE', #41485, #22272, #3514, .T. ) ;
#34287 = CARTESIAN_POINT ( 'NONE',  ( 5.000000000000000000, 8.660254037844385522, -178.7500000000000284 ) ) ;
#34288 = CYLINDRICAL_SURFACE ( 'NONE', #12372, 9.999999999999998224 ) ;
#34290 = ORIENTED_EDGE ( 'NONE', *, *, #42385, .T. ) ;
#34289 = CARTESIAN_POINT ( 'NONE',  ( 5.405949406249992428, -9.363379034771808662, -106.7812500020483810 ) ) ;
#34291 = FACE_OUTER_BOUND ( 'NONE', #9644, .T. ) ;
#34292 = VERTEX_POINT ( 'NONE', #22311 ) ;
#34293 = ORIENTED_EDGE ( 'NONE', *, *, #40949, .F. ) ;
#34294 = CARTESIAN_POINT ( 'NONE',  ( 10.81189881249999907, 6.242252689847868297, -37.40625000204836681 ) ) ;
#34295 = PERSON_AND_ORGANIZATION_ROLE ( 'creator' ) ;
#34296 = CARTESIAN_POINT ( 'NONE',  ( -10.81189881249999907, -6.242252689847864744, -84.46875000204836681 ) ) ;
#34297 = CARTESIAN_POINT ( 'NONE',  ( 9.999999999999998224, 0.000000000000000000, -69.87500000409677625 ) ) ;
#34298 = DIRECTION ( 'NONE',  ( 0.000000000000000000, 0.000000000000000000, -1.000000000000000000 ) ) ;
#34299 = CARTESIAN_POINT ( 'NONE',  ( 10.00000000000102318, -5.773502691895667560, -32.50000000409672651 ) ) ;
#34300 = CARTESIAN_POINT ( 'NONE',  ( -10.81189881249999729, 1.324075727343319199E-15, -164.2812500020484094 ) ) ;
#34301 = CARTESIAN_POINT ( 'NONE',  ( -9.999999999998969713, -5.773502691896847949, -68.62499999999995737 ) ) ;
#34302 = ADVANCED_FACE ( 'NONE', ( #25974 ), #22519, .F. ) ;
#34303 = CARTESIAN_POINT ( 'NONE',  ( -5.405949406249996869, 9.363379034771805109, -123.8437500020483952 ) ) ;
#34304 =( BOUNDED_CURVE ( )  B_SPLINE_CURVE ( 2, ( #31784, #35438, #25305, #18161, #35017, #2215, #5446 ),
 .UNSPECIFIED., .F., .F. ) 
 B_SPLINE_CURVE_WITH_KNOTS ( ( 3, 2, 2, 3 ),
 ( 0.1455223880597014963, 0.1467661691542288538, 0.1480099502487562391, 0.1492537313432835966 ),
 .UNSPECIFIED. ) 
 CURVE ( )  GEOMETRIC_REPRESENTATION_ITEM ( )  RATIONAL_B_SPLINE_CURVE ( ( 1.000000000000000000, 0.8660254037844387076, 1.000000000000000000, 0.8660254037844387076, 1.000000000000000000, 0.8660254037844357100, 1.000000000000003109 ) ) 
 REPRESENTATION_ITEM ( '' )  );
#34305 = CARTESIAN_POINT ( 'NONE',  ( -2.293366432827344421E-15, -12.48450537969573659, -97.71875000204838102 ) ) ;
#34306 = CARTESIAN_POINT ( 'NONE',  ( 10.70731569305672615, 1.500182182589836044, 0.000000000000000000 ) ) ;
#34307 = CARTESIAN_POINT ( 'NONE',  ( 5.405949406249992428, -9.363379034771808662, -195.0937500020484094 ) ) ;
#34308 = CARTESIAN_POINT ( 'NONE',  ( -10.81189881249999907, -6.242252689847864744, -96.65625000204839523 ) ) ;
#34309 = CARTESIAN_POINT ( 'NONE',  ( 5.000000000000000000, 8.660254037844385522, -177.6250000040968189 ) ) ;
#34310 = CARTESIAN_POINT ( 'NONE',  ( 5.405949406249992428, -9.363379034771808662, -105.0937500020483810 ) ) ;
#34311 = CARTESIAN_POINT ( 'NONE',  ( -10.81189881249999729, 1.324075727343319199E-15, -174.7812500020484094 ) ) ;
#34312 = CARTESIAN_POINT ( 'NONE',  ( 4.999999999999992006, -8.660254037844389075, -28.12500000409676204 ) ) ;
#34313 = CARTESIAN_POINT ( 'NONE',  ( -4.999999999999996447, 8.660254037844387298, -181.5000000000000000 ) ) ;
#34314 = CARTESIAN_POINT ( 'NONE',  ( 5.405949406249999534, 9.363379034771803333, -196.2812500020484094 ) ) ;
#34315 = CARTESIAN_POINT ( 'NONE',  ( -10.81189881249999729, 1.324075727343319199E-15, -54.59375000204835970 ) ) ;
#34316 = CARTESIAN_POINT ( 'NONE',  ( -9.999999999999998224, 1.224646799147353059E-15, -171.1250000040968189 ) ) ;
#34317 = CARTESIAN_POINT ( 'NONE',  ( 5.405949406249999534, 9.363379034771803333, -10.28125000204835260 ) ) ;
#34318 = CARTESIAN_POINT ( 'NONE',  ( 10.81189881249999551, -6.242252689847874514, -22.46875000204837036 ) ) ;
#34319 = CARTESIAN_POINT ( 'NONE',  ( 5.500000000000003553, 20.00000000000000000, -220.0000000000000000 ) ) ;
#34320 = CARTESIAN_POINT ( 'NONE',  ( -5.405949406250003975, -9.363379034771801557, -129.3437500020484094 ) ) ;
#34321 = CARTESIAN_POINT ( 'NONE',  ( 9.999999999999996447, -5.773502691896262640, -98.12499999999998579 ) ) ;
#34322 = CARTESIAN_POINT ( 'NONE',  ( 10.81189881249999729, 0.000000000000000000, -28.53125000204837036 ) ) ;
#34323 = CARTESIAN_POINT ( 'NONE',  ( 5.000000000000000000, 8.660254037844385522, -104.1250000040967763 ) ) ;
#34324 = CARTESIAN_POINT ( 'NONE',  ( -5.000000000000003553, -8.660254037844383745, -48.99999999999998579 ) ) ;
#34325 = CARTESIAN_POINT ( 'NONE',  ( -5.405949406249996869, 9.363379034771805109, -125.5312500020483952 ) ) ;
#34326 = CARTESIAN_POINT ( 'NONE',  ( -5.405949406249996869, 9.363379034771805109, -97.03125000204839523 ) ) ;
#34327 = ORIENTED_EDGE ( 'NONE', *, *, #3505, .T. ) ;
#34328 = CARTESIAN_POINT ( 'NONE',  ( 7.070501591499377789E-16, 11.54700538379251284, -102.5000000040967763 ) ) ;
#34329 = CARTESIAN_POINT ( 'NONE',  ( -4.999999999999996447, 8.660254037844387298, -141.3750000040967905 ) ) ;
#34330 = CARTESIAN_POINT ( 'NONE',  ( -10.81189881249999729, 1.324075727343319199E-15, -167.2812500020484094 ) ) ;
#34331 = CARTESIAN_POINT ( 'NONE',  ( 7.644554776091147741E-16, 12.48450537969573659, -54.96875000204836681 ) ) ;
#34332 = ORIENTED_EDGE ( 'NONE', *, *, #17831, .T. ) ;
#34333 = CARTESIAN_POINT ( 'NONE',  ( 10.00000000000000000, 5.773502691896255534, -22.87499999999997868 ) ) ;
#34334 = CARTESIAN_POINT ( 'NONE',  ( 10.81189881249999729, 0.000000000000000000, -39.03125000204838102 ) ) ;
#34335 = CARTESIAN_POINT ( 'NONE',  ( 4.999999999999992006, -8.660254037844389075, -161.2500000000000000 ) ) ;
#34336 = AXIS2_PLACEMENT_3D ( 'NONE', #31493, #7752, #27817 ) ;
#34337 = LINE ( 'NONE', #14225, #22152 ) ;
#34338 = CARTESIAN_POINT ( 'NONE',  ( -5.000000000000003553, -8.660254037844383745, -29.87500000409676204 ) ) ;
#34339 = CARTESIAN_POINT ( 'NONE',  ( -9.999999999999998224, 1.224646799147353059E-15, -23.74999999999996447 ) ) ;
#34340 = CARTESIAN_POINT ( 'NONE',  ( 5.405949406249999534, 9.363379034771803333, -130.2812500020483810 ) ) ;
#34341 = CARTESIAN_POINT ( 'NONE',  ( 5.000000000000000000, 8.660254037844385522, -111.2499999999999858 ) ) ;
#34342 = CARTESIAN_POINT ( 'NONE',  ( 5.000000000000000000, 8.660254037844385522, -129.6250000040967620 ) ) ;
#34343 = ORIENTED_EDGE ( 'NONE', *, *, #9091, .F. ) ;
#34344 = CARTESIAN_POINT ( 'NONE',  ( -10.81189881249999729, 1.324075727343319199E-15, -59.28125000204836681 ) ) ;
#34346 = ORIENTED_EDGE ( 'NONE', *, *, #32330, .T. ) ;
#34345 = ORIENTED_EDGE ( 'NONE', *, *, #18012, .T. ) ;
#34347 = CYLINDRICAL_SURFACE ( 'NONE', #34597, 9.999999999999998224 ) ;
#34348 =( BOUNDED_CURVE ( )  B_SPLINE_CURVE ( 2, ( #35225, #27674, #11895, #40812, #37595, #8680, #5221 ),
 .UNSPECIFIED., .F., .F. ) 
 B_SPLINE_CURVE_WITH_KNOTS ( ( 3, 2, 2, 3 ),
 ( 0.1753731343283582433, 0.1766169154228856009, 0.1778606965174129861, 0.1791044776119403437 ),
 .UNSPECIFIED. ) 
 CURVE ( )  GEOMETRIC_REPRESENTATION_ITEM ( )  RATIONAL_B_SPLINE_CURVE ( ( 0.9999999999999970024, 0.8660254037844417052, 1.000000000000000000, 0.8660254037844387076, 1.000000000000000000, 0.8660254037844327124, 1.000000000000005995 ) ) 
 REPRESENTATION_ITEM ( '' )  );
#34349 = CARTESIAN_POINT ( 'NONE',  ( -5.405949406250003975, -9.363379034771801557, -162.3437500020484094 ) ) ;
#34350 = CARTESIAN_POINT ( 'NONE',  ( 10.81189881249999551, -6.242252689847874514, -186.1562500020484379 ) ) ;
#34351 = CARTESIAN_POINT ( 'NONE',  ( -5.405949406250003975, -9.363379034771801557, -12.34375000204834905 ) ) ;
#34352 = CARTESIAN_POINT ( 'NONE',  ( -10.00000000000051337, 5.773502691895962435, -49.37499999999996447 ) ) ;
#34353 = EDGE_CURVE ( 'NONE', #26059, #37408, #33309, .T. ) ;
#34354 = CARTESIAN_POINT ( 'NONE',  ( -10.81189881249999729, 1.324075727343319199E-15, -147.5937500020483810 ) ) ;
#34355 = VECTOR ( 'NONE', #31386, 1000.000000000000000 ) ;
#34356 = CARTESIAN_POINT ( 'NONE',  ( -5.405949406250003975, -9.363379034771801557, -129.3437500020484094 ) ) ;
#34357 = EDGE_CURVE ( 'NONE', #25200, #35567, #3943, .T. ) ;
#34358 = CARTESIAN_POINT ( 'NONE',  ( 10.81189881249999729, 0.000000000000000000, -108.0312500020483810 ) ) ;
#34359 = CARTESIAN_POINT ( 'NONE',  ( 5.405949406249992428, -9.363379034771808662, -114.0937500020483810 ) ) ;
#34360 = CARTESIAN_POINT ( 'NONE',  ( -4.999999999999996447, 8.660254037844387298, -193.8750000040967905 ) ) ;
#34361 = CARTESIAN_POINT ( 'NONE',  ( 10.81189881249999729, 0.000000000000000000, -126.0312500020483952 ) ) ;
#34362 = CARTESIAN_POINT ( 'NONE',  ( -5.405949406249996869, 9.363379034771805109, -0.8437500020483656993 ) ) ;
#34363 = CARTESIAN_POINT ( 'NONE',  ( -2.293366432827344421E-15, -12.48450537969573659, -133.7187500020483810 ) ) ;
#34364 = CARTESIAN_POINT ( 'NONE',  ( 9.999999999999994671, -5.773502691896262640, -166.0000000040967905 ) ) ;
#34365 = CARTESIAN_POINT ( 'NONE',  ( -5.000000000000005329, -20.00000000000000000, -219.9999999999999716 ) ) ;
#34366 = CARTESIAN_POINT ( 'NONE',  ( -4.999999999999996447, 8.660254037844387298, -145.5000000000000000 ) ) ;
#34367 = CARTESIAN_POINT ( 'NONE',  ( -9.999999999999998224, 5.773502691896259087, -20.87499999999997868 ) ) ;
#34368 = CARTESIAN_POINT ( 'NONE',  ( -5.405949406249996869, 9.363379034771805109, -77.34375000204838102 ) ) ;
#34369 = CARTESIAN_POINT ( 'NONE',  ( 7.644554776091147741E-16, 12.48450537969573659, -63.96875000204837391 ) ) ;
#34370 = CARTESIAN_POINT ( 'NONE',  ( -2.121150477449813534E-15, -11.54700538379251284, -170.3750000000000000 ) ) ;
#34371 = CARTESIAN_POINT ( 'NONE',  ( -10.81189881249999729, 1.324075727343319199E-15, -32.28125000204837391 ) ) ;
#34372 = CARTESIAN_POINT ( 'NONE',  ( -2.293366432827344421E-15, -12.48450537969573659, -43.71875000204835970 ) ) ;
#34373 = CARTESIAN_POINT ( 'NONE',  ( -9.999999999999998224, 1.224646799147353059E-15, -31.62500000409676559 ) ) ;
#34374 = CARTESIAN_POINT ( 'NONE',  ( 10.81189881249999551, -6.242252689847874514, -154.4687500020484094 ) ) ;
#34375 = CARTESIAN_POINT ( 'NONE',  ( 4.999999999999992006, -8.660254037844389075, -122.2500000000000000 ) ) ;
#34376 = CARTESIAN_POINT ( 'NONE',  ( 10.81189881249999729, 0.000000000000000000, -130.5312500020484094 ) ) ;
#34377 = CARTESIAN_POINT ( 'NONE',  ( 5.502678791411631742, 8.887464070476337241, -179.9999999999999432 ) ) ;
#34378 = CARTESIAN_POINT ( 'NONE',  ( 9.999999999999996447, -5.773502691896262640, -74.12499999999997158 ) ) ;
#34379 = CARTESIAN_POINT ( 'NONE',  ( 7.644554776091147741E-16, 12.48450537969573659, -16.15625000204837747 ) ) ;
#34380 = VERTEX_POINT ( 'NONE', #4368 ) ;
#34381 = CARTESIAN_POINT ( 'NONE',  ( -10.81189881249999729, 1.324075727343319199E-15, -101.2812500020483952 ) ) ;
#34382 = CARTESIAN_POINT ( 'NONE',  ( -2.121150477449813534E-15, -11.54700538379251284, -122.7500000040967905 ) ) ;
#34383 = CARTESIAN_POINT ( 'NONE',  ( 10.00000000000038014, -5.773502691896040595, -179.5000000040967620 ) ) ;
#34384 = CARTESIAN_POINT ( 'NONE',  ( 9.999999999999996447, -5.773502691896262640, -35.50000000409675494 ) ) ;
#34385 = CARTESIAN_POINT ( 'NONE',  ( -4.999999999999996447, 8.660254037844387298, -74.99999999999998579 ) ) ;
#34386 = CARTESIAN_POINT ( 'NONE',  ( -10.81189881249999729, 1.324075727343319199E-15, -45.78125000204838813 ) ) ;
#34387 = CARTESIAN_POINT ( 'NONE',  ( 10.00000000000021672, -5.773502691896130301, -191.1249999999999716 ) ) ;
#34388 = CARTESIAN_POINT ( 'NONE',  ( 5.405949406249992428, -9.363379034771808662, -156.2812500020484094 ) ) ;
#34389 = CARTESIAN_POINT ( 'NONE',  ( -5.405949406250003975, -9.363379034771801557, -127.8437500020483952 ) ) ;
#34390 = CARTESIAN_POINT ( 'NONE',  ( -9.999999999999998224, 1.224646799147353059E-15, -8.749999999999952038 ) ) ;
#34391 = ADVANCED_FACE ( 'NONE', ( #14257 ), #719, .T. ) ;
#34392 = ORIENTED_EDGE ( 'NONE', *, *, #18399, .T. ) ;
#34393 = CARTESIAN_POINT ( 'NONE',  ( 10.40594940624999865, 0.000000000000000000, -199.1093750030726142 ) ) ;
#34394 = ORIENTED_EDGE ( 'NONE', *, *, #6160, .F. ) ;
#34395 = ORIENTED_EDGE ( 'NONE', *, *, #40441, .F. ) ;
#34396 = ORIENTED_EDGE ( 'NONE', *, *, #14409, .F. ) ;
#34397 = CARTESIAN_POINT ( 'NONE',  ( -10.00000000000022027, 5.773502691896128525, -188.8750000000000284 ) ) ;
#34398 = CARTESIAN_POINT ( 'NONE',  ( -5.405949406250003975, -9.363379034771801557, -193.8437500020484094 ) ) ;
#34399 = CARTESIAN_POINT ( 'NONE',  ( -10.81189881249999729, 1.324075727343319199E-15, -39.59375000204837391 ) ) ;
#34400 = CARTESIAN_POINT ( 'NONE',  ( 1.250775920587201551, -10.41851302423964221, 8.157905031340290035E-16 ) ) ;
#34401 = CARTESIAN_POINT ( 'NONE',  ( 9.999999999999998224, 0.000000000000000000, -14.37500000409674961 ) ) ;
#34402 = EDGE_CURVE ( 'NONE', #6396, #21320, #16667, .T. ) ;
#34403 = CARTESIAN_POINT ( 'NONE',  ( 5.405949406249992428, -9.363379034771808662, -175.5937500020484094 ) ) ;
#34404 = CARTESIAN_POINT ( 'NONE',  ( -10.81189881249999729, 6.242252689847871849, -158.2187500020483810 ) ) ;
#34405 = CARTESIAN_POINT ( 'NONE',  ( -7.959047257566134870E-15, 145.0000000000000000, 42.49999999999999289 ) ) ;
#34406 = CARTESIAN_POINT ( 'NONE',  ( -10.81189881249999907, -6.242252689847864744, -142.9687500020484094 ) ) ;
#34407 = CARTESIAN_POINT ( 'NONE',  ( -5.405949406249996869, 9.363379034771805109, -151.0312500020483810 ) ) ;
#34409 = EDGE_CURVE ( 'NONE', #42377, #5520, #21099, .T. ) ;
#34408 = CARTESIAN_POINT ( 'NONE',  ( 5.405949406249992428, -9.363379034771808662, -151.5937500020483810 ) ) ;
#34410 = DIRECTION ( 'NONE',  ( -0.000000000000000000, -0.000000000000000000, 1.000000000000000000 ) ) ;
#34411 = LINE ( 'NONE', #17762, #6178 ) ;
#34412 = CARTESIAN_POINT ( 'NONE',  ( -5.000000000000003553, -8.660254037844383745, -167.5000000000000000 ) ) ;
#34413 = EDGE_CURVE ( 'NONE', #41597, #1789, #25537, .T. ) ;
#34414 = CARTESIAN_POINT ( 'NONE',  ( 5.405949406249999534, 9.363379034771803333, -86.59375000204836681 ) ) ;
#34415 = CARTESIAN_POINT ( 'NONE',  ( -4.999999999999996447, 8.660254037844387298, -198.3750000040967905 ) ) ;
#34416 = CARTESIAN_POINT ( 'NONE',  ( -10.81189881249999729, 6.242252689847871849, -60.90625000204837391 ) ) ;
#34417 = CARTESIAN_POINT ( 'NONE',  ( -9.999999999998456346, -5.773502691897145489, -16.50000000409671941 ) ) ;
#34418 = CARTESIAN_POINT ( 'NONE',  ( 10.81189881249999729, 0.000000000000000000, -178.3437500020483810 ) ) ;
#34419 = CARTESIAN_POINT ( 'NONE',  ( -10.81189881249999729, 1.324075727343319199E-15, -113.2812500020483952 ) ) ;
#34420 = CARTESIAN_POINT ( 'NONE',  ( 10.81189881249999551, -6.242252689847874514, -153.1562500020484094 ) ) ;
#34421 = DIRECTION ( 'NONE',  ( -0.000000000000000000, -0.000000000000000000, -1.000000000000000000 ) ) ;
#34422 = CARTESIAN_POINT ( 'NONE',  ( -5.405949406249996869, 9.363379034771805109, -44.53125000204838102 ) ) ;
#34423 = CARTESIAN_POINT ( 'NONE',  ( -9.999999999999998224, 1.224646799147353059E-15, -133.6250000040967620 ) ) ;
#34424 = CARTESIAN_POINT ( 'NONE',  ( -9.999999999999998224, 5.773502691896259087, -110.8749999999999858 ) ) ;
#34425 = EDGE_LOOP ( 'NONE', ( #21491, #22290, #38291, #12902 ) ) ;
#34426 = CARTESIAN_POINT ( 'NONE',  ( 5.405949406249992428, -9.363379034771808662, -127.7812500020483810 ) ) ;
#34427 = CARTESIAN_POINT ( 'NONE',  ( 10.00000000000000000, 5.773502691896255534, -144.7500000040967905 ) ) ;
#34428 = LINE ( 'NONE', #34217, #7715 ) ;
#34429 = VECTOR ( 'NONE', #4243, 1000.000000000000000 ) ;
#34430 = CARTESIAN_POINT ( 'NONE',  ( 10.81189881249999551, -6.242252689847874514, -183.1562500020484094 ) ) ;
#34431 = VERTEX_POINT ( 'NONE', #27032 ) ;
#34432 = CARTESIAN_POINT ( 'NONE',  ( 5.405949406249999534, 9.363379034771803333, -172.0937500020484094 ) ) ;
#34433 = CARTESIAN_POINT ( 'NONE',  ( 4.999999999999992006, -8.660254037844389075, -55.12500000409675494 ) ) ;
#34434 = DIRECTION ( 'NONE',  ( 0.000000000000000000, 0.000000000000000000, -1.000000000000000000 ) ) ;
#34435 = CARTESIAN_POINT ( 'NONE',  ( -10.00000000000076916, 5.773502691895813221, -130.3750000000000000 ) ) ;
#34436 = CARTESIAN_POINT ( 'NONE',  ( 5.405949406249992428, -9.363379034771808662, -69.28125000204838102 ) ) ;
#34437 = CARTESIAN_POINT ( 'NONE',  ( 10.81189881249999551, -6.242252689847874514, -49.65625000204837391 ) ) ;
#34438 = EDGE_CURVE ( 'NONE', #7438, #6420, #10608, .T. ) ;
#34439 = CARTESIAN_POINT ( 'NONE',  ( 4.999999999999992006, -8.660254037844389075, -46.12500000409677625 ) ) ;
#34440 = AXIS2_PLACEMENT_3D ( 'NONE', #6903, #26963, #36679 ) ;
#34441 = CARTESIAN_POINT ( 'NONE',  ( -5.405949406249996869, 9.363379034771805109, -2.343750002048366810 ) ) ;
#34442 = CARTESIAN_POINT ( 'NONE',  ( -9.999999999999998224, 1.224646799147353059E-15, -200.0000000000000000 ) ) ;
#34443 = CARTESIAN_POINT ( 'NONE',  ( -5.405949406249996869, 9.363379034771805109, -176.5312500020483810 ) ) ;
#34444 = DIRECTION ( 'NONE',  ( -0.000000000000000000, -0.000000000000000000, 1.000000000000000000 ) ) ;
#34445 = PLANE ( 'NONE',  #31695 ) ;
#34446 = ORIENTED_EDGE ( 'NONE', *, *, #15885, .F. ) ;
#34447 = CARTESIAN_POINT ( 'NONE',  ( 4.999999999999992006, -8.660254037844389075, -0.7499999999999729106 ) ) ;
#34448 =( BOUNDED_CURVE ( )  B_SPLINE_CURVE ( 2, ( #36813, #26888, #27105, #30356, #3600, #6614, #40043 ),
 .UNSPECIFIED., .F., .F. ) 
 B_SPLINE_CURVE_WITH_KNOTS ( ( 3, 2, 2, 3 ),
 ( 0.1044776119402986148, 0.1057213930348259306, 0.1069651741293532465, 0.1082089552238805485 ),
 .UNSPECIFIED. ) 
 CURVE ( )  GEOMETRIC_REPRESENTATION_ITEM ( )  RATIONAL_B_SPLINE_CURVE ( ( 0.9999999999999880096, 0.8660254037844506980, 1.000000000000000000, 0.8660254037844387076, 1.000000000000000000, 0.8660254037844431485, 0.9999999999999955591 ) ) 
 REPRESENTATION_ITEM ( '' )  );
#34449 = DIRECTION ( 'NONE',  ( -0.000000000000000000, -0.000000000000000000, -1.000000000000000000 ) ) ;
#34451 = VERTEX_POINT ( 'NONE', #20539 ) ;
#34450 = CARTESIAN_POINT ( 'NONE',  ( 10.81189881249999551, -6.242252689847874514, -87.15625000204838102 ) ) ;
#34453 = EDGE_LOOP ( 'NONE', ( #6084, #4704, #10427, #7091 ) ) ;
#34452 = LINE ( 'NONE', #21482, #32396 ) ;
#34454 = ORIENTED_EDGE ( 'NONE', *, *, #16750, .F. ) ;
#34455 = CARTESIAN_POINT ( 'NONE',  ( 7.644554776091147741E-16, 12.48450537969573659, -35.46875000204835260 ) ) ;
#34456 = CARTESIAN_POINT ( 'NONE',  ( 10.81189881249999729, 0.000000000000000000, -29.84375000204836326 ) ) ;
#34457 = CARTESIAN_POINT ( 'NONE',  ( -10.81189881249999729, 6.242252689847871849, -17.40625000204838457 ) ) ;
#34458 = AXIS2_PLACEMENT_3D ( 'NONE', #26886, #156, #33590 ) ;
#34460 = ORIENTED_EDGE ( 'NONE', *, *, #12979, .F. ) ;
#34459 = CARTESIAN_POINT ( 'NONE',  ( 10.81189881249999729, 0.000000000000000000, -62.84375000204836681 ) ) ;
#34461 = CARTESIAN_POINT ( 'NONE',  ( -9.999999999999998224, 5.773502691896259087, -34.37499999999996447 ) ) ;
#34462 = CARTESIAN_POINT ( 'NONE',  ( 5.405949406249999534, 9.363379034771803333, -184.0937500020483810 ) ) ;
#34463 = CARTESIAN_POINT ( 'NONE',  ( 10.81189881249999551, -6.242252689847874514, -166.4687500020484094 ) ) ;
#34464 = CARTESIAN_POINT ( 'NONE',  ( 5.405949406249999534, 9.363379034771803333, -178.0937500020484094 ) ) ;
#34465 = CARTESIAN_POINT ( 'NONE',  ( 9.999999999998969713, 5.773502691896851502, -59.25000000409674783 ) ) ;
#34466 = CARTESIAN_POINT ( 'NONE',  ( 9.999999999999998224, 0.000000000000000000, -71.37500000409677625 ) ) ;
#34467 = CARTESIAN_POINT ( 'NONE',  ( -9.999999999999998224, 1.224646799147353059E-15, -104.7499999999999858 ) ) ;
#34468 = CARTESIAN_POINT ( 'NONE',  ( 9.999999999998969713, 5.773502691896851502, -60.75000000409676204 ) ) ;
#34469 = CARTESIAN_POINT ( 'NONE',  ( 5.405949406249992428, -9.363379034771808662, -114.0937500020483810 ) ) ;
#34470 = CARTESIAN_POINT ( 'NONE',  ( 9.999999999999998224, 0.000000000000000000, -111.4999999999999858 ) ) ;
#34471 = CARTESIAN_POINT ( 'NONE',  ( -10.81189881249999729, 1.324075727343319199E-15, -84.78125000204838102 ) ) ;
#34472 = CARTESIAN_POINT ( 'NONE',  ( 10.81189881249999551, -6.242252689847874514, -91.46875000204838102 ) ) ;
#34473 = CARTESIAN_POINT ( 'NONE',  ( 10.81189881249999907, 6.242252689847868297, -62.71875000204838102 ) ) ;
#34474 = CARTESIAN_POINT ( 'NONE',  ( 10.81189881249999907, 6.242252689847868297, -71.90625000204836681 ) ) ;
#34475 = CARTESIAN_POINT ( 'NONE',  ( -10.00000000000000000, -5.773502691896251982, -157.5000000040968189 ) ) ;
#34476 = CARTESIAN_POINT ( 'NONE',  ( 7.070501591499377789E-16, 11.54700538379251284, -129.1250000000000000 ) ) ;
#34477 =( BOUNDED_CURVE ( )  B_SPLINE_CURVE ( 2, ( #17907, #38204, #34341, #28077, #14450, #8649, #1103 ),
 .UNSPECIFIED., .F., .F. ) 
 B_SPLINE_CURVE_WITH_KNOTS ( ( 3, 2, 2, 3 ),
 ( 0.4402985074626867279, 0.4415422885572141132, 0.4427860696517414429, 0.4440298507462688282 ),
 .UNSPECIFIED. ) 
 CURVE ( )  GEOMETRIC_REPRESENTATION_ITEM ( )  RATIONAL_B_SPLINE_CURVE ( ( 0.9999999999999820144, 0.8660254037844566932, 1.000000000000000000, 0.8660254037844387076, 1.000000000000000000, 0.8660254037844207220, 1.000000000000017986 ) ) 
 REPRESENTATION_ITEM ( '' )  );
#34478 = CARTESIAN_POINT ( 'NONE',  ( 10.81189881249999729, 6.242252689847867408, -149.9062500020484094 ) ) ;
#34479 = CARTESIAN_POINT ( 'NONE',  ( 10.81189881249999729, 0.000000000000000000, -163.5312500020484094 ) ) ;
#34480 = ADVANCED_FACE ( 'NONE', ( #40176 ), #33728, .T. ) ;
#34481 = DIRECTION ( 'NONE',  ( 1.000000000000000000, 0.000000000000000000, 0.000000000000000000 ) ) ;
#34482 = CARTESIAN_POINT ( 'NONE',  ( -10.00000000000025580, 5.773502691896109873, -159.2500000040968189 ) ) ;
#34483 = CARTESIAN_POINT ( 'NONE',  ( 7.644554776091147741E-16, 12.48450537969573659, -99.96875000204839523 ) ) ;
#34484 = CARTESIAN_POINT ( 'NONE',  ( -4.999999999999996447, 8.660254037844387298, -10.49999999999995381 ) ) ;
#34485 = CARTESIAN_POINT ( 'NONE',  ( 9.999999999999998224, 0.000000000000000000, -73.99999999999998579 ) ) ;
#34486 = CARTESIAN_POINT ( 'NONE',  ( -10.81189881249999729, 6.242252689847871849, -195.7187500020484379 ) ) ;
#34487 = CARTESIAN_POINT ( 'NONE',  ( 9.999999999999996447, -5.773502691896262640, -79.00000000409677625 ) ) ;
#34488 = CARTESIAN_POINT ( 'NONE',  ( 3.754465651702444173, -9.907696901662989220, -180.0000000000000000 ) ) ;
#34489 = CARTESIAN_POINT ( 'NONE',  ( 5.405949406249999534, 9.363379034771803333, -94.28125000204838102 ) ) ;
#34490 = CARTESIAN_POINT ( 'NONE',  ( -5.405949406249996869, 9.363379034771805109, -79.03125000204838102 ) ) ;
#34491 =( BOUNDED_CURVE ( )  B_SPLINE_CURVE ( 2, ( #17566, #39819, #775, #567, #24078, #7033, #40236 ),
 .UNSPECIFIED., .F., .F. ) 
 B_SPLINE_CURVE_WITH_KNOTS ( ( 3, 2, 2, 3 ),
 ( 0.09701492537313441411, 0.09825870646766173000, 0.09950248756218905977, 0.1007462686567163757 ),
 .UNSPECIFIED. ) 
 CURVE ( )  GEOMETRIC_REPRESENTATION_ITEM ( )  RATIONAL_B_SPLINE_CURVE ( ( 0.9999999999999910072, 0.8660254037844477004, 1.000000000000000000, 0.8660254037844387076, 1.000000000000000000, 0.8660254037844431485, 0.9999999999999955591 ) ) 
 REPRESENTATION_ITEM ( '' )  );
#34492 = CARTESIAN_POINT ( 'NONE',  ( 9.999999999999996447, -5.773502691896262640, -65.50000000409677625 ) ) ;
#34493 = CARTESIAN_POINT ( 'NONE',  ( -10.81189881249999907, -6.242252689847864744, -28.96875000204835260 ) ) ;
#34494 = ORIENTED_EDGE ( 'NONE', *, *, #35036, .F. ) ;
#34495 = CARTESIAN_POINT ( 'NONE',  ( 9.999999999999996447, -5.773502691896262640, -3.624999999999953371 ) ) ;
#34496 = VECTOR ( 'NONE', #35770, 1000.000000000000000 ) ;
#34497 = CARTESIAN_POINT ( 'NONE',  ( 10.81189881249999551, -6.242252689847874514, -31.65625000204835615 ) ) ;
#34498 = CARTESIAN_POINT ( 'NONE',  ( 5.405949406249999534, 9.363379034771803333, -14.59375000204835082 ) ) ;
#34499 = CARTESIAN_POINT ( 'NONE',  ( -2.121150477449813534E-15, -11.54700538379251284, -64.25000000409677625 ) ) ;
#34500 = CARTESIAN_POINT ( 'NONE',  ( 9.999999999999998224, 0.000000000000000000, -5.375000004096769146 ) ) ;
#34501 = CARTESIAN_POINT ( 'NONE',  ( 4.999999999999992006, -8.660254037844389075, -138.7499999999999716 ) ) ;
#34502 = CARTESIAN_POINT ( 'NONE',  ( -10.81189881249999729, 6.242252689847871849, -129.9062500020483810 ) ) ;
#34503 =( BOUNDED_CURVE ( )  B_SPLINE_CURVE ( 2, ( #29530, #13314, #42672, #26297, #39446, #36211, #26503 ),
 .UNSPECIFIED., .F., .F. ) 
 B_SPLINE_CURVE_WITH_KNOTS ( ( 3, 2, 2, 3 ),
 ( 0.2126865671641791633, 0.2139303482587065208, 0.2151741293532339061, 0.2164179104477612636 ),
 .UNSPECIFIED. ) 
 CURVE ( )  GEOMETRIC_REPRESENTATION_ITEM ( )  RATIONAL_B_SPLINE_CURVE ( ( 0.9999999999999940048, 0.8660254037844447028, 1.000000000000000000, 0.8660254037844387076, 1.000000000000000000, 0.8660254037844297148, 1.000000000000008882 ) ) 
 REPRESENTATION_ITEM ( '' )  );
#34504 = CARTESIAN_POINT ( 'NONE',  ( -4.999999999999996447, 8.660254037844387298, -186.0000000000000000 ) ) ;
#34505 = CARTESIAN_POINT ( 'NONE',  ( 9.999999999999998224, 0.000000000000000000, -125.0000000000000000 ) ) ;
#34507 = VERTEX_POINT ( 'NONE', #10822 ) ;
#34506 = CARTESIAN_POINT ( 'NONE',  ( 5.405949406249999534, 9.363379034771803333, -106.2812500020483810 ) ) ;
#34508 = CARTESIAN_POINT ( 'NONE',  ( 9.999999999999998224, 0.000000000000000000, -170.3750000040968189 ) ) ;
#34509 = ORIENTED_EDGE ( 'NONE', *, *, #31909, .T. ) ;
#34510 = ORIENTED_EDGE ( 'NONE', *, *, #25926, .T. ) ;
#34511 = CARTESIAN_POINT ( 'NONE',  ( 5.405949406249999534, 9.363379034771803333, -41.78125000204838102 ) ) ;
#34512 = APPROVAL_DATE_TIME ( #8604, #31498 ) ;
#34513 = CARTESIAN_POINT ( 'NONE',  ( 10.81189881249999551, -6.242252689847874514, -88.46875000204836681 ) ) ;
#34514 = CARTESIAN_POINT ( 'NONE',  ( 9.999999999999998224, 0.000000000000000000, -128.3750000040967905 ) ) ;
#34515 = CARTESIAN_POINT ( 'NONE',  ( 4.999999999999992006, -8.660254037844389075, -128.6250000040967620 ) ) ;
#34516 = LINE ( 'NONE', #31281, #4001 ) ;
#34517 = CARTESIAN_POINT ( 'NONE',  ( 7.644554776091147741E-16, 12.48450537969573659, -167.6562500020483810 ) ) ;
#34518 = CARTESIAN_POINT ( 'NONE',  ( 7.070501591499376803E-16, 11.54700538379251284, -54.50000000409677625 ) ) ;
#34519 = AXIS2_PLACEMENT_3D ( 'NONE', #39345, #36332, #6763 ) ;
#34520 = CARTESIAN_POINT ( 'NONE',  ( 10.81189881249999729, 0.000000000000000000, -121.3437500020483952 ) ) ;
#34521 = CARTESIAN_POINT ( 'NONE',  ( 7.644554776091147741E-16, 12.48450537969573659, -84.96875000204835260 ) ) ;
#34522 = CARTESIAN_POINT ( 'NONE',  ( -10.81189881249999729, 6.242252689847871849, -5.406250002048357928 ) ) ;
#34523 = CARTESIAN_POINT ( 'NONE',  ( 10.81189881249999551, -6.242252689847874514, -196.4687500020484094 ) ) ;
#34524 = CARTESIAN_POINT ( 'NONE',  ( -2.293366432827344421E-15, -12.48450537969573659, -94.90625000204838102 ) ) ;
#34525 = CARTESIAN_POINT ( 'NONE',  ( 7.070501591499377789E-16, 11.54700538379251284, -177.5000000040967905 ) ) ;
#34526 = CARTESIAN_POINT ( 'NONE',  ( 10.81189881249999729, 0.000000000000000000, -169.5312500020484094 ) ) ;
#34527 = CARTESIAN_POINT ( 'NONE',  ( -5.405949406249996869, 9.363379034771805109, -176.5312500020483810 ) ) ;
#34528 = CARTESIAN_POINT ( 'NONE',  ( 10.81189881249999729, 0.000000000000000000, -190.5312500020484094 ) ) ;
#34529 = CARTESIAN_POINT ( 'NONE',  ( 5.405949406249992428, -9.363379034771808662, -55.59375000204835970 ) ) ;
#34530 = CARTESIAN_POINT ( 'NONE',  ( -2.121150477449813534E-15, -11.54700538379251284, -166.2500000040968189 ) ) ;
#34531 = CARTESIAN_POINT ( 'NONE',  ( -5.405949406249996869, 9.363379034771805109, -11.53125000204835438 ) ) ;
#34532 = CARTESIAN_POINT ( 'NONE',  ( 5.405949406249999534, 9.363379034771803333, -10.09375000204834549 ) ) ;
#34533 = FACE_OUTER_BOUND ( 'NONE', #3387, .T. ) ;
#34534 = CARTESIAN_POINT ( 'NONE',  ( -5.405949406250003975, -9.363379034771801557, -123.3437500020483952 ) ) ;
#34535 = CARTESIAN_POINT ( 'NONE',  ( -9.999999999999998224, 5.773502691896259087, -97.37500000000000000 ) ) ;
#34536 = CARTESIAN_POINT ( 'NONE',  ( 10.81189881249999551, -6.242252689847874514, -22.65625000204837747 ) ) ;
#34537 = CARTESIAN_POINT ( 'NONE',  ( 7.070501591499377789E-16, 11.54700538379251284, -104.0000000040967763 ) ) ;
#34538 = CARTESIAN_POINT ( 'NONE',  ( 4.999999999999992006, -8.660254037844389075, -51.74999999999996447 ) ) ;
#34539 = CARTESIAN_POINT ( 'NONE',  ( 10.81189881249999729, 0.000000000000000000, -112.5312500020483952 ) ) ;
#34540 = CARTESIAN_POINT ( 'NONE',  ( 10.81189881249999729, 6.242252689847867408, -103.4062500020483952 ) ) ;
#34541 = ORIENTED_EDGE ( 'NONE', *, *, #14180, .T. ) ;
#34542 = CARTESIAN_POINT ( 'NONE',  ( -2.121150477449813534E-15, -11.54700538379251284, -97.25000000409679046 ) ) ;
#34543 = CARTESIAN_POINT ( 'NONE',  ( -9.999999999999998224, 1.224646799147353059E-15, -163.6250000040967905 ) ) ;
#34544 = CARTESIAN_POINT ( 'NONE',  ( 5.405949406249999534, 9.363379034771803333, -163.2812500020484094 ) ) ;
#34545 = CARTESIAN_POINT ( 'NONE',  ( -10.81189881249999729, 1.324075727343319199E-15, -47.09375000204838102 ) ) ;
#34546 = EDGE_LOOP ( 'NONE', ( #208, #30936, #19272, #39666 ) ) ;
#34547 = CARTESIAN_POINT ( 'NONE',  ( -10.00000000000000000, -5.773502691896251982, -23.62499999999998224 ) ) ;
#34548 = CARTESIAN_POINT ( 'NONE',  ( 10.81189881249999729, 0.000000000000000000, -27.03125000204836681 ) ) ;
#34549 = CARTESIAN_POINT ( 'NONE',  ( -4.999999999999996447, 8.660254037844387298, -162.0000000000000000 ) ) ;
#34550 = CARTESIAN_POINT ( 'NONE',  ( -9.999999999999998224, 1.224646799147353059E-15, -25.62500000409675849 ) ) ;
#34551 = CARTESIAN_POINT ( 'NONE',  ( -4.999999999999996447, 8.660254037844387298, -27.37500000409676204 ) ) ;
#34552 = LOCAL_TIME ( 11, 57, 6.000000000000000000, #2184 ) ;
#34553 = CARTESIAN_POINT ( 'NONE',  ( -9.999999999999998224, 1.224646799147353059E-15, -167.7500000000000000 ) ) ;
#34554 = CARTESIAN_POINT ( 'NONE',  ( 5.405949406249992428, -9.363379034771808662, -133.7812500020483810 ) ) ;
#34555 = LINE ( 'NONE', #12078, #16225 ) ;
#34556 = ORIENTED_EDGE ( 'NONE', *, *, #26106, .T. ) ;
#34557 = CARTESIAN_POINT ( 'NONE',  ( -10.81189881249999729, 6.242252689847871849, -60.90625000204837391 ) ) ;
#34558 = DATE_AND_TIME ( #1758, #8396 ) ;
#34560 = ORIENTED_EDGE ( 'NONE', *, *, #32743, .T. ) ;
#34559 = ORIENTED_EDGE ( 'NONE', *, *, #20347, .F. ) ;
#34561 =( BOUNDED_CURVE ( )  B_SPLINE_CURVE ( 2, ( #10133, #6066, #32193, #15752, #32614, #2620, #3039 ),
 .UNSPECIFIED., .F., .F. ) 
 B_SPLINE_CURVE_WITH_KNOTS ( ( 3, 2, 2, 3 ),
 ( 0.2462686567164180107, 0.2475124378109453960, 0.2487562189054727535, 0.2500000000000001110 ),
 .UNSPECIFIED. ) 
 CURVE ( )  GEOMETRIC_REPRESENTATION_ITEM ( )  RATIONAL_B_SPLINE_CURVE ( ( 0.9999999999999880096, 0.8660254037844506980, 1.000000000000000000, 0.8660254037844387076, 1.000000000000000000, 0.8660254037844267172, 1.000000000000011990 ) ) 
 REPRESENTATION_ITEM ( '' )  );
#34562 = CARTESIAN_POINT ( 'NONE',  ( 9.999999999999676703, 5.773502691896441164, -182.2500000040967620 ) ) ;
#34563 = CARTESIAN_POINT ( 'NONE',  ( -9.999999999999868550, 5.773502691896333694, -174.2500000040967905 ) ) ;
#34564 = CARTESIAN_POINT ( 'NONE',  ( 10.81189881249999729, 0.000000000000000000, -160.3437500020484094 ) ) ;
#34565 = CARTESIAN_POINT ( 'NONE',  ( -5.405949406250003975, -9.363379034771801557, -185.0312500020484094 ) ) ;
#34566 = CARTESIAN_POINT ( 'NONE',  ( -5.405949406249996869, 9.363379034771805109, -11.34375000204834727 ) ) ;
#34567 = DIRECTION ( 'NONE',  ( 1.000000000000000000, 0.000000000000000000, 0.000000000000000000 ) ) ;
#34568 = CARTESIAN_POINT ( 'NONE',  ( 10.81189881249999729, 6.242252689847867408, -149.7187500020483810 ) ) ;
#34569 = CARTESIAN_POINT ( 'NONE',  ( -10.81189881249999907, -6.242252689847864744, -105.6562500020483952 ) ) ;
#34570 = CARTESIAN_POINT ( 'NONE',  ( -5.405949406250003975, -9.363379034771801557, -111.3437500020483810 ) ) ;
#34571 = CARTESIAN_POINT ( 'NONE',  ( -9.999999999999742428, -5.773502691896402084, -161.6250000000000284 ) ) ;
#34572 = CARTESIAN_POINT ( 'NONE',  ( 10.81189881249999551, -6.242252689847874514, -112.6562500020483810 ) ) ;
#34573 = CARTESIAN_POINT ( 'NONE',  ( 10.81189881249999729, 0.000000000000000000, -5.843750002048370362 ) ) ;
#34574 = CARTESIAN_POINT ( 'NONE',  ( 5.405949406249992428, -9.363379034771808662, -127.5937500020483668 ) ) ;
#34575 = CIRCLE ( 'NONE', #16610, 20.00000000000000355 ) ;
#34576 = CARTESIAN_POINT ( 'NONE',  ( -5.405949406249996869, 9.363379034771805109, -191.5312500020484094 ) ) ;
#34577 = CARTESIAN_POINT ( 'NONE',  ( 10.00000000000000000, 5.773502691896255534, -165.7500000040967905 ) ) ;
#34578 = CARTESIAN_POINT ( 'NONE',  ( 9.999999999999998224, 0.000000000000000000, -147.5000000000000000 ) ) ;
#34579 = CARTESIAN_POINT ( 'NONE',  ( 9.999999999999998224, 0.000000000000000000, -9.499999999999953815 ) ) ;
#34580 = CC_DESIGN_SECURITY_CLASSIFICATION ( #18005, ( #36620 ) ) ;
#34581 = CARTESIAN_POINT ( 'NONE',  ( 10.81189881249999729, 6.242252689847867408, -74.71875000204838102 ) ) ;
#34582 = CARTESIAN_POINT ( 'NONE',  ( 5.405949406249999534, 9.363379034771803333, -56.59375000204835970 ) ) ;
#34583 = CARTESIAN_POINT ( 'NONE',  ( 4.999999999999992006, -8.660254037844389075, -116.6250000040967905 ) ) ;
#34584 = CARTESIAN_POINT ( 'NONE',  ( 5.405949406249999534, 9.363379034771803333, -34.28125000204837391 ) ) ;
#34585 = CARTESIAN_POINT ( 'NONE',  ( 10.81189881249999729, 0.000000000000000000, -41.84375000204837391 ) ) ;
#34586 = CARTESIAN_POINT ( 'NONE',  ( 7.070501591499376803E-16, 11.54700538379251284, -53.00000000409676915 ) ) ;
#34587 = CARTESIAN_POINT ( 'NONE',  ( -5.405949406250003975, -9.363379034771801557, -144.3437500020483810 ) ) ;
#34588 = CARTESIAN_POINT ( 'NONE',  ( 9.999999999999996447, -5.773502691896262640, -125.1249999999999858 ) ) ;
#34589 = CARTESIAN_POINT ( 'NONE',  ( 5.000000000000000000, 8.660254037844385522, -42.24999999999997868 ) ) ;
#34590 = CARTESIAN_POINT ( 'NONE',  ( 9.999999999999996447, -5.773502691896262640, -78.62499999999998579 ) ) ;
#34591 = CARTESIAN_POINT ( 'NONE',  ( 7.644554776091147741E-16, 12.48450537969573659, -7.156250002048365921 ) ) ;
#34592 = VERTEX_POINT ( 'NONE', #30914 ) ;
#34593 = CARTESIAN_POINT ( 'NONE',  ( 10.81189881249999729, 6.242252689847867408, -100.4062500020483952 ) ) ;
#34594 = CARTESIAN_POINT ( 'NONE',  ( 5.000000000000000000, 8.660254037844385522, -126.6250000040967620 ) ) ;
#34595 = CARTESIAN_POINT ( 'NONE',  ( -5.000000000000003553, -8.660254037844383745, -143.8750000040967905 ) ) ;
#34596 = CARTESIAN_POINT ( 'NONE',  ( 10.81189881249999551, -6.242252689847874514, -79.46875000204838102 ) ) ;
#34597 = AXIS2_PLACEMENT_3D ( 'NONE', #27436, #40999, #31111 ) ;
#34598 = CARTESIAN_POINT ( 'NONE',  ( -5.000000000000003553, -8.660254037844383745, -31.37500000409676559 ) ) ;
#34599 = CARTESIAN_POINT ( 'NONE',  ( 9.999999999999742428, 5.773502691896404748, -130.8749999999999716 ) ) ;
#34600 = CARTESIAN_POINT ( 'NONE',  ( -10.81189881249999729, 1.324075727343319199E-15, -47.28125000204838813 ) ) ;
#34601 = CARTESIAN_POINT ( 'NONE',  ( -9.999999999999479527, -5.773502691896549521, -100.1249999999999574 ) ) ;
#34602 = CARTESIAN_POINT ( 'NONE',  ( -2.293366432827344421E-15, -12.48450537969573659, -147.4062500020483810 ) ) ;
#34603 = CARTESIAN_POINT ( 'NONE',  ( -2.293366432827344421E-15, -12.48450537969573659, -129.2187500020483810 ) ) ;
#34605 = EDGE_CURVE ( 'NONE', #18513, #27003, #29938, .T. ) ;
#34604 = CARTESIAN_POINT ( 'NONE',  ( -10.00000000000051337, 5.773502691895962435, -151.3750000000000284 ) ) ;
#34606 = EDGE_CURVE ( 'NONE', #8915, #21961, #16411, .T. ) ;
#34607 = CARTESIAN_POINT ( 'NONE',  ( 9.999999999999998224, 0.000000000000000000, -173.3750000040968189 ) ) ;
#34608 = ORIENTED_EDGE ( 'NONE', *, *, #3429, .F. ) ;
#34609 = AXIS2_PLACEMENT_3D ( 'NONE', #29357, #26119, #12713 ) ;
#34610 =( BOUNDED_CURVE ( )  B_SPLINE_CURVE ( 2, ( #35265, #5699, #8503, #21655, #19057, #28147, #18194 ),
 .UNSPECIFIED., .F., .T. ) 
 B_SPLINE_CURVE_WITH_KNOTS ( ( 3, 2, 2, 3 ),
 ( 0.3582089552238806873, 0.3594527363184080726, 0.3606965174129355134, 0.3619402985074628432 ),
 .UNSPECIFIED. ) 
 CURVE ( )  GEOMETRIC_REPRESENTATION_ITEM ( )  RATIONAL_B_SPLINE_CURVE ( ( 0.9999999999999880096, 0.8660254037844506980, 1.000000000000000000, 0.8660254037844387076, 1.000000000000000000, 0.8660254037844207220, 1.000000000000017986 ) ) 
 REPRESENTATION_ITEM ( '' )  );
#34611 = EDGE_LOOP ( 'NONE', ( #19987, #11271, #12339, #22740 ) ) ;
#34612 = ORIENTED_EDGE ( 'NONE', *, *, #10841, .F. ) ;
#34613 = CARTESIAN_POINT ( 'NONE',  ( -4.999999999999996447, 8.660254037844387298, -129.3750000040967905 ) ) ;
#34614 = CARTESIAN_POINT ( 'NONE',  ( 7.644554776091147741E-16, 12.48450537969573659, -183.9687500020484094 ) ) ;
#34615 = CARTESIAN_POINT ( 'NONE',  ( 10.81189881249999551, -6.242252689847874514, -35.96875000204835260 ) ) ;
#34616 = CARTESIAN_POINT ( 'NONE',  ( -10.00000000000025580, 5.773502691896109873, -118.3750000000000142 ) ) ;
#34617 = CARTESIAN_POINT ( 'NONE',  ( 7.644554776091147741E-16, 12.48450537969573659, -168.9687500020483810 ) ) ;
#34618 = CARTESIAN_POINT ( 'NONE',  ( 5.405949406249992428, -9.363379034771808662, -153.0937500020483810 ) ) ;
#34619 = CARTESIAN_POINT ( 'NONE',  ( 5.405949406249999534, 9.363379034771803333, -136.0937500020483810 ) ) ;
#34620 = CARTESIAN_POINT ( 'NONE',  ( -5.405949406249996869, 9.363379034771805109, -146.5312500020483810 ) ) ;
#34621 = CARTESIAN_POINT ( 'NONE',  ( 5.405949406249999534, 9.363379034771803333, -154.0937500020483810 ) ) ;
#34622 = CARTESIAN_POINT ( 'NONE',  ( -9.999999999999998224, 1.224646799147353059E-15, -40.62500000409677625 ) ) ;
#34623 = DIRECTION ( 'NONE',  ( 1.000000000000000000, 0.000000000000000000, 0.000000000000000000 ) ) ;
#34624 = CARTESIAN_POINT ( 'NONE',  ( 4.999999999999992006, -8.660254037844389075, -170.2500000000000000 ) ) ;
#34625 = CARTESIAN_POINT ( 'NONE',  ( 10.81189881249999551, -6.242252689847874514, -79.46875000204838102 ) ) ;
#34626 = CARTESIAN_POINT ( 'NONE',  ( -9.999999999999998224, 0.000000000000000000, -99.99999999999998579 ) ) ;
#34627 = CARTESIAN_POINT ( 'NONE',  ( -5.405949406250003975, -9.363379034771801557, -59.03125000204836681 ) ) ;
#34628 = CARTESIAN_POINT ( 'NONE',  ( -9.281563073697167709, 5.229554528500406363, -100.0000000000000000 ) ) ;
#34629 = CARTESIAN_POINT ( 'NONE',  ( -10.81189881249999729, 6.242252689847871849, -176.2187500020483810 ) ) ;
#34630 = CARTESIAN_POINT ( 'NONE',  ( -5.405949406250003975, -9.363379034771801557, -113.0312500020483952 ) ) ;
#34631 = CARTESIAN_POINT ( 'NONE',  ( 5.405949406249992428, -9.363379034771808662, -154.7812500020484094 ) ) ;
#34632 = FACE_BOUND ( 'NONE', #35194, .T. ) ;
#34633 = CARTESIAN_POINT ( 'NONE',  ( 7.644554776091147741E-16, 12.48450537969573659, -43.15625000204837391 ) ) ;
#34634 = CARTESIAN_POINT ( 'NONE',  ( -9.999999999999998224, 1.224646799147353059E-15, -126.1250000040967620 ) ) ;
#34635 = CARTESIAN_POINT ( 'NONE',  ( -2.121150477449813534E-15, -11.54700538379251284, -96.87500000000000000 ) ) ;
#34636 = VECTOR ( 'NONE', #18671, 1000.000000000000114 ) ;
#34637 = VERTEX_POINT ( 'NONE', #2211 ) ;
#34638 = CARTESIAN_POINT ( 'NONE',  ( 10.81189881249999729, 0.000000000000000000, -129.0312500020484094 ) ) ;
#34639 = CARTESIAN_POINT ( 'NONE',  ( -5.000000000000003553, -8.660254037844383745, -151.3750000040967905 ) ) ;
#34640 = CARTESIAN_POINT ( 'NONE',  ( 9.999999999999994671, -5.773502691896262640, -167.1250000000000000 ) ) ;
#34641 = CARTESIAN_POINT ( 'NONE',  ( 5.405949406249992428, -9.363379034771808662, -183.2812500020484094 ) ) ;
#34642 = ORIENTED_EDGE ( 'NONE', *, *, #30488, .T. ) ;
#34643 = CARTESIAN_POINT ( 'NONE',  ( 7.644554776091147741E-16, 12.48450537969573659, -171.9687500020483810 ) ) ;
#34644 = CARTESIAN_POINT ( 'NONE',  ( 9.999999999999998224, 0.000000000000000000, -59.37500000409676204 ) ) ;
#34645 = CARTESIAN_POINT ( 'NONE',  ( -9.999999999999998224, 1.224646799147353059E-15, -187.2500000000000000 ) ) ;
#34646 = CARTESIAN_POINT ( 'NONE',  ( 9.999999999999998224, 0.000000000000000000, -117.5000000000000000 ) ) ;
#34647 = CARTESIAN_POINT ( 'NONE',  ( 10.81189881249999551, -6.242252689847874514, -66.15625000204839523 ) ) ;
#34648 = CARTESIAN_POINT ( 'NONE',  ( 5.000000000000000000, 8.660254037844385522, -41.12500000409677625 ) ) ;
#34649 = CARTESIAN_POINT ( 'NONE',  ( -10.81189881249999729, 1.324075727343319199E-15, -2.093750002048366810 ) ) ;
#34650 = CARTESIAN_POINT ( 'NONE',  ( 4.999999999999992006, -8.660254037844389075, -148.1250000040967905 ) ) ;
#34651 = CARTESIAN_POINT ( 'NONE',  ( -10.81189881249999907, -6.242252689847864744, -174.6562500020483810 ) ) ;
#34652 = AXIS2_PLACEMENT_3D ( 'NONE', #19183, #22643, #5397 ) ;
#34653 = CARTESIAN_POINT ( 'NONE',  ( 5.000000000000000000, 8.660254037844385522, -2.125000004096766482 ) ) ;
#34654 = EDGE_CURVE ( 'NONE', #33286, #2320, #16450, .T. ) ;
#34655 = ORIENTED_EDGE ( 'NONE', *, *, #21492, .T. ) ;
#34656 = DIRECTION ( 'NONE',  ( -1.000000000000000000, 0.000000000000000000, 0.000000000000000000 ) ) ;
#34657 = EDGE_CURVE ( 'NONE', #8341, #17742, #10874, .T. ) ;
#34658 = EDGE_CURVE ( 'NONE', #13418, #7848, #34348, .T. ) ;
#34659 = CARTESIAN_POINT ( 'NONE',  ( -9.999999999999998224, 1.224646799147353059E-15, -61.24999999999997158 ) ) ;
#34660 = EDGE_CURVE ( 'NONE', #39053, #30365, #5102, .T. ) ;
#34661 = DIRECTION ( 'NONE',  ( -1.000000000000000000, 0.000000000000000000, 0.000000000000000000 ) ) ;
#34663 = ORIENTED_EDGE ( 'NONE', *, *, #34676, .T. ) ;
#34662 = CARTESIAN_POINT ( 'NONE',  ( -2.293366432827344421E-15, -12.48450537969573659, -81.40625000204838102 ) ) ;
#34664 =( NAMED_UNIT ( * ) PLANE_ANGLE_UNIT ( ) SI_UNIT ( $, .RADIAN. ) );
#34666 = EDGE_LOOP ( 'NONE', ( #40103, #11973, #19958, #20147 ) ) ;
#34665 = CARTESIAN_POINT ( 'NONE',  ( -1.040834085586084257E-14, 125.0000000000000000, 12.74999999999998934 ) ) ;
#34667 = CC_DESIGN_PERSON_AND_ORGANIZATION_ASSIGNMENT ( #5417, #21596, ( #36593 ) ) ;
#34668 = ORIENTED_EDGE ( 'NONE', *, *, #19927, .F. ) ;
#34669 = CARTESIAN_POINT ( 'NONE',  ( -5.405949406249996869, 9.363379034771805109, -36.84375000204836681 ) ) ;
#34670 = CARTESIAN_POINT ( 'NONE',  ( 5.000000000000000000, 8.660254037844385522, -77.12500000409677625 ) ) ;
#34671 = CARTESIAN_POINT ( 'NONE',  ( -2.293366432827344421E-15, -12.48450537969573659, -10.90625000204838457 ) ) ;
#34673 = ORIENTED_EDGE ( 'NONE', *, *, #38372, .T. ) ;
#34672 = CARTESIAN_POINT ( 'NONE',  ( 5.405949406249999534, 9.363379034771803333, -59.59375000204835970 ) ) ;
#34674 = CARTESIAN_POINT ( 'NONE',  ( -9.999999999999998224, 1.224646799147353059E-15, -148.2500000000000000 ) ) ;
#34675 = CARTESIAN_POINT ( 'NONE',  ( 4.999999999999992006, -8.660254037844389075, -38.24999999999997868 ) ) ;
#34676 = EDGE_CURVE ( 'NONE', #38192, #28563, #4594, .T. ) ;
#34677 = CARTESIAN_POINT ( 'NONE',  ( -5.405949406250003975, -9.363379034771801557, -192.3437500020484094 ) ) ;
#34678 = CARTESIAN_POINT ( 'NONE',  ( 7.644554776091147741E-16, 12.48450537969573659, -173.4687500020483810 ) ) ;
#34679 = CARTESIAN_POINT ( 'NONE',  ( -10.81189881249999907, -6.242252689847864744, -165.4687500020484094 ) ) ;
#34680 = DIRECTION ( 'NONE',  ( -0.000000000000000000, -0.000000000000000000, 1.000000000000000000 ) ) ;
#34681 = CARTESIAN_POINT ( 'NONE',  ( -4.999999999999996447, 8.660254037844387298, -58.87500000409676204 ) ) ;
#34682 = CARTESIAN_POINT ( 'NONE',  ( 0.000000000000000000, 0.000000000000000000, -99.99999999999998579 ) ) ;
#34683 = EDGE_CURVE ( 'NONE', #3609, #33095, #38752, .T. ) ;
#34684 = CARTESIAN_POINT ( 'NONE',  ( -4.999999999999996447, 8.660254037844387298, -195.0000000000000000 ) ) ;
#34685 = CARTESIAN_POINT ( 'NONE',  ( -10.81189881249999729, 1.324075727343319199E-15, -114.5937500020483810 ) ) ;
#34686 = DIRECTION ( 'NONE',  ( 1.000000000000000000, 0.000000000000000000, 0.000000000000000000 ) ) ;
#34687 = CARTESIAN_POINT ( 'NONE',  ( 10.81189881249999551, -6.242252689847874514, -81.15625000204839523 ) ) ;
#34688 = CARTESIAN_POINT ( 'NONE',  ( -10.81189881249999729, 1.324075727343319199E-15, -92.09375000204838102 ) ) ;
#34689 = CARTESIAN_POINT ( 'NONE',  ( 10.81189881249999551, -6.242252689847874514, -58.46875000204837391 ) ) ;
#34690 = CARTESIAN_POINT ( 'NONE',  ( -5.405949406250003975, -9.363379034771801557, -71.03125000204838102 ) ) ;
#34691 = CARTESIAN_POINT ( 'NONE',  ( -5.000000000000003553, -8.660254037844383745, -154.3750000040967905 ) ) ;
#34692 = CARTESIAN_POINT ( 'NONE',  ( 10.00000000000000000, 5.773502691896255534, -120.3749999999999858 ) ) ;
#34693 = CARTESIAN_POINT ( 'NONE',  ( -10.81189881249999729, 6.242252689847871849, -149.4062500020484094 ) ) ;
#34694 = CARTESIAN_POINT ( 'NONE',  ( -2.293366432827344421E-15, -12.48450537969573659, -162.4062500020483810 ) ) ;
#34695 = LINE ( 'NONE', #28215, #8234 ) ;
#34696 = CARTESIAN_POINT ( 'NONE',  ( 10.00000000000044764, -5.773502691896004180, -182.1250000000000000 ) ) ;
#34697 = CARTESIAN_POINT ( 'NONE',  ( -2.293366432827344421E-15, -12.48450537969573659, -100.7187500020483952 ) ) ;
#34698 = VERTEX_POINT ( 'NONE', #31566 ) ;
#34699 = CARTESIAN_POINT ( 'NONE',  ( -9.999999999999998224, 1.224646799147353059E-15, -62.74999999999997158 ) ) ;
#34700 = CARTESIAN_POINT ( 'NONE',  ( -10.81189881249999729, 1.324075727343319199E-15, -198.5937500020484094 ) ) ;
#34701 = CARTESIAN_POINT ( 'NONE',  ( -5.000000000000003553, -8.660254037844383745, -83.87500000409677625 ) ) ;
#34702 = ADVANCED_FACE ( 'NONE', ( #38027 ), #14699, .F. ) ;
#34703 = CARTESIAN_POINT ( 'NONE',  ( 10.00000000000051159, -5.773502691895965988, -142.0000000040967905 ) ) ;
#34704 = CARTESIAN_POINT ( 'NONE',  ( 5.405949406249999534, 9.363379034771803333, -91.28125000204838102 ) ) ;
#34705 = CARTESIAN_POINT ( 'NONE',  ( 10.81189881249999729, 0.000000000000000000, -72.03125000204838102 ) ) ;
#34706 = CARTESIAN_POINT ( 'NONE',  ( -10.00000000000000000, -5.773502691896251982, -67.50000000409679046 ) ) ;
#34707 = CARTESIAN_POINT ( 'NONE',  ( 4.999999999999992006, -8.660254037844389075, -77.62500000409677625 ) ) ;
#34708 = CARTESIAN_POINT ( 'NONE',  ( 10.81189881249999729, 0.000000000000000000, -25.34375000204835970 ) ) ;
#34709 = ORIENTED_EDGE ( 'NONE', *, *, #23326, .T. ) ;
#34710 = CARTESIAN_POINT ( 'NONE',  ( -5.405949406250003975, -9.363379034771801557, -198.5312500020484094 ) ) ;
#34711 = CARTESIAN_POINT ( 'NONE',  ( 10.81189881249999551, -6.242252689847874514, -24.15625000204837747 ) ) ;
#34712 = CARTESIAN_POINT ( 'NONE',  ( 10.81189881249999551, -6.242252689847874514, -10.46875000204836503 ) ) ;
#34713 = CARTESIAN_POINT ( 'NONE',  ( 5.405949406249992428, -9.363379034771808662, -145.5937500020483810 ) ) ;
#34714 = DIRECTION ( 'NONE',  ( -1.000000000000000000, 0.000000000000000000, 0.000000000000000000 ) ) ;
#34715 = CARTESIAN_POINT ( 'NONE',  ( 9.999999999998969713, 5.773502691896851502, -57.75000000409676915 ) ) ;
#34716 = CARTESIAN_POINT ( 'NONE',  ( 7.644554776091147741E-16, 12.48450537969573659, -128.6562500020483810 ) ) ;
#34717 = CARTESIAN_POINT ( 'NONE',  ( 9.999999999999998224, 0.000000000000000000, -186.5000000000000000 ) ) ;
#34718 = DIRECTION ( 'NONE',  ( -0.000000000000000000, -0.000000000000000000, 1.000000000000000000 ) ) ;
#34720 = ORIENTED_EDGE ( 'NONE', *, *, #7041, .T. ) ;
#34719 = CARTESIAN_POINT ( 'NONE',  ( 10.81189881249999551, -6.242252689847874514, -109.6562500020483810 ) ) ;
#34721 = LINE ( 'NONE', #11811, #11753 ) ;
#34722 = ORIENTED_EDGE ( 'NONE', *, *, #16959, .T. ) ;
#34723 = ORIENTED_EDGE ( 'NONE', *, *, #40550, .T. ) ;
#34724 = CARTESIAN_POINT ( 'NONE',  ( -10.81189881249999729, 1.324075727343319199E-15, -35.28125000204837391 ) ) ;
#34725 = SHAPE_DEFINITION_REPRESENTATION ( #8050, #40929 ) ;
#34726 = ADVANCED_FACE ( 'NONE', ( #11465 ), #17937, .T. ) ;
#34727 = CARTESIAN_POINT ( 'NONE',  ( 7.644554776091147741E-16, 12.48450537969573659, -90.96875000204838102 ) ) ;
#34728 = CARTESIAN_POINT ( 'NONE',  ( 0.000000000000000000, 0.000000000000000000, -200.0000000000000000 ) ) ;
#34729 = CARTESIAN_POINT ( 'NONE',  ( 5.000000000000000000, 8.660254037844385522, -174.2500000000000284 ) ) ;
#34730 =( BOUNDED_CURVE ( )  B_SPLINE_CURVE ( 2, ( #3018, #16141, #22437, #18773, #42272, #25688, #35406 ),
 .UNSPECIFIED., .F., .F. ) 
 B_SPLINE_CURVE_WITH_KNOTS ( ( 3, 2, 2, 3 ),
 ( 0.2350746268656717097, 0.2363184079601990950, 0.2375621890547264525, 0.2388059701492538378 ),
 .UNSPECIFIED. ) 
 CURVE ( )  GEOMETRIC_REPRESENTATION_ITEM ( )  RATIONAL_B_SPLINE_CURVE ( ( 0.9999999999999940048, 0.8660254037844447028, 1.000000000000000000, 0.8660254037844387076, 1.000000000000000000, 0.8660254037844267172, 1.000000000000011990 ) ) 
 REPRESENTATION_ITEM ( '' )  );
#34731 = CARTESIAN_POINT ( 'NONE',  ( 9.999999999999998224, 0.000000000000000000, -170.3750000040968189 ) ) ;
#34732 = CARTESIAN_POINT ( 'NONE',  ( 10.81189881249999907, 6.242252689847868297, -166.4062500020483810 ) ) ;
#34733 = CARTESIAN_POINT ( 'NONE',  ( 4.999999999999992006, -8.660254037844389075, -77.24999999999998579 ) ) ;
#34734 = CARTESIAN_POINT ( 'NONE',  ( 10.81189881249999551, -6.242252689847874514, -116.9687500020483810 ) ) ;
#34735 = CARTESIAN_POINT ( 'NONE',  ( 10.81189881249999907, 6.242252689847868297, -86.71875000204836681 ) ) ;
#34736 = FACE_OUTER_BOUND ( 'NONE', #626, .T. ) ;
#34737 = CARTESIAN_POINT ( 'NONE',  ( 10.81189881249999551, -6.242252689847874514, -190.4687500020484094 ) ) ;
#34738 = CARTESIAN_POINT ( 'NONE',  ( -10.81189881249999907, -6.242252689847864744, -95.15625000204839523 ) ) ;
#34739 = CARTESIAN_POINT ( 'NONE',  ( -4.999999999999996447, 8.660254037844387298, -181.8750000040967905 ) ) ;
#34740 = CARTESIAN_POINT ( 'NONE',  ( -5.405949406249996869, 9.363379034771805109, -172.0312500020484094 ) ) ;
#34741 =( BOUNDED_CURVE ( )  B_SPLINE_CURVE ( 2, ( #7429, #39585, #13666, #7217, #29894, #3774, #26648 ),
 .UNSPECIFIED., .F., .F. ) 
 B_SPLINE_CURVE_WITH_KNOTS ( ( 3, 2, 2, 3 ),
 ( 0.8208955223880598506, 0.8221393034825871249, 0.8233830845771146212, 0.8246268656716420065 ),
 .UNSPECIFIED. ) 
 CURVE ( )  GEOMETRIC_REPRESENTATION_ITEM ( )  RATIONAL_B_SPLINE_CURVE ( ( 0.9999999999999880096, 0.8660254037844506980, 1.000000000000000000, 0.8660254037844387076, 1.000000000000000000, 0.8660254037844148378, 1.000000000000023981 ) ) 
 REPRESENTATION_ITEM ( '' )  );
#34742 = CARTESIAN_POINT ( 'NONE',  ( -2.121150477449813534E-15, -11.54700538379251284, -70.25000000409679046 ) ) ;
#34743 = CARTESIAN_POINT ( 'NONE',  ( 10.81189881249999551, -6.242252689847874514, -177.1562500020484094 ) ) ;
#34744 = CARTESIAN_POINT ( 'NONE',  ( -5.405949406249996869, 9.363379034771805109, -190.0312500020484094 ) ) ;
#34745 = CARTESIAN_POINT ( 'NONE',  ( -10.81189881249999729, -6.242252689847864744, -55.96875000204836681 ) ) ;
#34746 = CARTESIAN_POINT ( 'NONE',  ( 10.00000000000000000, 5.773502691896255534, -167.2500000040968189 ) ) ;
#34747 = CARTESIAN_POINT ( 'NONE',  ( 7.644554776091147741E-16, 12.48450537969573659, 0.3437499979516377424 ) ) ;
#34748 = CARTESIAN_POINT ( 'NONE',  ( -10.81189881249999907, -6.242252689847864744, -15.46875000204836503 ) ) ;
#34749 = CYLINDRICAL_SURFACE ( 'NONE', #17128, 9.999999999999998224 ) ;
#34750 = CARTESIAN_POINT ( 'NONE',  ( 10.81189881249999729, 0.000000000000000000, -121.3437500020483952 ) ) ;
#34751 = CARTESIAN_POINT ( 'NONE',  ( -9.999999999999998224, 1.224646799147353059E-15, -100.2499999999999858 ) ) ;
#34752 = CARTESIAN_POINT ( 'NONE',  ( 5.405949406249992428, -9.363379034771808662, -18.28125000204835970 ) ) ;
#34753 = CARTESIAN_POINT ( 'NONE',  ( -2.121150477449813534E-15, -11.54700538379251284, -106.2500000040967763 ) ) ;
#34754 = CARTESIAN_POINT ( 'NONE',  ( 5.000000000000000000, 8.660254037844385522, -82.74999999999997158 ) ) ;
#34755 = CARTESIAN_POINT ( 'NONE',  ( 7.070501591499377789E-16, 11.54700538379251284, -49.62499999999997158 ) ) ;
#34756 = CARTESIAN_POINT ( 'NONE',  ( -2.293366432827344421E-15, -12.48450537969573659, -118.9062500020483952 ) ) ;
#34757 = CARTESIAN_POINT ( 'NONE',  ( 10.81189881249999551, -6.242252689847874514, -99.15625000204839523 ) ) ;
#34758 = VERTEX_POINT ( 'NONE', #41239 ) ;
#34759 = CARTESIAN_POINT ( 'NONE',  ( -10.00000000000000000, -5.773502691896251982, -96.00000000409679046 ) ) ;
#34760 = CARTESIAN_POINT ( 'NONE',  ( 5.405949406249999534, 9.363379034771803333, -157.2812500020484094 ) ) ;
#34761 = CARTESIAN_POINT ( 'NONE',  ( 7.644554776091147741E-16, 12.48450537969573659, -53.46875000204836681 ) ) ;
#34762 = ORIENTED_EDGE ( 'NONE', *, *, #34409, .T. ) ;
#34763 = CARTESIAN_POINT ( 'NONE',  ( -5.000000000000003553, -8.660254037844383745, -24.99999999999996803 ) ) ;
#34764 = APPLICATION_CONTEXT ( 'configuration controlled 3d designs of mechanical parts and assemblies' ) ;
#34765 = CARTESIAN_POINT ( 'NONE',  ( 10.81189881249999729, 6.242252689847867408, -26.90625000204837391 ) ) ;
#34766 = CARTESIAN_POINT ( 'NONE',  ( 7.070501591499377789E-16, 11.54700538379251284, -160.6250000000000284 ) ) ;
#34767 = CARTESIAN_POINT ( 'NONE',  ( -9.999999999999998224, 1.224646799147353059E-15, -190.6250000040967905 ) ) ;
#34768 = CARTESIAN_POINT ( 'NONE',  ( 7.070501591499377789E-16, 11.54700538379251284, -20.00000000409676559 ) ) ;
#34769 = CYLINDRICAL_SURFACE ( 'NONE', #41489, 10.00000000000000178 ) ;
#34770 = CARTESIAN_POINT ( 'NONE',  ( 10.81189881249999729, 0.000000000000000000, -136.5312500020484094 ) ) ;
#34771 = CARTESIAN_POINT ( 'NONE',  ( 5.000000000000000000, 8.660254037844385522, -75.62500000409677625 ) ) ;
#34772 = LINE ( 'NONE', #1966, #34878 ) ;
#34773 = ORIENTED_EDGE ( 'NONE', *, *, #21970, .F. ) ;
#34774 = CARTESIAN_POINT ( 'NONE',  ( 10.81189881249999729, 0.000000000000000000, -58.53125000204836681 ) ) ;
#34775 = DATE_AND_TIME ( #28514, #34552 ) ;
#34776 = ADVANCED_FACE ( 'NONE', ( #27888 ), #41021, .T. ) ;
#34778 = ORIENTED_EDGE ( 'NONE', *, *, #15100, .T. ) ;
#34777 = ORIENTED_EDGE ( 'NONE', *, *, #27718, .F. ) ;
#34779 = DIRECTION ( 'NONE',  ( -1.000000000000000000, 0.000000000000000000, 0.000000000000000000 ) ) ;
#34780 = CARTESIAN_POINT ( 'NONE',  ( 9.999999999999998224, 0.000000000000000000, -25.99999999999996803 ) ) ;
#34781 = CARTESIAN_POINT ( 'NONE',  ( -10.81189881249999729, 6.242252689847871849, -155.2187500020483810 ) ) ;
#34782 = CARTESIAN_POINT ( 'NONE',  ( -10.81189881249999729, 1.324075727343319199E-15, -188.2812500020484094 ) ) ;
#34783 = CARTESIAN_POINT ( 'NONE',  ( 10.81189881249999907, 6.242252689847868297, -5.718750002048342829 ) ) ;
#34784 = CARTESIAN_POINT ( 'NONE',  ( 5.405949406249999534, 9.363379034771803333, -139.0937500020483810 ) ) ;
#34785 = CARTESIAN_POINT ( 'NONE',  ( 7.644554776091147741E-16, 12.48450537969573659, -97.15625000204839523 ) ) ;
#34786 = CARTESIAN_POINT ( 'NONE',  ( 10.81189881249999907, 6.242252689847868297, -110.7187500020483810 ) ) ;
#34787 = FACE_OUTER_BOUND ( 'NONE', #8174, .T. ) ;
#34788 = CARTESIAN_POINT ( 'NONE',  ( -2.293366432827344421E-15, -12.48450537969573659, -115.9062500020483810 ) ) ;
#34789 = CARTESIAN_POINT ( 'NONE',  ( -5.405949406250003975, -9.363379034771801557, -6.343750002048370362 ) ) ;
#34791 = EDGE_CURVE ( 'NONE', #24289, #15832, #13389, .T. ) ;
#34790 = CARTESIAN_POINT ( 'NONE',  ( -10.81189881249999729, 1.324075727343319199E-15, -119.0937500020483810 ) ) ;
#34792 = CARTESIAN_POINT ( 'NONE',  ( 10.81189881249999729, 0.000000000000000000, -198.0312500020484094 ) ) ;
#34793 = CARTESIAN_POINT ( 'NONE',  ( 5.000000000000000000, 8.660254037844385522, -12.24999999999995559 ) ) ;
#34794 = CARTESIAN_POINT ( 'NONE',  ( 9.999999999999996447, -5.773502691896262640, -144.6250000000000000 ) ) ;
#34795 = CARTESIAN_POINT ( 'NONE',  ( 9.999999999999998224, 0.000000000000000000, -12.49999999999995559 ) ) ;
#34796 = CARTESIAN_POINT ( 'NONE',  ( -5.405949406250003975, -9.363379034771801557, -76.84375000204838102 ) ) ;
#34797 = CARTESIAN_POINT ( 'NONE',  ( 5.405949406249992428, -9.363379034771808662, -57.09375000204835970 ) ) ;
#34798 = CARTESIAN_POINT ( 'NONE',  ( 9.999999999999996447, -5.773502691896262640, -190.0000000040968189 ) ) ;
#34799 = CARTESIAN_POINT ( 'NONE',  ( -10.81189881249999729, 1.324075727343319199E-15, -30.78125000204837036 ) ) ;
#34800 = CARTESIAN_POINT ( 'NONE',  ( -5.405949406250003975, -9.363379034771801557, -40.84375000204837391 ) ) ;
#34801 = CARTESIAN_POINT ( 'NONE',  ( -4.999999999999996447, 8.660254037844387298, -136.5000000000000000 ) ) ;
#34802 = CARTESIAN_POINT ( 'NONE',  ( 10.81189881249999551, -6.242252689847874514, -143.9687500020483810 ) ) ;
#34803 = CARTESIAN_POINT ( 'NONE',  ( 10.00000000000000000, 5.773502691896255534, -120.3749999999999858 ) ) ;
#34804 = CARTESIAN_POINT ( 'NONE',  ( 9.999999999999998224, 0.000000000000000000, -144.8750000040967905 ) ) ;
#34805 = CARTESIAN_POINT ( 'NONE',  ( -5.000000000000003553, -8.660254037844383745, -74.49999999999998579 ) ) ;
#34806 = CARTESIAN_POINT ( 'NONE',  ( 5.405949406249999534, 9.363379034771803333, -140.7812500020483810 ) ) ;
#34807 = CARTESIAN_POINT ( 'NONE',  ( -5.405949406249996869, 9.363379034771805109, -7.031250002048378356 ) ) ;
#34808 = ORIENTED_EDGE ( 'NONE', *, *, #13142, .F. ) ;
#34809 = CARTESIAN_POINT ( 'NONE',  ( -10.81189881249999729, 6.242252689847871849, -101.4062500020483952 ) ) ;
#34810 = CARTESIAN_POINT ( 'NONE',  ( -2.121150477449813534E-15, -11.54700538379251284, -113.7500000040967905 ) ) ;
#34811 = CARTESIAN_POINT ( 'NONE',  ( 9.999999999999998224, 0.000000000000000000, -99.49999999999998579 ) ) ;
#34812 = CARTESIAN_POINT ( 'NONE',  ( -10.81189881249999729, 1.324075727343319199E-15, -72.59375000204838102 ) ) ;
#34813 = CARTESIAN_POINT ( 'NONE',  ( -5.000000000000003553, -8.660254037844383745, -23.87500000409675849 ) ) ;
#34814 = CARTESIAN_POINT ( 'NONE',  ( 7.070501591499376803E-16, 11.54700538379251284, -148.6250000000000000 ) ) ;
#34815 = CARTESIAN_POINT ( 'NONE',  ( -5.405949406249996869, 9.363379034771805109, -44.53125000204838102 ) ) ;
#34816 = CARTESIAN_POINT ( 'NONE',  ( 4.999999999999992006, -8.660254037844389075, -105.7499999999999858 ) ) ;
#34817 = CARTESIAN_POINT ( 'NONE',  ( -2.293366432827344421E-15, -12.48450537969573659, -148.9062500020483810 ) ) ;
#34818 = EDGE_CURVE ( 'NONE', #25640, #23180, #450, .T. ) ;
#34819 = CARTESIAN_POINT ( 'NONE',  ( 5.405949406249999534, 9.363379034771803333, -127.0937500020483668 ) ) ;
#34820 = CARTESIAN_POINT ( 'NONE',  ( 9.999999999999998224, 0.000000000000000000, -200.0000000000000000 ) ) ;
#34821 =( BOUNDED_CURVE ( )  B_SPLINE_CURVE ( 2, ( #40418, #37636, #10862, #7643, #24053, #20794, #8075 ),
 .UNSPECIFIED., .F., .F. ) 
 B_SPLINE_CURVE_WITH_KNOTS ( ( 3, 2, 2, 3 ),
 ( 0.6567164179104479915, 0.6579601990049753768, 0.6592039800995028731, 0.6604477611940301474 ),
 .UNSPECIFIED. ) 
 CURVE ( )  GEOMETRIC_REPRESENTATION_ITEM ( )  RATIONAL_B_SPLINE_CURVE ( ( 0.9999999999999761302, 0.8660254037844625774, 1.000000000000000000, 0.8660254037844387076, 1.000000000000000000, 0.8660254037844028474, 1.000000000000035971 ) ) 
 REPRESENTATION_ITEM ( '' )  );
#34822 = CARTESIAN_POINT ( 'NONE',  ( 9.999999999999866773, -5.773502691896336358, -173.5000000040967905 ) ) ;
#34823 = VERTEX_POINT ( 'NONE', #22903 ) ;
#34824 = EDGE_CURVE ( 'NONE', #39040, #23886, #4844, .T. ) ;
#34825 = ORIENTED_EDGE ( 'NONE', *, *, #31024, .F. ) ;
#34826 = ORIENTED_EDGE ( 'NONE', *, *, #22769, .T. ) ;
#34827 = CARTESIAN_POINT ( 'NONE',  ( 10.81189881249999907, 6.242252689847868297, -185.7187500020483810 ) ) ;
#34828 = CARTESIAN_POINT ( 'NONE',  ( 5.405949406249999534, 9.363379034771803333, -34.09375000204836681 ) ) ;
#34829 = CARTESIAN_POINT ( 'NONE',  ( -9.999999999999998224, 1.224646799147353059E-15, -41.74999999999997868 ) ) ;
#34830 = CARTESIAN_POINT ( 'NONE',  ( -5.405949406249996869, 9.363379034771805109, -174.8437500020484094 ) ) ;
#34831 = CARTESIAN_POINT ( 'NONE',  ( 7.644554776091147741E-16, 12.48450537969573659, -150.9687500020483810 ) ) ;
#34832 = LINE ( 'NONE', #11284, #23825 ) ;
#34833 = CARTESIAN_POINT ( 'NONE',  ( 10.81189881249999729, 0.000000000000000000, -134.8437500020484094 ) ) ;
#34834 = AXIS2_PLACEMENT_3D ( 'NONE', #2262, #15383, #5703 ) ;
#34835 = CARTESIAN_POINT ( 'NONE',  ( 10.81189881249999907, 6.242252689847868297, -143.9062500020484094 ) ) ;
#34836 = CARTESIAN_POINT ( 'NONE',  ( -10.81189881249999729, -6.242252689847864744, -151.9687500020484094 ) ) ;
#34837 = CARTESIAN_POINT ( 'NONE',  ( -10.00000000000076916, 5.773502691895813221, -128.8749999999999716 ) ) ;
#34838 = CARTESIAN_POINT ( 'NONE',  ( 9.999999999999998224, 0.000000000000000000, -173.0000000000000284 ) ) ;
#34839 = CARTESIAN_POINT ( 'NONE',  ( -2.293366432827344421E-15, -12.48450537969573659, -81.21875000204838102 ) ) ;
#34840 = CARTESIAN_POINT ( 'NONE',  ( 10.00000000000102318, -5.773502691895667560, -82.00000000409670520 ) ) ;
#34841 = CARTESIAN_POINT ( 'NONE',  ( -10.81189881249999729, 6.242252689847871849, -59.40625000204838813 ) ) ;
#34842 = CARTESIAN_POINT ( 'NONE',  ( -7.718883402056913923, -6.624744321260780389, -100.0000000000000284 ) ) ;
#34843 = EDGE_CURVE ( 'NONE', #31374, #530, #35735, .T. ) ;
#34844 = CARTESIAN_POINT ( 'NONE',  ( -5.405949406249996869, 9.363379034771805109, -173.3437500020484094 ) ) ;
#34845 = CARTESIAN_POINT ( 'NONE',  ( 10.81189881249999551, -6.242252689847874514, -115.6562500020483810 ) ) ;
#34846 = CARTESIAN_POINT ( 'NONE',  ( 5.405949406249992428, -9.363379034771808662, -145.7812500020483810 ) ) ;
#34847 = DIRECTION ( 'NONE',  ( -0.000000000000000000, -0.000000000000000000, -1.000000000000000000 ) ) ;
#34848 = CARTESIAN_POINT ( 'NONE',  ( -2.293366432827344421E-15, -12.48450537969573659, -46.90625000204837391 ) ) ;
#34849 = CARTESIAN_POINT ( 'NONE',  ( -2.121150477449813534E-15, -11.54700538379251284, -125.7500000040967763 ) ) ;
#34850 = CARTESIAN_POINT ( 'NONE',  ( 7.070501591499377789E-16, 11.54700538379251284, -96.12500000000000000 ) ) ;
#34851 = ORIENTED_EDGE ( 'NONE', *, *, #6433, .F. ) ;
#34852 = VECTOR ( 'NONE', #22055, 1000.000000000000000 ) ;
#34853 = CARTESIAN_POINT ( 'NONE',  ( -5.405949406249996869, 9.363379034771805109, -127.0312500020483952 ) ) ;
#34854 = CARTESIAN_POINT ( 'NONE',  ( -2.121150477449813534E-15, -11.54700538379251284, -146.7500000040968189 ) ) ;
#34855 = CARTESIAN_POINT ( 'NONE',  ( 0.000000000000000000, 0.000000000000000000, -200.0000000000000000 ) ) ;
#34856 = CARTESIAN_POINT ( 'NONE',  ( 10.81189881249999729, 0.000000000000000000, -184.5312500020484094 ) ) ;
#34857 = VERTEX_POINT ( 'NONE', #32413 ) ;
#34858 = CARTESIAN_POINT ( 'NONE',  ( -10.81189881249999907, -6.242252689847864744, -171.4687500020484094 ) ) ;
#34859 = CARTESIAN_POINT ( 'NONE',  ( -2.121150477449813534E-15, -11.54700538379251284, -56.75000000409676915 ) ) ;
#34860 = DIRECTION ( 'NONE',  ( 0.000000000000000000, 1.000000000000000000, 0.000000000000000000 ) ) ;
#34861 = CYLINDRICAL_SURFACE ( 'NONE', #15934, 9.999999999999998224 ) ;
#34862 = CARTESIAN_POINT ( 'NONE',  ( 10.81189881249999907, 6.242252689847868297, -65.90625000204839523 ) ) ;
#34863 =( BOUNDED_CURVE ( )  B_SPLINE_CURVE ( 2, ( #29946, #36195, #3397, #39847, #20213, #26279, #6632 ),
 .UNSPECIFIED., .F., .F. ) 
 B_SPLINE_CURVE_WITH_KNOTS ( ( 3, 2, 2, 3 ),
 ( 0.5932835820895523415, 0.5945273631840797268, 0.5957711442786072231, 0.5970149253731344974 ),
 .UNSPECIFIED. ) 
 CURVE ( )  GEOMETRIC_REPRESENTATION_ITEM ( )  RATIONAL_B_SPLINE_CURVE ( ( 0.9999999999999880096, 0.8660254037844506980, 1.000000000000000000, 0.8660254037844387076, 1.000000000000000000, 0.8660254037844148378, 1.000000000000023981 ) ) 
 REPRESENTATION_ITEM ( '' )  );
#34864 = CARTESIAN_POINT ( 'NONE',  ( -9.999999999999998224, 1.224646799147353059E-15, -42.12500000409677625 ) ) ;
#34865 = CARTESIAN_POINT ( 'NONE',  ( 7.644554776091147741E-16, 12.48450537969573659, -0.9687500020483519325 ) ) ;
#34866 = CARTESIAN_POINT ( 'NONE',  ( 5.405949406249999534, 9.363379034771803333, -166.2812500020484094 ) ) ;
#34867 = DIRECTION ( 'NONE',  ( -0.000000000000000000, -0.000000000000000000, 1.000000000000000000 ) ) ;
#34868 = CARTESIAN_POINT ( 'NONE',  ( -9.999999999999998224, 1.224646799147353059E-15, -23.74999999999996447 ) ) ;
#34869 = ORIENTED_EDGE ( 'NONE', *, *, #31375, .T. ) ;
#34870 = CARTESIAN_POINT ( 'NONE',  ( -4.999999999999996447, 8.660254037844387298, -84.37500000409677625 ) ) ;
#34871 = AXIS2_PLACEMENT_3D ( 'NONE', #31819, #28573, #22300 ) ;
#34872 = CARTESIAN_POINT ( 'NONE',  ( 9.999999999999998224, 0.000000000000000000, -150.8750000040967905 ) ) ;
#34874 = VERTEX_POINT ( 'NONE', #5862 ) ;
#34873 = CARTESIAN_POINT ( 'NONE',  ( 5.405949406249992428, -9.363379034771808662, -81.28125000204839523 ) ) ;
#34875 = DIRECTION ( 'NONE',  ( 1.000000000000000000, 0.000000000000000000, 0.000000000000000000 ) ) ;
#34877 = ORIENTED_EDGE ( 'NONE', *, *, #34897, .F. ) ;
#34876 = CARTESIAN_POINT ( 'NONE',  ( 5.000000000000000000, 8.660254037844385522, -30.24999999999997158 ) ) ;
#34878 = VECTOR ( 'NONE', #18349, 1000.000000000000000 ) ;
#34879 = VERTEX_POINT ( 'NONE', #38661 ) ;
#34880 = CARTESIAN_POINT ( 'NONE',  ( -2.293366432827344421E-15, -12.48450537969573659, -37.71875000204836681 ) ) ;
#34881 = CARTESIAN_POINT ( 'NONE',  ( -9.999999999999998224, 1.224646799147353059E-15, -187.2500000000000000 ) ) ;
#34882 = CARTESIAN_POINT ( 'NONE',  ( 5.405949406249992428, -9.363379034771808662, -7.781250002048350822 ) ) ;
#34884 = ORIENTED_EDGE ( 'NONE', *, *, #33532, .T. ) ;
#34883 = CARTESIAN_POINT ( 'NONE',  ( 10.81189881249999551, -6.242252689847874514, -64.46875000204838102 ) ) ;
#34885 = CARTESIAN_POINT ( 'NONE',  ( -9.999999999998969713, -5.773502691896847949, -4.124999999999929834 ) ) ;
#34886 = CARTESIAN_POINT ( 'NONE',  ( 9.999999999999998224, 0.000000000000000000, -34.99999999999997868 ) ) ;
#34887 = CYLINDRICAL_SURFACE ( 'NONE', #112, 9.999999999999998224 ) ;
#34888 = CARTESIAN_POINT ( 'NONE',  ( 10.81189881249999907, 6.242252689847868297, -178.2187500020483810 ) ) ;
#34889 = CARTESIAN_POINT ( 'NONE',  ( -2.293366432827344421E-15, -12.48450537969573659, -157.7187500020484094 ) ) ;
#34890 = CARTESIAN_POINT ( 'NONE',  ( 9.999999999999479527, 5.773502691896553074, -43.87499999999995737 ) ) ;
#34891 = CARTESIAN_POINT ( 'NONE',  ( -9.999999999999998224, 1.224646799147353059E-15, -127.6250000040967620 ) ) ;
#34892 = CARTESIAN_POINT ( 'NONE',  ( -5.000000000000003553, -8.660254037844383745, -101.8750000040967905 ) ) ;
#34893 = CARTESIAN_POINT ( 'NONE',  ( -5.000000000000003553, -8.660254037844383745, -191.5000000000000000 ) ) ;
#34894 = CARTESIAN_POINT ( 'NONE',  ( -10.81189881249999729, 6.242252689847871849, -105.7187500020483668 ) ) ;
#34895 = CARTESIAN_POINT ( 'NONE',  ( 0.000000000000000000, 0.000000000000000000, -200.0000000000000000 ) ) ;
#34896 = CARTESIAN_POINT ( 'NONE',  ( -10.81189881249999729, 6.242252689847871849, -81.90625000204838102 ) ) ;
#34897 = EDGE_CURVE ( 'NONE', #27376, #2118, #27478, .T. ) ;
#34898 = CARTESIAN_POINT ( 'NONE',  ( 10.81189881249999729, 0.000000000000000000, -89.84375000204838102 ) ) ;
#34899 = EDGE_CURVE ( 'NONE', #7087, #6715, #35434, .T. ) ;
#34900 = CARTESIAN_POINT ( 'NONE',  ( -10.81189881249999729, 1.324075727343319199E-15, -68.28125000204838102 ) ) ;
#34901 = CARTESIAN_POINT ( 'NONE',  ( 10.00000000000000000, 5.773502691896255534, -146.2500000040967905 ) ) ;
#34902 = CARTESIAN_POINT ( 'NONE',  ( 9.999999999999998224, 0.000000000000000000, -120.5000000000000000 ) ) ;
#34903 = CARTESIAN_POINT ( 'NONE',  ( -2.293366432827344421E-15, -12.48450537969573659, -151.9062500020483810 ) ) ;
#34904 = CARTESIAN_POINT ( 'NONE',  ( 5.405949406249992428, -9.363379034771808662, -163.7812500020484094 ) ) ;
#34905 = DIRECTION ( 'NONE',  ( -4.506943796211477094E-16, 1.000000000000000000, 0.000000000000000000 ) ) ;
#34906 = CARTESIAN_POINT ( 'NONE',  ( 9.999999999999998224, 0.000000000000000000, -197.0000000000000000 ) ) ;
#34907 = CARTESIAN_POINT ( 'NONE',  ( -10.81189881249999729, 6.242252689847871849, -99.71875000204839523 ) ) ;
#34908 = ORIENTED_EDGE ( 'NONE', *, *, #31002, .T. ) ;
#34909 = CARTESIAN_POINT ( 'NONE',  ( -9.999999999999998224, 5.773502691896259087, -68.87499999999998579 ) ) ;
#34910 = CARTESIAN_POINT ( 'NONE',  ( 5.405949406249999534, 9.363379034771803333, -199.0937500020484094 ) ) ;
#34911 = CARTESIAN_POINT ( 'NONE',  ( 9.999999999999998224, 0.000000000000000000, -80.37500000409677625 ) ) ;
#34912 = CARTESIAN_POINT ( 'NONE',  ( 9.999999999999998224, 0.000000000000000000, -46.99999999999998579 ) ) ;
#34913 = CARTESIAN_POINT ( 'NONE',  ( 7.070501591499376803E-16, 11.54700538379251284, -8.000000004096749606 ) ) ;
#34914 = CARTESIAN_POINT ( 'NONE',  ( 5.405949406249992428, -9.363379034771808662, -96.28125000204838102 ) ) ;
#34915 = CARTESIAN_POINT ( 'NONE',  ( -5.405949406249996869, 9.363379034771805109, -73.03125000204838102 ) ) ;
#34916 = CARTESIAN_POINT ( 'NONE',  ( 9.999999999999996447, -5.773502691896262640, -71.50000000409676204 ) ) ;
#34917 = DIRECTION ( 'NONE',  ( 0.4999999999999998335, 0.8660254037844387076, 0.000000000000000000 ) ) ;
#34918 = CARTESIAN_POINT ( 'NONE',  ( 5.405949406249992428, -9.363379034771808662, -28.59375000204836326 ) ) ;
#34919 = ORIENTED_EDGE ( 'NONE', *, *, #39416, .T. ) ;
#34920 = CARTESIAN_POINT ( 'NONE',  ( 10.81189881249999551, -6.242252689847874514, -193.6562500020484379 ) ) ;
#34921 = CARTESIAN_POINT ( 'NONE',  ( -10.81189881249999729, 1.324075727343319199E-15, -18.78125000204835970 ) ) ;
#34922 = CARTESIAN_POINT ( 'NONE',  ( 5.405949406249992428, -9.363379034771808662, -9.093750002048345493 ) ) ;
#34923 = CARTESIAN_POINT ( 'NONE',  ( -9.999999999999998224, 1.224646799147353059E-15, -15.12500000409674961 ) ) ;
#34924 = EDGE_CURVE ( 'NONE', #34758, #15268, #9257, .T. ) ;
#34925 = CARTESIAN_POINT ( 'NONE',  ( -2.293366432827344421E-15, -12.48450537969573659, -147.2187500020484094 ) ) ;
#34926 = CARTESIAN_POINT ( 'NONE',  ( 10.00000000000102318, -5.773502691895667560, -37.00000000409672651 ) ) ;
#34927 = FACE_OUTER_BOUND ( 'NONE', #34453, .T. ) ;
#34928 = CARTESIAN_POINT ( 'NONE',  ( -5.000000000000003553, -8.660254037844383745, -172.0000000000000000 ) ) ;
#34929 = CARTESIAN_POINT ( 'NONE',  ( -9.999999999999998224, 1.224646799147353059E-15, -36.12500000409676915 ) ) ;
#34931 = ORIENTED_EDGE ( 'NONE', *, *, #17469, .T. ) ;
#34930 = CARTESIAN_POINT ( 'NONE',  ( -5.405949406250003975, -9.363379034771801557, -104.0312500020483810 ) ) ;
#34932 = CARTESIAN_POINT ( 'NONE',  ( 0.000000000000000000, 0.000000000000000000, -200.0000000000000000 ) ) ;
#34933 = EDGE_CURVE ( 'NONE', #18938, #28436, #40120, .T. ) ;
#34934 = ORIENTED_EDGE ( 'NONE', *, *, #15931, .F. ) ;
#34935 = VERTEX_POINT ( 'NONE', #35853 ) ;
#34936 = CARTESIAN_POINT ( 'NONE',  ( 7.644554776091147741E-16, 12.48450537969573659, -28.15625000204838457 ) ) ;
#34937 = PERSON_AND_ORGANIZATION ( #11915, #17965 ) ;
#34938 = CARTESIAN_POINT ( 'NONE',  ( 10.81189881249999729, 0.000000000000000000, -89.84375000204838102 ) ) ;
#34939 = DIRECTION ( 'NONE',  ( 1.000000000000000000, 0.000000000000000000, 0.000000000000000000 ) ) ;
#34940 = CARTESIAN_POINT ( 'NONE',  ( 8.145196138936681152, 6.643413332909280378, -99.99999999999997158 ) ) ;
#34941 = CARTESIAN_POINT ( 'NONE',  ( 9.999999999999479527, 5.773502691896553074, -123.3749999999999858 ) ) ;
#34942 = CARTESIAN_POINT ( 'NONE',  ( -2.293366432827344421E-15, -12.48450537969573659, -163.9062500020483810 ) ) ;
#34943 = CARTESIAN_POINT ( 'NONE',  ( 7.070501591499377789E-16, 11.54700538379251284, -9.500000004096756712 ) ) ;
#34944 = EDGE_CURVE ( 'NONE', #36032, #16199, #13638, .T. ) ;
#34945 = CARTESIAN_POINT ( 'NONE',  ( -2.293366432827344421E-15, -12.48450537969573659, -118.7187500020483668 ) ) ;
#34946 = PRODUCT_DEFINITION_SHAPE ( 'NONE', 'NONE',  #42693 ) ;
#34947 = CARTESIAN_POINT ( 'NONE',  ( 7.644554776091147741E-16, 12.48450537969573659, -83.46875000204838102 ) ) ;
#34948 = CARTESIAN_POINT ( 'NONE',  ( 7.644554776091147741E-16, 12.48450537969573659, -2.656250002048344161 ) ) ;
#34949 = CARTESIAN_POINT ( 'NONE',  ( 10.81189881249999729, 0.000000000000000000, -193.3437500020484094 ) ) ;
#34950 = CARTESIAN_POINT ( 'NONE',  ( -2.293366432827344421E-15, -12.48450537969573659, -93.40625000204839523 ) ) ;
#34951 = CARTESIAN_POINT ( 'NONE',  ( 7.070501591499377789E-16, 11.54700538379251284, -180.5000000040967905 ) ) ;
#34952 = CARTESIAN_POINT ( 'NONE',  ( 5.405949406249999534, 9.363379034771803333, -172.2812500020484094 ) ) ;
#34953 = ADVANCED_FACE ( 'NONE', ( #875 ), #30230, .F. ) ;
#34954 = CARTESIAN_POINT ( 'NONE',  ( -9.999999999999998224, 1.224646799147353059E-15, -151.2500000000000000 ) ) ;
#34955 = CARTESIAN_POINT ( 'NONE',  ( 10.81189881249999729, 6.242252689847867408, -176.9062500020484094 ) ) ;
#34956 = CARTESIAN_POINT ( 'NONE',  ( 5.405949406249992428, -9.363379034771808662, -184.7812500020484094 ) ) ;
#34957 = CARTESIAN_POINT ( 'NONE',  ( -2.293366432827344421E-15, -12.48450537969573659, -42.21875000204835260 ) ) ;
#34958 = EDGE_CURVE ( 'NONE', #19609, #41727, #18073, .T. ) ;
#34959 = CARTESIAN_POINT ( 'NONE',  ( -9.999999999999998224, 5.773502691896259087, -160.7500000040967620 ) ) ;
#34960 = CARTESIAN_POINT ( 'NONE',  ( 10.81189881249999551, -6.242252689847874514, -1.656250002048371694 ) ) ;
#34961 = CARTESIAN_POINT ( 'NONE',  ( 10.81189881249999907, 6.242252689847868297, -13.21875000204836148 ) ) ;
#34962 = CARTESIAN_POINT ( 'NONE',  ( -2.121150477449813534E-15, -11.54700538379251284, -193.2500000040968473 ) ) ;
#34963 = CARTESIAN_POINT ( 'NONE',  ( 10.81189881249999907, 6.242252689847868297, -119.7187500020483810 ) ) ;
#34964 = CARTESIAN_POINT ( 'NONE',  ( 10.00000000000000000, 5.773502691896255534, -88.87499999999998579 ) ) ;
#34965 = CARTESIAN_POINT ( 'NONE',  ( 5.405949406249999534, 9.363379034771803333, -20.78125000204836326 ) ) ;
#34966 = CARTESIAN_POINT ( 'NONE',  ( -4.999999999999996447, 8.660254037844387298, -108.3750000040967763 ) ) ;
#34967 = DIRECTION ( 'NONE',  ( -0.000000000000000000, -0.000000000000000000, 1.000000000000000000 ) ) ;
#34968 = CARTESIAN_POINT ( 'NONE',  ( 7.070501591499377789E-16, 11.54700538379251284, -51.12499999999997868 ) ) ;
#34969 = CARTESIAN_POINT ( 'NONE',  ( -10.81189881249999729, 6.242252689847871849, -117.9062500020483952 ) ) ;
#34970 = CARTESIAN_POINT ( 'NONE',  ( 5.405949406249999534, 9.363379034771803333, -101.7812500020483952 ) ) ;
#34971 = EDGE_LOOP ( 'NONE', ( #38197, #28964, #26414, #15469 ) ) ;
#34972 = CARTESIAN_POINT ( 'NONE',  ( 5.000000000000000000, 8.660254037844385522, -90.62500000409677625 ) ) ;
#34973 = CARTESIAN_POINT ( 'NONE',  ( -9.999999999999998224, 1.224646799147353059E-15, -28.62500000409676204 ) ) ;
#34974 = CARTESIAN_POINT ( 'NONE',  ( -2.293366432827344421E-15, -12.48450537969573659, -154.9062500020483810 ) ) ;
#34975 = CARTESIAN_POINT ( 'NONE',  ( 5.405949406249992428, -9.363379034771808662, -54.09375000204835970 ) ) ;
#34976 = ORIENTED_EDGE ( 'NONE', *, *, #3590, .T. ) ;
#34977 = CARTESIAN_POINT ( 'NONE',  ( -2.121150477449813534E-15, -11.54700538379251284, -14.37499999999997158 ) ) ;
#34978 = CARTESIAN_POINT ( 'NONE',  ( -10.81189881249999729, 1.324075727343319199E-15, -29.28125000204837036 ) ) ;
#34979 = CARTESIAN_POINT ( 'NONE',  ( -9.999999999999998224, 1.224646799147353059E-15, -151.2500000000000000 ) ) ;
#34980 = CARTESIAN_POINT ( 'NONE',  ( -9.999999999999998224, 5.773502691896259087, -16.75000000409676559 ) ) ;
#34981 = ADVANCED_FACE ( 'NONE', ( #23322 ), #13575, .F. ) ;
#34982 = LINE ( 'NONE', #5409, #22917 ) ;
#34983 = CARTESIAN_POINT ( 'NONE',  ( -5.405949406250003975, -9.363379034771801557, -122.0312500020483952 ) ) ;
#34984 = CARTESIAN_POINT ( 'NONE',  ( 5.134740825434541023, 9.087941876063259983, -1.486633740873807081E-14 ) ) ;
#34985 = CARTESIAN_POINT ( 'NONE',  ( 4.999999999999992006, -8.660254037844389075, -44.62500000409677625 ) ) ;
#34986 = ORIENTED_EDGE ( 'NONE', *, *, #10314, .T. ) ;
#34987 =( BOUNDED_CURVE ( )  B_SPLINE_CURVE ( 2, ( #31851, #32264, #5505, #25153, #18876, #2285, #16035 ),
 .UNSPECIFIED., .F., .F. ) 
 B_SPLINE_CURVE_WITH_KNOTS ( ( 3, 2, 2, 3 ),
 ( 0.7126865671641793298, 0.7139303482587067151, 0.7151741293532342114, 0.7164179104477614857 ),
 .UNSPECIFIED. ) 
 CURVE ( )  GEOMETRIC_REPRESENTATION_ITEM ( )  RATIONAL_B_SPLINE_CURVE ( ( 0.9999999999999761302, 0.8660254037844625774, 1.000000000000000000, 0.8660254037844387076, 1.000000000000000000, 0.8660254037844028474, 1.000000000000035971 ) ) 
 REPRESENTATION_ITEM ( '' )  );
#34988 = CARTESIAN_POINT ( 'NONE',  ( 10.81189881249999551, -6.242252689847874514, -60.15625000204839523 ) ) ;
#34989 = DATE_AND_TIME ( #38209, #24905 ) ;
#34990 = CARTESIAN_POINT ( 'NONE',  ( 7.644554776091147741E-16, 12.48450537969573659, -110.4687500020483668 ) ) ;
#34992 = ORIENTED_EDGE ( 'NONE', *, *, #28859, .F. ) ;
#34991 = VERTEX_POINT ( 'NONE', #20704 ) ;
#34993 = DIRECTION ( 'NONE',  ( 1.000000000000000000, 0.000000000000000000, 0.000000000000000000 ) ) ;
#34994 = DIRECTION ( 'NONE',  ( -0.000000000000000000, -0.000000000000000000, 1.000000000000000000 ) ) ;
#34995 = CARTESIAN_POINT ( 'NONE',  ( 10.81189881249999907, 6.242252689847868297, -154.2187500020483810 ) ) ;
#34996 = CARTESIAN_POINT ( 'NONE',  ( -5.405949406250003975, -9.363379034771801557, -186.5312500020484094 ) ) ;
#34997 = CARTESIAN_POINT ( 'NONE',  ( 5.405949406249992428, -9.363379034771808662, -7.593750002048343717 ) ) ;
#34998 = CARTESIAN_POINT ( 'NONE',  ( -2.293366432827344421E-15, -12.48450537969573659, -139.7187500020483810 ) ) ;
#34999 = CARTESIAN_POINT ( 'NONE',  ( -10.81189881249999729, 1.324075727343319199E-15, -107.0937500020483810 ) ) ;
#35000 = DIRECTION ( 'NONE',  ( 1.000000000000000000, 0.000000000000000000, 0.000000000000000000 ) ) ;
#35001 = CARTESIAN_POINT ( 'NONE',  ( 5.405949406249992428, -9.363379034771808662, -115.7812500020483952 ) ) ;
#35002 = CARTESIAN_POINT ( 'NONE',  ( 5.405949406249999534, 9.363379034771803333, 0.4062499979516354109 ) ) ;
#35003 = CARTESIAN_POINT ( 'NONE',  ( -10.81189881249999729, 1.324075727343319199E-15, -125.0937500020483668 ) ) ;
#35004 = CARTESIAN_POINT ( 'NONE',  ( 5.405949406249992428, -9.363379034771808662, -193.7812500020484094 ) ) ;
#35005 = DIRECTION ( 'NONE',  ( -0.000000000000000000, -0.000000000000000000, -1.000000000000000000 ) ) ;
#35006 = CARTESIAN_POINT ( 'NONE',  ( -10.00000000000000000, -5.773502691896251982, -148.1249999999999716 ) ) ;
#35007 = CARTESIAN_POINT ( 'NONE',  ( -2.121150477449813534E-15, -11.54700538379251284, -15.87499999999997335 ) ) ;
#35008 = CARTESIAN_POINT ( 'NONE',  ( -10.81189881249999729, 6.242252689847871849, -71.21875000204839523 ) ) ;
#35009 = CARTESIAN_POINT ( 'NONE',  ( 7.644554776091147741E-16, 12.48450537969573659, -54.96875000204836681 ) ) ;
#35010 = CARTESIAN_POINT ( 'NONE',  ( -10.00000000000000000, -5.773502691896251982, -189.0000000040967905 ) ) ;
#35011 = CARTESIAN_POINT ( 'NONE',  ( -5.405949406249996869, 9.363379034771805109, -29.53125000204837036 ) ) ;
#35012 = VECTOR ( 'NONE', #389, 1000.000000000000000 ) ;
#35013 = CARTESIAN_POINT ( 'NONE',  ( 5.405949406249999534, 9.363379034771803333, -41.59375000204837391 ) ) ;
#35014 = CARTESIAN_POINT ( 'NONE',  ( -10.00000000000076916, 5.773502691895813221, -136.3749999999999716 ) ) ;
#35015 = CARTESIAN_POINT ( 'NONE',  ( -5.405949406250003975, -9.363379034771801557, -142.8437500020483810 ) ) ;
#35016 = CARTESIAN_POINT ( 'NONE',  ( 4.999999999999992006, -8.660254037844389075, -111.7499999999999858 ) ) ;
#35017 = CARTESIAN_POINT ( 'NONE',  ( 4.999999999999992006, -8.660254037844389075, -170.2500000000000000 ) ) ;
#35018 = CARTESIAN_POINT ( 'NONE',  ( -4.999999999999996447, 8.660254037844387298, -73.49999999999998579 ) ) ;
#35019 = CARTESIAN_POINT ( 'NONE',  ( 5.405949406249992428, -9.363379034771808662, -144.2812500020483810 ) ) ;
#35020 = CARTESIAN_POINT ( 'NONE',  ( 10.81189881249999729, 6.242252689847867408, -11.90625000204835615 ) ) ;
#35021 = VERTEX_POINT ( 'NONE', #30649 ) ;
#35022 = CARTESIAN_POINT ( 'NONE',  ( -9.999999999999998224, 5.773502691896259087, -117.2500000040967763 ) ) ;
#35023 = DIRECTION ( 'NONE',  ( 0.000000000000000000, 0.000000000000000000, -1.000000000000000000 ) ) ;
#35024 = CARTESIAN_POINT ( 'NONE',  ( -10.81189881249999907, -6.242252689847864744, -72.46875000204835260 ) ) ;
#35025 = CARTESIAN_POINT ( 'NONE',  ( -9.999999999999998224, 1.224646799147353059E-15, -47.74999999999998579 ) ) ;
#35026 = ADVANCED_FACE ( 'NONE', ( #27188 ), #40332, .F. ) ;
#35027 = CARTESIAN_POINT ( 'NONE',  ( -10.00000000000000000, -5.773502691896251982, -27.00000000409677625 ) ) ;
#35028 = CARTESIAN_POINT ( 'NONE',  ( -9.999999999998969713, -5.773502691896847949, -3.000000004096732731 ) ) ;
#35029 = CARTESIAN_POINT ( 'NONE',  ( 10.81189881249999729, 0.000000000000000000, -45.03125000204838102 ) ) ;
#35030 = CARTESIAN_POINT ( 'NONE',  ( -5.000000000000003553, -8.660254037844383745, -99.99999999999998579 ) ) ;
#35031 = CARTESIAN_POINT ( 'NONE',  ( -10.81189881249999907, -6.242252689847864744, -141.6562500020483810 ) ) ;
#35032 = CARTESIAN_POINT ( 'NONE',  ( -10.81189881249999729, 6.242252689847871849, -131.2187500020483810 ) ) ;
#35033 = CARTESIAN_POINT ( 'NONE',  ( -1.040834085586084257E-14, -139.9999999999999716, 22.49999999999999289 ) ) ;
#35034 = CARTESIAN_POINT ( 'NONE',  ( -2.121150477449813534E-15, -11.54700538379251284, -127.2500000040967763 ) ) ;
#35036 = EDGE_CURVE ( 'NONE', #2553, #18128, #37099, .T. ) ;
#35035 = VERTEX_POINT ( 'NONE', #3686 ) ;
#35037 = ORIENTED_EDGE ( 'NONE', *, *, #36779, .T. ) ;
#35038 = AXIS2_PLACEMENT_3D ( 'NONE', #26431, #23632, #19520 ) ;
#35039 = ORIENTED_EDGE ( 'NONE', *, *, #17227, .F. ) ;
#35040 = CIRCLE ( 'NONE', #19857, 9.750000000000001776 ) ;
#35041 = CARTESIAN_POINT ( 'NONE',  ( 0.000000000000000000, 0.000000000000000000, -200.0000000000000000 ) ) ;
#35042 = CARTESIAN_POINT ( 'NONE',  ( 7.644554776091147741E-16, 12.48450537969573659, -179.4687500020483810 ) ) ;
#35043 = CARTESIAN_POINT ( 'NONE',  ( -10.81189881249999729, 1.324075727343319199E-15, -33.59375000204836681 ) ) ;
#35044 = CARTESIAN_POINT ( 'NONE',  ( 5.405949406249992428, -9.363379034771808662, -168.0937500020484094 ) ) ;
#35045 = CARTESIAN_POINT ( 'NONE',  ( -10.81189881249999729, 6.242252689847871849, -153.7187500020483526 ) ) ;
#35046 = CYLINDRICAL_SURFACE ( 'NONE', #19678, 9.999999999999998224 ) ;
#35047 = CARTESIAN_POINT ( 'NONE',  ( -10.81189881249999729, 1.324075727343319199E-15, -135.5937500020483810 ) ) ;
#35048 = CARTESIAN_POINT ( 'NONE',  ( 10.81189881249999729, 0.000000000000000000, -144.0312500020483810 ) ) ;
#35049 = CARTESIAN_POINT ( 'NONE',  ( -10.81189881249999729, 1.324075727343319199E-15, -143.0937500020483810 ) ) ;
#35050 = CARTESIAN_POINT ( 'NONE',  ( 9.999999999999998224, 0.000000000000000000, -129.5000000000000000 ) ) ;
#35051 = CARTESIAN_POINT ( 'NONE',  ( 9.999999999999998224, 0.000000000000000000, -11.37500000409674783 ) ) ;
#35052 = CARTESIAN_POINT ( 'NONE',  ( 7.070501591499377789E-16, 11.54700538379251284, -174.1250000000000000 ) ) ;
#35053 = CARTESIAN_POINT ( 'NONE',  ( 5.405949406249992428, -9.363379034771808662, -79.59375000204838102 ) ) ;
#35054 = LINE ( 'NONE', #19061, #10685 ) ;
#35055 = CARTESIAN_POINT ( 'NONE',  ( 10.81189881249999551, -6.242252689847874514, -46.65625000204835970 ) ) ;
#35056 = CARTESIAN_POINT ( 'NONE',  ( -5.378272834344112852, -8.460370942358581559, -99.99999999999998579 ) ) ;
#35057 = CARTESIAN_POINT ( 'NONE',  ( 5.405949406249999534, 9.363379034771803333, -169.0937500020484094 ) ) ;
#35058 = CARTESIAN_POINT ( 'NONE',  ( -10.81189881249999729, 6.242252689847871849, -111.9062500020483810 ) ) ;
#35059 = CARTESIAN_POINT ( 'NONE',  ( -10.81189881249999729, 1.324075727343319199E-15, -146.2812500020483810 ) ) ;
#35060 = CARTESIAN_POINT ( 'NONE',  ( 9.999999999999998224, 0.000000000000000000, -143.3750000040967905 ) ) ;
#35061 = CARTESIAN_POINT ( 'NONE',  ( -10.81189881249999907, -6.242252689847864744, -44.15625000204837391 ) ) ;
#35062 = CARTESIAN_POINT ( 'NONE',  ( 10.00000000000000000, 5.773502691896255534, -123.7500000040967905 ) ) ;
#35063 = CARTESIAN_POINT ( 'NONE',  ( 9.999999999999998224, 0.000000000000000000, -99.49999999999998579 ) ) ;
#35064 = EDGE_CURVE ( 'NONE', #35302, #13289, #22495, .T. ) ;
#35065 = VERTEX_POINT ( 'NONE', #13366 ) ;
#35066 = CARTESIAN_POINT ( 'NONE',  ( -10.81189881249999729, 1.324075727343319199E-15, -128.2812500020483810 ) ) ;
#35067 = CARTESIAN_POINT ( 'NONE',  ( -10.00000000000000000, -5.773502691896251982, -136.5000000040967905 ) ) ;
#35068 = CARTESIAN_POINT ( 'NONE',  ( 9.999999999999678479, 5.773502691896442940, -184.8750000000000284 ) ) ;
#35069 = CARTESIAN_POINT ( 'NONE',  ( 5.405949406249999534, 9.363379034771803333, -182.7812500020484094 ) ) ;
#35070 = ORIENTED_EDGE ( 'NONE', *, *, #13176, .F. ) ;
#35071 = CARTESIAN_POINT ( 'NONE',  ( -10.00000000000000000, -5.773502691896251982, -51.00000000409676204 ) ) ;
#35072 = AXIS2_PLACEMENT_3D ( 'NONE', #12617, #13455, #39173 ) ;
#35073 =( BOUNDED_CURVE ( )  B_SPLINE_CURVE ( 2, ( #39014, #22833, #12877, #16537, #35996, #29519, #3402 ),
 .UNSPECIFIED., .F., .F. ) 
 B_SPLINE_CURVE_WITH_KNOTS ( ( 3, 2, 2, 3 ),
 ( 0.3880597014925373789, 0.3893034825870647087, 0.3905472636815920939, 0.3917910447761194792 ),
 .UNSPECIFIED. ) 
 CURVE ( )  GEOMETRIC_REPRESENTATION_ITEM ( )  RATIONAL_B_SPLINE_CURVE ( ( 0.9999999999999940048, 0.8660254037844447028, 1.000000000000000000, 0.8660254037844387076, 1.000000000000000000, 0.8660254037844327124, 1.000000000000005995 ) ) 
 REPRESENTATION_ITEM ( '' )  );
#35074 = CARTESIAN_POINT ( 'NONE',  ( -9.999999999999612754, -5.773502691896474914, -155.6249999999999716 ) ) ;
#35075 = CARTESIAN_POINT ( 'NONE',  ( -10.81189881249999729, 1.324075727343319199E-15, -65.28125000204838102 ) ) ;
#35076 = DIRECTION ( 'NONE',  ( -0.000000000000000000, -0.000000000000000000, 1.000000000000000000 ) ) ;
#35077 = CARTESIAN_POINT ( 'NONE',  ( 10.81189881249999907, 6.242252689847868297, -166.4062500020483810 ) ) ;
#35078 = CARTESIAN_POINT ( 'NONE',  ( 9.999999999999998224, 0.000000000000000000, -162.5000000000000000 ) ) ;
#35079 = CARTESIAN_POINT ( 'NONE',  ( 10.00000000000051159, -5.773502691895965988, -34.00000000409673362 ) ) ;
#35081 = ORIENTED_EDGE ( 'NONE', *, *, #11491, .F. ) ;
#35080 = EDGE_CURVE ( 'NONE', #1591, #36081, #4103, .T. ) ;
#35082 = CARTESIAN_POINT ( 'NONE',  ( 7.070501591499376803E-16, 11.54700538379251284, -17.00000000409675849 ) ) ;
#35083 = CARTESIAN_POINT ( 'NONE',  ( -2.121150477449813534E-15, -11.54700538379251284, -194.3750000000000284 ) ) ;
#35084 = CARTESIAN_POINT ( 'NONE',  ( -9.999999999999998224, 1.224646799147353059E-15, -136.6250000040967620 ) ) ;
#35086 = ORIENTED_EDGE ( 'NONE', *, *, #30941, .F. ) ;
#35085 = CARTESIAN_POINT ( 'NONE',  ( -10.81189881249999729, 6.242252689847871849, -80.40625000204839523 ) ) ;
#35088 = VERTEX_POINT ( 'NONE', #17244 ) ;
#35087 = CARTESIAN_POINT ( 'NONE',  ( -2.121150477449813534E-15, -11.54700538379251284, -178.2500000040968189 ) ) ;
#35089 = ORIENTED_EDGE ( 'NONE', *, *, #12748, .F. ) ;
#35090 = CARTESIAN_POINT ( 'NONE',  ( 7.644554776091147741E-16, 12.48450537969573659, -30.96875000204835260 ) ) ;
#35091 = FACE_OUTER_BOUND ( 'NONE', #5538, .T. ) ;
#35092 = CARTESIAN_POINT ( 'NONE',  ( -2.293366432827344421E-15, -12.48450537969573659, -3.406250002048348158 ) ) ;
#35094 = VERTEX_POINT ( 'NONE', #16814 ) ;
#35093 = CARTESIAN_POINT ( 'NONE',  ( 10.81189881249999729, 0.000000000000000000, -58.34375000204835970 ) ) ;
#35095 = DIRECTION ( 'NONE',  ( 1.000000000000000000, 0.000000000000000000, 0.000000000000000000 ) ) ;
#35096 = CARTESIAN_POINT ( 'NONE',  ( 5.000000000000000000, 8.660254037844385522, -36.24999999999997868 ) ) ;
#35097 = AXIS2_PLACEMENT_3D ( 'NONE', #27077, #8080, #40220 ) ;
#35098 = CARTESIAN_POINT ( 'NONE',  ( 10.81189881249999551, -6.242252689847874514, -184.4687500020483810 ) ) ;
#35099 = CARTESIAN_POINT ( 'NONE',  ( 7.644554776091147741E-16, 12.48450537969573659, -176.4687500020483810 ) ) ;
#35100 = CARTESIAN_POINT ( 'NONE',  ( 10.81189881249999729, 0.000000000000000000, -157.3437500020483810 ) ) ;
#35101 = CARTESIAN_POINT ( 'NONE',  ( 7.644554776091147741E-16, 12.48450537969573659, -171.9687500020483810 ) ) ;
#35102 = CARTESIAN_POINT ( 'NONE',  ( 9.999999999999998224, 0.000000000000000000, -129.5000000000000000 ) ) ;
#35103 = CARTESIAN_POINT ( 'NONE',  ( 9.999999999999998224, 0.000000000000000000, -191.3750000040967905 ) ) ;
#35104 = CARTESIAN_POINT ( 'NONE',  ( -5.000000000000003553, -8.660254037844383745, -194.5000000000000000 ) ) ;
#35105 = AXIS2_PLACEMENT_3D ( 'NONE', #34253, #1875, #8558 ) ;
#35106 = CARTESIAN_POINT ( 'NONE',  ( 10.81189881249999729, 0.000000000000000000, -101.8437500020483810 ) ) ;
#35107 = CARTESIAN_POINT ( 'NONE',  ( -9.999999999999998224, 1.224646799147353059E-15, -115.6250000040967905 ) ) ;
#35108 = CARTESIAN_POINT ( 'NONE',  ( -10.81189881249999729, 6.242252689847871849, -83.40625000204836681 ) ) ;
#35109 = CARTESIAN_POINT ( 'NONE',  ( -10.81189881249999729, -6.242252689847864744, -90.46875000204838102 ) ) ;
#35110 = CARTESIAN_POINT ( 'NONE',  ( 7.644554776091147741E-16, 12.48450537969573659, -70.15625000204839523 ) ) ;
#35111 = CARTESIAN_POINT ( 'NONE',  ( -9.999999999999998224, 1.224646799147353059E-15, -142.6250000040967905 ) ) ;
#35112 = CARTESIAN_POINT ( 'NONE',  ( -9.999999999999998224, 1.224646799147353059E-15, -125.7499999999999716 ) ) ;
#35113 =( BOUNDED_CURVE ( )  B_SPLINE_CURVE ( 2, ( #17386, #21062, #1229 ),
 .UNSPECIFIED., .F., .F. ) 
 B_SPLINE_CURVE_WITH_KNOTS ( ( 3, 3 ),
 ( 0.4962686567164180107, 0.4975124378109453960 ),
 .UNSPECIFIED. ) 
 CURVE ( )  GEOMETRIC_REPRESENTATION_ITEM ( )  RATIONAL_B_SPLINE_CURVE ( ( 0.9999999999999880096, 0.8660254037844387076, 1.000000000000011990 ) ) 
 REPRESENTATION_ITEM ( '' )  );
#35114 = EDGE_LOOP ( 'NONE', ( #765, #11259, #36239, #4537 ) ) ;
#35115 = CARTESIAN_POINT ( 'NONE',  ( -5.405949406249996869, 9.363379034771805109, -148.0312500020483810 ) ) ;
#35116 = CARTESIAN_POINT ( 'NONE',  ( 7.644554776091147741E-16, 12.48450537969573659, -161.6562500020484379 ) ) ;
#35117 = CARTESIAN_POINT ( 'NONE',  ( -9.999999999999998224, 1.224646799147353059E-15, -97.62500000409677625 ) ) ;
#35118 = CARTESIAN_POINT ( 'NONE',  ( -2.121150477449813534E-15, -11.54700538379251284, -51.87499999999997868 ) ) ;
#35119 = CARTESIAN_POINT ( 'NONE',  ( -10.81189881249999729, 1.324075727343319199E-15, -95.09375000204838102 ) ) ;
#35120 = ORIENTED_EDGE ( 'NONE', *, *, #27036, .T. ) ;
#35121 = CARTESIAN_POINT ( 'NONE',  ( -4.999999999999996447, 8.660254037844387298, -62.99999999999997158 ) ) ;
#35122 = CARTESIAN_POINT ( 'NONE',  ( 5.405949406249999534, 9.363379034771803333, -194.5937500020484094 ) ) ;
#35123 = CARTESIAN_POINT ( 'NONE',  ( 5.000000000000000000, 8.660254037844385522, -75.62500000409677625 ) ) ;
#35124 = CARTESIAN_POINT ( 'NONE',  ( 8.340417757194298787, -6.866608375281687771, -180.0000000000000284 ) ) ;
#35125 = CARTESIAN_POINT ( 'NONE',  ( -9.999999999999998224, 1.224646799147353059E-15, -145.2500000000000000 ) ) ;
#35126 = CARTESIAN_POINT ( 'NONE',  ( 7.644554776091147741E-16, 12.48450537969573659, -94.15625000204839523 ) ) ;
#35127 = CARTESIAN_POINT ( 'NONE',  ( -5.405949406250003975, -9.363379034771801557, -74.03125000204838102 ) ) ;
#35128 =( BOUNDED_CURVE ( )  B_SPLINE_CURVE ( 2, ( #35725, #30256, #12600, #16841, #23989, #6155, #33496 ),
 .UNSPECIFIED., .F., .F. ) 
 B_SPLINE_CURVE_WITH_KNOTS ( ( 3, 2, 2, 3 ),
 ( 0.4552238805970150737, 0.4564676616915424590, 0.4577114427860698442, 0.4589552238805971740 ),
 .UNSPECIFIED. ) 
 CURVE ( )  GEOMETRIC_REPRESENTATION_ITEM ( )  RATIONAL_B_SPLINE_CURVE ( ( 0.9999999999999820144, 0.8660254037844566932, 1.000000000000000000, 0.8660254037844387076, 1.000000000000000000, 0.8660254037844207220, 1.000000000000017986 ) ) 
 REPRESENTATION_ITEM ( '' )  );
#35129 = CARTESIAN_POINT ( 'NONE',  ( -2.121150477449813534E-15, -11.54700538379251284, -67.25000000409679046 ) ) ;
#35130 = DIRECTION ( 'NONE',  ( -0.000000000000000000, -0.000000000000000000, -1.000000000000000000 ) ) ;
#35131 = CARTESIAN_POINT ( 'NONE',  ( -2.293366432827344421E-15, -12.48450537969573659, -28.71875000204834905 ) ) ;
#35132 = VERTEX_POINT ( 'NONE', #30013 ) ;
#35133 = CARTESIAN_POINT ( 'NONE',  ( 5.405949406249992428, -9.363379034771808662, -192.2812500020484094 ) ) ;
#35134 = CARTESIAN_POINT ( 'NONE',  ( 5.405949406249992428, -9.363379034771808662, -22.78125000204836326 ) ) ;
#35135 = CARTESIAN_POINT ( 'NONE',  ( 7.644554776091147741E-16, 12.48450537969573659, -2.468750002048359704 ) ) ;
#35136 = CARTESIAN_POINT ( 'NONE',  ( 9.999999999999998224, 0.000000000000000000, -132.5000000000000000 ) ) ;
#35137 = CARTESIAN_POINT ( 'NONE',  ( 5.000000000000000000, 8.660254037844385522, 0.8749999959032361829 ) ) ;
#35138 = CARTESIAN_POINT ( 'NONE',  ( -9.999999999999998224, 5.773502691896259087, -175.3750000000000000 ) ) ;
#35139 = CARTESIAN_POINT ( 'NONE',  ( 0.000000000000000000, 0.000000000000000000, -200.0000000000000000 ) ) ;
#35141 = EDGE_LOOP ( 'NONE', ( #40437, #27511, #11872, #13011 ) ) ;
#35140 = CARTESIAN_POINT ( 'NONE',  ( -10.81189881249999729, 1.324075727343319199E-15, -104.2812500020483810 ) ) ;
#35142 = CARTESIAN_POINT ( 'NONE',  ( 5.000000000000000000, 8.660254037844385522, -170.1250000040968189 ) ) ;
#35143 = EDGE_CURVE ( 'NONE', #25583, #13583, #26766, .T. ) ;
#35144 = ORIENTED_EDGE ( 'NONE', *, *, #24156, .F. ) ;
#35145 = ADVANCED_FACE ( 'NONE', ( #10349 ), #23537, .T. ) ;
#35146 = ORIENTED_EDGE ( 'NONE', *, *, #21446, .F. ) ;
#35147 = CARTESIAN_POINT ( 'NONE',  ( 7.644554776091147741E-16, 12.48450537969573659, -31.15625000204835260 ) ) ;
#35148 = CALENDAR_DATE ( 2026, 28, 9 ) ;
#35149 = CARTESIAN_POINT ( 'NONE',  ( 10.81189881249999551, -6.242252689847874514, -80.96875000204838102 ) ) ;
#35150 = CARTESIAN_POINT ( 'NONE',  ( 4.999999999999992006, -8.660254037844389075, -4.125000004096768258 ) ) ;
#35151 = CARTESIAN_POINT ( 'NONE',  ( 10.81189881249999907, 6.242252689847868297, -199.2187500020484094 ) ) ;
#35152 = CARTESIAN_POINT ( 'NONE',  ( 9.999999999999998224, 0.000000000000000000, -69.87500000409677625 ) ) ;
#35153 = CARTESIAN_POINT ( 'NONE',  ( -10.81189881249999729, 6.242252689847871849, -161.4062500020483810 ) ) ;
#35154 = CARTESIAN_POINT ( 'NONE',  ( 10.00000000000000000, 5.773502691896255534, -14.25000000409676382 ) ) ;
#35155 = CARTESIAN_POINT ( 'NONE',  ( -10.00000000000000000, -5.773502691896252870, -172.5000000040967905 ) ) ;
#35156 = CARTESIAN_POINT ( 'NONE',  ( 10.81189881249999551, -6.242252689847874514, -125.9687500020483810 ) ) ;
#35157 = CARTESIAN_POINT ( 'NONE',  ( -10.81189881249999729, -6.242252689847864744, -118.9687500020483810 ) ) ;
#35158 = CARTESIAN_POINT ( 'NONE',  ( -10.81189881249999729, 1.324075727343319199E-15, -83.09375000204836681 ) ) ;
#35159 = CARTESIAN_POINT ( 'NONE',  ( 10.81189881249999551, -6.242252689847874514, -191.9687500020484379 ) ) ;
#35160 = CARTESIAN_POINT ( 'NONE',  ( -5.405949406249996869, 9.363379034771805109, -89.53125000204838102 ) ) ;
#35161 = CARTESIAN_POINT ( 'NONE',  ( 9.999999999999996447, -5.773502691896262640, -173.5000000040968189 ) ) ;
#35162 = CARTESIAN_POINT ( 'NONE',  ( 10.81189881249999729, 0.000000000000000000, -168.0312500020484094 ) ) ;
#35163 = CARTESIAN_POINT ( 'NONE',  ( -4.999999999999996447, 8.660254037844387298, -102.3750000040967905 ) ) ;
#35164 = CARTESIAN_POINT ( 'NONE',  ( -2.293366432827344421E-15, -12.48450537969573659, -172.9062500020484379 ) ) ;
#35165 = CARTESIAN_POINT ( 'NONE',  ( -10.81189881249999729, 1.324075727343319199E-15, -188.2812500020484094 ) ) ;
#35166 = CARTESIAN_POINT ( 'NONE',  ( 7.644554776091147741E-16, 12.48450537969573659, -41.46875000204835260 ) ) ;
#35167 = AXIS2_PLACEMENT_3D ( 'NONE', #14768, #41093, #21691 ) ;
#35168 = CARTESIAN_POINT ( 'NONE',  ( 9.999999999999996447, -5.773502691896262640, -163.0000000040967905 ) ) ;
#35169 = CARTESIAN_POINT ( 'NONE',  ( -5.405949406249996869, 9.363379034771805109, -4.031250002048375691 ) ) ;
#35170 = CARTESIAN_POINT ( 'NONE',  ( -10.81189881249999729, 1.324075727343319199E-15, -17.09375000204835260 ) ) ;
#35171 = CARTESIAN_POINT ( 'NONE',  ( -9.999999999999998224, 1.224646799147353059E-15, -64.24999999999997158 ) ) ;
#35172 = CARTESIAN_POINT ( 'NONE',  ( -2.293366432827344421E-15, -12.48450537969573659, -124.7187500020483668 ) ) ;
#35173 = CARTESIAN_POINT ( 'NONE',  ( 9.999999999999998224, 0.000000000000000000, -87.49999999999998579 ) ) ;
#35174 = CARTESIAN_POINT ( 'NONE',  ( -5.405949406249996869, 9.363379034771805109, -19.03125000204835970 ) ) ;
#35175 = CARTESIAN_POINT ( 'NONE',  ( -5.000000000000003553, -8.660254037844383745, -94.37500000409677625 ) ) ;
#35176 = DIRECTION ( 'NONE',  ( -0.000000000000000000, -0.000000000000000000, 1.000000000000000000 ) ) ;
#35177 = CARTESIAN_POINT ( 'NONE',  ( -5.405949406249996869, 9.363379034771805109, -113.5312500020483952 ) ) ;
#35178 = CARTESIAN_POINT ( 'NONE',  ( 5.405949406249999534, 9.363379034771803333, -97.28125000204839523 ) ) ;
#35179 = ORIENTED_EDGE ( 'NONE', *, *, #16145, .T. ) ;
#35180 = CARTESIAN_POINT ( 'NONE',  ( 9.999999999999996447, -5.773502691896262640, -89.50000000409676204 ) ) ;
#35181 = CARTESIAN_POINT ( 'NONE',  ( -2.293366432827344421E-15, -12.48450537969573659, -156.4062500020483810 ) ) ;
#35182 = CARTESIAN_POINT ( 'NONE',  ( 10.81189881249999907, 6.242252689847868297, -53.71875000204837391 ) ) ;
#35183 = EDGE_LOOP ( 'NONE', ( #3269, #17088, #32647, #7900 ) ) ;
#35184 = CARTESIAN_POINT ( 'NONE',  ( 9.999999999999996447, -5.773502691896262640, -14.12499999999997158 ) ) ;
#35185 = CARTESIAN_POINT ( 'NONE',  ( -10.81189881249999729, 1.324075727343319199E-15, -30.78125000204837036 ) ) ;
#35186 = CARTESIAN_POINT ( 'NONE',  ( 4.999999999999992006, -8.660254037844389075, -150.7500000000000000 ) ) ;
#35187 = CARTESIAN_POINT ( 'NONE',  ( -2.121150477449813534E-15, -11.54700538379251284, -19.25000000409676559 ) ) ;
#35188 = CARTESIAN_POINT ( 'NONE',  ( -9.999999999999998224, 1.224646799147353059E-15, -136.6250000040967620 ) ) ;
#35190 = VERTEX_POINT ( 'NONE', #13788 ) ;
#35189 = CARTESIAN_POINT ( 'NONE',  ( 10.81189881249999907, 6.242252689847868297, -127.4062500020483810 ) ) ;
#35191 = CARTESIAN_POINT ( 'NONE',  ( 9.999999999999479527, 5.773502691896553074, -90.37499999999997158 ) ) ;
#35192 = EDGE_CURVE ( 'NONE', #17989, #8964, #26971, .T. ) ;
#35193 = CARTESIAN_POINT ( 'NONE',  ( 9.999999999999998224, 0.000000000000000000, -44.37500000409677625 ) ) ;
#35194 = EDGE_LOOP ( 'NONE', ( #28278, #25842, #40340, #10209 ) ) ;
#35195 = EDGE_CURVE ( 'NONE', #28029, #16950, #23745, .T. ) ;
#35196 = CARTESIAN_POINT ( 'NONE',  ( 7.644554776091147741E-16, 12.48450537969573659, -53.65625000204838102 ) ) ;
#35197 = CALENDAR_DATE ( 2026, 28, 9 ) ;
#35198 = CARTESIAN_POINT ( 'NONE',  ( 10.81189881249999907, 6.242252689847868297, -103.2187500020483810 ) ) ;
#35200 = VERTEX_POINT ( 'NONE', #31512 ) ;
#35199 = ORIENTED_EDGE ( 'NONE', *, *, #31765, .F. ) ;
#35201 = CARTESIAN_POINT ( 'NONE',  ( -99.99999999999994316, 39.99999999999999289, -170.0000000000000000 ) ) ;
#35202 = CC_DESIGN_DATE_AND_TIME_ASSIGNMENT ( #13123, #19197, ( #9061 ) ) ;
#35203 = CARTESIAN_POINT ( 'NONE',  ( 9.999999999999479527, 5.773502691896553074, -144.7500000040967620 ) ) ;
#35204 = CARTESIAN_POINT ( 'NONE',  ( -10.81189881249999729, 6.242252689847871849, -161.2187500020483526 ) ) ;
#35205 = CARTESIAN_POINT ( 'NONE',  ( -5.405949406249996869, 9.363379034771805109, -190.0312500020484094 ) ) ;
#35206 = CARTESIAN_POINT ( 'NONE',  ( -10.81189881249999907, -6.242252689847864744, -4.968750002048339276 ) ) ;
#35207 = CARTESIAN_POINT ( 'NONE',  ( 5.000000000000000000, 8.660254037844385522, -14.12500000409674961 ) ) ;
#35208 = EDGE_CURVE ( 'NONE', #17371, #4845, #20840, .T. ) ;
#35209 = CARTESIAN_POINT ( 'NONE',  ( 5.405949406249992428, -9.363379034771808662, -141.0937500020483810 ) ) ;
#35210 = CARTESIAN_POINT ( 'NONE',  ( -2.293366432827344421E-15, -12.48450537969573659, -108.2187500020483668 ) ) ;
#35211 = CARTESIAN_POINT ( 'NONE',  ( -2.121150477449813534E-15, -11.54700538379251284, -149.7500000040968189 ) ) ;
#35212 = CARTESIAN_POINT ( 'NONE',  ( -10.81189881249999729, 6.242252689847871849, -117.9062500020483952 ) ) ;
#35213 = CARTESIAN_POINT ( 'NONE',  ( -4.999999999999996447, 8.660254037844387298, -190.8750000040967905 ) ) ;
#35214 = CARTESIAN_POINT ( 'NONE',  ( -5.405949406250003975, -9.363379034771801557, -124.8437500020483810 ) ) ;
#35215 = CARTESIAN_POINT ( 'NONE',  ( 10.81189881249999729, 6.242252689847867408, -196.4062500020484094 ) ) ;
#35216 = CARTESIAN_POINT ( 'NONE',  ( 4.999999999999992006, -8.660254037844389075, -5.625000004096769146 ) ) ;
#35217 = CARTESIAN_POINT ( 'NONE',  ( -10.00000000000000000, -5.773502691896251982, -143.6250000000000000 ) ) ;
#35218 = CARTESIAN_POINT ( 'NONE',  ( -9.999999999999998224, 1.224646799147353059E-15, -16.24999999999995737 ) ) ;
#35219 = ADVANCED_FACE ( 'NONE', ( #34533 ), #30859, .T. ) ;
#35220 = CARTESIAN_POINT ( 'NONE',  ( -10.81189881249999729, 6.242252689847871849, -68.21875000204838102 ) ) ;
#35221 = CARTESIAN_POINT ( 'NONE',  ( -10.81189881249999729, 6.242252689847871849, -57.71875000204836681 ) ) ;
#35222 = CARTESIAN_POINT ( 'NONE',  ( 5.000000000000000000, 8.660254037844385522, -188.1250000040967905 ) ) ;
#35223 = CARTESIAN_POINT ( 'NONE',  ( -10.81189881249999729, 1.324075727343319199E-15, -24.78125000204836681 ) ) ;
#35224 = CARTESIAN_POINT ( 'NONE',  ( -5.405949406250003975, -9.363379034771801557, -36.34375000204836681 ) ) ;
#35225 = CARTESIAN_POINT ( 'NONE',  ( -9.999999999999998224, 1.224646799147353059E-15, -163.6250000040967905 ) ) ;
#35226 = CARTESIAN_POINT ( 'NONE',  ( -10.81189881249999907, -6.242252689847864744, -148.9687500020484094 ) ) ;
#35227 = CARTESIAN_POINT ( 'NONE',  ( -2.121150477449813534E-15, -11.54700538379251284, -114.8749999999999716 ) ) ;
#35228 = CARTESIAN_POINT ( 'NONE',  ( -2.121150477449813534E-15, -11.54700538379251284, -101.7500000040967763 ) ) ;
#35229 = CARTESIAN_POINT ( 'NONE',  ( 5.000000000000000000, 8.660254037844385522, -78.24999999999998579 ) ) ;
#35230 = CARTESIAN_POINT ( 'NONE',  ( -5.405949406250003975, -9.363379034771801557, -137.0312500020484094 ) ) ;
#35231 = CARTESIAN_POINT ( 'NONE',  ( 5.405949406249999534, 9.363379034771803333, -13.28125000204835615 ) ) ;
#35232 = ORIENTED_EDGE ( 'NONE', *, *, #34065, .F. ) ;
#35233 = CARTESIAN_POINT ( 'NONE',  ( 9.999999999999966249, 5.773502691896273298, -197.2500000040968473 ) ) ;
#35234 = CARTESIAN_POINT ( 'NONE',  ( -9.999999999999998224, 5.773502691896259087, -114.2500000040967905 ) ) ;
#35235 = FACE_OUTER_BOUND ( 'NONE', #39525, .T. ) ;
#35236 = CARTESIAN_POINT ( 'NONE',  ( -2.293366432827344421E-15, -12.48450537969573659, -73.71875000204835260 ) ) ;
#35237 = CARTESIAN_POINT ( 'NONE',  ( 10.00000000000000000, 5.773502691896255534, -43.87499999999996447 ) ) ;
#35238 = LOCAL_TIME ( 11, 57, 6.000000000000000000, #39568 ) ;
#35239 = CARTESIAN_POINT ( 'NONE',  ( -10.00000000000000000, -5.773502691896251982, -22.50000000409676915 ) ) ;
#35240 = CARTESIAN_POINT ( 'NONE',  ( -10.81189881249999729, 1.324075727343319199E-15, -50.28125000204835970 ) ) ;
#35241 = DIRECTION ( 'NONE',  ( 0.000000000000000000, -1.000000000000000000, 0.000000000000000000 ) ) ;
#35242 = CARTESIAN_POINT ( 'NONE',  ( -5.405949406249996869, 9.363379034771805109, -40.03125000204838102 ) ) ;
#35243 =( BOUNDED_CURVE ( )  B_SPLINE_CURVE ( 2, ( #27960, #30993, #37882, #14115, #24949, #18227, #27317 ),
 .UNSPECIFIED., .F., .F. ) 
 B_SPLINE_CURVE_WITH_KNOTS ( ( 3, 2, 2, 3 ),
 ( 0.007462686567164185901, 0.008706467661691551230, 0.009950248756218915691, 0.01119402985074628015 ),
 .UNSPECIFIED. ) 
 CURVE ( )  GEOMETRIC_REPRESENTATION_ITEM ( )  RATIONAL_B_SPLINE_CURVE ( ( 0.9999999999999993339, 0.8660254037844394848, 1.000000000000000000, 0.8660254037844387076, 1.000000000000000000, 0.8660254037844373753, 1.000000000000001332 ) ) 
 REPRESENTATION_ITEM ( '' )  );
#35244 = CARTESIAN_POINT ( 'NONE',  ( -9.999999999999998224, 1.224646799147353059E-15, -100.2499999999999858 ) ) ;
#35245 = CARTESIAN_POINT ( 'NONE',  ( 10.81189881249999729, 0.000000000000000000, -145.5312500020483810 ) ) ;
#35246 = CARTESIAN_POINT ( 'NONE',  ( -5.405949406250003975, -9.363379034771801557, -153.5312500020484094 ) ) ;
#35247 = CARTESIAN_POINT ( 'NONE',  ( -4.999999999999996447, 8.660254037844387298, -78.37500000409677625 ) ) ;
#35248 = CARTESIAN_POINT ( 'NONE',  ( -2.121150477449813534E-15, -11.54700538379251284, -173.7500000040968189 ) ) ;
#35249 = ORIENTED_EDGE ( 'NONE', *, *, #3677, .F. ) ;
#35250 = ORIENTED_EDGE ( 'NONE', *, *, #41333, .F. ) ;
#35251 = ORIENTED_EDGE ( 'NONE', *, *, #1114, .F. ) ;
#35252 = CARTESIAN_POINT ( 'NONE',  ( -9.999999999999742428, -5.773502691896402084, -100.5000000040967905 ) ) ;
#35253 = CARTESIAN_POINT ( 'NONE',  ( 10.81189881249999729, 0.000000000000000000, -185.8437500020483810 ) ) ;
#35254 = CC_DESIGN_APPROVAL ( #21199, ( #26987 ) ) ;
#35256 = EDGE_CURVE ( 'NONE', #15045, #37944, #15301, .T. ) ;
#35255 = CARTESIAN_POINT ( 'NONE',  ( 10.81189881249999907, 6.242252689847868297, -34.21875000204835260 ) ) ;
#35257 = FACE_OUTER_BOUND ( 'NONE', #35444, .T. ) ;
#35258 = CARTESIAN_POINT ( 'NONE',  ( 5.405949406249999534, 9.363379034771803333, -163.0937500020484094 ) ) ;
#35259 = CARTESIAN_POINT ( 'NONE',  ( -5.405949406249996869, 9.363379034771805109, -155.3437500020483810 ) ) ;
#35260 = DIRECTION ( 'NONE',  ( -0.000000000000000000, -0.000000000000000000, 1.000000000000000000 ) ) ;
#35261 = CARTESIAN_POINT ( 'NONE',  ( 5.405949406249992428, -9.363379034771808662, -133.5937500020483810 ) ) ;
#35262 = CARTESIAN_POINT ( 'NONE',  ( 5.405949406249999534, 9.363379034771803333, -140.7812500020483810 ) ) ;
#35263 = CARTESIAN_POINT ( 'NONE',  ( 80.00000000000002842, -20.00000000000001421, -170.0000000000000000 ) ) ;
#35264 = CARTESIAN_POINT ( 'NONE',  ( 7.644554776091147741E-16, 12.48450537969573659, -146.4687500020484094 ) ) ;
#35265 = CARTESIAN_POINT ( 'NONE',  ( 9.999999999999998224, 0.000000000000000000, -128.0000000000000000 ) ) ;
#35266 = CARTESIAN_POINT ( 'NONE',  ( 9.999999999999742428, 5.773502691896404748, -157.8750000000000000 ) ) ;
#35267 = CARTESIAN_POINT ( 'NONE',  ( 5.000000000000000000, 8.660254037844385522, -174.2500000000000284 ) ) ;
#35268 = CONICAL_SURFACE ( 'NONE', #19407, 42.00000000000004974, 0.7853981633974495002 ) ;
#35269 = CARTESIAN_POINT ( 'NONE',  ( -10.81189881249999729, 6.242252689847871849, -77.21875000204838102 ) ) ;
#35270 = LINE ( 'NONE', #25129, #9319 ) ;
#35271 = CARTESIAN_POINT ( 'NONE',  ( 5.405949406249992428, -9.363379034771808662, -48.28125000204838813 ) ) ;
#35272 = CARTESIAN_POINT ( 'NONE',  ( -10.44810905595974759, 0.3217275869905217300, -99.99999999999998579 ) ) ;
#35273 = CARTESIAN_POINT ( 'NONE',  ( -2.293366432827344421E-15, -12.48450537969573659, -172.7187500020484094 ) ) ;
#35274 = CARTESIAN_POINT ( 'NONE',  ( 4.999999999999992006, -8.660254037844389075, -135.7499999999999716 ) ) ;
#35275 = CARTESIAN_POINT ( 'NONE',  ( -10.81189881249999729, 1.324075727343319199E-15, -144.7812500020483810 ) ) ;
#35276 = CARTESIAN_POINT ( 'NONE',  ( 7.070501591499376803E-16, 11.54700538379251284, -143.0000000040967905 ) ) ;
#35277 = CARTESIAN_POINT ( 'NONE',  ( -5.405949406250003975, -9.363379034771801557, -33.53125000204837391 ) ) ;
#35278 = CARTESIAN_POINT ( 'NONE',  ( -10.00000000000000000, -5.773502691896251982, -124.5000000040967620 ) ) ;
#35279 = CARTESIAN_POINT ( 'NONE',  ( 9.999999999999996447, -5.773502691896262640, -98.12499999999998579 ) ) ;
#35280 = EDGE_LOOP ( 'NONE', ( #36765, #3019, #34509, #31051 ) ) ;
#35281 = CARTESIAN_POINT ( 'NONE',  ( 5.405949406249999534, 9.363379034771803333, -115.2812500020483952 ) ) ;
#35282 = CARTESIAN_POINT ( 'NONE',  ( -10.00000000000000000, -5.773502691896251982, -139.5000000040967905 ) ) ;
#35283 = CARTESIAN_POINT ( 'NONE',  ( 9.999999999999998224, 0.000000000000000000, -48.49999999999998579 ) ) ;
#35284 = CARTESIAN_POINT ( 'NONE',  ( 5.405949406249999534, 9.363379034771803333, -173.7812500020484094 ) ) ;
#35285 = CARTESIAN_POINT ( 'NONE',  ( -9.999999999999998224, 1.224646799147353059E-15, -51.12500000409675494 ) ) ;
#35286 = CARTESIAN_POINT ( 'NONE',  ( -10.00000000000051337, 5.773502691895962435, -48.25000000409676204 ) ) ;
#35287 = CARTESIAN_POINT ( 'NONE',  ( -5.405949406249996869, 9.363379034771805109, -56.53125000204836681 ) ) ;
#35288 = VECTOR ( 'NONE', #4754, 1000.000000000000000 ) ;
#35289 = DIRECTION ( 'NONE',  ( 1.000000000000000000, 0.000000000000000000, 0.000000000000000000 ) ) ;
#35290 = CARTESIAN_POINT ( 'NONE',  ( -10.81189881249999729, 6.242252689847871849, -167.4062500020483810 ) ) ;
#35291 = APPROVAL_PERSON_ORGANIZATION ( #19359, #23837, #15889 ) ;
#35292 = CARTESIAN_POINT ( 'NONE',  ( -2.121150477449813534E-15, -11.54700538379251284, -106.2500000040967905 ) ) ;
#35293 = DIRECTION ( 'NONE',  ( 1.000000000000000000, 0.000000000000000000, 0.000000000000000000 ) ) ;
#35294 = ORIENTED_EDGE ( 'NONE', *, *, #523, .T. ) ;
#35295 = DIRECTION ( 'NONE',  ( -0.000000000000000000, -0.000000000000000000, -1.000000000000000000 ) ) ;
#35296 = CYLINDRICAL_SURFACE ( 'NONE', #23834, 9.999999999999998224 ) ;
#35297 = CARTESIAN_POINT ( 'NONE',  ( 7.070501591499376803E-16, 11.54700538379251284, -27.12499999999998224 ) ) ;
#35298 = VECTOR ( 'NONE', #28394, 1000.000000000000000 ) ;
#35300 = VERTEX_POINT ( 'NONE', #27619 ) ;
#35299 = CARTESIAN_POINT ( 'NONE',  ( 7.644554776091147741E-16, 12.48450537969573659, -77.65625000204838102 ) ) ;
#35302 = VERTEX_POINT ( 'NONE', #31080 ) ;
#35301 = CARTESIAN_POINT ( 'NONE',  ( -5.000000000000003553, -8.660254037844383745, -100.3750000040967905 ) ) ;
#35303 = VERTEX_POINT ( 'NONE', #34319 ) ;
#35304 = CARTESIAN_POINT ( 'NONE',  ( 10.81189881249999729, 0.000000000000000000, -32.84375000204836681 ) ) ;
#35305 = CARTESIAN_POINT ( 'NONE',  ( -5.000000000000003553, -8.660254037844383745, -187.0000000000000000 ) ) ;
#35306 = CARTESIAN_POINT ( 'NONE',  ( -5.405949406249996869, 9.363379034771805109, -4.031250002048375691 ) ) ;
#35308 = ORIENTED_EDGE ( 'NONE', *, *, #38704, .F. ) ;
#35307 = CARTESIAN_POINT ( 'NONE',  ( -10.81189881249999729, 6.242252689847871849, -53.21875000204837391 ) ) ;
#35309 = CARTESIAN_POINT ( 'NONE',  ( -5.000000000000003553, -8.660254037844383745, -112.3750000040967763 ) ) ;
#35310 = CARTESIAN_POINT ( 'NONE',  ( -9.999999999999998224, 1.224646799147353059E-15, -37.24999999999997868 ) ) ;
#35311 = CARTESIAN_POINT ( 'NONE',  ( -10.81189881249999729, 6.242252689847871849, -191.2187500020484663 ) ) ;
#35312 = CARTESIAN_POINT ( 'NONE',  ( 5.405949406249992428, -9.363379034771808662, -180.0937500020484094 ) ) ;
#35313 = CARTESIAN_POINT ( 'NONE',  ( 7.644554776091147741E-16, 12.48450537969573659, -156.9687500020484094 ) ) ;
#35314 = VECTOR ( 'NONE', #4713, 1000.000000000000000 ) ;
#35315 = CARTESIAN_POINT ( 'NONE',  ( -5.405949406249996869, 9.363379034771805109, -173.3437500020484094 ) ) ;
#35316 = DIRECTION ( 'NONE',  ( -0.000000000000000000, -0.000000000000000000, 1.000000000000000000 ) ) ;
#35317 = CARTESIAN_POINT ( 'NONE',  ( -4.999999999999996447, 8.660254037844387298, -132.0000000000000000 ) ) ;
#35318 = CARTESIAN_POINT ( 'NONE',  ( -9.999999999999998224, 5.773502691896259087, -193.3750000000000000 ) ) ;
#35319 = CARTESIAN_POINT ( 'NONE',  ( 10.81189881249999907, 6.242252689847868297, -107.7187500020483810 ) ) ;
#35320 = FACE_OUTER_BOUND ( 'NONE', #33691, .T. ) ;
#35321 = CARTESIAN_POINT ( 'NONE',  ( 10.81189881249999907, 6.242252689847868297, -74.90625000204839523 ) ) ;
#35322 = CARTESIAN_POINT ( 'NONE',  ( -5.405949406249996869, 9.363379034771805109, -92.34375000204838102 ) ) ;
#35323 =( BOUNDED_CURVE ( )  B_SPLINE_CURVE ( 2, ( #7111, #36669, #12920, #13134, #35836, #16157, #3447 ),
 .UNSPECIFIED., .F., .F. ) 
 B_SPLINE_CURVE_WITH_KNOTS ( ( 3, 2, 2, 3 ),
 ( 0.2574626865671643117, 0.2587064676616916414, 0.2599502487562190267, 0.2611940298507463565 ),
 .UNSPECIFIED. ) 
 CURVE ( )  GEOMETRIC_REPRESENTATION_ITEM ( )  RATIONAL_B_SPLINE_CURVE ( ( 0.9999999999999880096, 0.8660254037844506980, 1.000000000000000000, 0.8660254037844387076, 1.000000000000000000, 0.8660254037844267172, 1.000000000000011990 ) ) 
 REPRESENTATION_ITEM ( '' )  );
#35324 = CARTESIAN_POINT ( 'NONE',  ( -2.293366432827344421E-15, -12.48450537969573659, -60.40625000204838813 ) ) ;
#35325 = CARTESIAN_POINT ( 'NONE',  ( 9.999999999999996447, -5.773502691896262640, -146.5000000040967905 ) ) ;
#35326 = CARTESIAN_POINT ( 'NONE',  ( -10.00000000000000000, -5.773502691896251982, -124.1250000000000000 ) ) ;
#35327 = EDGE_CURVE ( 'NONE', #18023, #36134, #17665, .T. ) ;
#35328 = ORIENTED_EDGE ( 'NONE', *, *, #37982, .F. ) ;
#35329 = CARTESIAN_POINT ( 'NONE',  ( -5.405949406249996869, 9.363379034771805109, -139.0312500020484094 ) ) ;
#35330 = CARTESIAN_POINT ( 'NONE',  ( -5.405949406249996869, 9.363379034771805109, -160.0312500020484094 ) ) ;
#35331 = CARTESIAN_POINT ( 'NONE',  ( -9.999999999999998224, 1.224646799147353059E-15, -7.249999999999978684 ) ) ;
#35332 = CARTESIAN_POINT ( 'NONE',  ( 7.070501591499376803E-16, 11.54700538379251284, -105.1249999999999858 ) ) ;
#35333 = CARTESIAN_POINT ( 'NONE',  ( 7.644554776091147741E-16, 12.48450537969573659, -86.46875000204838102 ) ) ;
#35334 = ORIENTED_EDGE ( 'NONE', *, *, #29207, .T. ) ;
#35335 = CARTESIAN_POINT ( 'NONE',  ( 7.070501591499377789E-16, 11.54700538379251284, -61.62499999999998579 ) ) ;
#35336 = CARTESIAN_POINT ( 'NONE',  ( -5.405949406250003975, -9.363379034771801557, -0.5312500020483723606 ) ) ;
#35337 = CARTESIAN_POINT ( 'NONE',  ( 4.999999999999992006, -8.660254037844389075, -71.62500000409677625 ) ) ;
#35338 = CARTESIAN_POINT ( 'NONE',  ( -2.121150477449813534E-15, -11.54700538379251284, -117.8749999999999858 ) ) ;
#35339 = CARTESIAN_POINT ( 'NONE',  ( -10.81189881249999907, -6.242252689847864744, -95.15625000204839523 ) ) ;
#35340 = CARTESIAN_POINT ( 'NONE',  ( -5.405949406249996869, 9.363379034771805109, -67.03125000204838102 ) ) ;
#35341 = CARTESIAN_POINT ( 'NONE',  ( 5.000000000000000000, 8.660254037844385522, -71.12500000409677625 ) ) ;
#35342 = DIRECTION ( 'NONE',  ( 1.000000000000000000, 0.000000000000000000, 0.000000000000000000 ) ) ;
#35343 = CARTESIAN_POINT ( 'NONE',  ( -2.293366432827344421E-15, -12.48450537969573659, -22.71875000204837391 ) ) ;
#35344 = CARTESIAN_POINT ( 'NONE',  ( -10.00000000000051337, 5.773502691895962435, -100.3750000000000000 ) ) ;
#35345 = CARTESIAN_POINT ( 'NONE',  ( 10.81189881249999551, -6.242252689847874514, -195.1562500020484379 ) ) ;
#35346 = CARTESIAN_POINT ( 'NONE',  ( -10.81189881249999729, 6.242252689847871849, -21.90625000204837391 ) ) ;
#35347 = CARTESIAN_POINT ( 'NONE',  ( -10.81189881249999729, 6.242252689847871849, -8.218750002048354375 ) ) ;
#35348 = CARTESIAN_POINT ( 'NONE',  ( -9.999999999999998224, 1.224646799147353059E-15, -111.1250000040967763 ) ) ;
#35349 = CARTESIAN_POINT ( 'NONE',  ( -5.000000000000003553, -8.660254037844383745, -62.87500000409676204 ) ) ;
#35350 = CARTESIAN_POINT ( 'NONE',  ( 5.000000000000000000, 8.660254037844385522, -175.7500000000000284 ) ) ;
#35351 = DIRECTION ( 'NONE',  ( -0.000000000000000000, -0.000000000000000000, 1.000000000000000000 ) ) ;
#35353 = ORIENTED_EDGE ( 'NONE', *, *, #31488, .F. ) ;
#35352 = CARTESIAN_POINT ( 'NONE',  ( -10.81189881249999729, 1.324075727343319199E-15, -99.78125000204839523 ) ) ;
#35354 = EDGE_CURVE ( 'NONE', #15394, #35065, #6246, .T. ) ;
#35355 = CARTESIAN_POINT ( 'NONE',  ( -4.999999999999996447, 8.660254037844387298, -115.8750000040967905 ) ) ;
#35356 = ORIENTED_EDGE ( 'NONE', *, *, #29665, .F. ) ;
#35357 = VERTEX_POINT ( 'NONE', #1731 ) ;
#35358 = CARTESIAN_POINT ( 'NONE',  ( 10.81189881249999729, 0.000000000000000000, -33.03125000204837391 ) ) ;
#35359 = COORDINATED_UNIVERSAL_TIME_OFFSET ( 6, 0, .AHEAD. ) ;
#35360 = AXIS2_PLACEMENT_3D ( 'NONE', #36855, #7298, #16132 ) ;
#35361 = CARTESIAN_POINT ( 'NONE',  ( 5.405949406249992428, -9.363379034771808662, -82.59375000204836681 ) ) ;
#35362 = CARTESIAN_POINT ( 'NONE',  ( 0.000000000000000000, 0.000000000000000000, -200.0000000000000000 ) ) ;
#35363 = CARTESIAN_POINT ( 'NONE',  ( 5.405949406249999534, 9.363379034771803333, -197.5937500020484094 ) ) ;
#35364 =( BOUNDED_CURVE ( )  B_SPLINE_CURVE ( 2, ( #2898, #25990, #36118, #6551, #32888, #23605, #10202 ),
 .UNSPECIFIED., .F., .F. ) 
 B_SPLINE_CURVE_WITH_KNOTS ( ( 3, 2, 2, 3 ),
 ( 0.5335820895522389584, 0.5348258706467662327, 0.5360696517412936180, 0.5373134328358210032 ),
 .UNSPECIFIED. ) 
 CURVE ( )  GEOMETRIC_REPRESENTATION_ITEM ( )  RATIONAL_B_SPLINE_CURVE ( ( 0.9999999999999880096, 0.8660254037844506980, 1.000000000000000000, 0.8660254037844387076, 1.000000000000000000, 0.8660254037844267172, 1.000000000000011990 ) ) 
 REPRESENTATION_ITEM ( '' )  );
#35365 = DIRECTION ( 'NONE',  ( -0.000000000000000000, -0.000000000000000000, 1.000000000000000000 ) ) ;
#35366 = CARTESIAN_POINT ( 'NONE',  ( 7.070501591499376803E-16, 11.54700538379251284, -30.50000000409674428 ) ) ;
#35367 = CARTESIAN_POINT ( 'NONE',  ( 5.405949406249992428, -9.363379034771808662, -159.2812500020484094 ) ) ;
#35368 = CARTESIAN_POINT ( 'NONE',  ( -9.999999999999998224, 5.773502691896259087, -12.25000000409677092 ) ) ;
#35369 = CARTESIAN_POINT ( 'NONE',  ( 9.999999999999998224, 0.000000000000000000, -76.99999999999998579 ) ) ;
#35370 = CARTESIAN_POINT ( 'NONE',  ( -5.405949406250003975, -9.363379034771801557, -127.8437500020483952 ) ) ;
#35371 = CARTESIAN_POINT ( 'NONE',  ( -10.81189881249999729, 1.324075727343319199E-15, -117.5937500020483810 ) ) ;
#35372 = CARTESIAN_POINT ( 'NONE',  ( -10.81189881249999907, -6.242252689847864744, -81.46875000204838102 ) ) ;
#35373 = CARTESIAN_POINT ( 'NONE',  ( -10.81189881249999729, 6.242252689847871849, -92.40625000204838102 ) ) ;
#35374 = CARTESIAN_POINT ( 'NONE',  ( 10.00000000000000000, 5.773502691896255534, -170.2500000040967905 ) ) ;
#35375 = CARTESIAN_POINT ( 'NONE',  ( 10.81189881249999729, 0.000000000000000000, -171.0312500020484094 ) ) ;
#35376 =( BOUNDED_CURVE ( )  B_SPLINE_CURVE ( 2, ( #3218, #3647, #3425, #23277, #42685, #16563, #3855 ),
 .UNSPECIFIED., .F., .F. ) 
 B_SPLINE_CURVE_WITH_KNOTS ( ( 3, 2, 2, 3 ),
 ( 0.2873134328358210032, 0.2885572139303483885, 0.2898009950248757183, 0.2910447761194031036 ),
 .UNSPECIFIED. ) 
 CURVE ( )  GEOMETRIC_REPRESENTATION_ITEM ( )  RATIONAL_B_SPLINE_CURVE ( ( 0.9999999999999880096, 0.8660254037844506980, 1.000000000000000000, 0.8660254037844387076, 1.000000000000000000, 0.8660254037844267172, 1.000000000000011990 ) ) 
 REPRESENTATION_ITEM ( '' )  );
#35377 = CARTESIAN_POINT ( 'NONE',  ( 0.000000000000000000, 0.000000000000000000, -200.0000000000000000 ) ) ;
#35378 = CARTESIAN_POINT ( 'NONE',  ( 10.81189881249999729, 6.242252689847867408, -172.4062500020484094 ) ) ;
#35379 = CARTESIAN_POINT ( 'NONE',  ( -5.405949406250003975, -9.363379034771801557, -189.5312500020484094 ) ) ;
#35380 = CARTESIAN_POINT ( 'NONE',  ( -5.405949406249996869, 9.363379034771805109, -44.34375000204837391 ) ) ;
#35381 = CARTESIAN_POINT ( 'NONE',  ( -9.999999999999998224, 1.224646799147353059E-15, -168.1250000040967905 ) ) ;
#35382 = CARTESIAN_POINT ( 'NONE',  ( -10.81189881249999729, 6.242252689847871849, -3.906250002048350822 ) ) ;
#35383 = CARTESIAN_POINT ( 'NONE',  ( -2.293366432827344421E-15, -12.48450537969573659, -10.71875000204836148 ) ) ;
#35384 = DIRECTION ( 'NONE',  ( -0.000000000000000000, -0.000000000000000000, 1.000000000000000000 ) ) ;
#35385 = CARTESIAN_POINT ( 'NONE',  ( 5.405949406249992428, -9.363379034771808662, -118.5937500020483810 ) ) ;
#35386 = EDGE_CURVE ( 'NONE', #24195, #39779, #28299, .T. ) ;
#35387 = CARTESIAN_POINT ( 'NONE',  ( -2.121150477449813534E-15, -11.54700538379251284, -92.37500000000000000 ) ) ;
#35388 = CARTESIAN_POINT ( 'NONE',  ( 10.81189881249999551, -6.242252689847874514, -16.65625000204837391 ) ) ;
#35389 = CARTESIAN_POINT ( 'NONE',  ( 4.999999999999992006, -8.660254037844389075, -101.6250000040967905 ) ) ;
#35390 = LINE ( 'NONE', #22000, #5202 ) ;
#35391 = CARTESIAN_POINT ( 'NONE',  ( -10.81189881249999729, 1.324075727343319199E-15, -116.2812500020483952 ) ) ;
#35392 = CARTESIAN_POINT ( 'NONE',  ( -10.81189881249999729, 6.242252689847871849, -90.90625000204838102 ) ) ;
#35393 = ORIENTED_EDGE ( 'NONE', *, *, #27477, .F. ) ;
#35394 = CARTESIAN_POINT ( 'NONE',  ( 4.999999999999992006, -8.660254037844389075, -92.62500000409677625 ) ) ;
#35395 = CARTESIAN_POINT ( 'NONE',  ( 7.070501591499376803E-16, 11.54700538379251284, -72.12499999999995737 ) ) ;
#35396 = CARTESIAN_POINT ( 'NONE',  ( -2.293366432827344421E-15, -12.48450537969573659, -159.4062500020483810 ) ) ;
#35397 = CARTESIAN_POINT ( 'NONE',  ( 10.81189881249999907, 6.242252689847868297, -52.21875000204837391 ) ) ;
#35398 = VERTEX_POINT ( 'NONE', #40968 ) ;
#35399 = CARTESIAN_POINT ( 'NONE',  ( -5.000000000000003553, -8.660254037844383745, -17.49999999999996092 ) ) ;
#35400 = CARTESIAN_POINT ( 'NONE',  ( 10.81189881249999729, 6.242252689847867408, -23.90625000204838102 ) ) ;
#35401 = CARTESIAN_POINT ( 'NONE',  ( -10.00000000000000000, -5.773502691896251982, -155.6249999999999716 ) ) ;
#35402 = CARTESIAN_POINT ( 'NONE',  ( 10.00000000000000000, 5.773502691896255534, -21.75000000409676915 ) ) ;
#35403 = CARTESIAN_POINT ( 'NONE',  ( -4.999999999999996447, 8.660254037844387298, -198.0000000000000000 ) ) ;
#35405 = ORIENTED_EDGE ( 'NONE', *, *, #27279, .F. ) ;
#35404 = CARTESIAN_POINT ( 'NONE',  ( 10.81189881249999729, 0.000000000000000000, -129.0312500020484094 ) ) ;
#35406 = CARTESIAN_POINT ( 'NONE',  ( 9.999999999999998224, 0.000000000000000000, -152.0000000000000000 ) ) ;
#35407 = VERTEX_POINT ( 'NONE', #37973 ) ;
#35408 = CARTESIAN_POINT ( 'NONE',  ( 5.405949406249992428, -9.363379034771808662, -55.78125000204836681 ) ) ;
#35409 = PERSON_AND_ORGANIZATION ( #11915, #17965 ) ;
#35410 = CARTESIAN_POINT ( 'NONE',  ( 10.81189881249999551, -6.242252689847874514, -103.4687500020483810 ) ) ;
#35412 = ORIENTED_EDGE ( 'NONE', *, *, #24647, .F. ) ;
#35411 = ORIENTED_EDGE ( 'NONE', *, *, #29931, .T. ) ;
#35413 = DIRECTION ( 'NONE',  ( -0.000000000000000000, -0.000000000000000000, 1.000000000000000000 ) ) ;
#35414 = LINE ( 'NONE', #18574, #11109 ) ;
#35415 = CARTESIAN_POINT ( 'NONE',  ( -5.405949406250003975, -9.363379034771801557, -156.3437500020483810 ) ) ;
#35416 = CARTESIAN_POINT ( 'NONE',  ( 10.81189881249999729, 0.000000000000000000, -177.0312500020483810 ) ) ;
#35417 = CARTESIAN_POINT ( 'NONE',  ( 5.405949406249992428, -9.363379034771808662, -10.59375000204834727 ) ) ;
#35418 = CYLINDRICAL_SURFACE ( 'NONE', #19032, 9.999999999999998224 ) ;
#35419 = CARTESIAN_POINT ( 'NONE',  ( -10.81189881249999729, -6.242252689847864744, -139.9687500020483810 ) ) ;
#35420 = CARTESIAN_POINT ( 'NONE',  ( 10.81189881249999551, -6.242252689847874514, -107.9687500020483810 ) ) ;
#35421 = CARTESIAN_POINT ( 'NONE',  ( 0.000000000000000000, 0.000000000000000000, -200.0000000000000000 ) ) ;
#35422 = CARTESIAN_POINT ( 'NONE',  ( 7.644554776091147741E-16, 12.48450537969573659, -113.6562500020483952 ) ) ;
#35423 = CARTESIAN_POINT ( 'NONE',  ( -9.999999999999998224, 5.773502691896259087, -196.7500000040968189 ) ) ;
#35424 = CARTESIAN_POINT ( 'NONE',  ( -5.405949406249996869, 9.363379034771805109, -120.8437500020483952 ) ) ;
#35425 = CARTESIAN_POINT ( 'NONE',  ( 5.405949406249992428, -9.363379034771808662, -192.2812500020484094 ) ) ;
#35426 = CARTESIAN_POINT ( 'NONE',  ( 7.070501591499376803E-16, 11.54700538379251284, -157.6250000000000284 ) ) ;
#35427 = CARTESIAN_POINT ( 'NONE',  ( -5.000000000000003553, -8.660254037844383745, -137.5000000000000000 ) ) ;
#35428 = CARTESIAN_POINT ( 'NONE',  ( 4.999999999999992006, -8.660254037844389075, -11.24999999999995381 ) ) ;
#35429 = CARTESIAN_POINT ( 'NONE',  ( -10.81189881249999729, -6.242252689847864744, -69.46875000204838102 ) ) ;
#35430 = CARTESIAN_POINT ( 'NONE',  ( -5.405949406250003975, -9.363379034771801557, -58.84375000204835970 ) ) ;
#35431 = CARTESIAN_POINT ( 'NONE',  ( 4.999999999999992006, -8.660254037844389075, -187.1250000040967905 ) ) ;
#35432 = CARTESIAN_POINT ( 'NONE',  ( -10.81189881249999907, -6.242252689847864744, -26.15625000204837391 ) ) ;
#35433 = CARTESIAN_POINT ( 'NONE',  ( 10.81189881249999551, -6.242252689847874514, -38.96875000204835970 ) ) ;
#35434 = LINE ( 'NONE', #12938, #8874 ) ;
#35435 = CARTESIAN_POINT ( 'NONE',  ( 5.405949406249992428, -9.363379034771808662, -150.0937500020483810 ) ) ;
#35436 = ADVANCED_FACE ( 'NONE', ( #28054 ), #5385, .F. ) ;
#35437 = CARTESIAN_POINT ( 'NONE',  ( -9.999999999999998224, 1.224646799147353059E-15, -110.7499999999999858 ) ) ;
#35438 = CARTESIAN_POINT ( 'NONE',  ( -10.00000000000000000, -5.773502691896252870, -170.6249999999999716 ) ) ;
#35439 = EDGE_CURVE ( 'NONE', #29342, #23818, #3216, .T. ) ;
#35440 = CARTESIAN_POINT ( 'NONE',  ( 9.999999999999998224, 0.000000000000000000, -64.99999999999997158 ) ) ;
#35441 = CARTESIAN_POINT ( 'NONE',  ( -10.81189881249999729, 1.324075727343319199E-15, -138.7812500020483810 ) ) ;
#35442 = CARTESIAN_POINT ( 'NONE',  ( 7.644554776091147741E-16, 12.48450537969573659, -13.15625000204836326 ) ) ;
#35443 = ADVANCED_FACE ( 'NONE', ( #21568 ), #34749, .T. ) ;
#35444 = EDGE_LOOP ( 'NONE', ( #35879, #23161, #9856, #27210 ) ) ;
#35445 = CARTESIAN_POINT ( 'NONE',  ( 5.000000000000000000, 8.660254037844385522, -197.1250000040967905 ) ) ;
#35446 = CARTESIAN_POINT ( 'NONE',  ( -9.999999999999998224, 1.224646799147353059E-15, -115.6250000040967905 ) ) ;
#35447 = FACE_OUTER_BOUND ( 'NONE', #9982, .T. ) ;
#35448 = CARTESIAN_POINT ( 'NONE',  ( 7.644554776091147741E-16, 12.48450537969573659, -74.46875000204838102 ) ) ;
#35449 = CARTESIAN_POINT ( 'NONE',  ( 7.070501591499377789E-16, 11.54700538379251284, -40.62499999999997158 ) ) ;
#35450 = CARTESIAN_POINT ( 'NONE',  ( -9.999999999999998224, 1.224646799147353059E-15, -28.62500000409676204 ) ) ;
#35451 = CARTESIAN_POINT ( 'NONE',  ( 7.644554776091147741E-16, 12.48450537969573659, -55.15625000204837391 ) ) ;
#35452 =( BOUNDED_CURVE ( )  B_SPLINE_CURVE ( 2, ( #34004, #7032, #37218, #19969, #23653, #7665, #30765 ),
 .UNSPECIFIED., .F., .F. ) 
 B_SPLINE_CURVE_WITH_KNOTS ( ( 3, 2, 2, 3 ),
 ( 0.2313432835820896372, 0.2325870646766169947, 0.2338308457711443245, 0.2350746268656717097 ),
 .UNSPECIFIED. ) 
 CURVE ( )  GEOMETRIC_REPRESENTATION_ITEM ( )  RATIONAL_B_SPLINE_CURVE ( ( 0.9999999999999910072, 0.8660254037844477004, 1.000000000000000000, 0.8660254037844387076, 1.000000000000000000, 0.8660254037844327124, 1.000000000000005995 ) ) 
 REPRESENTATION_ITEM ( '' )  );
#35453 = CARTESIAN_POINT ( 'NONE',  ( 7.070501591499376803E-16, 11.54700538379251284, -119.0000000040967763 ) ) ;
#35454 = CC_DESIGN_DATE_AND_TIME_ASSIGNMENT ( #10695, #9859, ( #16278 ) ) ;
#35455 = CARTESIAN_POINT ( 'NONE',  ( -10.81189881249999729, 6.242252689847871849, -38.40625000204835970 ) ) ;
#35456 = CARTESIAN_POINT ( 'NONE',  ( -4.999999999999996447, 8.660254037844387298, -23.99999999999996447 ) ) ;
#35457 = CARTESIAN_POINT ( 'NONE',  ( 10.81189881249999907, 6.242252689847868297, -145.4062500020484094 ) ) ;
#35458 = CARTESIAN_POINT ( 'NONE',  ( 7.644554776091147741E-16, 12.48450537969573659, -149.6562500020484094 ) ) ;
#35459 = CARTESIAN_POINT ( 'NONE',  ( 10.00000000000012257, -5.773502691896187144, -164.5000000040967905 ) ) ;
#35460 = ADVANCED_FACE ( 'NONE', ( #15708 ), #39448, .T. ) ;
#35461 = ORIENTED_EDGE ( 'NONE', *, *, #11998, .F. ) ;
#35462 = EDGE_CURVE ( 'NONE', #24467, #27698, #25282, .T. ) ;
#35463 = VERTEX_POINT ( 'NONE', #32571 ) ;
#35464 = EDGE_LOOP ( 'NONE', ( #11331, #10271 ) ) ;
#35465 = EDGE_CURVE ( 'NONE', #29936, #5836, #9010, .T. ) ;
#35466 = DIRECTION ( 'NONE',  ( 0.000000000000000000, 1.000000000000000000, 0.000000000000000000 ) ) ;
#35467 = CARTESIAN_POINT ( 'NONE',  ( 5.405949406249992428, -9.363379034771808662, -183.0937500020483810 ) ) ;
#35468 = CARTESIAN_POINT ( 'NONE',  ( 5.405949406249992428, -9.363379034771808662, -33.09375000204836681 ) ) ;
#35469 = DIRECTION ( 'NONE',  ( -0.000000000000000000, -0.000000000000000000, 1.000000000000000000 ) ) ;
#35470 = CARTESIAN_POINT ( 'NONE',  ( 10.81189881249999729, 6.242252689847867408, -163.2187500020483810 ) ) ;
#35471 = CARTESIAN_POINT ( 'NONE',  ( -5.405949406250003975, -9.363379034771801557, -154.8437500020483810 ) ) ;
#35472 = CARTESIAN_POINT ( 'NONE',  ( -9.999999999999998224, 1.224646799147353059E-15, -147.1250000040967905 ) ) ;
#35473 = CARTESIAN_POINT ( 'NONE',  ( -5.405949406250003975, -9.363379034771801557, -133.8437500020484094 ) ) ;
#35474 = CARTESIAN_POINT ( 'NONE',  ( -5.405949406250003975, -9.363379034771801557, -144.5312500020483810 ) ) ;
#35475 = CARTESIAN_POINT ( 'NONE',  ( 5.405949406249992428, -9.363379034771808662, -18.09375000204835260 ) ) ;
#35476 = CARTESIAN_POINT ( 'NONE',  ( -10.81189881249999729, 1.324075727343319199E-15, -147.5937500020483810 ) ) ;
#35477 = CARTESIAN_POINT ( 'NONE',  ( 4.999999999999992006, -8.660254037844389075, -152.2500000000000000 ) ) ;
#35478 = CARTESIAN_POINT ( 'NONE',  ( -9.999999999999804601, 5.773502691896371886, -177.2500000040967905 ) ) ;
#35479 = CARTESIAN_POINT ( 'NONE',  ( 5.000000000000000000, 8.660254037844385522, -162.2500000000000000 ) ) ;
#35480 = CARTESIAN_POINT ( 'NONE',  ( 10.81189881249999907, 6.242252689847868297, -82.21875000204836681 ) ) ;
#35481 = CARTESIAN_POINT ( 'NONE',  ( 4.999999999999992006, -8.660254037844389075, -114.7499999999999858 ) ) ;
#35482 = CARTESIAN_POINT ( 'NONE',  ( -2.293366432827344421E-15, -12.48450537969573659, -46.90625000204836681 ) ) ;
#35483 = CARTESIAN_POINT ( 'NONE',  ( 10.81189881249999907, 6.242252689847868297, -64.21875000204838102 ) ) ;
#35484 = CARTESIAN_POINT ( 'NONE',  ( 4.999999999999992006, -8.660254037844389075, -16.12500000409675138 ) ) ;
#35485 = CARTESIAN_POINT ( 'NONE',  ( -10.81189881249999729, 1.324075727343319199E-15, -171.5937500020484094 ) ) ;
#35486 = CARTESIAN_POINT ( 'NONE',  ( -9.999999999999998224, 5.773502691896259087, -134.8750000000000000 ) ) ;
#35487 = CARTESIAN_POINT ( 'NONE',  ( -5.405949406249996869, 9.363379034771805109, -148.0312500020483810 ) ) ;
#35488 = CARTESIAN_POINT ( 'NONE',  ( 0.000000000000000000, 0.000000000000000000, -236.9999999999999716 ) ) ;
#35489 = CARTESIAN_POINT ( 'NONE',  ( 5.405949406249992428, -9.363379034771808662, -37.78125000204838102 ) ) ;
#35490 = CARTESIAN_POINT ( 'NONE',  ( -9.999999999999998224, 5.773502691896259087, -120.2500000040967763 ) ) ;
#35491 = CARTESIAN_POINT ( 'NONE',  ( 9.999999999999996447, -5.773502691896262640, -96.62500000000000000 ) ) ;
#35492 =( BOUNDED_CURVE ( )  B_SPLINE_CURVE ( 2, ( #17161, #29721, #26475, #39838, #20202, #39622, #6830 ),
 .UNSPECIFIED., .F., .F. ) 
 B_SPLINE_CURVE_WITH_KNOTS ( ( 3, 2, 2, 3 ),
 ( 0.1865671641791045166, 0.1878109452736318741, 0.1890547263681592594, 0.1902985074626866169 ),
 .UNSPECIFIED. ) 
 CURVE ( )  GEOMETRIC_REPRESENTATION_ITEM ( )  RATIONAL_B_SPLINE_CURVE ( ( 0.9999999999999970024, 0.8660254037844417052, 1.000000000000000000, 0.8660254037844387076, 1.000000000000000000, 0.8660254037844327124, 1.000000000000005995 ) ) 
 REPRESENTATION_ITEM ( '' )  );
#35493 = EDGE_CURVE ( 'NONE', #7848, #33176, #32702, .T. ) ;
#35494 = ORIENTED_EDGE ( 'NONE', *, *, #14322, .F. ) ;
#35495 = CARTESIAN_POINT ( 'NONE',  ( -2.293366432827344421E-15, -12.48450537969573659, -115.9062500020483952 ) ) ;
#35496 = CARTESIAN_POINT ( 'NONE',  ( 7.070501591499377789E-16, 11.54700538379251284, -137.0000000040967905 ) ) ;
#35497 = CARTESIAN_POINT ( 'NONE',  ( -10.00000000000012434, 5.773502691896184480, -158.8750000000000000 ) ) ;
#35498 = CARTESIAN_POINT ( 'NONE',  ( 5.405949406249992428, -9.363379034771808662, -172.7812500020484094 ) ) ;
#35499 = CARTESIAN_POINT ( 'NONE',  ( 4.999999999999992006, -8.660254037844389075, -52.12500000409675494 ) ) ;
#35500 = DIRECTION ( 'NONE',  ( -0.000000000000000000, -0.000000000000000000, 1.000000000000000000 ) ) ;
#35501 = CARTESIAN_POINT ( 'NONE',  ( 7.644554776091147741E-16, 12.48450537969573659, -59.65625000204838102 ) ) ;
#35502 = CIRCLE ( 'NONE', #3110, 42.00000000000004974 ) ;
#35503 = CARTESIAN_POINT ( 'NONE',  ( 9.999999999999479527, 5.773502691896553074, -147.7500000040967620 ) ) ;
#35504 = CARTESIAN_POINT ( 'NONE',  ( 5.405949406249992428, -9.363379034771808662, -169.7812500020484094 ) ) ;
#35505 = CARTESIAN_POINT ( 'NONE',  ( -2.121150477449813534E-15, -11.54700538379251284, -162.8750000000000000 ) ) ;
#35506 = CARTESIAN_POINT ( 'NONE',  ( -9.999999999999998224, 1.224646799147353059E-15, -64.24999999999997158 ) ) ;
#35507 = ORIENTED_EDGE ( 'NONE', *, *, #22283, .T. ) ;
#35508 = CARTESIAN_POINT ( 'NONE',  ( -2.121150477449813534E-15, -11.54700538379251284, -52.25000000409676915 ) ) ;
#35509 = EDGE_CURVE ( 'NONE', #12293, #29936, #41517, .T. ) ;
#35510 = CYLINDRICAL_SURFACE ( 'NONE', #28264, 9.999999999999998224 ) ;
#35512 = EDGE_LOOP ( 'NONE', ( #42067, #11322, #40940, #27966 ) ) ;
#35511 = CARTESIAN_POINT ( 'NONE',  ( 10.81189881249999729, 0.000000000000000000, -79.53125000204838102 ) ) ;
#35513 =( LENGTH_UNIT ( ) NAMED_UNIT ( * ) SI_UNIT ( .MILLI., .METRE. ) );
#35515 = VERTEX_POINT ( 'NONE', #25873 ) ;
#35514 = CARTESIAN_POINT ( 'NONE',  ( -9.999999999999998224, 1.224646799147353059E-15, -119.7500000000000000 ) ) ;
#35516 = ORIENTED_EDGE ( 'NONE', *, *, #34124, .F. ) ;
#35517 = CARTESIAN_POINT ( 'NONE',  ( -2.293366432827344421E-15, -12.48450537969573659, -27.21875000204838102 ) ) ;
#35518 = CYLINDRICAL_SURFACE ( 'NONE', #22473, 45.00000000000000711 ) ;
#35519 = CARTESIAN_POINT ( 'NONE',  ( -5.405949406249996869, 9.363379034771805109, -7.031250002048378356 ) ) ;
#35521 = VERTEX_POINT ( 'NONE', #2579 ) ;
#35520 = CARTESIAN_POINT ( 'NONE',  ( 7.644554776091147741E-16, 12.48450537969573659, -54.96875000204836681 ) ) ;
#35522 = CARTESIAN_POINT ( 'NONE',  ( -4.999999999999996447, 8.660254037844387298, -28.49999999999997158 ) ) ;
#35523 = CARTESIAN_POINT ( 'NONE',  ( 9.999999999999998224, 0.000000000000000000, -30.49999999999997158 ) ) ;
#35524 = CARTESIAN_POINT ( 'NONE',  ( 10.81189881249999729, 6.242252689847867408, -185.7187500020484094 ) ) ;
#35525 = CARTESIAN_POINT ( 'NONE',  ( -10.81189881249999907, -6.242252689847864744, -177.4687500020484094 ) ) ;
#35526 = CARTESIAN_POINT ( 'NONE',  ( 5.405949406249992428, -9.363379034771808662, -154.5937500020483810 ) ) ;
#35527 = CARTESIAN_POINT ( 'NONE',  ( 5.405949406249999534, 9.363379034771803333, -167.5937500020484094 ) ) ;
#35528 = CARTESIAN_POINT ( 'NONE',  ( -4.999999999999996447, 8.660254037844387298, -40.87500000409677625 ) ) ;
#35529 = CYLINDRICAL_SURFACE ( 'NONE', #30894, 9.999999999999998224 ) ;
#35530 = CARTESIAN_POINT ( 'NONE',  ( -2.121150477449813534E-15, -11.54700538379251284, -192.8750000000000284 ) ) ;
#35531 = CARTESIAN_POINT ( 'NONE',  ( -10.81189881249999907, -6.242252689847864744, -108.4687500020483810 ) ) ;
#35532 = DIRECTION ( 'NONE',  ( -1.000000000000000000, 0.000000000000000000, 0.000000000000000000 ) ) ;
#35533 = CARTESIAN_POINT ( 'NONE',  ( 10.81189881249999729, 0.000000000000000000, -72.03125000204838102 ) ) ;
#35534 = CARTESIAN_POINT ( 'NONE',  ( 10.81189881249999729, 6.242252689847867408, -86.71875000204836681 ) ) ;
#35535 = CARTESIAN_POINT ( 'NONE',  ( -10.81189881249999729, 6.242252689847871849, -60.90625000204837391 ) ) ;
#35536 = CARTESIAN_POINT ( 'NONE',  ( 10.00000000000000000, 5.773502691896255534, -147.7500000040967905 ) ) ;
#35537 = CARTESIAN_POINT ( 'NONE',  ( 10.00000000000000000, 5.773502691896255534, -121.8750000000000000 ) ) ;
#35538 = VERTEX_POINT ( 'NONE', #35171 ) ;
#35539 = CARTESIAN_POINT ( 'NONE',  ( -5.405949406249996869, 9.363379034771805109, -143.5312500020483810 ) ) ;
#35540 = CARTESIAN_POINT ( 'NONE',  ( -2.293366432827344421E-15, -12.48450537969573659, -157.9062500020483810 ) ) ;
#35541 = FACE_OUTER_BOUND ( 'NONE', #24206, .T. ) ;
#35542 = CARTESIAN_POINT ( 'NONE',  ( -9.999999999999998224, 1.224646799147353059E-15, -52.24999999999996447 ) ) ;
#35543 = CARTESIAN_POINT ( 'NONE',  ( -10.81189881249999729, 6.242252689847871849, -93.71875000204838102 ) ) ;
#35544 = ORIENTED_EDGE ( 'NONE', *, *, #25190, .T. ) ;
#35545 = CARTESIAN_POINT ( 'NONE',  ( -2.121150477449813534E-15, -11.54700538379251284, -65.37499999999998579 ) ) ;
#35546 = CARTESIAN_POINT ( 'NONE',  ( 5.405949406249999534, 9.363379034771803333, -187.0937500020483810 ) ) ;
#35547 = CARTESIAN_POINT ( 'NONE',  ( -5.000000000000003553, -8.660254037844383745, -70.37500000409677625 ) ) ;
#35548 = CARTESIAN_POINT ( 'NONE',  ( -9.999999999999998224, 1.224646799147353059E-15, -65.74999999999997158 ) ) ;
#35549 = CARTESIAN_POINT ( 'NONE',  ( 10.00000000000051159, -5.773502691895965988, -123.6250000000000142 ) ) ;
#35550 = CARTESIAN_POINT ( 'NONE',  ( 10.81189881249999729, 0.000000000000000000, -87.03125000204838102 ) ) ;
#35551 = AXIS2_PLACEMENT_3D ( 'NONE', #19756, #33156, #39399 ) ;
#35552 = CARTESIAN_POINT ( 'NONE',  ( -10.81189881249999729, -6.242252689847864744, -68.15625000204840944 ) ) ;
#35553 = CARTESIAN_POINT ( 'NONE',  ( 10.00000000000000000, 5.773502691896255534, -56.25000000409676915 ) ) ;
#35554 = CARTESIAN_POINT ( 'NONE',  ( -9.999999999999998224, 1.224646799147353059E-15, -93.12500000409677625 ) ) ;
#35555 = CARTESIAN_POINT ( 'NONE',  ( 5.405949406249992428, -9.363379034771808662, -15.09375000204835082 ) ) ;
#35556 = ORIENTED_EDGE ( 'NONE', *, *, #24377, .F. ) ;
#35557 = CARTESIAN_POINT ( 'NONE',  ( -10.81189881249999907, -6.242252689847864744, -191.1562500020484094 ) ) ;
#35558 = EDGE_CURVE ( 'NONE', #30518, #2913, #18333, .T. ) ;
#35559 = CARTESIAN_POINT ( 'NONE',  ( 10.81189881249999729, 0.000000000000000000, -18.03125000204835970 ) ) ;
#35560 = CARTESIAN_POINT ( 'NONE',  ( -5.405949406249996869, 9.363379034771805109, -3.843750002048368586 ) ) ;
#35561 = CARTESIAN_POINT ( 'NONE',  ( -4.999999999999996447, 8.660254037844387298, -186.3750000040967905 ) ) ;
#35562 = CARTESIAN_POINT ( 'NONE',  ( 7.070501591499377789E-16, 11.54700538379251284, 0.9999999959032501717 ) ) ;
#35563 = CARTESIAN_POINT ( 'NONE',  ( -9.999999999999998224, 1.224646799147353059E-15, -44.74999999999998579 ) ) ;
#35564 = CARTESIAN_POINT ( 'NONE',  ( -9.999999999999998224, 1.224646799147353059E-15, -178.2500000000000284 ) ) ;
#35565 = DIRECTION ( 'NONE',  ( -0.000000000000000000, -0.000000000000000000, 1.000000000000000000 ) ) ;
#35567 = VERTEX_POINT ( 'NONE', #6023 ) ;
#35566 = CARTESIAN_POINT ( 'NONE',  ( -2.293366432827344421E-15, -12.48450537969573659, -100.9062500020483952 ) ) ;
#35568 = CARTESIAN_POINT ( 'NONE',  ( 7.070501591499376803E-16, 11.54700538379251284, -116.0000000040967905 ) ) ;
#35569 = ORIENTED_EDGE ( 'NONE', *, *, #27910, .T. ) ;
#35570 = ORIENTED_EDGE ( 'NONE', *, *, #6673, .T. ) ;
#35571 = EDGE_CURVE ( 'NONE', #17005, #15077, #29676, .T. ) ;
#35572 = CARTESIAN_POINT ( 'NONE',  ( -5.405949406250003975, -9.363379034771801557, -32.03125000204837391 ) ) ;
#35573 = CARTESIAN_POINT ( 'NONE',  ( -10.81189881249999729, 1.324075727343319199E-15, -83.09375000204836681 ) ) ;
#35574 = DIRECTION ( 'NONE',  ( -0.000000000000000000, -0.000000000000000000, 1.000000000000000000 ) ) ;
#35575 =( BOUNDED_CURVE ( )  B_SPLINE_CURVE ( 2, ( #37879, #27957, #10892, #24511, #14110, #27099, #40241 ),
 .UNSPECIFIED., .F., .F. ) 
 B_SPLINE_CURVE_WITH_KNOTS ( ( 3, 2, 2, 3 ),
 ( 0.5522388059701495155, 0.5534825870646767898, 0.5547263681592041751, 0.5559701492537315604 ),
 .UNSPECIFIED. ) 
 CURVE ( )  GEOMETRIC_REPRESENTATION_ITEM ( )  RATIONAL_B_SPLINE_CURVE ( ( 0.9999999999999761302, 0.8660254037844625774, 1.000000000000000000, 0.8660254037844387076, 1.000000000000000000, 0.8660254037844148378, 1.000000000000023981 ) ) 
 REPRESENTATION_ITEM ( '' )  );
#35576 = VECTOR ( 'NONE', #35130, 1000.000000000000000 ) ;
#35577 = CARTESIAN_POINT ( 'NONE',  ( 9.999999999998969713, 5.773502691896851502, -30.75000000409672651 ) ) ;
#35578 = CARTESIAN_POINT ( 'NONE',  ( -10.81189881249999907, -6.242252689847864744, -159.6562500020484094 ) ) ;
#35579 = CARTESIAN_POINT ( 'NONE',  ( 7.070501591499377789E-16, 11.54700538379251284, -14.00000000409676382 ) ) ;
#35580 = CARTESIAN_POINT ( 'NONE',  ( 0.000000000000000000, 0.000000000000000000, -200.0000000000000000 ) ) ;
#35581 = CARTESIAN_POINT ( 'NONE',  ( -2.293366432827344421E-15, -12.48450537969573659, -129.2187500020483810 ) ) ;
#35582 = CARTESIAN_POINT ( 'NONE',  ( 7.644554776091147741E-16, 12.48450537969573659, -101.6562500020483952 ) ) ;
#35583 = CARTESIAN_POINT ( 'NONE',  ( 10.81189881249999551, -6.242252689847874514, -119.9687500020483952 ) ) ;
#35584 = AXIS2_PLACEMENT_3D ( 'NONE', #16688, #34193, #37187 ) ;
#35585 = CARTESIAN_POINT ( 'NONE',  ( 7.644554776091147741E-16, 12.48450537969573659, -74.46875000204838102 ) ) ;
#35586 = CARTESIAN_POINT ( 'NONE',  ( 10.81189881249999907, 6.242252689847868297, -83.90625000204836681 ) ) ;
#35587 = CARTESIAN_POINT ( 'NONE',  ( 5.000000000000000000, 8.660254037844385522, -170.1250000040968189 ) ) ;
#35588 = FACE_OUTER_BOUND ( 'NONE', #22239, .T. ) ;
#35589 = CARTESIAN_POINT ( 'NONE',  ( 10.81189881249999551, -6.242252689847874514, -163.6562500020484094 ) ) ;
#35590 = CARTESIAN_POINT ( 'NONE',  ( 5.405949406249992428, -9.363379034771808662, -178.7812500020484094 ) ) ;
#35591 = CARTESIAN_POINT ( 'NONE',  ( 10.81189881249999729, 0.000000000000000000, -44.84375000204837391 ) ) ;
#35592 = CARTESIAN_POINT ( 'NONE',  ( 7.070501591499377789E-16, 11.54700538379251284, -159.5000000040967905 ) ) ;
#35593 = CARTESIAN_POINT ( 'NONE',  ( 10.81189881249999907, 6.242252689847868297, -2.906250002048345937 ) ) ;
#35594 = CARTESIAN_POINT ( 'NONE',  ( 10.81189881249999907, 6.242252689847868297, -5.718750002048356151 ) ) ;
#35595 = LINE ( 'NONE', #19173, #24061 ) ;
#35596 = CARTESIAN_POINT ( 'NONE',  ( 10.81189881249999729, 0.000000000000000000, -110.8437500020483810 ) ) ;
#35597 = CARTESIAN_POINT ( 'NONE',  ( -2.121150477449813534E-15, -11.54700538379251284, -90.87499999999997158 ) ) ;
#35598 = CARTESIAN_POINT ( 'NONE',  ( 7.644554776091147741E-16, 12.48450537969573659, -8.656250002048365033 ) ) ;
#35599 = CARTESIAN_POINT ( 'NONE',  ( -10.00000000000000000, -5.773502691896251982, -96.00000000409679046 ) ) ;
#35600 = DIRECTION ( 'NONE',  ( -0.000000000000000000, -0.000000000000000000, 1.000000000000000000 ) ) ;
#35601 = CARTESIAN_POINT ( 'NONE',  ( -5.405949406250003975, -9.363379034771801557, -108.5312500020483810 ) ) ;
#35602 = CARTESIAN_POINT ( 'NONE',  ( 10.81189881249999729, 0.000000000000000000, -88.53125000204838102 ) ) ;
#35603 = EDGE_LOOP ( 'NONE', ( #37336, #16097, #7052, #25982 ) ) ;
#35604 = EDGE_CURVE ( 'NONE', #34874, #35982, #35595, .T. ) ;
#35605 = CARTESIAN_POINT ( 'NONE',  ( -9.999999999999998224, 1.224646799147353059E-15, -93.12500000409677625 ) ) ;
#35606 = FACE_OUTER_BOUND ( 'NONE', #1369, .T. ) ;
#35607 = CARTESIAN_POINT ( 'NONE',  ( -2.293366432827344421E-15, -12.48450537969573659, -43.71875000204835970 ) ) ;
#35608 = ORIENTED_EDGE ( 'NONE', *, *, #34791, .F. ) ;
#35609 = CARTESIAN_POINT ( 'NONE',  ( -5.000000000000003553, -8.660254037844383745, -14.49999999999995737 ) ) ;
#35610 = CARTESIAN_POINT ( 'NONE',  ( 5.405949406249992428, -9.363379034771808662, -22.78125000204836326 ) ) ;
#35611 = CARTESIAN_POINT ( 'NONE',  ( 5.000000000000000000, 8.660254037844385522, -153.2500000000000000 ) ) ;
#35612 = CARTESIAN_POINT ( 'NONE',  ( -9.999999999999998224, 1.224646799147353059E-15, -19.62500000409675494 ) ) ;
#35613 = CARTESIAN_POINT ( 'NONE',  ( 5.000000000000000000, 8.660254037844385522, -195.2500000000000000 ) ) ;
#35615 = ORIENTED_EDGE ( 'NONE', *, *, #22537, .F. ) ;
#35614 = CARTESIAN_POINT ( 'NONE',  ( 10.81189881249999551, -6.242252689847874514, -123.1562500020483952 ) ) ;
#35616 = ORIENTED_EDGE ( 'NONE', *, *, #24908, .F. ) ;
#35617 =( BOUNDED_CURVE ( )  B_SPLINE_CURVE ( 2, ( #262, #37124, #23981, #26575, #36494, #20722, #13593 ),
 .UNSPECIFIED., .F., .F. ) 
 B_SPLINE_CURVE_WITH_KNOTS ( ( 3, 2, 2, 3 ),
 ( 0.8134328358208956500, 0.8146766169154230353, 0.8159203980099504205, 0.8171641791044778058 ),
 .UNSPECIFIED. ) 
 CURVE ( )  GEOMETRIC_REPRESENTATION_ITEM ( )  RATIONAL_B_SPLINE_CURVE ( ( 0.9999999999999880096, 0.8660254037844506980, 1.000000000000000000, 0.8660254037844387076, 1.000000000000000000, 0.8660254037844148378, 1.000000000000023981 ) ) 
 REPRESENTATION_ITEM ( '' )  );
#35618 = CARTESIAN_POINT ( 'NONE',  ( 10.81189881249999551, -6.242252689847874514, -51.15625000204838813 ) ) ;
#35619 = COORDINATED_UNIVERSAL_TIME_OFFSET ( 6, 0, .AHEAD. ) ;
#35620 = CARTESIAN_POINT ( 'NONE',  ( 5.405949406249992428, -9.363379034771808662, -105.0937500020483810 ) ) ;
#35621 = EDGE_CURVE ( 'NONE', #30674, #34637, #32362, .T. ) ;
#35623 = ORIENTED_EDGE ( 'NONE', *, *, #20247, .T. ) ;
#35622 = EDGE_LOOP ( 'NONE', ( #25309, #17425, #38033, #10306 ) ) ;
#35624 = DIRECTION ( 'NONE',  ( -1.000000000000000000, 0.000000000000000000, 0.000000000000000000 ) ) ;
#35625 = CARTESIAN_POINT ( 'NONE',  ( 5.000000000000000000, 8.660254037844385522, -144.6250000040967905 ) ) ;
#35626 = CARTESIAN_POINT ( 'NONE',  ( 10.81189881249999907, 6.242252689847868297, -152.7187500020483810 ) ) ;
#35627 =( BOUNDED_CURVE ( )  B_SPLINE_CURVE ( 2, ( #12295, #38640, #21600, #22448, #28731, #5422, #5633 ),
 .UNSPECIFIED., .F., .F. ) 
 B_SPLINE_CURVE_WITH_KNOTS ( ( 3, 2, 2, 3 ),
 ( 0.003731343283582092950, 0.004975124378109457846, 0.006218905472636822307, 0.007462686567164185901 ),
 .UNSPECIFIED. ) 
 CURVE ( )  GEOMETRIC_REPRESENTATION_ITEM ( )  RATIONAL_B_SPLINE_CURVE ( ( 0.9999999999999996669, 0.8660254037844390407, 1.000000000000000000, 0.8660254037844387076, 1.000000000000000000, 0.8660254037844379305, 1.000000000000000666 ) ) 
 REPRESENTATION_ITEM ( '' )  );
#35628 = CARTESIAN_POINT ( 'NONE',  ( 10.81189881249999907, 6.242252689847868297, -176.9062500020484094 ) ) ;
#35629 = CARTESIAN_POINT ( 'NONE',  ( -10.81189881249999729, 6.242252689847871849, -11.21875000204836859 ) ) ;
#35630 = CARTESIAN_POINT ( 'NONE',  ( 35.00000000000000711, 4.286263797015737285E-15, -169.9999999999999716 ) ) ;
#35631 = CARTESIAN_POINT ( 'NONE',  ( 5.405949406249999534, 9.363379034771803333, -137.5937500020483810 ) ) ;
#35632 = CARTESIAN_POINT ( 'NONE',  ( 5.405949406249999534, 9.363379034771803333, -103.0937500020483810 ) ) ;
#35633 = CARTESIAN_POINT ( 'NONE',  ( -9.999999999999998224, 1.224646799147353059E-15, -115.6250000040967905 ) ) ;
#35634 = CARTESIAN_POINT ( 'NONE',  ( -10.81189881249999729, 6.242252689847871849, -110.4062500020483810 ) ) ;
#35635 = CARTESIAN_POINT ( 'NONE',  ( 7.070501591499377789E-16, 11.54700538379251284, -195.5000000040968189 ) ) ;
#35636 = CARTESIAN_POINT ( 'NONE',  ( 5.405949406249992428, -9.363379034771808662, -118.5937500020483810 ) ) ;
#35637 = CARTESIAN_POINT ( 'NONE',  ( 5.405949406249992428, -9.363379034771808662, -189.2812500020484094 ) ) ;
#35638 = DIRECTION ( 'NONE',  ( 0.000000000000000000, 0.000000000000000000, 1.000000000000000000 ) ) ;
#35639 = CARTESIAN_POINT ( 'NONE',  ( 9.999999999999996447, -5.773502691896262640, -135.6250000000000000 ) ) ;
#35640 = CARTESIAN_POINT ( 'NONE',  ( 10.00000000000000000, 5.773502691896255534, -4.874999999999962697 ) ) ;
#35641 = CARTESIAN_POINT ( 'NONE',  ( 5.405949406249992428, -9.363379034771808662, -69.09375000204836681 ) ) ;
#35642 = CARTESIAN_POINT ( 'NONE',  ( -5.405949406249996869, 9.363379034771805109, -50.34375000204835260 ) ) ;
#35643 = CARTESIAN_POINT ( 'NONE',  ( -10.00000000000000000, -5.773502691896251982, -187.5000000040967905 ) ) ;
#35644 = CARTESIAN_POINT ( 'NONE',  ( -10.81189881249999907, -6.242252689847864744, -23.15625000204837747 ) ) ;
#35645 = CARTESIAN_POINT ( 'NONE',  ( 7.644554776091147741E-16, 12.48450537969573659, -39.96875000204835970 ) ) ;
#35646 = CARTESIAN_POINT ( 'NONE',  ( 7.070501591499376803E-16, 11.54700538379251284, -149.0000000040967905 ) ) ;
#35647 = CARTESIAN_POINT ( 'NONE',  ( -10.81189881249999729, 1.324075727343319199E-15, -135.5937500020483810 ) ) ;
#35648 = CARTESIAN_POINT ( 'NONE',  ( 9.999999999999998224, 0.000000000000000000, -114.4999999999999858 ) ) ;
#35649 = CARTESIAN_POINT ( 'NONE',  ( 9.999999999999998224, 0.000000000000000000, -114.4999999999999858 ) ) ;
#35650 = CARTESIAN_POINT ( 'NONE',  ( 5.000000000000000000, 8.660254037844385522, -67.74999999999997158 ) ) ;
#35651 = CARTESIAN_POINT ( 'NONE',  ( 10.81189881249999551, -6.242252689847874514, -136.6562500020484094 ) ) ;
#35652 = CARTESIAN_POINT ( 'NONE',  ( 10.81189881249999729, 0.000000000000000000, -112.5312500020483952 ) ) ;
#35653 = ORIENTED_EDGE ( 'NONE', *, *, #17595, .T. ) ;
#35654 = CARTESIAN_POINT ( 'NONE',  ( -4.999999999999996447, 8.660254037844387298, -196.8750000040967905 ) ) ;
#35655 = CARTESIAN_POINT ( 'NONE',  ( -2.121150477449813534E-15, -11.54700538379251284, -116.7500000040967905 ) ) ;
#35656 = DIRECTION ( 'NONE',  ( -1.000000000000000000, 0.000000000000000000, 0.000000000000000000 ) ) ;
#35657 = CARTESIAN_POINT ( 'NONE',  ( 10.81189881249999907, 6.242252689847868297, -73.21875000204836681 ) ) ;
#35658 = CARTESIAN_POINT ( 'NONE',  ( -9.999999999999998224, 5.773502691896259087, -43.37499999999997158 ) ) ;
#35659 = CARTESIAN_POINT ( 'NONE',  ( 9.999999999999998224, 0.000000000000000000, -26.37500000409676204 ) ) ;
#35660 = CARTESIAN_POINT ( 'NONE',  ( -10.81189881249999729, 6.242252689847871849, -42.90625000204838102 ) ) ;
#35661 = CARTESIAN_POINT ( 'NONE',  ( 0.000000000000000000, 0.000000000000000000, -200.0000000000000000 ) ) ;
#35662 = CARTESIAN_POINT ( 'NONE',  ( 10.00000000000000000, 5.773502691896255534, -47.25000000409676204 ) ) ;
#35663 = CARTESIAN_POINT ( 'NONE',  ( 5.405949406249992428, -9.363379034771808662, -33.28125000204837391 ) ) ;
#35664 = CARTESIAN_POINT ( 'NONE',  ( -10.00000000000025580, 5.773502691896109873, -156.2500000040968189 ) ) ;
#35665 = CARTESIAN_POINT ( 'NONE',  ( -10.81189881249999729, 1.324075727343319199E-15, -138.7812500020483810 ) ) ;
#35666 = CARTESIAN_POINT ( 'NONE',  ( -10.81189881249999907, -6.242252689847864744, -152.1562500020484094 ) ) ;
#35667 = CARTESIAN_POINT ( 'NONE',  ( -4.999999999999996447, 8.660254037844387298, -59.99999999999997158 ) ) ;
#35668 = CARTESIAN_POINT ( 'NONE',  ( -9.999999999999998224, 1.224646799147353059E-15, -124.2500000000000000 ) ) ;
#35669 = VERTEX_POINT ( 'NONE', #16764 ) ;
#35670 = EDGE_LOOP ( 'NONE', ( #41518, #11705, #13071, #32645 ) ) ;
#35671 = EDGE_CURVE ( 'NONE', #33809, #40301, #17402, .T. ) ;
#35672 = ORIENTED_EDGE ( 'NONE', *, *, #34605, .F. ) ;
#35673 = EDGE_CURVE ( 'NONE', #35190, #24289, #34091, .T. ) ;
#35674 = CARTESIAN_POINT ( 'NONE',  ( -9.999999999999998224, 1.224646799147353059E-15, -117.1250000040967905 ) ) ;
#35675 = CARTESIAN_POINT ( 'NONE',  ( -10.81189881249999729, 1.324075727343319199E-15, -170.0937500020484094 ) ) ;
#35676 = CARTESIAN_POINT ( 'NONE',  ( -10.81189881249999907, -6.242252689847864744, -31.96875000204835970 ) ) ;
#35677 = FACE_OUTER_BOUND ( 'NONE', #28194, .T. ) ;
#35678 = AXIS2_PLACEMENT_3D ( 'NONE', #21976, #5155, #12457 ) ;
#35679 = CARTESIAN_POINT ( 'NONE',  ( -5.405949406249996869, 9.363379034771805109, -167.3437500020484094 ) ) ;
#35680 = CARTESIAN_POINT ( 'NONE',  ( -10.81189881249999907, -6.242252689847864744, -148.9687500020484094 ) ) ;
#35681 = CARTESIAN_POINT ( 'NONE',  ( -9.999999999999998224, 1.224646799147353059E-15, -176.7500000000000284 ) ) ;
#35682 = CARTESIAN_POINT ( 'NONE',  ( 10.81189881249999551, -6.242252689847874514, -128.9687500020483810 ) ) ;
#35683 = CARTESIAN_POINT ( 'NONE',  ( -10.81189881249999729, 1.324075727343319199E-15, -135.7812500020483810 ) ) ;
#35684 = CARTESIAN_POINT ( 'NONE',  ( -2.293366432827344421E-15, -12.48450537969573659, -16.71875000204836326 ) ) ;
#35685 = CARTESIAN_POINT ( 'NONE',  ( 5.405949406249992428, -9.363379034771808662, -150.0937500020483810 ) ) ;
#35686 = CARTESIAN_POINT ( 'NONE',  ( 5.000000000000000000, 8.660254037844385522, -135.2499999999999716 ) ) ;
#35687 = CARTESIAN_POINT ( 'NONE',  ( 7.070501591499376803E-16, 11.54700538379251284, -141.5000000040967905 ) ) ;
#35688 = CARTESIAN_POINT ( 'NONE',  ( 10.00000000000000000, 5.773502691896255534, -166.8750000000000000 ) ) ;
#35689 = CARTESIAN_POINT ( 'NONE',  ( -10.81189881249999729, 1.324075727343319199E-15, -69.59375000204836681 ) ) ;
#35690 = CARTESIAN_POINT ( 'NONE',  ( 5.405949406249999534, 9.363379034771803333, -52.28125000204835970 ) ) ;
#35691 = CARTESIAN_POINT ( 'NONE',  ( -5.405949406249996869, 9.363379034771805109, -57.84375000204835970 ) ) ;
#35692 = DIRECTION ( 'NONE',  ( -0.000000000000000000, -0.000000000000000000, -1.000000000000000000 ) ) ;
#35693 = CARTESIAN_POINT ( 'NONE',  ( 5.405949406249992428, -9.363379034771808662, -169.5937500020484094 ) ) ;
#35694 = CARTESIAN_POINT ( 'NONE',  ( 9.999999999999996447, -5.773502691896262640, -134.1250000000000000 ) ) ;
#35695 = CARTESIAN_POINT ( 'NONE',  ( -2.293366432827344421E-15, -12.48450537969573659, -148.9062500020484379 ) ) ;
#35696 =( BOUNDED_CURVE ( )  B_SPLINE_CURVE ( 2, ( #34056, #40710, #23919, #17620, #411, #7936, #29969 ),
 .UNSPECIFIED., .F., .F. ) 
 B_SPLINE_CURVE_WITH_KNOTS ( ( 3, 2, 2, 3 ),
 ( 0.4179104477611941260, 0.4191542288557215112, 0.4203980099502488965, 0.4216417910447762818 ),
 .UNSPECIFIED. ) 
 CURVE ( )  GEOMETRIC_REPRESENTATION_ITEM ( )  RATIONAL_B_SPLINE_CURVE ( ( 0.9999999999999880096, 0.8660254037844506980, 1.000000000000000000, 0.8660254037844387076, 1.000000000000000000, 0.8660254037844207220, 1.000000000000017986 ) ) 
 REPRESENTATION_ITEM ( '' )  );
#35697 = CARTESIAN_POINT ( 'NONE',  ( -4.999999999999996447, 8.660254037844387298, -15.37500000409675138 ) ) ;
#35698 = CARTESIAN_POINT ( 'NONE',  ( 5.000000000000000000, 8.660254037844385522, -125.1250000040967620 ) ) ;
#35699 = CARTESIAN_POINT ( 'NONE',  ( 9.999999999999996447, -5.773502691896262640, -93.62499999999998579 ) ) ;
#35700 = EDGE_LOOP ( 'NONE', ( #8516, #5887, #33699, #27796 ) ) ;
#35701 = CARTESIAN_POINT ( 'NONE',  ( 5.405949406249999534, 9.363379034771803333, -121.2812500020483952 ) ) ;
#35702 = CARTESIAN_POINT ( 'NONE',  ( 9.999999999999996447, -5.773502691896262640, -142.0000000040967905 ) ) ;
#35703 = CARTESIAN_POINT ( 'NONE',  ( 9.999999999998969713, 5.773502691896851502, -52.87499999999995737 ) ) ;
#35704 = CARTESIAN_POINT ( 'NONE',  ( -10.81189881249999729, 6.242252689847871849, -168.9062500020483810 ) ) ;
#35705 = CARTESIAN_POINT ( 'NONE',  ( 7.070501591499377789E-16, 11.54700538379251284, -48.50000000409676915 ) ) ;
#35706 = CARTESIAN_POINT ( 'NONE',  ( 10.00000000000025402, -5.773502691896113426, -159.6250000000000284 ) ) ;
#35707 = CARTESIAN_POINT ( 'NONE',  ( 5.405949406249999534, 9.363379034771803333, -62.78125000204837391 ) ) ;
#35708 = CARTESIAN_POINT ( 'NONE',  ( -22.00000000000000711, 0.000000000000000000, -99.99999999999998579 ) ) ;
#35709 = CARTESIAN_POINT ( 'NONE',  ( 10.81189881249999907, 6.242252689847868297, -164.9062500020484094 ) ) ;
#35710 = CARTESIAN_POINT ( 'NONE',  ( -2.293366432827344421E-15, -12.48450537969573659, -141.2187500020483810 ) ) ;
#35711 = AXIS2_PLACEMENT_3D ( 'NONE', #10755, #37091, #11185 ) ;
#35712 = LINE ( 'NONE', #9993, #29102 ) ;
#35713 = CARTESIAN_POINT ( 'NONE',  ( 7.070501591499376803E-16, 11.54700538379251284, -80.00000000409677625 ) ) ;
#35714 = AXIS2_PLACEMENT_3D ( 'NONE', #9230, #41603, #38377 ) ;
#35715 = VERTEX_POINT ( 'NONE', #10298 ) ;
#35717 = EDGE_LOOP ( 'NONE', ( #10691, #38745 ) ) ;
#35716 = CARTESIAN_POINT ( 'NONE',  ( 5.405949406249999534, 9.363379034771803333, -68.78125000204838102 ) ) ;
#35718 = CARTESIAN_POINT ( 'NONE',  ( 0.000000000000000000, 0.000000000000000000, 0.000000000000000000 ) ) ;
#35719 = EDGE_CURVE ( 'NONE', #22184, #8341, #38498, .T. ) ;
#35721 = ORIENTED_EDGE ( 'NONE', *, *, #15405, .T. ) ;
#35720 = CARTESIAN_POINT ( 'NONE',  ( -10.00000000000154188, 5.773502691895366468, -29.87499999999990763 ) ) ;
#35722 = ORIENTED_EDGE ( 'NONE', *, *, #7691, .F. ) ;
#35723 = EDGE_CURVE ( 'NONE', #27003, #10661, #30389, .T. ) ;
#35724 = CARTESIAN_POINT ( 'NONE',  ( -10.81189881249999729, 1.324075727343319199E-15, -29.09375000204836326 ) ) ;
#35725 = CARTESIAN_POINT ( 'NONE',  ( 9.999999999999998224, 0.000000000000000000, -108.4999999999999858 ) ) ;
#35726 = CARTESIAN_POINT ( 'NONE',  ( -5.405949406249996869, 9.363379034771805109, -2.531250002048373915 ) ) ;
#35728 = EDGE_CURVE ( 'NONE', #27698, #17741, #3637, .T. ) ;
#35727 = CARTESIAN_POINT ( 'NONE',  ( 10.81189881249999729, 0.000000000000000000, -56.84375000204835970 ) ) ;
#35729 = CARTESIAN_POINT ( 'NONE',  ( 9.999999999999998224, 0.000000000000000000, -138.5000000000000000 ) ) ;
#35730 = CARTESIAN_POINT ( 'NONE',  ( -9.999999999999998224, 1.224646799147353059E-15, -31.24999999999997158 ) ) ;
#35731 = CARTESIAN_POINT ( 'NONE',  ( -5.405949406250003975, -9.363379034771801557, -187.8437500020483810 ) ) ;
#35732 = CARTESIAN_POINT ( 'NONE',  ( 5.405949406249999534, 9.363379034771803333, -167.5937500020484094 ) ) ;
#35733 = CC_DESIGN_DATE_AND_TIME_ASSIGNMENT ( #16357, #3021, ( #3281 ) ) ;
#35734 = CARTESIAN_POINT ( 'NONE',  ( -5.405949406250003975, -9.363379034771801557, -156.3437500020483810 ) ) ;
#35735 =( BOUNDED_CURVE ( )  B_SPLINE_CURVE ( 2, ( #22685, #15550, #42511, #12528, #13151, #23108, #25513 ),
 .UNSPECIFIED., .F., .F. ) 
 B_SPLINE_CURVE_WITH_KNOTS ( ( 3, 2, 2, 3 ),
 ( 0.4664179104477613191, 0.4676616915422886489, 0.4689054726368160342, 0.4701492537313434195 ),
 .UNSPECIFIED. ) 
 CURVE ( )  GEOMETRIC_REPRESENTATION_ITEM ( )  RATIONAL_B_SPLINE_CURVE ( ( 0.9999999999999880096, 0.8660254037844506980, 1.000000000000000000, 0.8660254037844387076, 1.000000000000000000, 0.8660254037844267172, 1.000000000000011990 ) ) 
 REPRESENTATION_ITEM ( '' )  );
#35736 = CARTESIAN_POINT ( 'NONE',  ( -5.405949406250003975, -9.363379034771801557, -171.3437500020484094 ) ) ;
#35737 = CARTESIAN_POINT ( 'NONE',  ( 0.000000000000000000, 0.000000000000000000, -99.99999999999998579 ) ) ;
#35738 = CARTESIAN_POINT ( 'NONE',  ( 9.999999999999998224, 0.000000000000000000, -168.5000000000000000 ) ) ;
#35739 = CARTESIAN_POINT ( 'NONE',  ( 9.999999999999998224, 0.000000000000000000, -188.0000000000000000 ) ) ;
#35740 = CARTESIAN_POINT ( 'NONE',  ( -5.405949406249996869, 9.363379034771805109, -104.3437500020483810 ) ) ;
#35741 = DIRECTION ( 'NONE',  ( -0.000000000000000000, -0.000000000000000000, 1.000000000000000000 ) ) ;
#35742 = CARTESIAN_POINT ( 'NONE',  ( -10.81189881249999729, 1.324075727343319199E-15, -71.28125000204838102 ) ) ;
#35743 = CARTESIAN_POINT ( 'NONE',  ( -9.999999999999998224, 1.224646799147353059E-15, -160.2500000000000000 ) ) ;
#35744 = CARTESIAN_POINT ( 'NONE',  ( -10.81189881249999729, 1.324075727343319199E-15, -81.59375000204838102 ) ) ;
#35745 = VECTOR ( 'NONE', #22305, 1000.000000000000000 ) ;
#35746 = CARTESIAN_POINT ( 'NONE',  ( 5.405949406249999534, 9.363379034771803333, -59.78125000204836681 ) ) ;
#35747 = CARTESIAN_POINT ( 'NONE',  ( -9.999999999999998224, 5.773502691896259087, -142.7500000040967905 ) ) ;
#35748 = CARTESIAN_POINT ( 'NONE',  ( -10.00000000000000000, -5.773502691896251982, -118.1250000000000142 ) ) ;
#35749 = EDGE_CURVE ( 'NONE', #8116, #9826, #30177, .T. ) ;
#35750 = ORIENTED_EDGE ( 'NONE', *, *, #31975, .T. ) ;
#35751 = CARTESIAN_POINT ( 'NONE',  ( 10.81189881249999729, 0.000000000000000000, -142.5312500020483810 ) ) ;
#35752 = CARTESIAN_POINT ( 'NONE',  ( 10.81189881249999551, -6.242252689847874514, -159.1562500020484094 ) ) ;
#35753 = CARTESIAN_POINT ( 'NONE',  ( 10.81189881249999729, 0.000000000000000000, -193.5312500020484094 ) ) ;
#35754 = CARTESIAN_POINT ( 'NONE',  ( 9.999999999999998224, 0.000000000000000000, -179.0000000000000000 ) ) ;
#35755 = CARTESIAN_POINT ( 'NONE',  ( -5.405949406250003975, -9.363379034771801557, -88.84375000204838102 ) ) ;
#35756 = EDGE_LOOP ( 'NONE', ( #29290, #25167 ) ) ;
#35757 = CARTESIAN_POINT ( 'NONE',  ( -9.999999999999998224, 1.224646799147353059E-15, -59.74999999999997158 ) ) ;
#35758 = CARTESIAN_POINT ( 'NONE',  ( 5.405949406249992428, -9.363379034771808662, -192.0937500020484094 ) ) ;
#35759 = CARTESIAN_POINT ( 'NONE',  ( -10.00000000000000000, -5.773502691896251982, -75.00000000409677625 ) ) ;
#35760 = CARTESIAN_POINT ( 'NONE',  ( 9.999999999999998224, 1.224646799147353059E-15, -99.99999999999998579 ) ) ;
#35761 = CARTESIAN_POINT ( 'NONE',  ( -9.999999999999479527, -5.773502691896549521, -145.1250000000000000 ) ) ;
#35762 = CARTESIAN_POINT ( 'NONE',  ( 7.644554776091147741E-16, 12.48450537969573659, -85.15625000204838102 ) ) ;
#35763 = CARTESIAN_POINT ( 'NONE',  ( 10.81189881249999729, 0.000000000000000000, -69.03125000204838102 ) ) ;
#35764 = CARTESIAN_POINT ( 'NONE',  ( 9.999999999999996447, -5.773502691896262640, -64.00000000409677625 ) ) ;
#35765 = CARTESIAN_POINT ( 'NONE',  ( -5.405949406250003975, -9.363379034771801557, -16.84375000204835260 ) ) ;
#35766 = CARTESIAN_POINT ( 'NONE',  ( 5.000000000000000000, 8.660254037844385522, -100.7499999999999858 ) ) ;
#35767 = CARTESIAN_POINT ( 'NONE',  ( 10.81189881249999907, 6.242252689847868297, -196.4062500020484379 ) ) ;
#35768 = CARTESIAN_POINT ( 'NONE',  ( -2.293366432827344421E-15, -12.48450537969573659, -12.40625000204836859 ) ) ;
#35769 = CARTESIAN_POINT ( 'NONE',  ( 10.81189881249999551, -6.242252689847874514, -1.468750002048354819 ) ) ;
#35770 = DIRECTION ( 'NONE',  ( -0.000000000000000000, -0.000000000000000000, 1.000000000000000000 ) ) ;
#35771 = FACE_OUTER_BOUND ( 'NONE', #41722, .T. ) ;
#35772 = CARTESIAN_POINT ( 'NONE',  ( -23.09401076758503280, 0.000000000000000000, 45.00000000000009237 ) ) ;
#35773 = CARTESIAN_POINT ( 'NONE',  ( 7.070501591499377789E-16, 11.54700538379251284, -171.1250000000000000 ) ) ;
#35774 = CARTESIAN_POINT ( 'NONE',  ( -45.00000000000000711, 0.000000000000000000, -203.0000000000000000 ) ) ;
#35776 = ORIENTED_EDGE ( 'NONE', *, *, #5401, .F. ) ;
#35775 = CARTESIAN_POINT ( 'NONE',  ( -2.293366432827344421E-15, -12.48450537969573659, -105.4062500020483810 ) ) ;
#35777 = AXIS2_PLACEMENT_3D ( 'NONE', #8837, #8198, #21347 ) ;
#35778 = ORIENTED_EDGE ( 'NONE', *, *, #7449, .T. ) ;
#35779 = EDGE_LOOP ( 'NONE', ( #3608, #5945, #6356, #24689 ) ) ;
#35780 = CARTESIAN_POINT ( 'NONE',  ( 5.405949406249999534, 9.363379034771803333, -32.59375000204836681 ) ) ;
#35781 = CARTESIAN_POINT ( 'NONE',  ( 10.81189881249999907, 6.242252689847868297, -29.90625000204836326 ) ) ;
#35782 = COORDINATED_UNIVERSAL_TIME_OFFSET ( 6, 0, .AHEAD. ) ;
#35783 = AXIS2_PLACEMENT_3D ( 'NONE', #36426, #30600, #13316 ) ;
#35784 = CARTESIAN_POINT ( 'NONE',  ( 5.405949406249999534, 9.363379034771803333, -80.59375000204838102 ) ) ;
#35785 = DIRECTION ( 'NONE',  ( 0.7071067811865417996, 0.000000000000000000, 0.7071067811865532349 ) ) ;
#35786 = CARTESIAN_POINT ( 'NONE',  ( -2.293366432827344421E-15, -12.48450537969573659, -198.2187500020484379 ) ) ;
#35787 = CARTESIAN_POINT ( 'NONE',  ( 9.999999999999998224, 0.000000000000000000, -125.0000000000000000 ) ) ;
#35788 = FACE_BOUND ( 'NONE', #8985, .T. ) ;
#35789 = CARTESIAN_POINT ( 'NONE',  ( -10.81189881249999729, 1.324075727343319199E-15, -158.2812500020484094 ) ) ;
#35790 = CARTESIAN_POINT ( 'NONE',  ( -2.121150477449813534E-15, -11.54700538379251284, -8.750000004096753159 ) ) ;
#35791 = CARTESIAN_POINT ( 'NONE',  ( -9.999999999999998224, 1.224646799147353059E-15, -103.6250000040967763 ) ) ;
#35792 = EDGE_CURVE ( 'NONE', #41070, #41327, #17806, .T. ) ;
#35793 = CARTESIAN_POINT ( 'NONE',  ( -10.81189881249999729, 1.324075727343319199E-15, -129.5937500020483810 ) ) ;
#35794 = CARTESIAN_POINT ( 'NONE',  ( -10.81189881249999729, 6.242252689847871849, -99.90625000204838102 ) ) ;
#35795 = CARTESIAN_POINT ( 'NONE',  ( -2.293366432827344421E-15, -12.48450537969573659, -108.2187500020483668 ) ) ;
#35796 = CARTESIAN_POINT ( 'NONE',  ( 10.81189881249999551, -6.242252689847874514, -77.96875000204838102 ) ) ;
#35797 = CARTESIAN_POINT ( 'NONE',  ( 10.81189881249999551, -6.242252689847874514, -85.65625000204838102 ) ) ;
#35798 = CARTESIAN_POINT ( 'NONE',  ( -9.999999999999998224, 5.773502691896259087, -172.7500000040967905 ) ) ;
#35799 = CARTESIAN_POINT ( 'NONE',  ( 0.000000000000000000, 0.000000000000000000, -200.0000000000000000 ) ) ;
#35800 = CARTESIAN_POINT ( 'NONE',  ( -10.81189881249999729, -6.242252689847864744, -168.6562500020484094 ) ) ;
#35801 = CARTESIAN_POINT ( 'NONE',  ( 7.644554776091147741E-16, 12.48450537969573659, -179.6562500020484094 ) ) ;
#35802 = CARTESIAN_POINT ( 'NONE',  ( -2.121150477449813534E-15, -11.54700538379251284, -155.7500000040967620 ) ) ;
#35803 = CARTESIAN_POINT ( 'NONE',  ( 0.000000000000000000, 0.000000000000000000, -220.0000000000000000 ) ) ;
#35804 = CARTESIAN_POINT ( 'NONE',  ( -2.293366432827344421E-15, -12.48450537969573659, -9.218750002048359704 ) ) ;
#35805 = CARTESIAN_POINT ( 'NONE',  ( 9.999999999999998224, 0.000000000000000000, -59.37500000409676204 ) ) ;
#35806 = CARTESIAN_POINT ( 'NONE',  ( -5.405949406249996869, 9.363379034771805109, -114.8437500020483810 ) ) ;
#35807 = CARTESIAN_POINT ( 'NONE',  ( 10.00000000000000000, 5.773502691896255534, -87.37499999999998579 ) ) ;
#35808 = CARTESIAN_POINT ( 'NONE',  ( -10.81189881249999907, -6.242252689847864744, -14.15625000204837036 ) ) ;
#35809 = CARTESIAN_POINT ( 'NONE',  ( -9.999999999999998224, 5.773502691896259087, -97.75000000409677625 ) ) ;
#35810 = CYLINDRICAL_SURFACE ( 'NONE', #27213, 9.999999999999998224 ) ;
#35811 = CARTESIAN_POINT ( 'NONE',  ( -10.81189881249999729, 6.242252689847871849, -105.9062500020483810 ) ) ;
#35812 = CARTESIAN_POINT ( 'NONE',  ( -10.81189881249999729, 6.242252689847871849, -93.90625000204838102 ) ) ;
#35813 = EDGE_LOOP ( 'NONE', ( #349, #9056, #37, #5450 ) ) ;
#35814 = CARTESIAN_POINT ( 'NONE',  ( 9.999999999999996447, -5.773502691896262640, -85.00000000409677625 ) ) ;
#35815 = CARTESIAN_POINT ( 'NONE',  ( -35.00000000000000711, 0.000000000000000000, -176.9999999999999432 ) ) ;
#35816 = CARTESIAN_POINT ( 'NONE',  ( 10.81189881249999907, 6.242252689847868297, -43.21875000204835970 ) ) ;
#35817 = ORIENTED_EDGE ( 'NONE', *, *, #31517, .T. ) ;
#35818 = CARTESIAN_POINT ( 'NONE',  ( -9.999999999999998224, 1.224646799147353059E-15, -16.24999999999995737 ) ) ;
#35819 = VECTOR ( 'NONE', #38731, 1000.000000000000000 ) ;
#35820 = CARTESIAN_POINT ( 'NONE',  ( -10.00000000000000000, -5.773502691896251982, -154.1250000000000284 ) ) ;
#35821 = CARTESIAN_POINT ( 'NONE',  ( 10.00000000000000000, 5.773502691896255534, -11.25000000409676204 ) ) ;
#35822 = CARTESIAN_POINT ( 'NONE',  ( 4.999999999999992006, -8.660254037844389075, -119.6250000040967905 ) ) ;
#35824 = ORIENTED_EDGE ( 'NONE', *, *, #13545, .F. ) ;
#35823 = CARTESIAN_POINT ( 'NONE',  ( 10.81189881249999551, -6.242252689847874514, -129.1562500020483810 ) ) ;
#35825 = CARTESIAN_POINT ( 'NONE',  ( -10.00000000000051337, 5.773502691895962435, -89.87499999999998579 ) ) ;
#35826 =( BOUNDED_CURVE ( )  B_SPLINE_CURVE ( 2, ( #12378, #35503, #25573, #14976, #28390, #1850, #15611 ),
 .UNSPECIFIED., .F., .F. ) 
 B_SPLINE_CURVE_WITH_KNOTS ( ( 3, 2, 2, 3 ),
 ( 0.2537313432835822113, 0.2549751243781095411, 0.2562189054726369264, 0.2574626865671643117 ),
 .UNSPECIFIED. ) 
 CURVE ( )  GEOMETRIC_REPRESENTATION_ITEM ( )  RATIONAL_B_SPLINE_CURVE ( ( 0.9999999999999880096, 0.8660254037844506980, 1.000000000000000000, 0.8660254037844387076, 1.000000000000000000, 0.8660254037844267172, 1.000000000000011990 ) ) 
 REPRESENTATION_ITEM ( '' )  );
#35827 = ORIENTED_EDGE ( 'NONE', *, *, #23291, .T. ) ;
#35828 = CARTESIAN_POINT ( 'NONE',  ( -5.405949406249996869, 9.363379034771805109, -55.03125000204836681 ) ) ;
#35829 = PERSON_AND_ORGANIZATION_ROLE ( 'design_supplier' ) ;
#35830 = CARTESIAN_POINT ( 'NONE',  ( 5.405949406249992428, -9.363379034771808662, -100.5937500020483810 ) ) ;
#35832 = ORIENTED_EDGE ( 'NONE', *, *, #28465, .F. ) ;
#35831 = ORIENTED_EDGE ( 'NONE', *, *, #38942, .T. ) ;
#35833 = CARTESIAN_POINT ( 'NONE',  ( -9.999999999999998224, 1.224646799147353059E-15, -77.74999999999998579 ) ) ;
#35834 = CARTESIAN_POINT ( 'NONE',  ( -2.293366432827344421E-15, -12.48450537969573659, -180.4062500020484379 ) ) ;
#35835 = CARTESIAN_POINT ( 'NONE',  ( -5.405949406249996869, 9.363379034771805109, -2.343750002048366810 ) ) ;
#35836 = CARTESIAN_POINT ( 'NONE',  ( 4.999999999999992006, -8.660254037844389075, -146.6250000040967905 ) ) ;
#35837 = AXIS2_PLACEMENT_3D ( 'NONE', #9432, #39415, #38569 ) ;
#35838 = CARTESIAN_POINT ( 'NONE',  ( 10.81189881249999729, 6.242252689847867408, -128.7187500020483810 ) ) ;
#35839 = CARTESIAN_POINT ( 'NONE',  ( 10.81189881249999551, -6.242252689847874514, -103.4687500020483810 ) ) ;
#35840 = CARTESIAN_POINT ( 'NONE',  ( 9.999999999999742428, 5.773502691896404748, -116.2500000040967620 ) ) ;
#35841 = CARTESIAN_POINT ( 'NONE',  ( 5.405949406249999534, 9.363379034771803333, -109.2812500020483810 ) ) ;
#35842 = CARTESIAN_POINT ( 'NONE',  ( 9.999999999999998224, 0.000000000000000000, -197.3750000040967905 ) ) ;
#35843 = CARTESIAN_POINT ( 'NONE',  ( -10.81189881249999729, -6.242252689847864744, -117.4687500020483810 ) ) ;
#35844 = CARTESIAN_POINT ( 'NONE',  ( -5.405949406249996869, 9.363379034771805109, -184.0312500020484094 ) ) ;
#35845 = DIRECTION ( 'NONE',  ( -0.5000000000000003331, 0.8660254037844383745, 0.000000000000000000 ) ) ;
#35846 = CARTESIAN_POINT ( 'NONE',  ( 5.000000000000000000, 8.660254037844385522, -138.2499999999999716 ) ) ;
#35847 = CARTESIAN_POINT ( 'NONE',  ( -9.999999999999998224, 5.773502691896259087, -5.874999999999963585 ) ) ;
#35848 = CARTESIAN_POINT ( 'NONE',  ( 10.81189881249999729, 0.000000000000000000, -65.84375000204836681 ) ) ;
#35849 = CARTESIAN_POINT ( 'NONE',  ( 10.81189881249999729, 0.000000000000000000, -47.84375000204838102 ) ) ;
#35850 = CARTESIAN_POINT ( 'NONE',  ( 9.999999999999998224, 0.000000000000000000, -176.3750000040967905 ) ) ;
#35851 = CARTESIAN_POINT ( 'NONE',  ( 5.405949406249992428, -9.363379034771808662, -24.28125000204836681 ) ) ;
#35852 = CARTESIAN_POINT ( 'NONE',  ( 10.81189881249999551, -6.242252689847874514, -31.46875000204835260 ) ) ;
#35853 = CARTESIAN_POINT ( 'NONE',  ( -99.99999999999994316, 19.99999999999998934, -170.0000000000000000 ) ) ;
#35854 = CARTESIAN_POINT ( 'NONE',  ( 10.81189881249999907, 6.242252689847868297, -139.2187500020484094 ) ) ;
#35855 = CARTESIAN_POINT ( 'NONE',  ( 9.999999999999996447, -5.773502691896262640, -110.1250000000000000 ) ) ;
#35856 = CARTESIAN_POINT ( 'NONE',  ( 9.999999999999742428, 5.773502691896404748, -163.8750000000000284 ) ) ;
#35857 = CARTESIAN_POINT ( 'NONE',  ( -9.999999999999998224, 5.773502691896259087, -70.37499999999998579 ) ) ;
#35858 = CARTESIAN_POINT ( 'NONE',  ( 7.644554776091147741E-16, 12.48450537969573659, -136.1562500020483810 ) ) ;
#35859 = CARTESIAN_POINT ( 'NONE',  ( -10.81189881249999729, -6.242252689847864744, -113.1562500020483952 ) ) ;
#35860 = EDGE_CURVE ( 'NONE', #39730, #30625, #22243, .T. ) ;
#35861 = ORIENTED_EDGE ( 'NONE', *, *, #8579, .T. ) ;
#35862 = CARTESIAN_POINT ( 'NONE',  ( -9.999999999999998224, 1.224646799147353059E-15, -160.6250000040967905 ) ) ;
#35863 = CARTESIAN_POINT ( 'NONE',  ( -4.999999999999996447, 8.660254037844387298, -106.8750000040967763 ) ) ;
#35864 = DIRECTION ( 'NONE',  ( 0.5000000000000007772, -0.8660254037844381525, -0.000000000000000000 ) ) ;
#35865 = CARTESIAN_POINT ( 'NONE',  ( -5.405949406249996869, 9.363379034771805109, -65.34375000204836681 ) ) ;
#35866 = VERTEX_POINT ( 'NONE', #20649 ) ;
#35867 = CARTESIAN_POINT ( 'NONE',  ( -10.00000000000000000, -5.773502691896251982, -41.62499999999997158 ) ) ;
#35868 = CARTESIAN_POINT ( 'NONE',  ( 4.999999999999992006, -8.660254037844389075, -19.12500000409675494 ) ) ;
#35869 = CARTESIAN_POINT ( 'NONE',  ( -10.81189881249999729, 1.324075727343319199E-15, -42.78125000204838102 ) ) ;
#35870 = CARTESIAN_POINT ( 'NONE',  ( 7.070501591499377789E-16, 11.54700538379251284, -44.00000000409676204 ) ) ;
#35871 = CARTESIAN_POINT ( 'NONE',  ( -10.81189881249999729, 6.242252689847871849, -39.90625000204836681 ) ) ;
#35872 =( BOUNDED_CURVE ( )  B_SPLINE_CURVE ( 2, ( #42417, #22584, #9418, #13056, #38777, #3369, #42207 ),
 .UNSPECIFIED., .F., .F. ) 
 B_SPLINE_CURVE_WITH_KNOTS ( ( 3, 2, 2, 3 ),
 ( 0.9253731343283585487, 0.9266169154228859339, 0.9278606965174133192, 0.9291044776119405935 ),
 .UNSPECIFIED. ) 
 CURVE ( )  GEOMETRIC_REPRESENTATION_ITEM ( )  RATIONAL_B_SPLINE_CURVE ( ( 0.9999999999999641398, 0.8660254037844745678, 1.000000000000000000, 0.8660254037844387076, 1.000000000000000000, 0.8660254037844028474, 1.000000000000035971 ) ) 
 REPRESENTATION_ITEM ( '' )  );
#35873 = DIRECTION ( 'NONE',  ( -0.000000000000000000, -0.000000000000000000, 1.000000000000000000 ) ) ;
#35874 = CARTESIAN_POINT ( 'NONE',  ( -10.81189881249999729, 6.242252689847871849, -137.4062500020484094 ) ) ;
#35875 = CARTESIAN_POINT ( 'NONE',  ( 5.405949406249999534, 9.363379034771803333, -151.2812500020484094 ) ) ;
#35876 = CARTESIAN_POINT ( 'NONE',  ( 7.070501591499376803E-16, 11.54700538379251284, -150.5000000040968189 ) ) ;
#35877 = VERTEX_POINT ( 'NONE', #40078 ) ;
#35878 =( BOUNDED_CURVE ( )  B_SPLINE_CURVE ( 2, ( #12380, #22329, #5931, #5290, #19082, #41534, #29021 ),
 .UNSPECIFIED., .F., .F. ) 
 B_SPLINE_CURVE_WITH_KNOTS ( ( 3, 2, 2, 3 ),
 ( 0.07462686567164185381, 0.07587064676616922521, 0.07711442786069658273, 0.07835820895522395413 ),
 .UNSPECIFIED. ) 
 CURVE ( )  GEOMETRIC_REPRESENTATION_ITEM ( )  RATIONAL_B_SPLINE_CURVE ( ( 0.9999999999999925615, 0.8660254037844461461, 1.000000000000000000, 0.8660254037844387076, 1.000000000000000000, 0.8660254037844312691, 1.000000000000007550 ) ) 
 REPRESENTATION_ITEM ( '' )  );
#35879 = ORIENTED_EDGE ( 'NONE', *, *, #18294, .F. ) ;
#35880 = VERTEX_POINT ( 'NONE', #29750 ) ;
#35881 = CARTESIAN_POINT ( 'NONE',  ( 7.644554776091147741E-16, 12.48450537969573659, -174.9687500020484094 ) ) ;
#35882 = CARTESIAN_POINT ( 'NONE',  ( 10.81189881249999907, 6.242252689847868297, -22.21875000204837036 ) ) ;
#35883 = CARTESIAN_POINT ( 'NONE',  ( -9.999999999999998224, 1.224646799147353059E-15, -61.62500000409676204 ) ) ;
#35884 = CARTESIAN_POINT ( 'NONE',  ( -10.81189881249999729, 6.242252689847871849, -161.2187500020483810 ) ) ;
#35885 = CARTESIAN_POINT ( 'NONE',  ( 5.405949406249999534, 9.363379034771803333, -142.0937500020483810 ) ) ;
#35886 = CARTESIAN_POINT ( 'NONE',  ( -2.121150477449813534E-15, -11.54700538379251284, -119.3749999999999858 ) ) ;
#35887 = CARTESIAN_POINT ( 'NONE',  ( 5.405949406249992428, -9.363379034771808662, -123.0937500020483952 ) ) ;
#35888 = CARTESIAN_POINT ( 'NONE',  ( 10.81189881249999729, 0.000000000000000000, -129.0312500020484094 ) ) ;
#35889 = CARTESIAN_POINT ( 'NONE',  ( 5.405949406249992428, -9.363379034771808662, -15.09375000204835082 ) ) ;
#35890 = CARTESIAN_POINT ( 'NONE',  ( 7.644554776091147741E-16, 12.48450537969573659, -147.9687500020484094 ) ) ;
#35891 = CARTESIAN_POINT ( 'NONE',  ( -2.121150477449813534E-15, -11.54700538379251284, -125.7500000040967763 ) ) ;
#35892 = DIRECTION ( 'NONE',  ( -0.000000000000000000, -0.000000000000000000, 1.000000000000000000 ) ) ;
#35893 = CARTESIAN_POINT ( 'NONE',  ( 4.999999999999992006, -8.660254037844389075, -161.2500000000000000 ) ) ;
#35894 = CARTESIAN_POINT ( 'NONE',  ( -10.00000000000000000, -5.773502691896252870, -168.0000000040968189 ) ) ;
#35895 = VECTOR ( 'NONE', #42013, 1000.000000000000000 ) ;
#35896 = CARTESIAN_POINT ( 'NONE',  ( 5.405949406249999534, 9.363379034771803333, -76.09375000204838102 ) ) ;
#35897 = CARTESIAN_POINT ( 'NONE',  ( 10.81189881249999551, -6.242252689847874514, -51.15625000204838813 ) ) ;
#35898 = CARTESIAN_POINT ( 'NONE',  ( -10.81189881249999729, 1.324075727343319199E-15, -54.59375000204835970 ) ) ;
#35899 = DIRECTION ( 'NONE',  ( -1.000000000000000000, 0.000000000000000000, 0.000000000000000000 ) ) ;
#35900 = CARTESIAN_POINT ( 'NONE',  ( 5.405949406249992428, -9.363379034771808662, -160.5937500020484094 ) ) ;
#35901 = CARTESIAN_POINT ( 'NONE',  ( -10.00000000000000000, -5.773502691896251982, -139.1250000000000000 ) ) ;
#35902 = CARTESIAN_POINT ( 'NONE',  ( -5.405949406249996869, 9.363379034771805109, -139.0312500020484094 ) ) ;
#35903 = CARTESIAN_POINT ( 'NONE',  ( 0.000000000000000000, 0.000000000000000000, -99.99999999999998579 ) ) ;
#35904 = CARTESIAN_POINT ( 'NONE',  ( -9.999999999999998224, 5.773502691896259087, -114.2500000040967905 ) ) ;
#35905 = CARTESIAN_POINT ( 'NONE',  ( 5.000000000000000000, 8.660254037844385522, -93.24999999999998579 ) ) ;
#35906 = VERTEX_POINT ( 'NONE', #10509 ) ;
#35907 = CARTESIAN_POINT ( 'NONE',  ( 7.644554776091147741E-16, 12.48450537969573659, -116.6562500020483952 ) ) ;
#35908 = CARTESIAN_POINT ( 'NONE',  ( -9.999999999999998224, 5.773502691896259087, -136.7500000040967905 ) ) ;
#35909 = FACE_OUTER_BOUND ( 'NONE', #15781, .T. ) ;
#35910 = CARTESIAN_POINT ( 'NONE',  ( 5.405949406249999534, 9.363379034771803333, -175.2812500020484094 ) ) ;
#35911 = CARTESIAN_POINT ( 'NONE',  ( -9.999999999999998224, 1.224646799147353059E-15, -40.62500000409677625 ) ) ;
#35912 = ADVANCED_FACE ( 'NONE', ( #20439 ), #32986, .F. ) ;
#35913 = DIRECTION ( 'NONE',  ( -0.000000000000000000, -0.000000000000000000, -1.000000000000000000 ) ) ;
#35914 = CARTESIAN_POINT ( 'NONE',  ( 5.405949406249999534, 9.363379034771803333, -58.28125000204836681 ) ) ;
#35915 = CARTESIAN_POINT ( 'NONE',  ( -10.00000000000051337, 5.773502691895962435, -73.37499999999995737 ) ) ;
#35916 = CARTESIAN_POINT ( 'NONE',  ( 5.405949406249992428, -9.363379034771808662, -159.2812500020484094 ) ) ;
#35917 = CARTESIAN_POINT ( 'NONE',  ( -5.405949406249996869, 9.363379034771805109, -140.3437500020484094 ) ) ;
#35918 = ORIENTED_EDGE ( 'NONE', *, *, #22174, .T. ) ;
#35919 = CARTESIAN_POINT ( 'NONE',  ( 10.00000000000154010, -5.773502691895370020, -30.62499999999991118 ) ) ;
#35920 = AXIS2_PLACEMENT_3D ( 'NONE', #14987, #29029, #12180 ) ;
#35922 = EDGE_LOOP ( 'NONE', ( #30666, #23644, #33232, #10213 ) ) ;
#35921 = CARTESIAN_POINT ( 'NONE',  ( 10.81189881249999551, -6.242252689847874514, -70.65625000204839523 ) ) ;
#35924 = EDGE_LOOP ( 'NONE', ( #40834, #17211, #29777, #36581 ) ) ;
#35923 = CARTESIAN_POINT ( 'NONE',  ( -5.405949406250003975, -9.363379034771801557, -121.8437500020483952 ) ) ;
#35925 = EDGE_LOOP ( 'NONE', ( #20499, #11210, #6416, #15472 ) ) ;
#35926 = CARTESIAN_POINT ( 'NONE',  ( 10.81189881249999729, 6.242252689847867408, -26.71875000204837391 ) ) ;
#35927 = CARTESIAN_POINT ( 'NONE',  ( -10.81189881249999729, 6.242252689847871849, -0.9062500020483681418 ) ) ;
#35928 = CARTESIAN_POINT ( 'NONE',  ( -2.293366432827344421E-15, -12.48450537969573659, -45.21875000204836681 ) ) ;
#35929 = CARTESIAN_POINT ( 'NONE',  ( -10.00000000000000000, -5.773502691896251982, -32.62499999999995737 ) ) ;
#35930 = CARTESIAN_POINT ( 'NONE',  ( -10.81189881249999729, -6.242252689847864744, -190.9687500020484094 ) ) ;
#35931 = CARTESIAN_POINT ( 'NONE',  ( 10.81189881249999551, -6.242252689847874514, -172.4687500020484094 ) ) ;
#35932 =( BOUNDED_CURVE ( )  B_SPLINE_CURVE ( 2, ( #9088, #18369, #11886, #25294, #35216, #25082, #8881 ),
 .UNSPECIFIED., .F., .F. ) 
 B_SPLINE_CURVE_WITH_KNOTS ( ( 3, 2, 2, 3 ),
 ( 0.9589552238805971740, 0.9601990049751244483, 0.9614427860696519446, 0.9626865671641793298 ),
 .UNSPECIFIED. ) 
 CURVE ( )  GEOMETRIC_REPRESENTATION_ITEM ( )  RATIONAL_B_SPLINE_CURVE ( ( 0.9999999999999880096, 0.8660254037844506980, 1.000000000000000000, 0.8660254037844387076, 1.000000000000000000, 0.8660254037844148378, 1.000000000000023981 ) ) 
 REPRESENTATION_ITEM ( '' )  );
#35933 = CARTESIAN_POINT ( 'NONE',  ( -5.405949406250003975, -9.363379034771801557, -151.8437500020483810 ) ) ;
#35934 = CARTESIAN_POINT ( 'NONE',  ( -5.405949406250003975, -9.363379034771801557, -168.3437500020484094 ) ) ;
#35935 = CARTESIAN_POINT ( 'NONE',  ( -10.00000000000102496, 5.773502691895664007, -40.75000000409673362 ) ) ;
#35936 = CARTESIAN_POINT ( 'NONE',  ( 9.999999999998456346, 5.773502691897149042, -20.25000000409673717 ) ) ;
#35937 = CARTESIAN_POINT ( 'NONE',  ( -4.999999999999996447, 8.660254037844387298, -186.0000000000000000 ) ) ;
#35938 = CARTESIAN_POINT ( 'NONE',  ( -10.81189881249999729, 1.324075727343319199E-15, -96.59375000204838102 ) ) ;
#35939 = CARTESIAN_POINT ( 'NONE',  ( -9.999999999998969713, -5.773502691896847949, -85.12499999999995737 ) ) ;
#35940 = CARTESIAN_POINT ( 'NONE',  ( 10.81189881249999907, 6.242252689847868297, -76.40625000204839523 ) ) ;
#35941 = CARTESIAN_POINT ( 'NONE',  ( -5.000000000000003553, -8.660254037844383745, -160.0000000000000000 ) ) ;
#35942 = CARTESIAN_POINT ( 'NONE',  ( 5.405949406249999534, 9.363379034771803333, -184.0937500020483810 ) ) ;
#35943 = CARTESIAN_POINT ( 'NONE',  ( -10.81189881249999729, 6.242252689847871849, -81.71875000204838102 ) ) ;
#35944 = CARTESIAN_POINT ( 'NONE',  ( 5.405949406249999534, 9.363379034771803333, -64.28125000204836681 ) ) ;
#35945 = CARTESIAN_POINT ( 'NONE',  ( -5.000000000000003553, -8.660254037844383745, -134.8750000040967905 ) ) ;
#35946 = CARTESIAN_POINT ( 'NONE',  ( -2.121150477449813534E-15, -11.54700538379251284, -113.3749999999999858 ) ) ;
#35947 = VECTOR ( 'NONE', #39062, 1000.000000000000000 ) ;
#35948 = ORIENTED_EDGE ( 'NONE', *, *, #1695, .F. ) ;
#35949 = CARTESIAN_POINT ( 'NONE',  ( -10.81189881249999729, 6.242252689847871849, -141.9062500020484094 ) ) ;
#35950 = CARTESIAN_POINT ( 'NONE',  ( 10.81189881249999551, -6.242252689847874514, -157.6562500020484094 ) ) ;
#35951 = APPROVAL_PERSON_ORGANIZATION ( #10536, #30720, #33011 ) ;
#35952 = CARTESIAN_POINT ( 'NONE',  ( 10.81189881249999907, 6.242252689847868297, -197.9062500020484379 ) ) ;
#35953 = CARTESIAN_POINT ( 'NONE',  ( 10.00000000000102318, -5.773502691895667560, -38.12499999999992184 ) ) ;
#35954 = CARTESIAN_POINT ( 'NONE',  ( 10.81189881249999729, 0.000000000000000000, -92.84375000204838102 ) ) ;
#35955 = ORIENTED_EDGE ( 'NONE', *, *, #23459, .T. ) ;
#35956 = CARTESIAN_POINT ( 'NONE',  ( -4.999999999999996447, 8.660254037844387298, -55.49999999999996447 ) ) ;
#35957 = CARTESIAN_POINT ( 'NONE',  ( 7.644554776091147741E-16, 12.48450537969573659, -189.9687500020484094 ) ) ;
#35958 = CARTESIAN_POINT ( 'NONE',  ( -4.999999999999996447, 8.660254037844387298, -76.87500000409677625 ) ) ;
#35959 = ADVANCED_FACE ( 'NONE', ( #33836 ), #1029, .T. ) ;
#35960 = CARTESIAN_POINT ( 'NONE',  ( -4.999999999999996447, 8.660254037844387298, -65.99999999999997158 ) ) ;
#35961 = FACE_OUTER_BOUND ( 'NONE', #33901, .T. ) ;
#35962 = ADVANCED_FACE ( 'NONE', ( #195 ), #26505, .T. ) ;
#35963 = CARTESIAN_POINT ( 'NONE',  ( -2.293366432827344421E-15, -12.48450537969573659, -82.90625000204838102 ) ) ;
#35964 = CARTESIAN_POINT ( 'NONE',  ( -10.81189881249999729, -6.242252689847864744, -71.15625000204839523 ) ) ;
#35965 = ADVANCED_FACE ( 'NONE', ( #1674 ), #31671, .T. ) ;
#35966 = CARTESIAN_POINT ( 'NONE',  ( -4.999999999999996447, 8.660254037844387298, -61.87500000409676204 ) ) ;
#35967 = CARTESIAN_POINT ( 'NONE',  ( -10.81189881249999907, -6.242252689847864744, -19.96875000204837036 ) ) ;
#35968 = DIRECTION ( 'NONE',  ( -0.000000000000000000, -0.000000000000000000, 1.000000000000000000 ) ) ;
#35969 = CARTESIAN_POINT ( 'NONE',  ( 5.405949406249999534, 9.363379034771803333, -187.2812500020484094 ) ) ;
#35970 = CIRCLE ( 'NONE', #41472, 35.00000000000000711 ) ;
#35971 = CARTESIAN_POINT ( 'NONE',  ( 10.81189881249999729, 0.000000000000000000, -9.031250002048352599 ) ) ;
#35972 = CARTESIAN_POINT ( 'NONE',  ( 7.070501591499376803E-16, 11.54700538379251284, -186.5000000040968189 ) ) ;
#35973 = CARTESIAN_POINT ( 'NONE',  ( 80.00000000000002842, -20.00000000000001421, -160.0000000000000000 ) ) ;
#35974 = PRODUCT_RELATED_PRODUCT_CATEGORY ( 'detail', '', ( #2800 ) ) ;
#35975 = CARTESIAN_POINT ( 'NONE',  ( -9.999999999999998224, 1.224646799147353059E-15, -124.6250000040967763 ) ) ;
#35976 = CARTESIAN_POINT ( 'NONE',  ( -10.00000000000000000, -5.773502691896251982, -166.1249999999999716 ) ) ;
#35978 = VERTEX_POINT ( 'NONE', #24988 ) ;
#35977 = CARTESIAN_POINT ( 'NONE',  ( 10.81189881249999729, 0.000000000000000000, -93.03125000204838102 ) ) ;
#35979 = CARTESIAN_POINT ( 'NONE',  ( -5.000000000000003553, -8.660254037844383745, -160.3750000040967905 ) ) ;
#35980 = EDGE_CURVE ( 'NONE', #31308, #32304, #9505, .T. ) ;
#35982 = VERTEX_POINT ( 'NONE', #34049 ) ;
#35981 = CARTESIAN_POINT ( 'NONE',  ( 5.405949406249999534, 9.363379034771803333, -103.0937500020483810 ) ) ;
#35983 = ORIENTED_EDGE ( 'NONE', *, *, #30362, .F. ) ;
#35984 =( BOUNDED_CURVE ( )  B_SPLINE_CURVE ( 2, ( #20865, #28434, #12626, #12209, #26032, #35953, #25198 ),
 .UNSPECIFIED., .F., .F. ) 
 B_SPLINE_CURVE_WITH_KNOTS ( ( 3, 2, 2, 3 ),
 ( 0.8022388059701494045, 0.8034825870646766788, 0.8047263681592041751, 0.8059701492537315604 ),
 .UNSPECIFIED. ) 
 CURVE ( )  GEOMETRIC_REPRESENTATION_ITEM ( )  RATIONAL_B_SPLINE_CURVE ( ( 0.9999999999999880096, 0.8660254037844506980, 1.000000000000000000, 0.8660254037844387076, 1.000000000000000000, 0.8660254037844148378, 1.000000000000023981 ) ) 
 REPRESENTATION_ITEM ( '' )  );
#35985 = CARTESIAN_POINT ( 'NONE',  ( 5.405949406249992428, -9.363379034771808662, -37.59375000204837391 ) ) ;
#35986 = CARTESIAN_POINT ( 'NONE',  ( 5.405949406249999534, 9.363379034771803333, -23.78125000204836681 ) ) ;
#35987 = DATE_AND_TIME ( #38371, #11131 ) ;
#35988 = EDGE_CURVE ( 'NONE', #10458, #6, #22748, .T. ) ;
#35989 = CARTESIAN_POINT ( 'NONE',  ( -10.81189881249999729, 6.242252689847871849, -75.71875000204836681 ) ) ;
#35990 = CARTESIAN_POINT ( 'NONE',  ( -9.999999999999998224, 1.224646799147353059E-15, -174.1250000040968189 ) ) ;
#35991 = CARTESIAN_POINT ( 'NONE',  ( 10.81189881249999551, -6.242252689847874514, -196.4687500020484094 ) ) ;
#35992 = CARTESIAN_POINT ( 'NONE',  ( -10.00000000000051337, 5.773502691895962435, -72.25000000409674783 ) ) ;
#35993 = CARTESIAN_POINT ( 'NONE',  ( -2.121150477449813534E-15, -11.54700538379251284, -143.7500000040967905 ) ) ;
#35994 = CARTESIAN_POINT ( 'NONE',  ( 7.644554776091147741E-16, 12.48450537969573659, -154.1562500020484094 ) ) ;
#35995 = CARTESIAN_POINT ( 'NONE',  ( -10.00000000000000000, -5.773502691896251982, -6.000000004096739836 ) ) ;
#35996 = CARTESIAN_POINT ( 'NONE',  ( -4.999999999999996447, 8.660254037844387298, -121.5000000000000000 ) ) ;
#35997 = CARTESIAN_POINT ( 'NONE',  ( 7.644554776091147741E-16, 12.48450537969573659, -117.9687500020483668 ) ) ;
#35998 = CARTESIAN_POINT ( 'NONE',  ( 7.644554776091147741E-16, 12.48450537969573659, -100.1562500020483952 ) ) ;
#35999 = CARTESIAN_POINT ( 'NONE',  ( 10.81189881249999729, 6.242252689847867408, -104.7187500020483810 ) ) ;
#36000 = EDGE_CURVE ( 'NONE', #4655, #22659, #11359, .T. ) ;
#36001 = CARTESIAN_POINT ( 'NONE',  ( -5.405949406249996869, 9.363379034771805109, -75.84375000204838102 ) ) ;
#36002 = CARTESIAN_POINT ( 'NONE',  ( 7.644554776091147741E-16, 12.48450537969573659, -83.65625000204838102 ) ) ;
#36003 = CARTESIAN_POINT ( 'NONE',  ( 4.999999999999992006, -8.660254037844389075, -169.1250000040967905 ) ) ;
#36004 = CARTESIAN_POINT ( 'NONE',  ( 5.405949406249999534, 9.363379034771803333, -163.2812500020484094 ) ) ;
#36005 = CARTESIAN_POINT ( 'NONE',  ( 10.81189881249999551, -6.242252689847874514, -177.1562500020484094 ) ) ;
#36006 = CARTESIAN_POINT ( 'NONE',  ( 9.999999999999998224, 0.000000000000000000, -153.8750000040967905 ) ) ;
#36007 = FACE_OUTER_BOUND ( 'NONE', #36665, .T. ) ;
#36008 = CARTESIAN_POINT ( 'NONE',  ( 10.81189881249999729, 0.000000000000000000, -5.843750002048370362 ) ) ;
#36009 = CARTESIAN_POINT ( 'NONE',  ( -5.000000000000003553, -8.660254037844383745, -59.87500000409676204 ) ) ;
#36010 = CARTESIAN_POINT ( 'NONE',  ( 10.81189881249999907, 6.242252689847868297, -116.7187500020483810 ) ) ;
#36011 = CARTESIAN_POINT ( 'NONE',  ( 5.000000000000000000, 8.660254037844385522, -84.24999999999997158 ) ) ;
#36012 = CARTESIAN_POINT ( 'NONE',  ( 5.405949406249992428, -9.363379034771808662, -12.28125000204835438 ) ) ;
#36013 = CARTESIAN_POINT ( 'NONE',  ( 4.999999999999992006, -8.660254037844389075, -95.62500000409677625 ) ) ;
#36014 = CARTESIAN_POINT ( 'NONE',  ( -9.999999999999998224, 1.224646799147353059E-15, -200.0000000000000000 ) ) ;
#36015 = CARTESIAN_POINT ( 'NONE',  ( -5.405949406249996869, 9.363379034771805109, -110.5312500020483810 ) ) ;
#36016 = CARTESIAN_POINT ( 'NONE',  ( -10.81189881249999729, -6.242252689847864744, -89.15625000204836681 ) ) ;
#36017 = VERTEX_POINT ( 'NONE', #27782 ) ;
#36018 = AXIS2_PLACEMENT_3D ( 'NONE', #34728, #20895, #14403 ) ;
#36019 = CARTESIAN_POINT ( 'NONE',  ( -10.00000000000000000, -5.773502691896251982, -81.00000000409677625 ) ) ;
#36020 = DIRECTION ( 'NONE',  ( -0.000000000000000000, -0.000000000000000000, 1.000000000000000000 ) ) ;
#36021 = CARTESIAN_POINT ( 'NONE',  ( -5.405949406250003975, -9.363379034771801557, -42.34375000204837391 ) ) ;
#36022 = ORIENTED_EDGE ( 'NONE', *, *, #34605, .T. ) ;
#36023 = CARTESIAN_POINT ( 'NONE',  ( 7.070501591499377789E-16, 11.54700538379251284, -12.12499999999996270 ) ) ;
#36024 = CARTESIAN_POINT ( 'NONE',  ( -5.000000000000003553, -8.660254037844383745, -145.0000000000000000 ) ) ;
#36025 = CARTESIAN_POINT ( 'NONE',  ( 9.999999999999998224, 0.000000000000000000, -14.37500000409674961 ) ) ;
#36026 = AXIS2_PLACEMENT_3D ( 'NONE', #42524, #9312, #12949 ) ;
#36027 = CARTESIAN_POINT ( 'NONE',  ( 9.999999999999996447, -5.773502691896262640, -198.6250000000000284 ) ) ;
#36028 = ADVANCED_FACE ( 'NONE', ( #27998 ), #14802, .T. ) ;
#36030 = EDGE_LOOP ( 'NONE', ( #37461, #3334, #33214, #28512 ) ) ;
#36029 = CARTESIAN_POINT ( 'NONE',  ( 10.81189881249999907, 6.242252689847868297, -116.9062500020483952 ) ) ;
#36031 = DIRECTION ( 'NONE',  ( 1.000000000000000000, 0.000000000000000000, -0.000000000000000000 ) ) ;
#36032 = VERTEX_POINT ( 'NONE', #2105 ) ;
#36033 = CARTESIAN_POINT ( 'NONE',  ( 10.81189881249999907, 6.242252689847868297, -55.40625000204837391 ) ) ;
#36034 = PERSON_AND_ORGANIZATION_ROLE ( 'design_owner' ) ;
#36035 = CARTESIAN_POINT ( 'NONE',  ( -10.81189881249999729, 6.242252689847871849, -101.2187500020483810 ) ) ;
#36036 = CARTESIAN_POINT ( 'NONE',  ( -5.405949406250003975, -9.363379034771801557, -122.0312500020483952 ) ) ;
#36037 = ORIENTED_EDGE ( 'NONE', *, *, #36084, .F. ) ;
#36038 = DIRECTION ( 'NONE',  ( -1.000000000000000000, 0.000000000000000000, 0.000000000000000000 ) ) ;
#36039 = CARTESIAN_POINT ( 'NONE',  ( -9.999999999999479527, -5.773502691896549521, -116.6249999999999574 ) ) ;
#36040 = CARTESIAN_POINT ( 'NONE',  ( 10.81189881249999729, 0.000000000000000000, -181.5312500020483810 ) ) ;
#36041 = CARTESIAN_POINT ( 'NONE',  ( -2.293366432827344421E-15, -12.48450537969573659, -1.718750002048355929 ) ) ;
#36042 = CARTESIAN_POINT ( 'NONE',  ( -9.999999999999998224, 1.224646799147353059E-15, -154.6250000040967905 ) ) ;
#36043 = CARTESIAN_POINT ( 'NONE',  ( 10.81189881249999729, 0.000000000000000000, -131.8437500020484094 ) ) ;
#36044 = CARTESIAN_POINT ( 'NONE',  ( 10.81189881249999729, 0.000000000000000000, -104.8437500020483810 ) ) ;
#36045 = CARTESIAN_POINT ( 'NONE',  ( -5.000000000000003553, -8.660254037844383745, -158.5000000000000000 ) ) ;
#36046 = CARTESIAN_POINT ( 'NONE',  ( 10.81189881249999729, 0.000000000000000000, -109.5312500020483810 ) ) ;
#36047 = CARTESIAN_POINT ( 'NONE',  ( -9.999999999999998224, 1.224646799147353059E-15, -195.1250000040967905 ) ) ;
#36048 = CARTESIAN_POINT ( 'NONE',  ( -10.81189881249999729, 6.242252689847871849, -117.7187500020483952 ) ) ;
#36049 = CARTESIAN_POINT ( 'NONE',  ( 7.644554776091147741E-16, 12.48450537969573659, -188.6562500020484094 ) ) ;
#36050 = CARTESIAN_POINT ( 'NONE',  ( -9.999999999999998224, 1.224646799147353059E-15, -186.1250000040967905 ) ) ;
#36051 = CARTESIAN_POINT ( 'NONE',  ( 9.999999999999996447, -5.773502691896262640, -141.6250000000000000 ) ) ;
#36052 = CARTESIAN_POINT ( 'NONE',  ( 10.00000000000000000, 5.773502691896255534, -6.374999999999963585 ) ) ;
#36053 = CARTESIAN_POINT ( 'NONE',  ( 10.81189881249999729, 0.000000000000000000, -61.34375000204836681 ) ) ;
#36054 = CARTESIAN_POINT ( 'NONE',  ( -2.293366432827344421E-15, -12.48450537969573659, -52.71875000204837391 ) ) ;
#36055 = DESIGN_CONTEXT ( 'detailed design', #17898, 'design' ) ;
#36056 = CARTESIAN_POINT ( 'NONE',  ( 9.999999999999996447, -5.773502691896262640, -181.0000000040968189 ) ) ;
#36057 = CARTESIAN_POINT ( 'NONE',  ( -10.81189881249999729, 1.324075727343319199E-15, -21.78125000204836326 ) ) ;
#36058 = CARTESIAN_POINT ( 'NONE',  ( -5.405949406250003975, -9.363379034771801557, -30.34375000204836326 ) ) ;
#36059 = CARTESIAN_POINT ( 'NONE',  ( -9.999999999998456346, -5.773502691897145489, -8.624999999999937828 ) ) ;
#36060 = CARTESIAN_POINT ( 'NONE',  ( -10.81189881249999729, 1.324075727343319199E-15, -141.5937500020483810 ) ) ;
#36061 = CARTESIAN_POINT ( 'NONE',  ( 7.070501591499377789E-16, 11.54700538379251284, -106.6249999999999716 ) ) ;
#36062 = CARTESIAN_POINT ( 'NONE',  ( 9.999999999999998224, 0.000000000000000000, -164.0000000000000000 ) ) ;
#36063 = CARTESIAN_POINT ( 'NONE',  ( -2.121150477449813534E-15, -11.54700538379251284, -69.87500000000000000 ) ) ;
#36064 = CARTESIAN_POINT ( 'NONE',  ( 5.405949406249999534, 9.363379034771803333, -134.7812500020483810 ) ) ;
#36065 = CARTESIAN_POINT ( 'NONE',  ( -5.405949406249996869, 9.363379034771805109, -119.5312500020483952 ) ) ;
#36066 = ORIENTED_EDGE ( 'NONE', *, *, #19118, .T. ) ;
#36067 = CARTESIAN_POINT ( 'NONE',  ( 9.999999999999998224, 0.000000000000000000, -108.8750000040967763 ) ) ;
#36068 = CARTESIAN_POINT ( 'NONE',  ( -9.999999999999998224, 1.224646799147353059E-15, -113.7499999999999858 ) ) ;
#36069 = CARTESIAN_POINT ( 'NONE',  ( 10.81189881249999907, 6.242252689847868297, -64.21875000204838102 ) ) ;
#36070 = ORIENTED_EDGE ( 'NONE', *, *, #10961, .T. ) ;
#36071 = CARTESIAN_POINT ( 'NONE',  ( -4.999999999999996447, 8.660254037844387298, -41.99999999999997868 ) ) ;
#36072 = CARTESIAN_POINT ( 'NONE',  ( 10.00000000000000000, 5.773502691896255534, -15.75000000409677270 ) ) ;
#36073 = CARTESIAN_POINT ( 'NONE',  ( 7.644554776091147741E-16, 12.48450537969573659, -44.65625000204836681 ) ) ;
#36074 = CARTESIAN_POINT ( 'NONE',  ( -2.121150477449813534E-15, -11.54700538379251284, -131.7500000040967905 ) ) ;
#36075 = CARTESIAN_POINT ( 'NONE',  ( -10.00000000000000000, -5.773502691896251982, -33.00000000409675494 ) ) ;
#36076 = CARTESIAN_POINT ( 'NONE',  ( 7.070501591499376803E-16, 11.54700538379251284, -117.5000000040967905 ) ) ;
#36077 = CARTESIAN_POINT ( 'NONE',  ( -10.81189881249999907, -6.242252689847864744, -135.6562500020484094 ) ) ;
#36078 = ADVANCED_FACE ( 'NONE', ( #14592, #27568 ), #7717, .F. ) ;
#36079 = CARTESIAN_POINT ( 'NONE',  ( 10.81189881249999729, 0.000000000000000000, -144.0312500020483810 ) ) ;
#36080 = CARTESIAN_POINT ( 'NONE',  ( 5.000000000000000000, 8.660254037844385522, -150.6250000040967905 ) ) ;
#36081 = VERTEX_POINT ( 'NONE', #40917 ) ;
#36082 = EDGE_LOOP ( 'NONE', ( #12911, #28296, #40514, #21901 ) ) ;
#36083 = VERTEX_POINT ( 'NONE', #15236 ) ;
#36084 = EDGE_CURVE ( 'NONE', #16838, #12159, #27155, .T. ) ;
#36085 = CARTESIAN_POINT ( 'NONE',  ( 9.999999999999998224, 0.000000000000000000, -103.9999999999999858 ) ) ;
#36086 = CARTESIAN_POINT ( 'NONE',  ( 7.644554776091147741E-16, 12.48450537969573659, -173.4687500020483810 ) ) ;
#36087 = CARTESIAN_POINT ( 'NONE',  ( -10.81189881249999907, -6.242252689847864744, -25.96875000204837391 ) ) ;
#36088 = CARTESIAN_POINT ( 'NONE',  ( -4.999999999999996447, 8.660254037844387298, -111.3750000040967763 ) ) ;
#36089 = CARTESIAN_POINT ( 'NONE',  ( -10.81189881249999729, 6.242252689847871849, -159.7187500020483810 ) ) ;
#36090 = CARTESIAN_POINT ( 'NONE',  ( -5.405949406250003975, -9.363379034771801557, -141.3437500020483810 ) ) ;
#36091 = FACE_OUTER_BOUND ( 'NONE', #16575, .T. ) ;
#36092 = CARTESIAN_POINT ( 'NONE',  ( 7.644554776091147741E-16, 12.48450537969573659, -126.9687500020483668 ) ) ;
#36093 = CARTESIAN_POINT ( 'NONE',  ( -5.405949406250003975, -9.363379034771801557, -131.0312500020484094 ) ) ;
#36095 = CARTESIAN_POINT ( 'NONE',  ( -10.81189881249999907, -6.242252689847864744, -21.46875000204836681 ) ) ;
#36094 =( BOUNDED_CURVE ( )  B_SPLINE_CURVE ( 2, ( #41206, #27859, #34771, #14228, #21805, #28289, #11009 ),
 .UNSPECIFIED., .F., .F. ) 
 B_SPLINE_CURVE_WITH_KNOTS ( ( 3, 2, 2, 3 ),
 ( 0.6119402985074627876, 0.6131840796019901729, 0.6144278606965176692, 0.6156716417910449435 ),
 .UNSPECIFIED. ) 
 CURVE ( )  GEOMETRIC_REPRESENTATION_ITEM ( )  RATIONAL_B_SPLINE_CURVE ( ( 0.9999999999999880096, 0.8660254037844506980, 1.000000000000000000, 0.8660254037844387076, 1.000000000000000000, 0.8660254037844148378, 1.000000000000023981 ) ) 
 REPRESENTATION_ITEM ( '' )  );
#36096 = CARTESIAN_POINT ( 'NONE',  ( -5.405949406249996869, 9.363379034771805109, -141.8437500020483810 ) ) ;
#36097 = CYLINDRICAL_SURFACE ( 'NONE', #14323, 9.999999999999998224 ) ;
#36098 = CARTESIAN_POINT ( 'NONE',  ( -9.999999999999998224, 1.224646799147353059E-15, -28.24999999999996803 ) ) ;
#36099 = CARTESIAN_POINT ( 'NONE',  ( 9.999999999999996447, -5.773502691896262640, -165.6250000000000000 ) ) ;
#36100 = CARTESIAN_POINT ( 'NONE',  ( 9.999999999999998224, 0.000000000000000000, -174.5000000000000284 ) ) ;
#36101 = CARTESIAN_POINT ( 'NONE',  ( -10.81189881249999907, -6.242252689847864744, -72.46875000204835260 ) ) ;
#36102 = CARTESIAN_POINT ( 'NONE',  ( -10.81189881249999729, 1.324075727343319199E-15, -42.78125000204838102 ) ) ;
#36103 = CARTESIAN_POINT ( 'NONE',  ( -10.81189881249999729, 6.242252689847871849, -56.21875000204837391 ) ) ;
#36104 = CARTESIAN_POINT ( 'NONE',  ( 9.999999999999866773, -5.773502691896336358, -174.6249999999999716 ) ) ;
#36105 = CARTESIAN_POINT ( 'NONE',  ( -10.81189881249999729, 1.324075727343319199E-15, -159.5937500020484094 ) ) ;
#36106 = CARTESIAN_POINT ( 'NONE',  ( -9.999999999999998224, 1.224646799147353059E-15, -140.7500000000000000 ) ) ;
#36107 = CARTESIAN_POINT ( 'NONE',  ( -2.293366432827344421E-15, -12.48450537969573659, -135.4062500020483810 ) ) ;
#36108 = CARTESIAN_POINT ( 'NONE',  ( -5.000000000000003553, -8.660254037844383745, -98.87500000409677625 ) ) ;
#36109 = CARTESIAN_POINT ( 'NONE',  ( -4.999999999999996447, 8.660254037844387298, -111.3750000040967763 ) ) ;
#36110 = CARTESIAN_POINT ( 'NONE',  ( -2.121150477449813534E-15, -11.54700538379251284, -87.87499999999997158 ) ) ;
#36111 = VERTEX_POINT ( 'NONE', #31454 ) ;
#36112 =( BOUNDED_CURVE ( )  B_SPLINE_CURVE ( 2, ( #27984, #37473, #41113, #1443, #1017, #14137, #11346 ),
 .UNSPECIFIED., .F., .F. ) 
 B_SPLINE_CURVE_WITH_KNOTS ( ( 3, 2, 2, 3 ),
 ( 0.8843283582089555006, 0.8855721393034827749, 0.8868159203980102712, 0.8880597014925376564 ),
 .UNSPECIFIED. ) 
 CURVE ( )  GEOMETRIC_REPRESENTATION_ITEM ( )  RATIONAL_B_SPLINE_CURVE ( ( 0.9999999999999761302, 0.8660254037844625774, 1.000000000000000000, 0.8660254037844387076, 1.000000000000000000, 0.8660254037844028474, 1.000000000000035971 ) ) 
 REPRESENTATION_ITEM ( '' )  );
#36113 = CARTESIAN_POINT ( 'NONE',  ( 10.81189881249999729, 0.000000000000000000, -120.0312500020483952 ) ) ;
#36114 = CARTESIAN_POINT ( 'NONE',  ( -9.999999999999998224, 1.224646799147353059E-15, -133.6250000040967620 ) ) ;
#36115 = CARTESIAN_POINT ( 'NONE',  ( 10.00000000000051159, -5.773502691895965988, -140.5000000040967620 ) ) ;
#36116 = CARTESIAN_POINT ( 'NONE',  ( -10.81189881249999907, -6.242252689847864744, -173.1562500020484094 ) ) ;
#36117 = CARTESIAN_POINT ( 'NONE',  ( 10.00000000000000000, 5.773502691896255534, -39.75000000409675494 ) ) ;
#36118 = CARTESIAN_POINT ( 'NONE',  ( -5.000000000000003553, -8.660254037844383745, -91.37500000409677625 ) ) ;
#36119 = CARTESIAN_POINT ( 'NONE',  ( -2.293366432827344421E-15, -12.48450537969573659, -60.40625000204838813 ) ) ;
#36120 = EDGE_CURVE ( 'NONE', #38469, #35463, #31587, .T. ) ;
#36121 =( BOUNDED_CURVE ( )  B_SPLINE_CURVE ( 2, ( #12325, #19027, #38881, #8691, #16184, #42315, #15562 ),
 .UNSPECIFIED., .F., .F. ) 
 B_SPLINE_CURVE_WITH_KNOTS ( ( 3, 2, 2, 3 ),
 ( 0.5559701492537315604, 0.5572139303482589456, 0.5584577114427863309, 0.5597014925373136052 ),
 .UNSPECIFIED. ) 
 CURVE ( )  GEOMETRIC_REPRESENTATION_ITEM ( )  RATIONAL_B_SPLINE_CURVE ( ( 0.9999999999999761302, 0.8660254037844625774, 1.000000000000000000, 0.8660254037844387076, 1.000000000000000000, 0.8660254037844148378, 1.000000000000023981 ) ) 
 REPRESENTATION_ITEM ( '' )  );
#36122 = CARTESIAN_POINT ( 'NONE',  ( -5.321294541346989426, 5.321294541346989426, -220.0000000000000000 ) ) ;
#36123 = CARTESIAN_POINT ( 'NONE',  ( -10.81189881249999907, -6.242252689847864744, -159.6562500020484094 ) ) ;
#36124 = CARTESIAN_POINT ( 'NONE',  ( 10.81189881249999551, -6.242252689847874514, -139.4687500020483810 ) ) ;
#36125 = CARTESIAN_POINT ( 'NONE',  ( -9.999999999999998224, 1.224646799147353059E-15, -46.24999999999998579 ) ) ;
#36126 = CARTESIAN_POINT ( 'NONE',  ( -9.999999999999998224, 1.224646799147353059E-15, -173.7500000000000284 ) ) ;
#36127 = VERTEX_POINT ( 'NONE', #40487 ) ;
#36128 = CARTESIAN_POINT ( 'NONE',  ( 10.00000000000051159, -5.773502691895965988, -78.62499999999997158 ) ) ;
#36130 = ORIENTED_EDGE ( 'NONE', *, *, #9486, .F. ) ;
#36129 = CARTESIAN_POINT ( 'NONE',  ( -10.81189881249999729, 1.324075727343319199E-15, -68.28125000204838102 ) ) ;
#36131 = COORDINATED_UNIVERSAL_TIME_OFFSET ( 6, 0, .AHEAD. ) ;
#36133 = ORIENTED_EDGE ( 'NONE', *, *, #25690, .F. ) ;
#36132 = CARTESIAN_POINT ( 'NONE',  ( 10.81189881249999907, 6.242252689847868297, -116.7187500020483810 ) ) ;
#36134 = VERTEX_POINT ( 'NONE', #10933 ) ;
#36135 = CARTESIAN_POINT ( 'NONE',  ( 10.81189881249999729, 6.242252689847867408, -23.71875000204836681 ) ) ;
#36136 = CARTESIAN_POINT ( 'NONE',  ( -10.81189881249999729, 1.324075727343319199E-15, -198.5937500020484094 ) ) ;
#36137 = CARTESIAN_POINT ( 'NONE',  ( 5.405949406249992428, -9.363379034771808662, -48.09375000204838102 ) ) ;
#36138 = CARTESIAN_POINT ( 'NONE',  ( -9.999999999999227285, -5.773502691896698735, -134.6249999999999716 ) ) ;
#36139 = EDGE_CURVE ( 'NONE', #14232, #34637, #35984, .T. ) ;
#36140 = CARTESIAN_POINT ( 'NONE',  ( 9.999999999999998224, 0.000000000000000000, -25.99999999999996803 ) ) ;
#36141 = CARTESIAN_POINT ( 'NONE',  ( -2.293366432827344421E-15, -12.48450537969573659, -177.2187500020484094 ) ) ;
#36142 = CARTESIAN_POINT ( 'NONE',  ( 10.81189881249999729, 0.000000000000000000, -170.8437500020484094 ) ) ;
#36143 = CARTESIAN_POINT ( 'NONE',  ( 10.81189881249999729, 0.000000000000000000, -151.3437500020483810 ) ) ;
#36144 = CARTESIAN_POINT ( 'NONE',  ( -2.293366432827344421E-15, -12.48450537969573659, -163.7187500020483810 ) ) ;
#36145 = CARTESIAN_POINT ( 'NONE',  ( -2.121150477449813534E-15, -11.54700538379251284, -104.7500000040967763 ) ) ;
#36146 = CARTESIAN_POINT ( 'NONE',  ( -9.999999999999998224, 5.773502691896259087, -190.3750000000000000 ) ) ;
#36147 = CARTESIAN_POINT ( 'NONE',  ( -5.405949406249996869, 9.363379034771805109, -93.84375000204838102 ) ) ;
#36148 = CARTESIAN_POINT ( 'NONE',  ( -9.999999999999998224, 1.224646799147353059E-15, -108.1250000040967763 ) ) ;
#36149 = CARTESIAN_POINT ( 'NONE',  ( -10.81189881249999907, -6.242252689847864744, -71.15625000204839523 ) ) ;
#36150 = CARTESIAN_POINT ( 'NONE',  ( 9.999999999999998224, 0.000000000000000000, -4.999999999999976907 ) ) ;
#36151 = CARTESIAN_POINT ( 'NONE',  ( 10.81189881249999551, -6.242252689847874514, -184.4687500020483810 ) ) ;
#36152 = CARTESIAN_POINT ( 'NONE',  ( 7.644554776091147741E-16, 12.48450537969573659, -161.6562500020484094 ) ) ;
#36153 = CARTESIAN_POINT ( 'NONE',  ( 10.81189881249999907, 6.242252689847868297, -59.90625000204838102 ) ) ;
#36154 = CARTESIAN_POINT ( 'NONE',  ( 4.999999999999992006, -8.660254037844389075, -140.6250000040967905 ) ) ;
#36155 = CARTESIAN_POINT ( 'NONE',  ( -10.00000000000000000, -5.773502691896251982, -116.6249999999999858 ) ) ;
#36156 = ORIENTED_EDGE ( 'NONE', *, *, #22506, .T. ) ;
#36157 = CARTESIAN_POINT ( 'NONE',  ( -10.81189881249999729, 1.324075727343319199E-15, -144.7812500020483810 ) ) ;
#36158 = CARTESIAN_POINT ( 'NONE',  ( -10.81189881249999729, 1.324075727343319199E-15, -153.7812500020484094 ) ) ;
#36159 = DIRECTION ( 'NONE',  ( -0.000000000000000000, -1.000000000000000000, -0.000000000000000000 ) ) ;
#36160 = FACE_OUTER_BOUND ( 'NONE', #16412, .T. ) ;
#36161 = CARTESIAN_POINT ( 'NONE',  ( -2.293366432827344421E-15, -12.48450537969573659, -90.21875000204838102 ) ) ;
#36162 = ORIENTED_EDGE ( 'NONE', *, *, #42434, .T. ) ;
#36163 = CARTESIAN_POINT ( 'NONE',  ( -10.00000000000000000, -5.773502691896251982, -58.12499999999998579 ) ) ;
#36164 = CARTESIAN_POINT ( 'NONE',  ( 10.81189881249999729, 0.000000000000000000, -188.8437500020483810 ) ) ;
#36165 = CARTESIAN_POINT ( 'NONE',  ( -10.00000000000000000, -5.773502691896251982, -67.50000000409679046 ) ) ;
#36166 = CARTESIAN_POINT ( 'NONE',  ( 9.999999999999998224, 0.000000000000000000, -168.8750000040967905 ) ) ;
#36167 = DIRECTION ( 'NONE',  ( -0.000000000000000000, -0.000000000000000000, 1.000000000000000000 ) ) ;
#36168 = CARTESIAN_POINT ( 'NONE',  ( -5.405949406250003975, -9.363379034771801557, -84.53125000204838102 ) ) ;
#36169 = CARTESIAN_POINT ( 'NONE',  ( -10.81189881249999729, 6.242252689847871849, -68.40625000204840944 ) ) ;
#36170 = CARTESIAN_POINT ( 'NONE',  ( 5.000000000000000000, 8.660254037844385522, -60.62500000409676204 ) ) ;
#36171 = CARTESIAN_POINT ( 'NONE',  ( 10.81189881249999907, 6.242252689847868297, -20.71875000204837036 ) ) ;
#36172 = CARTESIAN_POINT ( 'NONE',  ( 5.405949406249999534, 9.363379034771803333, -184.2812500020484094 ) ) ;
#36173 = CARTESIAN_POINT ( 'NONE',  ( 7.644554776091147741E-16, 12.48450537969573659, -11.65625000204836859 ) ) ;
#36174 = CARTESIAN_POINT ( 'NONE',  ( 8.614196012143713332, -6.533971456633876684, 2.775557561562891351E-14 ) ) ;
#36175 = CARTESIAN_POINT ( 'NONE',  ( 4.999999999999992006, -8.660254037844389075, -117.7500000000000000 ) ) ;
#36176 = DIRECTION ( 'NONE',  ( -0.000000000000000000, -0.000000000000000000, -1.000000000000000000 ) ) ;
#36177 = CARTESIAN_POINT ( 'NONE',  ( -5.000000000000003553, -8.660254037844383745, -166.0000000000000000 ) ) ;
#36178 = CARTESIAN_POINT ( 'NONE',  ( -9.999999999999998224, 1.224646799147353059E-15, -122.7500000000000000 ) ) ;
#36180 = VERTEX_POINT ( 'NONE', #38770 ) ;
#36179 = CARTESIAN_POINT ( 'NONE',  ( -2.293366432827344421E-15, -12.48450537969573659, -91.90625000204838102 ) ) ;
#36181 = LINE ( 'NONE', #39419, #25553 ) ;
#36183 = EDGE_LOOP ( 'NONE', ( #30676, #24950, #4984, #26211 ) ) ;
#36182 = DIRECTION ( 'NONE',  ( -1.000000000000000000, 0.000000000000000000, 0.000000000000000000 ) ) ;
#36184 =( BOUNDED_CURVE ( )  B_SPLINE_CURVE ( 2, ( #42658, #42447, #13082, #35993, #33612, #26069, #39220 ),
 .UNSPECIFIED., .F., .F. ) 
 B_SPLINE_CURVE_WITH_KNOTS ( ( 3, 2, 2, 3 ),
 ( 0.2723880597014926574, 0.2736318407960199872, 0.2748756218905473725, 0.2761194029850747578 ),
 .UNSPECIFIED. ) 
 CURVE ( )  GEOMETRIC_REPRESENTATION_ITEM ( )  RATIONAL_B_SPLINE_CURVE ( ( 0.9999999999999880096, 0.8660254037844506980, 1.000000000000000000, 0.8660254037844387076, 1.000000000000000000, 0.8660254037844267172, 1.000000000000011990 ) ) 
 REPRESENTATION_ITEM ( '' )  );
#36185 = EDGE_LOOP ( 'NONE', ( #23509, #25323, #31841, #25221 ) ) ;
#36186 = CARTESIAN_POINT ( 'NONE',  ( 7.644554776091147741E-16, 12.48450537969573659, -35.46875000204835260 ) ) ;
#36187 = VECTOR ( 'NONE', #40838, 1000.000000000000000 ) ;
#36188 = CARTESIAN_POINT ( 'NONE',  ( -10.81189881249999907, -6.242252689847864744, -23.15625000204837747 ) ) ;
#36189 = APPROVAL_STATUS ( 'not_yet_approved' ) ;
#36190 = CARTESIAN_POINT ( 'NONE',  ( -5.405949406250003975, -9.363379034771801557, -70.84375000204836681 ) ) ;
#36191 = CARTESIAN_POINT ( 'NONE',  ( 9.999999999999479527, 5.773502691896553074, -105.3749999999999716 ) ) ;
#36192 = EDGE_CURVE ( 'NONE', #530, #13652, #40359, .T. ) ;
#36193 = CARTESIAN_POINT ( 'NONE',  ( 10.81189881249999907, 6.242252689847868297, -190.2187500020484094 ) ) ;
#36194 = EDGE_CURVE ( 'NONE', #36127, #6564, #28853, .T. ) ;
#36195 = CARTESIAN_POINT ( 'NONE',  ( -9.999999999999479527, -5.773502691896549521, -79.50000000409677625 ) ) ;
#36196 = CARTESIAN_POINT ( 'NONE',  ( 5.000000000000000000, 8.660254037844385522, -172.7500000000000284 ) ) ;
#36197 = CARTESIAN_POINT ( 'NONE',  ( 7.644554776091147741E-16, 12.48450537969573659, -155.6562500020484094 ) ) ;
#36198 = CARTESIAN_POINT ( 'NONE',  ( 9.999999999999998224, 0.000000000000000000, -6.875000004096742501 ) ) ;
#36199 = CARTESIAN_POINT ( 'NONE',  ( 10.00000000000102318, -5.773502691895667560, -80.12499999999997158 ) ) ;
#36200 = CARTESIAN_POINT ( 'NONE',  ( 10.81189881249999551, -6.242252689847874514, -118.4687500020483810 ) ) ;
#36201 = CARTESIAN_POINT ( 'NONE',  ( -5.405949406250003975, -9.363379034771801557, -96.53125000204839523 ) ) ;
#36202 = CARTESIAN_POINT ( 'NONE',  ( -10.81189881249999729, 6.242252689847871849, -110.2187500020483810 ) ) ;
#36203 = CARTESIAN_POINT ( 'NONE',  ( -2.293366432827344421E-15, -12.48450537969573659, -79.71875000204838102 ) ) ;
#36204 = AXIS2_PLACEMENT_3D ( 'NONE', #3889, #30437, #868 ) ;
#36205 = CARTESIAN_POINT ( 'NONE',  ( 10.81189881249999729, 0.000000000000000000, -81.03125000204839523 ) ) ;
#36206 = CARTESIAN_POINT ( 'NONE',  ( -9.999999999999998224, 1.224646799147353059E-15, -165.1250000040967905 ) ) ;
#36207 = CARTESIAN_POINT ( 'NONE',  ( 4.999999999999992006, -8.660254037844389075, -66.74999999999997158 ) ) ;
#36208 = CARTESIAN_POINT ( 'NONE',  ( 10.81189881249999729, 6.242252689847867408, -163.4062500020483810 ) ) ;
#36209 = CARTESIAN_POINT ( 'NONE',  ( 5.405949406249999534, 9.363379034771803333, -184.2812500020484094 ) ) ;
#36210 = CARTESIAN_POINT ( 'NONE',  ( 10.00000000000000000, 5.773502691896255534, -155.2500000040967905 ) ) ;
#36211 = CARTESIAN_POINT ( 'NONE',  ( 10.00000000000038369, -5.773502691896038819, -156.6250000000000284 ) ) ;
#36212 = CARTESIAN_POINT ( 'NONE',  ( -2.293366432827344421E-15, -12.48450537969573659, -4.718750002048355263 ) ) ;
#36213 = CARTESIAN_POINT ( 'NONE',  ( 9.999999999999479527, 5.773502691896553074, -108.7500000040967620 ) ) ;
#36214 = CARTESIAN_POINT ( 'NONE',  ( -5.405949406249996869, 9.363379034771805109, -111.8437500020483810 ) ) ;
#36215 = CARTESIAN_POINT ( 'NONE',  ( 7.070501591499377789E-16, 11.54700538379251284, -78.12500000000000000 ) ) ;
#36216 = CARTESIAN_POINT ( 'NONE',  ( 5.405949406249999534, 9.363379034771803333, -10.28125000204835260 ) ) ;
#36217 = CARTESIAN_POINT ( 'NONE',  ( -9.999999999999998224, 5.773502691896259087, -87.25000000409676204 ) ) ;
#36218 = EDGE_CURVE ( 'NONE', #21702, #2376, #21938, .T. ) ;
#36219 = CARTESIAN_POINT ( 'NONE',  ( 9.999999999999998224, 0.000000000000000000, -150.8750000040967905 ) ) ;
#36220 = CARTESIAN_POINT ( 'NONE',  ( 5.405949406249999534, 9.363379034771803333, -107.7812500020483810 ) ) ;
#36221 = CARTESIAN_POINT ( 'NONE',  ( -10.81189881249999729, 1.324075727343319199E-15, -95.28125000204838102 ) ) ;
#36222 = VERTEX_POINT ( 'NONE', #38975 ) ;
#36223 = CARTESIAN_POINT ( 'NONE',  ( 9.999999999999998224, 0.000000000000000000, -80.37500000409677625 ) ) ;
#36224 = DIRECTION ( 'NONE',  ( 0.000000000000000000, -1.000000000000000000, 0.000000000000000000 ) ) ;
#36225 = CARTESIAN_POINT ( 'NONE',  ( 10.81189881249999729, 0.000000000000000000, -44.84375000204837391 ) ) ;
#36226 = ORIENTED_EDGE ( 'NONE', *, *, #3031, .T. ) ;
#36227 = CARTESIAN_POINT ( 'NONE',  ( 4.999999999999992006, -8.660254037844389075, -9.749999999999953815 ) ) ;
#36228 = ADVANCED_FACE ( 'NONE', ( #12418 ), #16073, .T. ) ;
#36229 = CARTESIAN_POINT ( 'NONE',  ( 7.070501591499377789E-16, 11.54700538379251284, -142.6250000000000000 ) ) ;
#36230 = CARTESIAN_POINT ( 'NONE',  ( -9.999999999999998224, 1.224646799147353059E-15, -32.74999999999997158 ) ) ;
#36231 = EDGE_CURVE ( 'NONE', #4695, #28503, #9411, .T. ) ;
#36232 = CARTESIAN_POINT ( 'NONE',  ( -9.999999999999998224, 1.224646799147353059E-15, -15.12500000409674961 ) ) ;
#36233 =( BOUNDED_CURVE ( )  B_SPLINE_CURVE ( 2, ( #5957, #15845, #29249, #19305, #8975, #12611, #25804 ),
 .UNSPECIFIED., .F., .F. ) 
 B_SPLINE_CURVE_WITH_KNOTS ( ( 3, 2, 2, 3 ),
 ( 0.3731343283582090331, 0.3743781094527363629, 0.3756218905472638037, 0.3768656716417911334 ),
 .UNSPECIFIED. ) 
 CURVE ( )  GEOMETRIC_REPRESENTATION_ITEM ( )  RATIONAL_B_SPLINE_CURVE ( ( 0.9999999999999940048, 0.8660254037844447028, 1.000000000000000000, 0.8660254037844387076, 1.000000000000000000, 0.8660254037844267172, 1.000000000000011990 ) ) 
 REPRESENTATION_ITEM ( '' )  );
#36234 = CARTESIAN_POINT ( 'NONE',  ( -2.121150477449813534E-15, -11.54700538379251284, -192.8750000000000284 ) ) ;
#36236 = ORIENTED_EDGE ( 'NONE', *, *, #27718, .T. ) ;
#36235 = CARTESIAN_POINT ( 'NONE',  ( 10.81189881249999729, 0.000000000000000000, -120.0312500020483952 ) ) ;
#36237 = CARTESIAN_POINT ( 'NONE',  ( -9.999999999999998224, 1.224646799147353059E-15, -22.62500000409675849 ) ) ;
#36238 = VECTOR ( 'NONE', #41360, 1000.000000000000000 ) ;
#36239 = ORIENTED_EDGE ( 'NONE', *, *, #36721, .T. ) ;
#36240 = AXIS2_PLACEMENT_3D ( 'NONE', #39304, #12749, #29185 ) ;
#36241 = CARTESIAN_POINT ( 'NONE',  ( -2.293366432827344421E-15, -12.48450537969573659, -48.40625000204837391 ) ) ;
#36242 = PERSON_AND_ORGANIZATION ( #11915, #17965 ) ;
#36243 = CARTESIAN_POINT ( 'NONE',  ( 7.644554776091147741E-16, 12.48450537969573659, -93.96875000204838102 ) ) ;
#36244 = CARTESIAN_POINT ( 'NONE',  ( -5.405949406249996869, 9.363379034771805109, -121.0312500020483952 ) ) ;
#36246 = EDGE_LOOP ( 'NONE', ( #27148, #14340, #2706, #26401 ) ) ;
#36245 = EDGE_CURVE ( 'NONE', #4845, #4157, #42410, .T. ) ;
#36247 = DIRECTION ( 'NONE',  ( -0.000000000000000000, -0.000000000000000000, 1.000000000000000000 ) ) ;
#36248 = DIRECTION ( 'NONE',  ( 0.000000000000000000, 0.000000000000000000, -1.000000000000000000 ) ) ;
#36249 = ADVANCED_FACE ( 'NONE', ( #25612 ), #5542, .F. ) ;
#36250 = CARTESIAN_POINT ( 'NONE',  ( -5.405949406249996869, 9.363379034771805109, -181.0312500020483810 ) ) ;
#36251 = DIRECTION ( 'NONE',  ( 1.000000000000000000, 0.000000000000000000, 0.000000000000000000 ) ) ;
#36252 = EDGE_CURVE ( 'NONE', #13704, #29829, #2088, .T. ) ;
#36253 = CARTESIAN_POINT ( 'NONE',  ( -2.293366432827344421E-15, -12.48450537969573659, -135.2187500020483810 ) ) ;
#36254 = CC_DESIGN_DATE_AND_TIME_ASSIGNMENT ( #22975, #13650, ( #19626 ) ) ;
#36255 = CARTESIAN_POINT ( 'NONE',  ( -2.293366432827344421E-15, -12.48450537969573659, -99.21875000204839523 ) ) ;
#36256 = CARTESIAN_POINT ( 'NONE',  ( -79.99999999999992895, 39.99999999999999289, -160.0000000000000000 ) ) ;
#36257 = CARTESIAN_POINT ( 'NONE',  ( 10.81189881249999551, -6.242252689847874514, -105.1562500020483810 ) ) ;
#36258 = CARTESIAN_POINT ( 'NONE',  ( -4.999999999999996447, 8.660254037844387298, -183.3750000040967905 ) ) ;
#36259 = CARTESIAN_POINT ( 'NONE',  ( 5.405949406249999534, 9.363379034771803333, -113.5937500020483810 ) ) ;
#36260 = CARTESIAN_POINT ( 'NONE',  ( 10.81189881249999551, -6.242252689847874514, -183.1562500020484094 ) ) ;
#36261 = DIRECTION ( 'NONE',  ( -0.000000000000000000, -0.000000000000000000, 1.000000000000000000 ) ) ;
#36262 = CARTESIAN_POINT ( 'NONE',  ( 9.999999999999998224, 0.000000000000000000, -140.0000000000000000 ) ) ;
#36263 = CARTESIAN_POINT ( 'NONE',  ( -9.999999999999998224, 5.773502691896259087, -139.3750000000000000 ) ) ;
#36264 = CARTESIAN_POINT ( 'NONE',  ( -5.000000000000003553, -8.660254037844383745, -6.999999999999978684 ) ) ;
#36265 = CARTESIAN_POINT ( 'NONE',  ( 5.405949406249992428, -9.363379034771808662, -57.09375000204835970 ) ) ;
#36266 = CARTESIAN_POINT ( 'NONE',  ( 5.405949406249992428, -9.363379034771808662, -46.59375000204838102 ) ) ;
#36267 = CARTESIAN_POINT ( 'NONE',  ( -2.121150477449813534E-15, -11.54700538379251284, -179.7500000040967905 ) ) ;
#36268 = CARTESIAN_POINT ( 'NONE',  ( -2.293366432827344421E-15, -12.48450537969573659, -18.40625000204837036 ) ) ;
#36269 = CARTESIAN_POINT ( 'NONE',  ( -10.81189881249999729, 1.324075727343319199E-15, -27.59375000204836326 ) ) ;
#36270 = CARTESIAN_POINT ( 'NONE',  ( -9.999999999999998224, 1.224646799147353059E-15, -142.6250000040967905 ) ) ;
#36271 = CARTESIAN_POINT ( 'NONE',  ( 7.644554776091147741E-16, 12.48450537969573659, -135.9687500020483810 ) ) ;
#36272 = CARTESIAN_POINT ( 'NONE',  ( 9.999999999999998224, 0.000000000000000000, -105.4999999999999858 ) ) ;
#36273 = CARTESIAN_POINT ( 'NONE',  ( -10.81189881249999729, 6.242252689847871849, -36.90625000204835970 ) ) ;
#36274 = CYLINDRICAL_SURFACE ( 'NONE', #21749, 9.999999999999998224 ) ;
#36275 = AXIS2_PLACEMENT_3D ( 'NONE', #32803, #23517, #7321 ) ;
#36276 = CARTESIAN_POINT ( 'NONE',  ( 9.999999999999998224, 0.000000000000000000, -70.99999999999998579 ) ) ;
#36277 = CARTESIAN_POINT ( 'NONE',  ( 10.81189881249999551, -6.242252689847874514, -135.1562500020484094 ) ) ;
#36278 = CARTESIAN_POINT ( 'NONE',  ( -10.81189881249999729, 6.242252689847871849, -117.9062500020483952 ) ) ;
#36279 = EDGE_CURVE ( 'NONE', #11060, #32933, #6486, .T. ) ;
#36280 = VERTEX_POINT ( 'NONE', #19321 ) ;
#36281 = CARTESIAN_POINT ( 'NONE',  ( 5.000000000000000000, 8.660254037844385522, -142.7500000000000000 ) ) ;
#36282 = CARTESIAN_POINT ( 'NONE',  ( -5.000000000000003553, -8.660254037844383745, -107.8750000040967763 ) ) ;
#36283 = CARTESIAN_POINT ( 'NONE',  ( 5.000000000000000000, 8.660254037844385522, -162.2500000000000000 ) ) ;
#36284 = CARTESIAN_POINT ( 'NONE',  ( -10.81189881249999907, -6.242252689847864744, -66.46875000204838102 ) ) ;
#36285 = ORIENTED_EDGE ( 'NONE', *, *, #16955, .F. ) ;
#36286 = CARTESIAN_POINT ( 'NONE',  ( 10.00000000000000000, 5.773502691896255534, -31.87499999999995737 ) ) ;
#36287 = CARTESIAN_POINT ( 'NONE',  ( 10.00000000000000000, 5.773502691896255534, -17.25000000409676204 ) ) ;
#36288 = CARTESIAN_POINT ( 'NONE',  ( -10.81189881249999729, 1.324075727343319199E-15, -47.28125000204838813 ) ) ;
#36289 = CARTESIAN_POINT ( 'NONE',  ( 7.070501591499376803E-16, 11.54700538379251284, -125.0000000040967763 ) ) ;
#36290 = CARTESIAN_POINT ( 'NONE',  ( 10.00000000000000000, 5.773502691896255534, -36.75000000409675494 ) ) ;
#36291 = CARTESIAN_POINT ( 'NONE',  ( 5.000000000000000000, 8.660254037844385522, -117.6250000040967905 ) ) ;
#36292 = CARTESIAN_POINT ( 'NONE',  ( 10.81189881249999551, -6.242252689847874514, -136.6562500020484094 ) ) ;
#36293 = SHAPE_REPRESENTATION ( 'adapter key', ( #39998 ), #13832 ) ;
#36294 = CARTESIAN_POINT ( 'NONE',  ( 5.405949406249992428, -9.363379034771808662, -142.7812500020483810 ) ) ;
#36295 = CARTESIAN_POINT ( 'NONE',  ( 9.999999999999998224, 0.000000000000000000, -123.5000000000000000 ) ) ;
#36296 = EDGE_LOOP ( 'NONE', ( #38739, #30506, #20933, #28855 ) ) ;
#36297 = VERTEX_POINT ( 'NONE', #2945 ) ;
#36298 = ORIENTED_EDGE ( 'NONE', *, *, #15514, .F. ) ;
#36299 = CARTESIAN_POINT ( 'NONE',  ( -9.999999999999998224, 1.224646799147353059E-15, -104.7499999999999858 ) ) ;
#36300 = CARTESIAN_POINT ( 'NONE',  ( -10.81189881249999729, 6.242252689847871849, -173.2187500020483810 ) ) ;
#36301 = CARTESIAN_POINT ( 'NONE',  ( -10.81189881249999729, 6.242252689847871849, -24.71875000204837036 ) ) ;
#36302 = CARTESIAN_POINT ( 'NONE',  ( 9.999999999999998224, 0.000000000000000000, -38.37500000409676915 ) ) ;
#36303 = CARTESIAN_POINT ( 'NONE',  ( 10.81189881249999551, -6.242252689847874514, -152.9687500020484094 ) ) ;
#36304 = CARTESIAN_POINT ( 'NONE',  ( -10.81189881249999907, -6.242252689847864744, -145.9687500020484094 ) ) ;
#36305 = CARTESIAN_POINT ( 'NONE',  ( 10.00000000000154010, -5.773502691895370020, -8.500000004096712303 ) ) ;
#36306 = CARTESIAN_POINT ( 'NONE',  ( -2.293366432827344421E-15, -12.48450537969573659, -129.2187500020483810 ) ) ;
#36307 = CARTESIAN_POINT ( 'NONE',  ( 5.405949406249992428, -9.363379034771808662, -129.2812500020483810 ) ) ;
#36308 = CARTESIAN_POINT ( 'NONE',  ( 10.81189881249999907, 6.242252689847868297, -22.21875000204837036 ) ) ;
#36309 = CARTESIAN_POINT ( 'NONE',  ( 5.405949406249999534, 9.363379034771803333, -142.0937500020483810 ) ) ;
#36310 = DIRECTION ( 'NONE',  ( -0.000000000000000000, -0.000000000000000000, -1.000000000000000000 ) ) ;
#36311 = CARTESIAN_POINT ( 'NONE',  ( -2.121150477449813534E-15, -11.54700538379251284, -161.3750000000000000 ) ) ;
#36312 = CARTESIAN_POINT ( 'NONE',  ( 9.999999999999998224, 0.000000000000000000, -167.3750000040967905 ) ) ;
#36313 = EDGE_CURVE ( 'NONE', #38258, #684, #9619, .T. ) ;
#36314 = CARTESIAN_POINT ( 'NONE',  ( -10.81189881249999729, 1.324075727343319199E-15, -71.09375000204836681 ) ) ;
#36315 = CARTESIAN_POINT ( 'NONE',  ( 10.81189881249999907, 6.242252689847868297, -46.40625000204835970 ) ) ;
#36316 = CARTESIAN_POINT ( 'NONE',  ( 10.81189881249999907, 6.242252689847868297, -56.71875000204838813 ) ) ;
#36317 = DIRECTION ( 'NONE',  ( -1.000000000000000000, 0.000000000000000000, 0.000000000000000000 ) ) ;
#36318 = CARTESIAN_POINT ( 'NONE',  ( 10.81189881249999729, 0.000000000000000000, -158.8437500020483810 ) ) ;
#36319 = CARTESIAN_POINT ( 'NONE',  ( 5.000000000000000000, 8.660254037844385522, -129.2499999999999716 ) ) ;
#36320 = CARTESIAN_POINT ( 'NONE',  ( -10.81189881249999729, 1.324075727343319199E-15, -137.2812500020483810 ) ) ;
#36321 = DIRECTION ( 'NONE',  ( -0.000000000000000000, -0.000000000000000000, -1.000000000000000000 ) ) ;
#36322 = CARTESIAN_POINT ( 'NONE',  ( 7.070501591499377789E-16, 11.54700538379251284, -117.5000000040967905 ) ) ;
#36323 = CARTESIAN_POINT ( 'NONE',  ( -9.999999999999998224, 1.224646799147353059E-15, -91.24999999999998579 ) ) ;
#36324 = ORIENTED_EDGE ( 'NONE', *, *, #9661, .F. ) ;
#36325 = CARTESIAN_POINT ( 'NONE',  ( 10.81189881249999551, -6.242252689847874514, -112.6562500020483952 ) ) ;
#36326 = CARTESIAN_POINT ( 'NONE',  ( 5.000000000000000000, 8.660254037844385522, -132.6250000040967620 ) ) ;
#36327 = CARTESIAN_POINT ( 'NONE',  ( 4.999999999999992006, -8.660254037844389075, -177.7500000000000284 ) ) ;
#36328 = CARTESIAN_POINT ( 'NONE',  ( 5.405949406249992428, -9.363379034771808662, -160.7812500020484094 ) ) ;
#36329 = CARTESIAN_POINT ( 'NONE',  ( 10.00000000000000000, 5.773502691896255534, -41.25000000409676204 ) ) ;
#36330 = DIRECTION ( 'NONE',  ( -1.000000000000000000, 0.000000000000000000, 0.000000000000000000 ) ) ;
#36331 = CARTESIAN_POINT ( 'NONE',  ( 10.81189881249999551, -6.242252689847874514, -54.15625000204837391 ) ) ;
#36332 = DIRECTION ( 'NONE',  ( -0.000000000000000000, -0.000000000000000000, 1.000000000000000000 ) ) ;
#36333 = CARTESIAN_POINT ( 'NONE',  ( 5.405949406249999534, 9.363379034771803333, -163.2812500020484094 ) ) ;
#36334 = CARTESIAN_POINT ( 'NONE',  ( -10.81189881249999729, 1.324075727343319199E-15, -132.5937500020483810 ) ) ;
#36335 = LINE ( 'NONE', #6766, #27701 ) ;
#36336 = CARTESIAN_POINT ( 'NONE',  ( -9.999999999999998224, 1.224646799147353059E-15, -171.1250000040968189 ) ) ;
#36337 = VERTEX_POINT ( 'NONE', #18694 ) ;
#36338 = CARTESIAN_POINT ( 'NONE',  ( -9.999999999998969713, -5.773502691896847949, -31.12499999999993250 ) ) ;
#36340 = VERTEX_POINT ( 'NONE', #31890 ) ;
#36339 = CARTESIAN_POINT ( 'NONE',  ( -10.81189881249999907, -6.242252689847864744, -72.65625000204836681 ) ) ;
#36341 = PERSON_AND_ORGANIZATION_ROLE ( 'design_owner' ) ;
#36343 = VERTEX_POINT ( 'NONE', #15447 ) ;
#36342 = CARTESIAN_POINT ( 'NONE',  ( 5.405949406249999534, 9.363379034771803333, -116.5937500020483810 ) ) ;
#36344 = ORIENTED_EDGE ( 'NONE', *, *, #303, .F. ) ;
#36345 =( BOUNDED_CURVE ( )  B_SPLINE_CURVE ( 2, ( #12649, #18717, #9849, #15676, #2755, #31911, #29286 ),
 .UNSPECIFIED., .F., .F. ) 
 B_SPLINE_CURVE_WITH_KNOTS ( ( 3, 2, 2, 3 ),
 ( 0.8097014925373136052, 0.8109452736318409904, 0.8121890547263682647, 0.8134328358208956500 ),
 .UNSPECIFIED. ) 
 CURVE ( )  GEOMETRIC_REPRESENTATION_ITEM ( )  RATIONAL_B_SPLINE_CURVE ( ( 0.9999999999999761302, 0.8660254037844625774, 1.000000000000000000, 0.8660254037844387076, 1.000000000000000000, 0.8660254037844267172, 1.000000000000011990 ) ) 
 REPRESENTATION_ITEM ( '' )  );
#36346 = CARTESIAN_POINT ( 'NONE',  ( -5.405949406249996869, 9.363379034771805109, -21.84375000204835615 ) ) ;
#36347 = CARTESIAN_POINT ( 'NONE',  ( 10.81189881249999907, 6.242252689847868297, -1.406250002048370584 ) ) ;
#36348 = CARTESIAN_POINT ( 'NONE',  ( -10.81189881249999729, 1.324075727343319199E-15, -44.09375000204837391 ) ) ;
#36349 = CYLINDRICAL_SURFACE ( 'NONE', #17065, 9.999999999999998224 ) ;
#36350 = CARTESIAN_POINT ( 'NONE',  ( -2.121150477449813534E-15, -11.54700538379251284, -24.87499999999997868 ) ) ;
#36351 = CARTESIAN_POINT ( 'NONE',  ( 10.81189881249999551, -6.242252689847874514, -181.4687500020484094 ) ) ;
#36352 = CARTESIAN_POINT ( 'NONE',  ( -5.405949406249996869, 9.363379034771805109, -170.3437500020484094 ) ) ;
#36353 = CARTESIAN_POINT ( 'NONE',  ( -5.405949406250003975, -9.363379034771801557, -148.8437500020483810 ) ) ;
#36354 = CARTESIAN_POINT ( 'NONE',  ( 5.405949406249992428, -9.363379034771808662, -162.0937500020484094 ) ) ;
#36355 = CYLINDRICAL_SURFACE ( 'NONE', #15044, 5.500000000000003553 ) ;
#36356 = CARTESIAN_POINT ( 'NONE',  ( 5.000000000000000000, 8.660254037844385522, -102.6250000040967905 ) ) ;
#36357 = CARTESIAN_POINT ( 'NONE',  ( 4.999999999999992006, -8.660254037844389075, -188.2500000000000000 ) ) ;
#36358 = CARTESIAN_POINT ( 'NONE',  ( -10.81189881249999729, 1.324075727343319199E-15, -99.59375000204838102 ) ) ;
#36359 = CARTESIAN_POINT ( 'NONE',  ( 10.00000000000000000, 5.773502691896255534, -138.3750000000000000 ) ) ;
#36360 = CARTESIAN_POINT ( 'NONE',  ( 7.644554776091147741E-16, 12.48450537969573659, -62.65625000204838813 ) ) ;
#36361 = CARTESIAN_POINT ( 'NONE',  ( 10.00000000000025402, -5.773502691896113426, -159.6250000000000284 ) ) ;
#36362 = CARTESIAN_POINT ( 'NONE',  ( -10.81189881249999907, -6.242252689847864744, -186.4687500020484094 ) ) ;
#36363 = CARTESIAN_POINT ( 'NONE',  ( -5.405949406249996869, 9.363379034771805109, -119.5312500020483952 ) ) ;
#36364 = CARTESIAN_POINT ( 'NONE',  ( 5.405949406249999534, 9.363379034771803333, -161.7812500020484094 ) ) ;
#36365 = CARTESIAN_POINT ( 'NONE',  ( 10.81189881249999907, 6.242252689847868297, -50.90625000204837391 ) ) ;
#36366 = CARTESIAN_POINT ( 'NONE',  ( -4.999999999999996447, 8.660254037844387298, -135.3750000040967905 ) ) ;
#36367 = CARTESIAN_POINT ( 'NONE',  ( 10.00000000000000000, 5.773502691896255534, -115.8749999999999858 ) ) ;
#36368 = VERTEX_POINT ( 'NONE', #28645 ) ;
#36369 = CARTESIAN_POINT ( 'NONE',  ( 5.405949406249992428, -9.363379034771808662, -136.7812500020483810 ) ) ;
#36370 = CARTESIAN_POINT ( 'NONE',  ( 7.644554776091147741E-16, 12.48450537969573659, -145.1562500020484094 ) ) ;
#36371 = CYLINDRICAL_SURFACE ( 'NONE', #17853, 9.999999999999998224 ) ;
#36372 = CARTESIAN_POINT ( 'NONE',  ( -5.000000000000003553, -8.660254037844383745, -43.37500000409677625 ) ) ;
#36373 = CARTESIAN_POINT ( 'NONE',  ( -10.81189881249999907, -6.242252689847864744, -84.46875000204836681 ) ) ;
#36374 = AXIS2_PLACEMENT_3D ( 'NONE', #700, #30893, #4133 ) ;
#36375 = ORIENTED_EDGE ( 'NONE', *, *, #4854, .F. ) ;
#36376 = CARTESIAN_POINT ( 'NONE',  ( -2.121150477449813534E-15, -11.54700538379251284, -54.87499999999997158 ) ) ;
#36377 = CARTESIAN_POINT ( 'NONE',  ( -10.81189881249999729, 6.242252689847871849, -185.2187500020483810 ) ) ;
#36378 = CARTESIAN_POINT ( 'NONE',  ( 9.999999999999996447, -5.773502691896262640, -65.50000000409677625 ) ) ;
#36379 = VECTOR ( 'NONE', #17750, 1000.000000000000000 ) ;
#36380 = EDGE_CURVE ( 'NONE', #25635, #6986, #24149, .T. ) ;
#36381 = CARTESIAN_POINT ( 'NONE',  ( 7.070501591499376803E-16, 11.54700538379251284, -21.50000000409676559 ) ) ;
#36382 = CYLINDRICAL_SURFACE ( 'NONE', #33960, 9.999999999999998224 ) ;
#36383 = CARTESIAN_POINT ( 'NONE',  ( -5.405949406250003975, -9.363379034771801557, -81.53125000204839523 ) ) ;
#36384 = CARTESIAN_POINT ( 'NONE',  ( 10.81189881249999729, 6.242252689847867408, -61.40625000204838813 ) ) ;
#36385 = CARTESIAN_POINT ( 'NONE',  ( -9.999999999999998224, 5.773502691896259087, -63.25000000409678336 ) ) ;
#36386 = CARTESIAN_POINT ( 'NONE',  ( 10.81189881249999551, -6.242252689847874514, -19.46875000204836681 ) ) ;
#36387 = CARTESIAN_POINT ( 'NONE',  ( -9.999999999999998224, 1.224646799147353059E-15, -160.2500000000000000 ) ) ;
#36388 = CARTESIAN_POINT ( 'NONE',  ( 10.81189881249999551, -6.242252689847874514, -189.1562500020484379 ) ) ;
#36389 = CARTESIAN_POINT ( 'NONE',  ( 5.405949406249992428, -9.363379034771808662, -13.78125000204835615 ) ) ;
#36390 = CARTESIAN_POINT ( 'NONE',  ( 7.070501591499376803E-16, 11.54700538379251284, -40.62499999999996447 ) ) ;
#36391 = CARTESIAN_POINT ( 'NONE',  ( -9.999999999999998224, 1.224646799147353059E-15, -148.6250000040967905 ) ) ;
#36392 = LINE ( 'NONE', #158, #13889 ) ;
#36393 = DIRECTION ( 'NONE',  ( -0.000000000000000000, -0.000000000000000000, 1.000000000000000000 ) ) ;
#36394 = CARTESIAN_POINT ( 'NONE',  ( 9.999999999999998224, 0.000000000000000000, -170.0000000000000000 ) ) ;
#36395 = CARTESIAN_POINT ( 'NONE',  ( -9.999999999999998224, 1.224646799147353059E-15, -51.12500000409675494 ) ) ;
#36397 = ORIENTED_EDGE ( 'NONE', *, *, #10365, .T. ) ;
#36396 = CARTESIAN_POINT ( 'NONE',  ( 10.81189881249999907, 6.242252689847868297, -94.40625000204836681 ) ) ;
#36398 = CARTESIAN_POINT ( 'NONE',  ( 9.999999999999998224, 0.000000000000000000, -30.87500000409676559 ) ) ;
#36399 = ORIENTED_EDGE ( 'NONE', *, *, #39797, .F. ) ;
#36400 = ORIENTED_EDGE ( 'NONE', *, *, #32796, .F. ) ;
#36401 = CARTESIAN_POINT ( 'NONE',  ( 10.81189881249999907, 6.242252689847868297, -32.71875000204834549 ) ) ;
#36402 = CARTESIAN_POINT ( 'NONE',  ( 10.81189881249999729, 0.000000000000000000, -19.53125000204835970 ) ) ;
#36403 = COORDINATED_UNIVERSAL_TIME_OFFSET ( 6, 0, .AHEAD. ) ;
#36404 = CARTESIAN_POINT ( 'NONE',  ( -10.81189881249999729, 1.324075727343319199E-15, -69.59375000204836681 ) ) ;
#36405 = CARTESIAN_POINT ( 'NONE',  ( 5.000000000000000000, 8.660254037844385522, -105.2499999999999858 ) ) ;
#36406 = VECTOR ( 'NONE', #20160, 1000.000000000000000 ) ;
#36407 = CARTESIAN_POINT ( 'NONE',  ( -10.81189881249999729, 1.324075727343319199E-15, -189.5937500020483810 ) ) ;
#36408 = CARTESIAN_POINT ( 'NONE',  ( 10.81189881249999551, -6.242252689847874514, -151.4687500020483810 ) ) ;
#36409 = CARTESIAN_POINT ( 'NONE',  ( 0.000000000000000000, 0.000000000000000000, -203.0000000000000000 ) ) ;
#36410 = CARTESIAN_POINT ( 'NONE',  ( -9.999999999999998224, 1.224646799147353059E-15, -112.2499999999999858 ) ) ;
#36411 = CARTESIAN_POINT ( 'NONE',  ( 10.81189881249999907, 6.242252689847868297, -149.9062500020484094 ) ) ;
#36412 = CARTESIAN_POINT ( 'NONE',  ( 9.999999999999998224, 0.000000000000000000, -3.875000004096768258 ) ) ;
#36413 = CARTESIAN_POINT ( 'NONE',  ( -9.999999999999998224, 1.224646799147353059E-15, -49.62500000409675494 ) ) ;
#36414 = CARTESIAN_POINT ( 'NONE',  ( -10.81189881249999907, -6.242252689847864744, -117.4687500020483952 ) ) ;
#36415 = CARTESIAN_POINT ( 'NONE',  ( 5.000000000000000000, 8.660254037844385522, -141.2500000000000000 ) ) ;
#36416 = CARTESIAN_POINT ( 'NONE',  ( 7.644554776091147741E-16, 12.48450537969573659, -86.65625000204838102 ) ) ;
#36417 = CARTESIAN_POINT ( 'NONE',  ( -10.81189881249999729, 1.324075727343319199E-15, -108.5937500020483810 ) ) ;
#36418 = CARTESIAN_POINT ( 'NONE',  ( -10.81189881249999729, 6.242252689847871849, -66.71875000204838102 ) ) ;
#36419 = CARTESIAN_POINT ( 'NONE',  ( -10.81189881249999729, 6.242252689847871849, -80.40625000204839523 ) ) ;
#36420 = CARTESIAN_POINT ( 'NONE',  ( -9.999999999999998224, 5.773502691896259087, -160.7500000040967620 ) ) ;
#36421 = DIRECTION ( 'NONE',  ( -0.000000000000000000, -0.000000000000000000, 1.000000000000000000 ) ) ;
#36422 = CARTESIAN_POINT ( 'NONE',  ( 10.81189881249999551, -6.242252689847874514, -169.6562500020484094 ) ) ;
#36423 = CARTESIAN_POINT ( 'NONE',  ( 7.644554776091147741E-16, 12.48450537969573659, -184.1562500020484094 ) ) ;
#36424 = CYLINDRICAL_SURFACE ( 'NONE', #14591, 9.999999999999998224 ) ;
#36425 = CARTESIAN_POINT ( 'NONE',  ( -10.81189881249999729, 1.324075727343319199E-15, -3.593750002048368142 ) ) ;
#36426 = CARTESIAN_POINT ( 'NONE',  ( 0.000000000000000000, 0.000000000000000000, -200.0000000000000000 ) ) ;
#36427 = CARTESIAN_POINT ( 'NONE',  ( 5.405949406249999534, 9.363379034771803333, -113.5937500020483810 ) ) ;
#36428 = CARTESIAN_POINT ( 'NONE',  ( -2.121150477449813534E-15, -11.54700538379251284, -80.37499999999997158 ) ) ;
#36429 = CARTESIAN_POINT ( 'NONE',  ( -10.81189881249999907, -6.242252689847864744, -15.65625000204837214 ) ) ;
#36430 = CARTESIAN_POINT ( 'NONE',  ( 7.070501591499377789E-16, 11.54700538379251284, -90.50000000409677625 ) ) ;
#36431 = DIRECTION ( 'NONE',  ( 1.000000000000000000, 0.000000000000000000, 0.000000000000000000 ) ) ;
#36432 = CARTESIAN_POINT ( 'NONE',  ( 7.644554776091147741E-16, 12.48450537969573659, -106.1562500020483952 ) ) ;
#36433 = CARTESIAN_POINT ( 'NONE',  ( 5.405949406249999534, 9.363379034771803333, -85.28125000204838102 ) ) ;
#36434 = VERTEX_POINT ( 'NONE', #23431 ) ;
#36435 = CARTESIAN_POINT ( 'NONE',  ( -10.00000000000000000, -5.773502691896251982, -84.00000000409677625 ) ) ;
#36436 = CARTESIAN_POINT ( 'NONE',  ( 10.81189881249999729, 0.000000000000000000, -199.4375000020484094 ) ) ;
#36437 = CARTESIAN_POINT ( 'NONE',  ( 5.405949406249999534, 9.363379034771803333, -44.59375000204837391 ) ) ;
#36438 = VERTEX_POINT ( 'NONE', #16281 ) ;
#36439 = CARTESIAN_POINT ( 'NONE',  ( 7.070501591499377789E-16, 11.54700538379251284, -6.124999999999965361 ) ) ;
#36440 = EDGE_CURVE ( 'NONE', #28824, #10829, #7026, .T. ) ;
#36441 = CARTESIAN_POINT ( 'NONE',  ( -10.00000000000000000, -5.773502691896251982, -145.1250000000000284 ) ) ;
#36442 = DIRECTION ( 'NONE',  ( -0.000000000000000000, -0.000000000000000000, 1.000000000000000000 ) ) ;
#36443 =( BOUNDED_CURVE ( )  B_SPLINE_CURVE ( 2, ( #20475, #31061, #8182, #34518, #1496, #33662, #41165 ),
 .UNSPECIFIED., .F., .F. ) 
 B_SPLINE_CURVE_WITH_KNOTS ( ( 3, 2, 2, 3 ),
 ( 0.7164179104477614857, 0.7176616915422888709, 0.7189054726368161452, 0.7201492537313435305 ),
 .UNSPECIFIED. ) 
 CURVE ( )  GEOMETRIC_REPRESENTATION_ITEM ( )  RATIONAL_B_SPLINE_CURVE ( ( 0.9999999999999641398, 0.8660254037844745678, 1.000000000000000000, 0.8660254037844387076, 1.000000000000000000, 0.8660254037844148378, 1.000000000000023981 ) ) 
 REPRESENTATION_ITEM ( '' )  );
#36444 = CARTESIAN_POINT ( 'NONE',  ( 5.000000000000000000, 8.660254037844385522, -14.12500000409674961 ) ) ;
#36445 = EDGE_CURVE ( 'NONE', #26792, #11948, #140, .T. ) ;
#36446 = CARTESIAN_POINT ( 'NONE',  ( -2.121150477449813534E-15, -11.54700538379251284, -189.8750000000000000 ) ) ;
#36447 = CARTESIAN_POINT ( 'NONE',  ( 7.071067811865472841, 7.071067811865472841, -200.0000000000000000 ) ) ;
#36449 = ORIENTED_EDGE ( 'NONE', *, *, #5790, .F. ) ;
#36448 = CARTESIAN_POINT ( 'NONE',  ( -5.405949406250003975, -9.363379034771801557, -119.0312500020483952 ) ) ;
#36450 = FACE_OUTER_BOUND ( 'NONE', #22439, .T. ) ;
#36451 = ORIENTED_EDGE ( 'NONE', *, *, #11850, .F. ) ;
#36452 = CARTESIAN_POINT ( 'NONE',  ( -5.405949406249996869, 9.363379034771805109, -49.03125000204838813 ) ) ;
#36453 = APPLICATION_PROTOCOL_DEFINITION ( 'international standard', 'config_control_design', 1994, #29772 ) ;
#36454 = CARTESIAN_POINT ( 'NONE',  ( -10.81189881249999729, 1.324075727343319199E-15, -96.59375000204838102 ) ) ;
#36455 = CARTESIAN_POINT ( 'NONE',  ( 10.81189881249999729, 6.242252689847867408, -124.4062500020483810 ) ) ;
#36456 = ORIENTED_EDGE ( 'NONE', *, *, #28864, .F. ) ;
#36457 = CARTESIAN_POINT ( 'NONE',  ( -2.121150477449813534E-15, -11.54700538379251284, -111.8749999999999858 ) ) ;
#36458 = CARTESIAN_POINT ( 'NONE',  ( 5.405949406249992428, -9.363379034771808662, -174.2812500020484094 ) ) ;
#36459 = CARTESIAN_POINT ( 'NONE',  ( -10.00000000000102496, 5.773502691895664007, -0.2500000040967191861 ) ) ;
#36460 = CARTESIAN_POINT ( 'NONE',  ( 10.81189881249999551, -6.242252689847874514, -133.4687500020483810 ) ) ;
#36461 = CARTESIAN_POINT ( 'NONE',  ( -10.81189881249999907, -6.242252689847864744, -99.46875000204838102 ) ) ;
#36462 = DIRECTION ( 'NONE',  ( -0.000000000000000000, -0.000000000000000000, 1.000000000000000000 ) ) ;
#36463 = CARTESIAN_POINT ( 'NONE',  ( 5.405949406249999534, 9.363379034771803333, -106.2812500020483810 ) ) ;
#36464 = CARTESIAN_POINT ( 'NONE',  ( 9.999999999999998224, 0.000000000000000000, -186.8750000040967905 ) ) ;
#36465 = CARTESIAN_POINT ( 'NONE',  ( -2.293366432827344421E-15, -12.48450537969573659, -115.7187500020483668 ) ) ;
#36466 = CARTESIAN_POINT ( 'NONE',  ( -5.405949406249996869, 9.363379034771805109, -190.0312500020484094 ) ) ;
#36467 = CARTESIAN_POINT ( 'NONE',  ( -9.999999999999998224, 1.224646799147353059E-15, -95.74999999999998579 ) ) ;
#36468 = CARTESIAN_POINT ( 'NONE',  ( -9.999999999999227285, -5.773502691896698735, -114.0000000040967478 ) ) ;
#36469 = CARTESIAN_POINT ( 'NONE',  ( 5.000000000000000000, 8.660254037844385522, -129.2499999999999716 ) ) ;
#36470 = CARTESIAN_POINT ( 'NONE',  ( 7.070501591499377789E-16, 11.54700538379251284, -1.624999999999959810 ) ) ;
#36471 = CARTESIAN_POINT ( 'NONE',  ( -2.293366432827344421E-15, -12.48450537969573659, -60.21875000204837391 ) ) ;
#36472 = VECTOR ( 'NONE', #9824, 1000.000000000000000 ) ;
#36473 = CARTESIAN_POINT ( 'NONE',  ( -10.81189881249999729, 6.242252689847871849, -50.21875000204836681 ) ) ;
#36474 = CARTESIAN_POINT ( 'NONE',  ( -9.999999999999998224, 5.773502691896259087, -180.2500000040967905 ) ) ;
#36475 = CARTESIAN_POINT ( 'NONE',  ( -10.81189881249999729, 6.242252689847871849, -15.90625000204837391 ) ) ;
#36476 = CARTESIAN_POINT ( 'NONE',  ( 7.644554776091147741E-16, 12.48450537969573659, -27.96875000204837747 ) ) ;
#36477 = CARTESIAN_POINT ( 'NONE',  ( -5.000000000000003553, -8.660254037844383745, -92.87500000409677625 ) ) ;
#36478 = CARTESIAN_POINT ( 'NONE',  ( -2.293366432827344421E-15, -12.48450537969573659, -136.7187500020483810 ) ) ;
#36479 = CARTESIAN_POINT ( 'NONE',  ( -2.121150477449813534E-15, -11.54700538379251284, -105.8749999999999858 ) ) ;
#36480 = CARTESIAN_POINT ( 'NONE',  ( -5.405949406250003975, -9.363379034771801557, -35.03125000204837391 ) ) ;
#36481 = CARTESIAN_POINT ( 'NONE',  ( 10.00000000000000000, 5.773502691896255534, -63.37499999999998579 ) ) ;
#36482 = CARTESIAN_POINT ( 'NONE',  ( -10.81189881249999907, -6.242252689847864744, -131.1562500020483810 ) ) ;
#36483 = CARTESIAN_POINT ( 'NONE',  ( -10.81189881249999729, 6.242252689847871849, -108.9062500020483810 ) ) ;
#36484 = ORIENTED_EDGE ( 'NONE', *, *, #29172, .T. ) ;
#36485 =( BOUNDED_CURVE ( )  B_SPLINE_CURVE ( 2, ( #31225, #4882, #17591, #37244, #24105, #1651, #20845 ),
 .UNSPECIFIED., .F., .F. ) 
 B_SPLINE_CURVE_WITH_KNOTS ( ( 3, 2, 2, 3 ),
 ( 0.3395522388059703522, 0.3407960199004976820, 0.3420398009950250118, 0.3432835820895522860 ),
 .UNSPECIFIED. ) 
 CURVE ( )  GEOMETRIC_REPRESENTATION_ITEM ( )  RATIONAL_B_SPLINE_CURVE ( ( 0.9999999999999761302, 0.8660254037844625774, 1.000000000000000000, 0.8660254037844387076, 1.000000000000000000, 0.8660254037844327124, 1.000000000000005995 ) ) 
 REPRESENTATION_ITEM ( '' )  );
#36486 = AXIS2_PLACEMENT_3D ( 'NONE', #12671, #12464, #32765 ) ;
#36487 = CARTESIAN_POINT ( 'NONE',  ( 9.999999999999996447, -5.773502691896262640, -107.5000000040967763 ) ) ;
#36488 = CARTESIAN_POINT ( 'NONE',  ( -10.81189881249999729, 6.242252689847871849, -66.71875000204838102 ) ) ;
#36489 = ORIENTED_EDGE ( 'NONE', *, *, #40653, .T. ) ;
#36490 = CARTESIAN_POINT ( 'NONE',  ( -2.121150477449813534E-15, -11.54700538379251284, -32.37499999999996447 ) ) ;
#36491 = CARTESIAN_POINT ( 'NONE',  ( -9.999999999999998224, 5.773502691896259087, -16.75000000409675849 ) ) ;
#36492 = EDGE_CURVE ( 'NONE', #39036, #4760, #10122, .T. ) ;
#36493 = CARTESIAN_POINT ( 'NONE',  ( 5.405949406249999534, 9.363379034771803333, -46.28125000204838813 ) ) ;
#36494 = CARTESIAN_POINT ( 'NONE',  ( -4.999999999999996447, 8.660254037844387298, -34.87500000409676915 ) ) ;
#36495 = CARTESIAN_POINT ( 'NONE',  ( 7.070501591499377789E-16, 11.54700538379251284, -33.50000000409675494 ) ) ;
#36496 = EDGE_CURVE ( 'NONE', #35398, #17462, #32467, .T. ) ;
#36497 = DIRECTION ( 'NONE',  ( -1.000000000000000000, 0.000000000000000000, 0.000000000000000000 ) ) ;
#36498 = CARTESIAN_POINT ( 'NONE',  ( -2.293366432827344421E-15, -12.48450537969573659, -145.9062500020484094 ) ) ;
#36499 = CC_DESIGN_PERSON_AND_ORGANIZATION_ASSIGNMENT ( #7413, #18131, ( #36593 ) ) ;
#36500 = CARTESIAN_POINT ( 'NONE',  ( -5.000000000000003553, -8.660254037844383745, -110.4999999999999858 ) ) ;
#36501 = ORIENTED_EDGE ( 'NONE', *, *, #38069, .T. ) ;
#36502 = EDGE_LOOP ( 'NONE', ( #13916, #12603, #12444, #37981 ) ) ;
#36503 = ORIENTED_EDGE ( 'NONE', *, *, #13828, .T. ) ;
#36504 = CARTESIAN_POINT ( 'NONE',  ( -4.999999999999996447, 8.660254037844387298, -159.0000000000000000 ) ) ;
#36505 = CARTESIAN_POINT ( 'NONE',  ( -9.999999999999227285, -5.773502691896698735, -130.1249999999999716 ) ) ;
#36506 = CARTESIAN_POINT ( 'NONE',  ( 10.81189881249999907, 6.242252689847868297, -172.2187500020483810 ) ) ;
#36507 = EDGE_CURVE ( 'NONE', #23032, #42377, #16922, .T. ) ;
#36508 = CARTESIAN_POINT ( 'NONE',  ( 10.81189881249999907, 6.242252689847868297, -20.71875000204836681 ) ) ;
#36509 = CARTESIAN_POINT ( 'NONE',  ( -2.121150477449813534E-15, -11.54700538379251284, -61.25000000409677625 ) ) ;
#36510 = CARTESIAN_POINT ( 'NONE',  ( -9.999999999999998224, 1.224646799147353059E-15, -157.6250000040967905 ) ) ;
#36511 = CARTESIAN_POINT ( 'NONE',  ( 10.81189881249999729, 0.000000000000000000, -158.8437500020483810 ) ) ;
#36512 = CARTESIAN_POINT ( 'NONE',  ( 7.644554776091147741E-16, 12.48450537969573659, -141.9687500020483810 ) ) ;
#36513 = CARTESIAN_POINT ( 'NONE',  ( 9.999999999999998224, 0.000000000000000000, -87.87500000409677625 ) ) ;
#36514 = CARTESIAN_POINT ( 'NONE',  ( -10.81189881249999729, 6.242252689847871849, -122.2187500020483810 ) ) ;
#36515 = CARTESIAN_POINT ( 'NONE',  ( -10.81189881249999729, 1.324075727343319199E-15, -132.7812500020483810 ) ) ;
#36516 = CARTESIAN_POINT ( 'NONE',  ( -10.81189881249999729, 1.324075727343319199E-15, -12.59375000204834905 ) ) ;
#36517 = CARTESIAN_POINT ( 'NONE',  ( 10.81189881249999729, 0.000000000000000000, -139.3437500020484094 ) ) ;
#36518 = DIRECTION ( 'NONE',  ( 1.000000000000000000, 0.000000000000000000, 0.000000000000000000 ) ) ;
#36519 = CARTESIAN_POINT ( 'NONE',  ( -9.999999999999998224, 5.773502691896259087, -155.8749999999999716 ) ) ;
#36520 = CARTESIAN_POINT ( 'NONE',  ( 9.999999999999998224, 0.000000000000000000, -106.9999999999999858 ) ) ;
#36521 = CARTESIAN_POINT ( 'NONE',  ( -5.405949406250003975, -9.363379034771801557, -75.34375000204838102 ) ) ;
#36522 = CARTESIAN_POINT ( 'NONE',  ( -5.405949406250003975, -9.363379034771801557, -45.53125000204838102 ) ) ;
#36523 = CARTESIAN_POINT ( 'NONE',  ( -2.293366432827344421E-15, -12.48450537969573659, -54.21875000204837391 ) ) ;
#36524 = CARTESIAN_POINT ( 'NONE',  ( -2.121150477449813534E-15, -11.54700538379251284, -113.7500000040967763 ) ) ;
#36525 = CARTESIAN_POINT ( 'NONE',  ( 10.81189881249999907, 6.242252689847868297, -160.2187500020483810 ) ) ;
#36526 = CARTESIAN_POINT ( 'NONE',  ( -9.999999999999998224, 5.773502691896259087, -125.8749999999999858 ) ) ;
#36527 = CARTESIAN_POINT ( 'NONE',  ( -2.293366432827344421E-15, -12.48450537969573659, -139.9062500020484094 ) ) ;
#36528 = DIRECTION ( 'NONE',  ( -0.000000000000000000, -0.000000000000000000, 1.000000000000000000 ) ) ;
#36529 = CARTESIAN_POINT ( 'NONE',  ( 4.999999999999992006, -8.660254037844389075, -113.6250000040967763 ) ) ;
#36530 = CARTESIAN_POINT ( 'NONE',  ( 10.00000000000000000, 5.773502691896255534, -91.87499999999998579 ) ) ;
#36531 = ORIENTED_EDGE ( 'NONE', *, *, #7995, .F. ) ;
#36532 = CARTESIAN_POINT ( 'NONE',  ( 5.405949406249999534, 9.363379034771803333, -109.2812500020483810 ) ) ;
#36533 = CARTESIAN_POINT ( 'NONE',  ( -2.121150477449813534E-15, -11.54700538379251284, -131.7500000040967905 ) ) ;
#36534 = CYLINDRICAL_SURFACE ( 'NONE', #11889, 9.999999999999998224 ) ;
#36535 = VECTOR ( 'NONE', #37720, 1000.000000000000000 ) ;
#36536 = CARTESIAN_POINT ( 'NONE',  ( 10.81189881249999729, 0.000000000000000000, -168.0312500020484094 ) ) ;
#36537 = CARTESIAN_POINT ( 'NONE',  ( 9.999999999999996447, -5.773502691896262640, -43.00000000409676204 ) ) ;
#36538 = CYLINDRICAL_SURFACE ( 'NONE', #15230, 9.999999999999998224 ) ;
#36539 = CARTESIAN_POINT ( 'NONE',  ( 5.405949406249999534, 9.363379034771803333, -49.28125000204838813 ) ) ;
#36540 = FACE_OUTER_BOUND ( 'NONE', #8808, .T. ) ;
#36541 = CARTESIAN_POINT ( 'NONE',  ( 5.405949406249992428, -9.363379034771808662, -163.7812500020484094 ) ) ;
#36542 = CARTESIAN_POINT ( 'NONE',  ( -10.81189881249999729, 1.324075727343319199E-15, -134.0937500020483810 ) ) ;
#36543 = LINE ( 'NONE', #3750, #20116 ) ;
#36544 = EDGE_LOOP ( 'NONE', ( #41958, #11012, #10521, #24294 ) ) ;
#36545 = DIRECTION ( 'NONE',  ( 0.7071067811865451302, 0.000000000000000000, 0.7071067811865500152 ) ) ;
#36546 = EDGE_CURVE ( 'NONE', #1269, #5836, #26243, .T. ) ;
#36548 = ORIENTED_EDGE ( 'NONE', *, *, #26621, .T. ) ;
#36547 = CARTESIAN_POINT ( 'NONE',  ( -10.81189881249999729, 6.242252689847871849, -66.90625000204839523 ) ) ;
#36549 = CALENDAR_DATE ( 2026, 28, 9 ) ;
#36551 = EDGE_LOOP ( 'NONE', ( #4811, #19023, #1956, #18237 ) ) ;
#36550 = CARTESIAN_POINT ( 'NONE',  ( 5.405949406249992428, -9.363379034771808662, -120.0937500020483952 ) ) ;
#36552 = CARTESIAN_POINT ( 'NONE',  ( 7.644554776091147741E-16, 12.48450537969573659, -17.46875000204836681 ) ) ;
#36553 = CARTESIAN_POINT ( 'NONE',  ( -5.405949406250003975, -9.363379034771801557, -196.8437500020484094 ) ) ;
#36554 = CARTESIAN_POINT ( 'NONE',  ( -5.405949406250003975, -9.363379034771801557, -43.84375000204837391 ) ) ;
#36555 = CARTESIAN_POINT ( 'NONE',  ( 9.999999999999998224, 0.000000000000000000, -72.49999999999998579 ) ) ;
#36556 = CARTESIAN_POINT ( 'NONE',  ( 5.000000000000000000, 8.660254037844385522, -0.2499999999999724665 ) ) ;
#36557 = AXIS2_PLACEMENT_3D ( 'NONE', #5502, #8743, #18651 ) ;
#36558 = CARTESIAN_POINT ( 'NONE',  ( 5.405949406249999534, 9.363379034771803333, -184.0937500020483810 ) ) ;
#36559 = CARTESIAN_POINT ( 'NONE',  ( 10.81189881249999907, 6.242252689847868297, -166.2187500020484094 ) ) ;
#36560 = CARTESIAN_POINT ( 'NONE',  ( 5.405949406249999534, 9.363379034771803333, -149.5937500020483810 ) ) ;
#36561 = CARTESIAN_POINT ( 'NONE',  ( 5.405949406249992428, -9.363379034771808662, -160.5937500020484094 ) ) ;
#36562 = CARTESIAN_POINT ( 'NONE',  ( -4.999999999999996447, 8.660254037844387298, -106.8750000040967763 ) ) ;
#36563 = CARTESIAN_POINT ( 'NONE',  ( -10.00000000000012434, 5.773502691896184480, -193.7500000040967620 ) ) ;
#36564 = CARTESIAN_POINT ( 'NONE',  ( 9.999999999999998224, 0.000000000000000000, -179.0000000000000000 ) ) ;
#36565 = CARTESIAN_POINT ( 'NONE',  ( 10.81189881249999551, -6.242252689847874514, -100.4687500020483952 ) ) ;
#36566 = CARTESIAN_POINT ( 'NONE',  ( 0.000000000000000000, 0.000000000000000000, -99.99999999999998579 ) ) ;
#36567 = CARTESIAN_POINT ( 'NONE',  ( 7.644554776091147741E-16, 12.48450537969573659, -65.65625000204838102 ) ) ;
#36568 = CYLINDRICAL_SURFACE ( 'NONE', #32966, 9.999999999999998224 ) ;
#36569 = CARTESIAN_POINT ( 'NONE',  ( 5.405949406249999534, 9.363379034771803333, -185.5937500020483810 ) ) ;
#36570 = CARTESIAN_POINT ( 'NONE',  ( 10.81189881249999551, -6.242252689847874514, -120.1562500020483810 ) ) ;
#36571 = CARTESIAN_POINT ( 'NONE',  ( -5.405949406249996869, 9.363379034771805109, -163.0312500020484094 ) ) ;
#36572 = CARTESIAN_POINT ( 'NONE',  ( 10.81189881249999551, -6.242252689847874514, -54.15625000204837391 ) ) ;
#36573 = CARTESIAN_POINT ( 'NONE',  ( -9.999999999999998224, 5.773502691896259087, -135.2500000040967905 ) ) ;
#36574 = CARTESIAN_POINT ( 'NONE',  ( 5.000000000000000000, 8.660254037844385522, -115.7499999999999858 ) ) ;
#36575 = ORIENTED_EDGE ( 'NONE', *, *, #7506, .T. ) ;
#36576 = CARTESIAN_POINT ( 'NONE',  ( 10.81189881249999729, 0.000000000000000000, -133.5312500020484094 ) ) ;
#36577 = CARTESIAN_POINT ( 'NONE',  ( -10.81189881249999729, 1.324075727343319199E-15, -147.7812500020483810 ) ) ;
#36578 = CARTESIAN_POINT ( 'NONE',  ( 10.81189881249999729, 0.000000000000000000, -189.0312500020484094 ) ) ;
#36579 = CARTESIAN_POINT ( 'NONE',  ( 10.00000000000025402, -5.773502691896113426, -125.1249999999999574 ) ) ;
#36580 = CARTESIAN_POINT ( 'NONE',  ( -10.81189881249999907, -6.242252689847864744, -82.96875000204836681 ) ) ;
#36581 = ORIENTED_EDGE ( 'NONE', *, *, #25986, .F. ) ;
#36582 = CARTESIAN_POINT ( 'NONE',  ( -10.00000000000000000, -5.773502691896251982, -56.62499999999997868 ) ) ;
#36583 = CARTESIAN_POINT ( 'NONE',  ( 10.81189881249999907, 6.242252689847868297, -176.7187500020483810 ) ) ;
#36584 = CARTESIAN_POINT ( 'NONE',  ( 9.999999999999998224, 0.000000000000000000, -65.37500000409676204 ) ) ;
#36585 = CARTESIAN_POINT ( 'NONE',  ( -10.00000000000000000, -5.773502691896252870, -172.1250000000000284 ) ) ;
#36586 = LINE ( 'NONE', #37219, #20839 ) ;
#36587 = CARTESIAN_POINT ( 'NONE',  ( -5.405949406249996869, 9.363379034771805109, -76.03125000204838102 ) ) ;
#36588 = CARTESIAN_POINT ( 'NONE',  ( -10.81189881249999729, 1.324075727343319199E-15, -60.78125000204836681 ) ) ;
#36589 = CARTESIAN_POINT ( 'NONE',  ( 9.999999999999998224, 0.000000000000000000, -53.37500000409675494 ) ) ;
#36590 = CARTESIAN_POINT ( 'NONE',  ( -10.81189881249999729, 6.242252689847871849, -8.218750002048357928 ) ) ;
#36591 = CARTESIAN_POINT ( 'NONE',  ( -9.999999999999998224, 1.224646799147353059E-15, -133.6250000040967620 ) ) ;
#36592 = CARTESIAN_POINT ( 'NONE',  ( -10.81189881249999729, 6.242252689847871849, -188.4062500020484094 ) ) ;
#36593 = PRODUCT_DEFINITION_FORMATION_WITH_SPECIFIED_SOURCE ( 'ANY', '', #14563, .NOT_KNOWN. ) ;
#36594 = CARTESIAN_POINT ( 'NONE',  ( 10.81189881249999551, -6.242252689847874514, -4.656250002048361480 ) ) ;
#36595 = CARTESIAN_POINT ( 'NONE',  ( -9.999999999999998224, 1.224646799147353059E-15, -107.7499999999999858 ) ) ;
#36596 = CARTESIAN_POINT ( 'NONE',  ( -99.99999999999994316, 19.99999999999998934, -160.0000000000000000 ) ) ;
#36597 = CARTESIAN_POINT ( 'NONE',  ( 9.999999999999998224, 1.224646799147353059E-15, -99.99999999999998579 ) ) ;
#36598 = FACE_OUTER_BOUND ( 'NONE', #36296, .T. ) ;
#36599 =( BOUNDED_CURVE ( )  B_SPLINE_CURVE ( 2, ( #25584, #22126, #35301, #38738, #22338, #577, #4011 ),
 .UNSPECIFIED., .F., .F. ) 
 B_SPLINE_CURVE_WITH_KNOTS ( ( 3, 2, 2, 3 ),
 ( 0.4888059701492538101, 0.4900497512437811398, 0.4912935323383084696, 0.4919154229045888393 ),
 .UNSPECIFIED. ) 
 CURVE ( )  GEOMETRIC_REPRESENTATION_ITEM ( )  RATIONAL_B_SPLINE_CURVE ( ( 0.9999999999999940048, 0.8660254037844447028, 1.000000000000000000, 0.8660254037844387076, 1.000000000000000000, 0.9330126998438240671, 0.9330127018922194093 ) ) 
 REPRESENTATION_ITEM ( '' )  );
#36600 = CARTESIAN_POINT ( 'NONE',  ( 9.999999999999998224, 0.000000000000000000, -61.99999999999997158 ) ) ;
#36602 = ORIENTED_EDGE ( 'NONE', *, *, #4036, .F. ) ;
#36601 = CARTESIAN_POINT ( 'NONE',  ( -10.81189881249999907, -6.242252689847864744, -90.65625000204836681 ) ) ;
#36603 = CARTESIAN_POINT ( 'NONE',  ( 5.000000000000000000, 8.660254037844385522, -83.12500000409676204 ) ) ;
#36605 = EDGE_LOOP ( 'NONE', ( #1356, #27542, #30575, #7953 ) ) ;
#36604 = CARTESIAN_POINT ( 'NONE',  ( -10.81189881249999729, 6.242252689847871849, -101.2187500020483810 ) ) ;
#36606 = ORIENTED_EDGE ( 'NONE', *, *, #26241, .T. ) ;
#36607 = CARTESIAN_POINT ( 'NONE',  ( -5.405949406249996869, 9.363379034771805109, -33.84375000204836681 ) ) ;
#36608 = CARTESIAN_POINT ( 'NONE',  ( 5.405949406249999534, 9.363379034771803333, -19.28125000204835970 ) ) ;
#36609 = CARTESIAN_POINT ( 'NONE',  ( -10.81189881249999729, 1.324075727343319199E-15, -72.59375000204838102 ) ) ;
#36610 = CARTESIAN_POINT ( 'NONE',  ( -9.999999999999998224, 1.224646799147353059E-15, -133.6250000040967620 ) ) ;
#36611 = CARTESIAN_POINT ( 'NONE',  ( 7.070501591499377789E-16, 11.54700538379251284, -42.12499999999997158 ) ) ;
#36612 = CARTESIAN_POINT ( 'NONE',  ( 10.81189881249999907, 6.242252689847868297, -194.7187500020484094 ) ) ;
#36613 = CARTESIAN_POINT ( 'NONE',  ( -10.81189881249999729, 6.242252689847871849, -150.7187500020483810 ) ) ;
#36614 = ADVANCED_FACE ( 'NONE', ( #36160 ), #6593, .F. ) ;
#36615 = CARTESIAN_POINT ( 'NONE',  ( 7.070501591499376803E-16, 11.54700538379251284, -99.12500000000000000 ) ) ;
#36616 = DIRECTION ( 'NONE',  ( -1.000000000000000000, 3.469446951953614805E-17, 0.000000000000000000 ) ) ;
#36617 = CARTESIAN_POINT ( 'NONE',  ( 7.644554776091147741E-16, 12.48450537969573659, -145.1562500020484094 ) ) ;
#36618 = CARTESIAN_POINT ( 'NONE',  ( -4.999999999999996447, 8.660254037844387298, -1.875000004096766260 ) ) ;
#36619 = CARTESIAN_POINT ( 'NONE',  ( 0.000000000000000000, 0.000000000000000000, -200.0000000000000000 ) ) ;
#36620 = PRODUCT_DEFINITION_FORMATION_WITH_SPECIFIED_SOURCE ( 'ANY', '', #2800, .NOT_KNOWN. ) ;
#36621 = CARTESIAN_POINT ( 'NONE',  ( 5.405949406249999534, 9.363379034771803333, -122.5937500020483952 ) ) ;
#36622 = FACE_OUTER_BOUND ( 'NONE', #41633, .T. ) ;
#36623 = CARTESIAN_POINT ( 'NONE',  ( 10.81189881249999907, 6.242252689847868297, -91.40625000204836681 ) ) ;
#36624 = CARTESIAN_POINT ( 'NONE',  ( -10.81189881249999729, -6.242252689847864744, -105.4687500020483668 ) ) ;
#36625 = CARTESIAN_POINT ( 'NONE',  ( -5.405949406249996869, 9.363379034771805109, -68.34375000204836681 ) ) ;
#36626 = CARTESIAN_POINT ( 'NONE',  ( 10.81189881249999729, 0.000000000000000000, -73.53125000204838102 ) ) ;
#36627 = CARTESIAN_POINT ( 'NONE',  ( 4.999999999999992006, -8.660254037844389075, -158.6250000040967905 ) ) ;
#36628 = CARTESIAN_POINT ( 'NONE',  ( 7.644554776091147741E-16, 12.48450537969573659, -161.6562500020484094 ) ) ;
#36629 = CARTESIAN_POINT ( 'NONE',  ( 7.644554776091147741E-16, 12.48450537969573659, -170.6562500020484094 ) ) ;
#36630 = CIRCLE ( 'NONE', #42138, 9.999999999999998224 ) ;
#36631 = CARTESIAN_POINT ( 'NONE',  ( 0.000000000000000000, 0.000000000000000000, -200.0000000000000000 ) ) ;
#36632 = CARTESIAN_POINT ( 'NONE',  ( 0.000000000000000000, 0.000000000000000000, -99.99999999999998579 ) ) ;
#36633 = CARTESIAN_POINT ( 'NONE',  ( -5.000000000000003553, -8.660254037844383745, -53.87500000409675494 ) ) ;
#36634 = CARTESIAN_POINT ( 'NONE',  ( -10.81189881249999729, 6.242252689847871849, -104.2187500020483810 ) ) ;
#36635 = CARTESIAN_POINT ( 'NONE',  ( 9.999999999999996447, -5.773502691896262640, -84.62499999999998579 ) ) ;
#36636 = CARTESIAN_POINT ( 'NONE',  ( 10.81189881249999729, 0.000000000000000000, -7.531250002048350822 ) ) ;
#36637 = CARTESIAN_POINT ( 'NONE',  ( -4.999999999999996447, 8.660254037844387298, -88.87500000409677625 ) ) ;
#36638 = CARTESIAN_POINT ( 'NONE',  ( 9.999999999999998224, 0.000000000000000000, -119.3750000040967905 ) ) ;
#36639 = CARTESIAN_POINT ( 'NONE',  ( -2.293366432827344421E-15, -12.48450537969573659, -96.40625000204839523 ) ) ;
#36640 = CARTESIAN_POINT ( 'NONE',  ( -5.405949406250003975, -9.363379034771801557, -81.53125000204839523 ) ) ;
#36641 = ORIENTED_EDGE ( 'NONE', *, *, #24740, .T. ) ;
#36642 = ADVANCED_FACE ( 'NONE', ( #36928 ), #17061, .F. ) ;
#36643 = CARTESIAN_POINT ( 'NONE',  ( 7.070501591499377789E-16, 11.54700538379251284, -81.50000000409677625 ) ) ;
#36644 = CARTESIAN_POINT ( 'NONE',  ( -9.999999999999998224, 0.000000000000000000, -99.99999999999998579 ) ) ;
#36645 = CARTESIAN_POINT ( 'NONE',  ( 5.405949406249999534, 9.363379034771803333, -34.09375000204836681 ) ) ;
#36646 = ORIENTED_EDGE ( 'NONE', *, *, #20111, .F. ) ;
#36647 = CARTESIAN_POINT ( 'NONE',  ( -10.00000000000000000, -5.773502691896251982, -11.62499999999995914 ) ) ;
#36648 = ADVANCED_FACE ( 'NONE', ( #11018 ), #30817, .T. ) ;
#36649 = CARTESIAN_POINT ( 'NONE',  ( -10.81189881249999729, 1.324075727343319199E-15, -38.28125000204838102 ) ) ;
#36650 = CARTESIAN_POINT ( 'NONE',  ( -10.00000000000000000, -5.773502691896251982, -146.6249999999999716 ) ) ;
#36651 = CYLINDRICAL_SURFACE ( 'NONE', #42039, 9.999999999999998224 ) ;
#36652 = CARTESIAN_POINT ( 'NONE',  ( 7.070501591499377789E-16, 11.54700538379251284, -12.50000000409676026 ) ) ;
#36653 = ADVANCED_FACE ( 'NONE', ( #7929 ), #30388, .F. ) ;
#36654 = CARTESIAN_POINT ( 'NONE',  ( -4.999999999999996447, 8.660254037844387298, -190.5000000000000000 ) ) ;
#36655 = CARTESIAN_POINT ( 'NONE',  ( 9.999999999999998224, 0.000000000000000000, -47.37500000409677625 ) ) ;
#36657 = VERTEX_POINT ( 'NONE', #16978 ) ;
#36656 = CARTESIAN_POINT ( 'NONE',  ( -2.293366432827344421E-15, -12.48450537969573659, -117.4062500020483952 ) ) ;
#36658 = DIRECTION ( 'NONE',  ( 1.000000000000000000, 1.502314598737160017E-16, 0.000000000000000000 ) ) ;
#36659 = VERTEX_POINT ( 'NONE', #26919 ) ;
#36660 = CARTESIAN_POINT ( 'NONE',  ( -10.81189881249999907, -6.242252689847864744, -44.15625000204838102 ) ) ;
#36661 = CALENDAR_DATE ( 2026, 28, 9 ) ;
#36662 = VECTOR ( 'NONE', #30776, 1000.000000000000000 ) ;
#36663 = CARTESIAN_POINT ( 'NONE',  ( 10.81189881249999907, 6.242252689847868297, -94.21875000204838102 ) ) ;
#36664 = CARTESIAN_POINT ( 'NONE',  ( -10.81189881249999729, 1.324075727343319199E-15, -120.7812500020483952 ) ) ;
#36665 = EDGE_LOOP ( 'NONE', ( #32488, #27324, #14995, #7511 ) ) ;
#36666 = CARTESIAN_POINT ( 'NONE',  ( -9.999999999999998224, 1.224646799147353059E-15, -96.12500000409677625 ) ) ;
#36667 = CARTESIAN_POINT ( 'NONE',  ( -9.999999999999998224, 1.224646799147353059E-15, -193.2500000000000000 ) ) ;
#36668 = CARTESIAN_POINT ( 'NONE',  ( 5.405949406249992428, -9.363379034771808662, -169.7812500020484094 ) ) ;
#36669 = CARTESIAN_POINT ( 'NONE',  ( -9.999999999999479527, -5.773502691896549521, -147.0000000040967620 ) ) ;
#36670 = ADVANCED_FACE ( 'NONE', ( #20438 ), #17189, .F. ) ;
#36671 = CARTESIAN_POINT ( 'NONE',  ( 10.81189881249999729, 6.242252689847867408, -131.7187500020483810 ) ) ;
#36672 = CARTESIAN_POINT ( 'NONE',  ( -5.405949406250003975, -9.363379034771801557, -90.34375000204838102 ) ) ;
#36673 = DIRECTION ( 'NONE',  ( 1.000000000000000000, 0.000000000000000000, 0.000000000000000000 ) ) ;
#36674 = CARTESIAN_POINT ( 'NONE',  ( -10.81189881249999729, 6.242252689847871849, -101.4062500020483952 ) ) ;
#36675 = CARTESIAN_POINT ( 'NONE',  ( -10.00000000000000000, -5.773502691896251982, -189.0000000040967905 ) ) ;
#36676 = CARTESIAN_POINT ( 'NONE',  ( 10.81189881249999729, 0.000000000000000000, -113.8437500020483810 ) ) ;
#36677 = AXIS2_PLACEMENT_3D ( 'NONE', #40895, #40465, #27548 ) ;
#36678 = CARTESIAN_POINT ( 'NONE',  ( -10.81189881249999729, 6.242252689847871849, -180.9062500020484094 ) ) ;
#36679 = DIRECTION ( 'NONE',  ( -1.000000000000000000, 0.000000000000000000, 0.000000000000000000 ) ) ;
#36680 = CARTESIAN_POINT ( 'NONE',  ( -4.999999999999996447, 8.660254037844387298, -132.3750000040967905 ) ) ;
#36681 = CARTESIAN_POINT ( 'NONE',  ( -2.293366432827344421E-15, -12.48450537969573659, -198.4062500020484094 ) ) ;
#36682 = CARTESIAN_POINT ( 'NONE',  ( 5.405949406249992428, -9.363379034771808662, -63.09375000204836681 ) ) ;
#36683 = CARTESIAN_POINT ( 'NONE',  ( -10.81189881249999729, 1.324075727343319199E-15, -39.59375000204837391 ) ) ;
#36684 = CARTESIAN_POINT ( 'NONE',  ( -5.000000000000003553, -8.660254037844383745, -172.3750000040968189 ) ) ;
#36685 = CARTESIAN_POINT ( 'NONE',  ( 5.405949406249992428, -9.363379034771808662, -16.78125000204835970 ) ) ;
#36686 = CARTESIAN_POINT ( 'NONE',  ( 10.81189881249999551, -6.242252689847874514, -19.46875000204836681 ) ) ;
#36687 = CARTESIAN_POINT ( 'NONE',  ( 4.999999999999992006, -8.660254037844389075, -92.62500000409677625 ) ) ;
#36688 = CARTESIAN_POINT ( 'NONE',  ( -10.81189881249999729, 1.324075727343319199E-15, -126.5937500020483668 ) ) ;
#36689 = CARTESIAN_POINT ( 'NONE',  ( -5.000000000000003553, -8.660254037844383745, -108.9999999999999858 ) ) ;
#36690 = CARTESIAN_POINT ( 'NONE',  ( 10.81189881249999551, -6.242252689847874514, -39.15625000204835970 ) ) ;
#36691 =( BOUNDED_CURVE ( )  B_SPLINE_CURVE ( 2, ( #10371, #24424, #4550, #30673, #690, #10580, #20944 ),
 .UNSPECIFIED., .F., .F. ) 
 B_SPLINE_CURVE_WITH_KNOTS ( ( 3, 2, 2, 3 ),
 ( 0.1567164179104477695, 0.1579601990049751270, 0.1592039800995025123, 0.1604477611940298698 ),
 .UNSPECIFIED. ) 
 CURVE ( )  GEOMETRIC_REPRESENTATION_ITEM ( )  RATIONAL_B_SPLINE_CURVE ( ( 1.000000000000000000, 0.8660254037844387076, 1.000000000000000000, 0.8660254037844387076, 1.000000000000000000, 0.8660254037844357100, 1.000000000000003109 ) ) 
 REPRESENTATION_ITEM ( '' )  );
#36692 = CARTESIAN_POINT ( 'NONE',  ( -5.000000000000003553, -8.660254037844383745, -26.87500000409676204 ) ) ;
#36693 = CARTESIAN_POINT ( 'NONE',  ( 7.070501591499377789E-16, 11.54700538379251284, -60.12499999999997868 ) ) ;
#36694 = CARTESIAN_POINT ( 'NONE',  ( -5.405949406249996869, 9.363379034771805109, -133.0312500020484094 ) ) ;
#36695 = CARTESIAN_POINT ( 'NONE',  ( -10.81189881249999729, 1.324075727343319199E-15, -110.2812500020483810 ) ) ;
#36696 = ORIENTED_EDGE ( 'NONE', *, *, #22279, .F. ) ;
#36697 = CARTESIAN_POINT ( 'NONE',  ( -9.999999999999998224, 5.773502691896259087, -109.7500000040967763 ) ) ;
#36698 = CARTESIAN_POINT ( 'NONE',  ( 9.999999999999479527, 5.773502691896553074, -101.2500000040967763 ) ) ;
#36699 = CARTESIAN_POINT ( 'NONE',  ( 10.81189881249999907, 6.242252689847868297, -62.71875000204838102 ) ) ;
#36700 = ORIENTED_EDGE ( 'NONE', *, *, #40000, .F. ) ;
#36701 = CARTESIAN_POINT ( 'NONE',  ( 9.999999999999996447, -5.773502691896262640, -33.62499999999997158 ) ) ;
#36702 = AXIS2_PLACEMENT_3D ( 'NONE', #17255, #30458, #14004 ) ;
#36703 = CARTESIAN_POINT ( 'NONE',  ( 10.81189881249999729, 0.000000000000000000, -34.53125000204837391 ) ) ;
#36704 = CARTESIAN_POINT ( 'NONE',  ( 9.999999999999998224, 0.000000000000000000, -29.37500000409676204 ) ) ;
#36705 = CARTESIAN_POINT ( 'NONE',  ( -4.999999999999996447, 8.660254037844387298, -39.37500000409676915 ) ) ;
#36706 = CARTESIAN_POINT ( 'NONE',  ( 10.00000000000000000, 5.773502691896255534, -133.8750000000000000 ) ) ;
#36707 = CARTESIAN_POINT ( 'NONE',  ( -5.405949406250003975, -9.363379034771801557, -141.5312500020483810 ) ) ;
#36708 = CARTESIAN_POINT ( 'NONE',  ( -4.999999999999996447, 8.660254037844387298, -129.3750000040967905 ) ) ;
#36709 = ORIENTED_EDGE ( 'NONE', *, *, #12040, .F. ) ;
#36710 = VERTEX_POINT ( 'NONE', #27567 ) ;
#36711 = CARTESIAN_POINT ( 'NONE',  ( 9.999999999999998224, 0.000000000000000000, -155.3750000040967905 ) ) ;
#36712 = CARTESIAN_POINT ( 'NONE',  ( -9.999999999999998224, 1.224646799147353059E-15, -121.6250000040967905 ) ) ;
#36713 = CARTESIAN_POINT ( 'NONE',  ( -10.81189881249999729, 6.242252689847871849, -167.2187500020483810 ) ) ;
#36714 = CARTESIAN_POINT ( 'NONE',  ( 7.644554776091147741E-16, 12.48450537969573659, -199.1562500020484094 ) ) ;
#36715 = ADVANCED_FACE ( 'NONE', ( #10508 ), #24344, .T. ) ;
#36716 = CARTESIAN_POINT ( 'NONE',  ( 5.405949406249992428, -9.363379034771808662, -19.59375000204835615 ) ) ;
#36717 = PLANE ( 'NONE',  #36374 ) ;
#36718 = EDGE_CURVE ( 'NONE', #17318, #11384, #7109, .T. ) ;
#36719 = CARTESIAN_POINT ( 'NONE',  ( 5.405949406249999534, 9.363379034771803333, -160.0937500020484094 ) ) ;
#36720 = CARTESIAN_POINT ( 'NONE',  ( 5.405949406249999534, 9.363379034771803333, -140.5937500020483810 ) ) ;
#36721 = EDGE_CURVE ( 'NONE', #31616, #33286, #23695, .T. ) ;
#36722 = CARTESIAN_POINT ( 'NONE',  ( -5.405949406250003975, -9.363379034771801557, -120.3437500020483952 ) ) ;
#36723 = CARTESIAN_POINT ( 'NONE',  ( -9.999999999999998224, 5.773502691896259087, -198.2500000040968189 ) ) ;
#36724 = CARTESIAN_POINT ( 'NONE',  ( 5.405949406249992428, -9.363379034771808662, -123.2812500020483952 ) ) ;
#36725 = CARTESIAN_POINT ( 'NONE',  ( -2.293366432827344421E-15, -12.48450537969573659, -10.71875000204836681 ) ) ;
#36726 = CARTESIAN_POINT ( 'NONE',  ( -2.293366432827344421E-15, -12.48450537969573659, -138.2187500020483810 ) ) ;
#36727 = CARTESIAN_POINT ( 'NONE',  ( 9.999999999999998224, 0.000000000000000000, -63.87500000409676915 ) ) ;
#36728 =( BOUNDED_CURVE ( )  B_SPLINE_CURVE ( 2, ( #12514, #9917, #29152, #32188, #19210, #42496, #19003 ),
 .UNSPECIFIED., .F., .F. ) 
 B_SPLINE_CURVE_WITH_KNOTS ( ( 3, 2, 2, 3 ),
 ( 0.2798507462686568026, 0.2810945273631841879, 0.2823383084577115731, 0.2835820895522389029 ),
 .UNSPECIFIED. ) 
 CURVE ( )  GEOMETRIC_REPRESENTATION_ITEM ( )  RATIONAL_B_SPLINE_CURVE ( ( 0.9999999999999880096, 0.8660254037844506980, 1.000000000000000000, 0.8660254037844387076, 1.000000000000000000, 0.8660254037844267172, 1.000000000000011990 ) ) 
 REPRESENTATION_ITEM ( '' )  );
#36729 = CARTESIAN_POINT ( 'NONE',  ( 9.999999999999742428, 5.773502691896404748, -125.2500000040967478 ) ) ;
#36730 = CARTESIAN_POINT ( 'NONE',  ( 4.999999999999992006, -8.660254037844389075, -152.2500000000000000 ) ) ;
#36731 = CARTESIAN_POINT ( 'NONE',  ( 10.00000000000154010, -5.773502691895370020, -17.12499999999992895 ) ) ;
#36732 = CARTESIAN_POINT ( 'NONE',  ( 7.644554776091147741E-16, 12.48450537969573659, -84.96875000204838102 ) ) ;
#36733 = CARTESIAN_POINT ( 'NONE',  ( -5.405949406249996869, 9.363379034771805109, -62.34375000204836681 ) ) ;
#36734 = CARTESIAN_POINT ( 'NONE',  ( -10.81189881249999729, 1.324075727343319199E-15, -45.78125000204838813 ) ) ;
#36735 = CARTESIAN_POINT ( 'NONE',  ( 10.81189881249999551, -6.242252689847874514, -50.96875000204836681 ) ) ;
#36736 = DIRECTION ( 'NONE',  ( -0.000000000000000000, -0.000000000000000000, 1.000000000000000000 ) ) ;
#36737 = CARTESIAN_POINT ( 'NONE',  ( -10.81189881249999729, 6.242252689847871849, -159.7187500020483526 ) ) ;
#36738 = CARTESIAN_POINT ( 'NONE',  ( -2.121150477449813534E-15, -11.54700538379251284, -126.8749999999999858 ) ) ;
#36739 = CARTESIAN_POINT ( 'NONE',  ( 10.81189881249999551, -6.242252689847874514, -141.1562500020484094 ) ) ;
#36740 = FACE_OUTER_BOUND ( 'NONE', #36906, .T. ) ;
#36741 = CARTESIAN_POINT ( 'NONE',  ( -5.000000000000003553, -8.660254037844383745, -86.49999999999998579 ) ) ;
#36742 = CARTESIAN_POINT ( 'NONE',  ( 10.81189881249999729, 0.000000000000000000, -21.03125000204836326 ) ) ;
#36743 = ORIENTED_EDGE ( 'NONE', *, *, #18509, .T. ) ;
#36744 =( BOUNDED_CURVE ( )  B_SPLINE_CURVE ( 2, ( #20930, #24617, #10998, #30664, #40770, #1092, #34112 ),
 .UNSPECIFIED., .F., .F. ) 
 B_SPLINE_CURVE_WITH_KNOTS ( ( 3, 2, 2, 3 ),
 ( 0.2350746268656717097, 0.2363184079601990950, 0.2375621890547264525, 0.2388059701492538378 ),
 .UNSPECIFIED. ) 
 CURVE ( )  GEOMETRIC_REPRESENTATION_ITEM ( )  RATIONAL_B_SPLINE_CURVE ( ( 0.9999999999999940048, 0.8660254037844447028, 1.000000000000000000, 0.8660254037844387076, 1.000000000000000000, 0.8660254037844267172, 1.000000000000011990 ) ) 
 REPRESENTATION_ITEM ( '' )  );
#36745 = CARTESIAN_POINT ( 'NONE',  ( 5.405949406249992428, -9.363379034771808662, -106.7812500020483810 ) ) ;
#36746 = CARTESIAN_POINT ( 'NONE',  ( -2.121150477449813534E-15, -11.54700538379251284, -133.2500000040967905 ) ) ;
#36747 = CARTESIAN_POINT ( 'NONE',  ( -2.121150477449813534E-15, -11.54700538379251284, -111.8749999999999858 ) ) ;
#36748 = CARTESIAN_POINT ( 'NONE',  ( -5.000000000000003553, -8.660254037844383745, -40.37500000409677625 ) ) ;
#36749 = ADVANCED_FACE ( 'NONE', ( #33623, #1246 ), #821, .F. ) ;
#36750 = CARTESIAN_POINT ( 'NONE',  ( -2.121150477449813534E-15, -11.54700538379251284, -58.25000000409677625 ) ) ;
#36751 = CARTESIAN_POINT ( 'NONE',  ( 7.644554776091147741E-16, 12.48450537969573659, -50.65625000204837391 ) ) ;
#36752 = CARTESIAN_POINT ( 'NONE',  ( 10.00000000000051159, -5.773502691895965988, -146.1250000000000284 ) ) ;
#36753 = CARTESIAN_POINT ( 'NONE',  ( 7.644554776091147741E-16, 12.48450537969573659, -152.6562500020484094 ) ) ;
#36754 = EDGE_CURVE ( 'NONE', #42281, #24195, #36853, .T. ) ;
#36755 = CARTESIAN_POINT ( 'NONE',  ( -10.81189881249999729, 6.242252689847871849, -137.2187500020483810 ) ) ;
#36756 = CARTESIAN_POINT ( 'NONE',  ( -5.000000000000003553, -8.660254037844383745, -23.49999999999996447 ) ) ;
#36757 = CARTESIAN_POINT ( 'NONE',  ( 10.00000000000012790, 5.773502691896179151, -174.3750000000000000 ) ) ;
#36758 = ADVANCED_FACE ( 'NONE', ( #40702, #37703 ), #31027, .F. ) ;
#36759 = ORIENTED_EDGE ( 'NONE', *, *, #21422, .F. ) ;
#36760 = CARTESIAN_POINT ( 'NONE',  ( -5.000000000000003553, -8.660254037844383745, -30.99999999999997158 ) ) ;
#36762 = EDGE_LOOP ( 'NONE', ( #12963, #26613, #25607, #14770 ) ) ;
#36761 = CARTESIAN_POINT ( 'NONE',  ( -10.81189881249999907, -6.242252689847864744, -65.15625000204838102 ) ) ;
#36763 = DATE_AND_TIME ( #7197, #35238 ) ;
#36765 = ORIENTED_EDGE ( 'NONE', *, *, #16143, .F. ) ;
#36764 = CARTESIAN_POINT ( 'NONE',  ( 10.81189881249999551, -6.242252689847874514, -122.9687500020483810 ) ) ;
#36766 = CARTESIAN_POINT ( 'NONE',  ( -10.81189881249999729, -6.242252689847864744, -24.46875000204837036 ) ) ;
#36767 = CARTESIAN_POINT ( 'NONE',  ( 5.405949406249999534, 9.363379034771803333, -194.5937500020484094 ) ) ;
#36768 = CARTESIAN_POINT ( 'NONE',  ( 5.405949406249992428, -9.363379034771808662, -51.09375000204835260 ) ) ;
#36769 = CARTESIAN_POINT ( 'NONE',  ( 10.00000000000038369, -5.773502691896038819, -155.5000000040967905 ) ) ;
#36770 = FACE_OUTER_BOUND ( 'NONE', #22497, .T. ) ;
#36771 = CARTESIAN_POINT ( 'NONE',  ( 7.644554776091147741E-16, 12.48450537969573659, -183.9687500020484663 ) ) ;
#36772 = CARTESIAN_POINT ( 'NONE',  ( -5.405949406250003975, -9.363379034771801557, -162.3437500020484094 ) ) ;
#36773 = CARTESIAN_POINT ( 'NONE',  ( 5.405949406249999534, 9.363379034771803333, -152.5937500020483810 ) ) ;
#36775 = EDGE_CURVE ( 'NONE', #9067, #35021, #34695, .T. ) ;
#36774 = CARTESIAN_POINT ( 'NONE',  ( -10.81189881249999729, -6.242252689847864744, -159.4687500020484094 ) ) ;
#36776 = CARTESIAN_POINT ( 'NONE',  ( 4.999999999999992006, -8.660254037844389075, -118.1250000040967905 ) ) ;
#36777 = DIRECTION ( 'NONE',  ( -0.000000000000000000, -0.000000000000000000, 1.000000000000000000 ) ) ;
#36778 = CARTESIAN_POINT ( 'NONE',  ( -9.999999999999998224, 5.773502691896259087, -176.8750000000000000 ) ) ;
#36779 = EDGE_CURVE ( 'NONE', #982, #6545, #37998, .T. ) ;
#36780 = CARTESIAN_POINT ( 'NONE',  ( -5.405949406249996869, 9.363379034771805109, -98.34375000204838102 ) ) ;
#36781 = CARTESIAN_POINT ( 'NONE',  ( 7.070501591499376803E-16, 11.54700538379251284, -138.1250000000000000 ) ) ;
#36782 = CARTESIAN_POINT ( 'NONE',  ( 5.405949406249999534, 9.363379034771803333, -70.28125000204838102 ) ) ;
#36783 = CARTESIAN_POINT ( 'NONE',  ( 9.999999999999998224, 0.000000000000000000, -146.3750000040967905 ) ) ;
#36784 = CARTESIAN_POINT ( 'NONE',  ( -10.81189881249999729, 1.324075727343319199E-15, -185.0937500020483810 ) ) ;
#36785 = CARTESIAN_POINT ( 'NONE',  ( 10.81189881249999729, 0.000000000000000000, -118.5312500020483952 ) ) ;
#36786 = CARTESIAN_POINT ( 'NONE',  ( 7.644554776091147741E-16, 12.48450537969573659, -158.6562500020484094 ) ) ;
#36787 = CARTESIAN_POINT ( 'NONE',  ( -10.81189881249999729, 6.242252689847871849, -53.40625000204837391 ) ) ;
#36788 = CARTESIAN_POINT ( 'NONE',  ( 9.999999999999998224, 0.000000000000000000, -140.3750000040967905 ) ) ;
#36789 = CARTESIAN_POINT ( 'NONE',  ( -10.00000000000000000, -5.773502691896251982, -107.6249999999999858 ) ) ;
#36790 = VERTEX_POINT ( 'NONE', #38547 ) ;
#36791 = CARTESIAN_POINT ( 'NONE',  ( -10.81189881249999729, 1.324075727343319199E-15, -131.2812500020483810 ) ) ;
#36792 = CARTESIAN_POINT ( 'NONE',  ( -5.405949406249996869, 9.363379034771805109, -148.0312500020483810 ) ) ;
#36793 = CARTESIAN_POINT ( 'NONE',  ( 10.81189881249999551, -6.242252689847874514, -189.1562500020484379 ) ) ;
#36794 = CARTESIAN_POINT ( 'NONE',  ( 5.405949406249999534, 9.363379034771803333, -79.09375000204838102 ) ) ;
#36795 = VERTEX_POINT ( 'NONE', #38338 ) ;
#36796 = CARTESIAN_POINT ( 'NONE',  ( -9.999999999999998224, 1.224646799147353059E-15, -46.24999999999998579 ) ) ;
#36797 = CARTESIAN_POINT ( 'NONE',  ( 10.81189881249999729, 0.000000000000000000, -182.8437500020483810 ) ) ;
#36798 = CARTESIAN_POINT ( 'NONE',  ( 10.00000000000000000, 5.773502691896255534, -69.75000000409679046 ) ) ;
#36799 = CARTESIAN_POINT ( 'NONE',  ( -9.999999999999998224, 1.224646799147353059E-15, -172.2500000000000000 ) ) ;
#36800 = FACE_OUTER_BOUND ( 'NONE', #8121, .T. ) ;
#36801 = CARTESIAN_POINT ( 'NONE',  ( -5.405949406249996869, 9.363379034771805109, -79.03125000204838102 ) ) ;
#36802 = CARTESIAN_POINT ( 'NONE',  ( 7.644554776091147741E-16, 12.48450537969573659, -59.65625000204838813 ) ) ;
#36803 = ADVANCED_FACE ( 'NONE', ( #28644 ), #18050, .T. ) ;
#36804 = CARTESIAN_POINT ( 'NONE',  ( 10.00000000000000000, 5.773502691896255534, -54.75000000409676915 ) ) ;
#36805 = CARTESIAN_POINT ( 'NONE',  ( -10.81189881249999729, 6.242252689847871849, -6.718750002048357040 ) ) ;
#36806 = CARTESIAN_POINT ( 'NONE',  ( -9.999999999999525713, -2.663671193123883896, -0.06732983108239683212 ) ) ;
#36807 = CARTESIAN_POINT ( 'NONE',  ( -5.405949406250003975, -9.363379034771801557, -185.0312500020484094 ) ) ;
#36808 = CARTESIAN_POINT ( 'NONE',  ( -10.81189881249999729, 1.324075727343319199E-15, -3.781250002048375247 ) ) ;
#36809 = CARTESIAN_POINT ( 'NONE',  ( -2.293366432827344421E-15, -12.48450537969573659, -0.2187500020483489072 ) ) ;
#36810 = LINE ( 'NONE', #42636, #8946 ) ;
#36811 =( BOUNDED_CURVE ( )  B_SPLINE_CURVE ( 2, ( #2373, #8204, #8842, #11844, #21787, #31945, #21574 ),
 .UNSPECIFIED., .F., .F. ) 
 B_SPLINE_CURVE_WITH_KNOTS ( ( 3, 2, 2, 3 ),
 ( 0.2425373134328359381, 0.2437810945273632957, 0.2450248756218906532, 0.2462686567164180107 ),
 .UNSPECIFIED. ) 
 CURVE ( )  GEOMETRIC_REPRESENTATION_ITEM ( )  RATIONAL_B_SPLINE_CURVE ( ( 0.9999999999999880096, 0.8660254037844506980, 1.000000000000000000, 0.8660254037844387076, 1.000000000000000000, 0.8660254037844267172, 1.000000000000011990 ) ) 
 REPRESENTATION_ITEM ( '' )  );
#36812 = CARTESIAN_POINT ( 'NONE',  ( 4.999999999999992006, -8.660254037844389075, -89.24999999999998579 ) ) ;
#36813 = CARTESIAN_POINT ( 'NONE',  ( 9.999999999999998224, 0.000000000000000000, -177.8750000040967905 ) ) ;
#36814 = CARTESIAN_POINT ( 'NONE',  ( -9.999999999999998224, 1.224646799147353059E-15, -80.74999999999998579 ) ) ;
#36816 = ORIENTED_EDGE ( 'NONE', *, *, #25843, .T. ) ;
#36815 = CARTESIAN_POINT ( 'NONE',  ( -5.405949406250003975, -9.363379034771801557, -87.53125000204838102 ) ) ;
#36818 = ORIENTED_EDGE ( 'NONE', *, *, #16142, .T. ) ;
#36817 = CARTESIAN_POINT ( 'NONE',  ( 9.999999999999998224, 0.000000000000000000, -167.3750000040967905 ) ) ;
#36819 = ORIENTED_EDGE ( 'NONE', *, *, #27968, .T. ) ;
#36820 = CARTESIAN_POINT ( 'NONE',  ( -5.405949406249996869, 9.363379034771805109, -24.84375000204835970 ) ) ;
#36821 = CARTESIAN_POINT ( 'NONE',  ( 10.81189881249999907, 6.242252689847868297, -25.40625000204838813 ) ) ;
#36822 = CARTESIAN_POINT ( 'NONE',  ( 10.81189881249999907, 6.242252689847868297, -74.71875000204838102 ) ) ;
#36823 = CARTESIAN_POINT ( 'NONE',  ( -9.999999999999998224, 1.224646799147353059E-15, -84.12500000409677625 ) ) ;
#36824 = CARTESIAN_POINT ( 'NONE',  ( 9.999999999999998224, 0.000000000000000000, -46.99999999999998579 ) ) ;
#36825 = CARTESIAN_POINT ( 'NONE',  ( 10.81189881249999729, 0.000000000000000000, -193.3437500020484094 ) ) ;
#36826 = CARTESIAN_POINT ( 'NONE',  ( 5.405949406249992428, -9.363379034771808662, -153.0937500020483810 ) ) ;
#36827 = CARTESIAN_POINT ( 'NONE',  ( -5.405949406250003975, -9.363379034771801557, -0.3437500020483652552 ) ) ;
#36828 = FACE_OUTER_BOUND ( 'NONE', #2842, .T. ) ;
#36829 = CARTESIAN_POINT ( 'NONE',  ( 7.070501591499376803E-16, 11.54700538379251284, -112.6249999999999858 ) ) ;
#36830 = CARTESIAN_POINT ( 'NONE',  ( -10.00000000000000000, -5.773502691896251982, -3.000000004096758044 ) ) ;
#36831 = DIRECTION ( 'NONE',  ( -0.000000000000000000, -0.000000000000000000, 1.000000000000000000 ) ) ;
#36832 = CARTESIAN_POINT ( 'NONE',  ( 10.81189881249999551, -6.242252689847874514, -121.4687500020484094 ) ) ;
#36833 = CARTESIAN_POINT ( 'NONE',  ( 9.999999999999998224, 0.000000000000000000, -141.5000000000000000 ) ) ;
#36834 = CARTESIAN_POINT ( 'NONE',  ( 10.81189881249999729, 0.000000000000000000, -87.03125000204838102 ) ) ;
#36835 = CARTESIAN_POINT ( 'NONE',  ( 7.644554776091147741E-16, 12.48450537969573659, -96.96875000204838102 ) ) ;
#36836 = CARTESIAN_POINT ( 'NONE',  ( 10.81189881249999729, 0.000000000000000000, -68.84375000204836681 ) ) ;
#36837 = CARTESIAN_POINT ( 'NONE',  ( 10.81189881249999907, 6.242252689847868297, -73.40625000204836681 ) ) ;
#36838 = CARTESIAN_POINT ( 'NONE',  ( -9.999999999999998224, 5.773502691896259087, -162.2500000040967620 ) ) ;
#36839 = CARTESIAN_POINT ( 'NONE',  ( -5.405949406249996869, 9.363379034771805109, -155.5312500020484094 ) ) ;
#36840 = CARTESIAN_POINT ( 'NONE',  ( -2.293366432827344421E-15, -12.48450537969573659, -169.9062500020483810 ) ) ;
#36841 = EDGE_CURVE ( 'NONE', #2222, #29057, #27997, .T. ) ;
#36842 = CARTESIAN_POINT ( 'NONE',  ( -9.999999999999998224, 1.224646799147353059E-15, -200.0000000000000000 ) ) ;
#36843 = CARTESIAN_POINT ( 'NONE',  ( 10.81189881249999907, 6.242252689847868297, -1.218750002048352155 ) ) ;
#36844 = CARTESIAN_POINT ( 'NONE',  ( 9.999999999999998224, 0.000000000000000000, -53.37500000409675494 ) ) ;
#36845 = CARTESIAN_POINT ( 'NONE',  ( 10.81189881249999907, 6.242252689847868297, -103.2187500020483810 ) ) ;
#36846 = CARTESIAN_POINT ( 'NONE',  ( -1.040834085586084257E-14, 145.0000000000000000, 22.49999999999999289 ) ) ;
#36847 = CARTESIAN_POINT ( 'NONE',  ( -2.121150477449813534E-15, -11.54700538379251284, -78.87500000000000000 ) ) ;
#36848 = CARTESIAN_POINT ( 'NONE',  ( 10.81189881249999551, -6.242252689847874514, -1.656250002048359482 ) ) ;
#36849 = CARTESIAN_POINT ( 'NONE',  ( -9.999999999999998224, 5.773502691896259087, -88.75000000409677625 ) ) ;
#36850 = CARTESIAN_POINT ( 'NONE',  ( 0.000000000000000000, 0.000000000000000000, -200.0000000000000000 ) ) ;
#36851 = CARTESIAN_POINT ( 'NONE',  ( -10.81189881249999729, 1.324075727343319199E-15, -101.2812500020483952 ) ) ;
#36852 = CARTESIAN_POINT ( 'NONE',  ( -2.293366432827344421E-15, -12.48450537969573659, -81.40625000204838102 ) ) ;
#36853 =( BOUNDED_CURVE ( )  B_SPLINE_CURVE ( 2, ( #24126, #37267, #20864, #30807, #4470, #34048, #17612 ),
 .UNSPECIFIED., .F., .F. ) 
 B_SPLINE_CURVE_WITH_KNOTS ( ( 3, 2, 2, 3 ),
 ( 0.2238805970149254365, 0.2251243781094527940, 0.2263681592039801793, 0.2276119402985075368 ),
 .UNSPECIFIED. ) 
 CURVE ( )  GEOMETRIC_REPRESENTATION_ITEM ( )  RATIONAL_B_SPLINE_CURVE ( ( 0.9999999999999940048, 0.8660254037844447028, 1.000000000000000000, 0.8660254037844387076, 1.000000000000000000, 0.8660254037844297148, 1.000000000000008882 ) ) 
 REPRESENTATION_ITEM ( '' )  );
#36854 = CARTESIAN_POINT ( 'NONE',  ( -2.121150477449813534E-15, -11.54700538379251284, -73.25000000409674783 ) ) ;
#36855 = CARTESIAN_POINT ( 'NONE',  ( 0.000000000000000000, 0.000000000000000000, -160.0000000000000000 ) ) ;
#36856 = CARTESIAN_POINT ( 'NONE',  ( 5.405949406249992428, -9.363379034771808662, -33.09375000204836681 ) ) ;
#36857 = ORIENTED_EDGE ( 'NONE', *, *, #22229, .T. ) ;
#36858 = CARTESIAN_POINT ( 'NONE',  ( -9.999999999999998224, 5.773502691896259087, -8.874999999999976907 ) ) ;
#36859 = CARTESIAN_POINT ( 'NONE',  ( 5.405949406249992428, -9.363379034771808662, -28.78125000204837036 ) ) ;
#36860 = CARTESIAN_POINT ( 'NONE',  ( -9.999999999999998224, 1.224646799147353059E-15, -143.7500000000000000 ) ) ;
#36861 = CARTESIAN_POINT ( 'NONE',  ( -5.500000000000003553, 20.00000000000000000, -232.0000000000000000 ) ) ;
#36862 = CARTESIAN_POINT ( 'NONE',  ( 10.00000000000000000, 5.773502691896255534, -3.750000004096754047 ) ) ;
#36863 = EDGE_CURVE ( 'NONE', #33393, #36337, #21722, .T. ) ;
#36864 = AXIS2_PLACEMENT_3D ( 'NONE', #36850, #1253, #14377 ) ;
#36865 = CARTESIAN_POINT ( 'NONE',  ( 9.999999999999998224, 0.000000000000000000, -194.0000000000000000 ) ) ;
#36866 = DIRECTION ( 'NONE',  ( -0.000000000000000000, -0.000000000000000000, 1.000000000000000000 ) ) ;
#36868 = ORIENTED_EDGE ( 'NONE', *, *, #37982, .T. ) ;
#36867 = CARTESIAN_POINT ( 'NONE',  ( -10.81189881249999729, 1.324075727343319199E-15, -114.7812500020483952 ) ) ;
#36869 = CARTESIAN_POINT ( 'NONE',  ( 100.0000000000000142, 19.99999999999999645, -160.0000000000000000 ) ) ;
#36870 = ORIENTED_EDGE ( 'NONE', *, *, #10491, .F. ) ;
#36871 = VERTEX_POINT ( 'NONE', #25197 ) ;
#36872 = CARTESIAN_POINT ( 'NONE',  ( 5.405949406249999534, 9.363379034771803333, -46.28125000204838813 ) ) ;
#36873 = DATE_AND_TIME ( #36661, #101 ) ;
#36874 = CARTESIAN_POINT ( 'NONE',  ( -10.81189881249999729, 6.242252689847871849, -93.71875000204838102 ) ) ;
#36875 = CARTESIAN_POINT ( 'NONE',  ( 5.405949406249999534, 9.363379034771803333, -127.2812500020483810 ) ) ;
#36876 = EDGE_LOOP ( 'NONE', ( #27646, #15449, #33574, #41300 ) ) ;
#36877 = CARTESIAN_POINT ( 'NONE',  ( 4.999999999999992006, -8.660254037844389075, -83.24999999999997158 ) ) ;
#36878 = CARTESIAN_POINT ( 'NONE',  ( -10.81189881249999729, 6.242252689847871849, -195.7187500020484379 ) ) ;
#36879 = CARTESIAN_POINT ( 'NONE',  ( 10.81189881249999551, -6.242252689847874514, -174.1562500020484094 ) ) ;
#36880 = CARTESIAN_POINT ( 'NONE',  ( -9.999999999999227285, -5.773502691896698735, -139.1249999999999716 ) ) ;
#36881 = CARTESIAN_POINT ( 'NONE',  ( -10.81189881249999729, -6.242252689847864744, -120.4687500020483952 ) ) ;
#36882 = CARTESIAN_POINT ( 'NONE',  ( -10.81189881249999729, 6.242252689847871849, -92.21875000204838102 ) ) ;
#36883 = CARTESIAN_POINT ( 'NONE',  ( -10.81189881249999907, -6.242252689847864744, -198.4687500020484379 ) ) ;
#36884 = CARTESIAN_POINT ( 'NONE',  ( 5.405949406249999534, 9.363379034771803333, -101.7812500020483952 ) ) ;
#36885 = CARTESIAN_POINT ( 'NONE',  ( 9.999999999999996447, -5.773502691896262640, -187.0000000040968189 ) ) ;
#36886 = CARTESIAN_POINT ( 'NONE',  ( 7.644554776091147741E-16, 12.48450537969573659, -104.4687500020483668 ) ) ;
#36887 = CARTESIAN_POINT ( 'NONE',  ( 7.644554776091147741E-16, 12.48450537969573659, -181.1562500020484379 ) ) ;
#36888 = ADVANCED_FACE ( 'NONE', ( #5115 ), #41348, .F. ) ;
#36889 = AXIS2_PLACEMENT_3D ( 'NONE', #22268, #5020, #21837 ) ;
#36890 = CARTESIAN_POINT ( 'NONE',  ( 9.999999999999479527, 5.773502691896553074, -3.374999999999938716 ) ) ;
#36891 = CARTESIAN_POINT ( 'NONE',  ( 5.000000000000000000, 8.660254037844385522, -122.1250000040967905 ) ) ;
#36892 = CARTESIAN_POINT ( 'NONE',  ( 7.644554776091147741E-16, 12.48450537969573659, -193.1562500020484094 ) ) ;
#36893 = CARTESIAN_POINT ( 'NONE',  ( -5.405949406249996869, 9.363379034771805109, -57.84375000204835970 ) ) ;
#36894 = CARTESIAN_POINT ( 'NONE',  ( 7.644554776091147741E-16, 12.48450537969573659, -39.96875000204835970 ) ) ;
#36895 = CARTESIAN_POINT ( 'NONE',  ( 10.00000000000000000, 5.773502691896255534, -168.7500000040967905 ) ) ;
#36896 = CARTESIAN_POINT ( 'NONE',  ( 7.644554776091147741E-16, 12.48450537969573659, -20.65625000204838102 ) ) ;
#36897 = CARTESIAN_POINT ( 'NONE',  ( -10.81189881249999729, 1.324075727343319199E-15, -21.59375000204835615 ) ) ;
#36898 = CARTESIAN_POINT ( 'NONE',  ( 5.321294541346989426, 0.000000000000000000, -219.9999999999999716 ) ) ;
#36899 = CARTESIAN_POINT ( 'NONE',  ( 5.405949406249999534, 9.363379034771803333, -133.0937500020483810 ) ) ;
#36900 = CARTESIAN_POINT ( 'NONE',  ( -9.999999999999998224, 1.224646799147353059E-15, -104.7499999999999858 ) ) ;
#36901 = CARTESIAN_POINT ( 'NONE',  ( -10.81189881249999907, -6.242252689847864744, -24.65625000204838102 ) ) ;
#36902 = DIRECTION ( 'NONE',  ( -1.000000000000000000, 0.000000000000000000, 0.000000000000000000 ) ) ;
#36903 = CARTESIAN_POINT ( 'NONE',  ( -4.999999999999996447, 8.660254037844387298, -62.99999999999997158 ) ) ;
#36904 = CARTESIAN_POINT ( 'NONE',  ( 10.81189881249999551, -6.242252689847874514, -123.1562500020483952 ) ) ;
#36905 = CARTESIAN_POINT ( 'NONE',  ( 7.644554776091147741E-16, 12.48450537969573659, -107.6562500020483810 ) ) ;
#36906 = EDGE_LOOP ( 'NONE', ( #35144, #15349, #8753, #40602 ) ) ;
#36907 = PLANE ( 'NONE',  #6566 ) ;
#36908 = CARTESIAN_POINT ( 'NONE',  ( -9.999999999999998224, 5.773502691896259087, -96.25000000409677625 ) ) ;
#36909 = FACE_OUTER_BOUND ( 'NONE', #4075, .T. ) ;
#36910 = CARTESIAN_POINT ( 'NONE',  ( 10.81189881249999729, 0.000000000000000000, -55.34375000204835970 ) ) ;
#36911 = VERTEX_POINT ( 'NONE', #4903 ) ;
#36912 = CARTESIAN_POINT ( 'NONE',  ( -5.000000000000003553, -8.660254037844383745, -36.99999999999997868 ) ) ;
#36913 = CARTESIAN_POINT ( 'NONE',  ( 10.81189881249999729, 0.000000000000000000, -37.53125000204838102 ) ) ;
#36914 = EDGE_CURVE ( 'NONE', #41090, #26035, #19203, .T. ) ;
#36915 = DIRECTION ( 'NONE',  ( -0.000000000000000000, -0.000000000000000000, -1.000000000000000000 ) ) ;
#36916 = CARTESIAN_POINT ( 'NONE',  ( -2.121150477449813534E-15, -11.54700538379251284, -37.25000000409675494 ) ) ;
#36917 = AXIS2_PLACEMENT_3D ( 'NONE', #21525, #25000, #5128 ) ;
#36918 = VECTOR ( 'NONE', #33386, 1000.000000000000000 ) ;
#36919 = CARTESIAN_POINT ( 'NONE',  ( -9.999999999999998224, 1.224646799147353059E-15, -90.12500000409677625 ) ) ;
#36920 = CARTESIAN_POINT ( 'NONE',  ( -10.81189881249999729, 1.324075727343319199E-15, -141.7812500020483810 ) ) ;
#36921 = CIRCLE ( 'NONE', #17585, 5.500000000000003553 ) ;
#36922 = LINE ( 'NONE', #37353, #12124 ) ;
#36923 = VERTEX_POINT ( 'NONE', #22157 ) ;
#36924 = ORIENTED_EDGE ( 'NONE', *, *, #31765, .T. ) ;
#36925 = CARTESIAN_POINT ( 'NONE',  ( -9.999999999999998224, 1.224646799147353059E-15, -106.6250000040967763 ) ) ;
#36926 = CARTESIAN_POINT ( 'NONE',  ( -9.999999999999998224, 1.224646799147353059E-15, -200.0000000000000000 ) ) ;
#36927 = CARTESIAN_POINT ( 'NONE',  ( -10.81189881249999729, 1.324075727343319199E-15, -167.0937500020484094 ) ) ;
#36928 = FACE_OUTER_BOUND ( 'NONE', #29031, .T. ) ;
#36929 = CARTESIAN_POINT ( 'NONE',  ( 5.405949406249992428, -9.363379034771808662, -15.09375000204835082 ) ) ;
#36930 = DIRECTION ( 'NONE',  ( 1.000000000000000000, 0.000000000000000000, 0.000000000000000000 ) ) ;
#36931 = CARTESIAN_POINT ( 'NONE',  ( 5.405949406249992428, -9.363379034771808662, -154.5937500020483810 ) ) ;
#36932 = CARTESIAN_POINT ( 'NONE',  ( 5.405949406249999534, 9.363379034771803333, -136.0937500020483810 ) ) ;
#36933 =( BOUNDED_CURVE ( )  B_SPLINE_CURVE ( 2, ( #13853, #41899, #5675, #32219, #35456, #38252, #41256 ),
 .UNSPECIFIED., .F., .F. ) 
 B_SPLINE_CURVE_WITH_KNOTS ( ( 3, 2, 2, 3 ),
 ( 0.8731343283582092551, 0.8743781094527366404, 0.8756218905472639147, 0.8768656716417913000 ),
 .UNSPECIFIED. ) 
 CURVE ( )  GEOMETRIC_REPRESENTATION_ITEM ( )  RATIONAL_B_SPLINE_CURVE ( ( 0.9999999999999641398, 0.8660254037844745678, 1.000000000000000000, 0.8660254037844387076, 1.000000000000000000, 0.8660254037844148378, 1.000000000000023981 ) ) 
 REPRESENTATION_ITEM ( '' )  );
#36934 = CARTESIAN_POINT ( 'NONE',  ( -5.405949406250003975, -9.363379034771801557, -110.0312500020483810 ) ) ;
#36935 = CARTESIAN_POINT ( 'NONE',  ( 7.644554776091147741E-16, 12.48450537969573659, -119.4687500020483952 ) ) ;
#36936 = CARTESIAN_POINT ( 'NONE',  ( 9.999999999999996447, -5.773502691896262640, -197.5000000040968189 ) ) ;
#36937 = VECTOR ( 'NONE', #26910, 1000.000000000000000 ) ;
#36938 = CARTESIAN_POINT ( 'NONE',  ( -10.81189881249999729, 1.324075727343319199E-15, -122.2812500020483952 ) ) ;
#36939 = CARTESIAN_POINT ( 'NONE',  ( -10.81189881249999907, -6.242252689847864744, -6.468750002048346381 ) ) ;
#36940 = CARTESIAN_POINT ( 'NONE',  ( 5.405949406249999534, 9.363379034771803333, -136.0937500020483810 ) ) ;
#36941 = CARTESIAN_POINT ( 'NONE',  ( -4.999999999999996447, 8.660254037844387298, -163.5000000000000000 ) ) ;
#36942 = CARTESIAN_POINT ( 'NONE',  ( -9.999999999999998224, 1.224646799147353059E-15, -99.12500000409677625 ) ) ;
#36943 = CARTESIAN_POINT ( 'NONE',  ( 9.999999999999998224, 0.000000000000000000, -156.5000000000000000 ) ) ;
#36944 = CARTESIAN_POINT ( 'NONE',  ( 4.999999999999992006, -8.660254037844389075, -18.74999999999996092 ) ) ;
#36945 = CARTESIAN_POINT ( 'NONE',  ( -5.405949406249996869, 9.363379034771805109, -83.34375000204836681 ) ) ;
#36946 = CARTESIAN_POINT ( 'NONE',  ( 5.405949406249999534, 9.363379034771803333, -67.09375000204836681 ) ) ;
#36947 = CARTESIAN_POINT ( 'NONE',  ( 10.00000000000012257, -5.773502691896187144, -170.1250000000000000 ) ) ;
#36948 = CARTESIAN_POINT ( 'NONE',  ( 10.81189881249999551, -6.242252689847874514, -42.15625000204836681 ) ) ;
#36949 = CARTESIAN_POINT ( 'NONE',  ( -10.81189881249999729, 6.242252689847871849, -45.71875000204836681 ) ) ;
#36950 = CARTESIAN_POINT ( 'NONE',  ( 4.999999999999992006, -8.660254037844389075, -110.6250000040967763 ) ) ;
#36951 = CARTESIAN_POINT ( 'NONE',  ( 10.81189881249999729, 0.000000000000000000, -155.8437500020483810 ) ) ;
#36952 = CARTESIAN_POINT ( 'NONE',  ( -4.999999999999996447, 8.660254037844387298, -132.0000000000000000 ) ) ;
#36953 = CARTESIAN_POINT ( 'NONE',  ( 5.405949406249992428, -9.363379034771808662, -130.7812500020483810 ) ) ;
#36954 = CARTESIAN_POINT ( 'NONE',  ( 0.2237483581476167049, 10.23237876573678307, -180.0000000000000000 ) ) ;
#36955 = CARTESIAN_POINT ( 'NONE',  ( 5.000000000000000000, 8.660254037844385522, -82.74999999999997158 ) ) ;
#36956 = CARTESIAN_POINT ( 'NONE',  ( -10.81189881249999729, -6.242252689847864744, -17.15625000204838102 ) ) ;
#36957 = VERTEX_POINT ( 'NONE', #35331 ) ;
#36958 = CARTESIAN_POINT ( 'NONE',  ( -10.81189881249999729, 1.324075727343319199E-15, -110.2812500020483810 ) ) ;
#36959 = CARTESIAN_POINT ( 'NONE',  ( 5.000000000000000000, 8.660254037844385522, -131.1250000040967620 ) ) ;
#36960 = LINE ( 'NONE', #3743, #19463 ) ;
#36961 = CARTESIAN_POINT ( 'NONE',  ( -2.121150477449813534E-15, -11.54700538379251284, -35.75000000409675494 ) ) ;
#36962 = DIRECTION ( 'NONE',  ( -0.000000000000000000, -0.000000000000000000, -1.000000000000000000 ) ) ;
#36963 = CARTESIAN_POINT ( 'NONE',  ( -5.405949406250003975, -9.363379034771801557, -50.03125000204838813 ) ) ;
#36964 = CARTESIAN_POINT ( 'NONE',  ( 9.999999999999998224, 0.000000000000000000, -76.99999999999998579 ) ) ;
#36965 = CARTESIAN_POINT ( 'NONE',  ( 7.644554776091147741E-16, 12.48450537969573659, -149.6562500020484094 ) ) ;
#36966 = CARTESIAN_POINT ( 'NONE',  ( -5.405949406250003975, -9.363379034771801557, -132.3437500020484094 ) ) ;
#36968 = EDGE_CURVE ( 'NONE', #25614, #4287, #15906, .T. ) ;
#36967 = CARTESIAN_POINT ( 'NONE',  ( 5.000000000000000000, 8.660254037844385522, -144.2500000000000000 ) ) ;
#36969 = ORIENTED_EDGE ( 'NONE', *, *, #41499, .T. ) ;
#36970 = EDGE_CURVE ( 'NONE', #14017, #37834, #23629, .T. ) ;
#36971 = FACE_OUTER_BOUND ( 'NONE', #26776, .T. ) ;
#36972 = AXIS2_PLACEMENT_3D ( 'NONE', #1234, #14792, #27987 ) ;
#36973 = VERTEX_POINT ( 'NONE', #12002 ) ;
#36975 = ORIENTED_EDGE ( 'NONE', *, *, #41196, .T. ) ;
#36974 = CARTESIAN_POINT ( 'NONE',  ( 7.644554776091147741E-16, 12.48450537969573659, -59.65625000204838813 ) ) ;
#36976 = DATE_AND_TIME ( #17319, #15201 ) ;
#36978 = EDGE_LOOP ( 'NONE', ( #39264, #41213, #11045, #11964 ) ) ;
#36977 = CARTESIAN_POINT ( 'NONE',  ( 5.405949406249999534, 9.363379034771803333, -110.5937500020483810 ) ) ;
#36979 = CARTESIAN_POINT ( 'NONE',  ( 10.81189881249999729, 6.242252689847867408, -25.21875000204837036 ) ) ;
#36980 =( BOUNDED_CURVE ( )  B_SPLINE_CURVE ( 2, ( #38566, #2546, #28873, #24792, #28455, #34926, #42007 ),
 .UNSPECIFIED., .F., .F. ) 
 B_SPLINE_CURVE_WITH_KNOTS ( ( 3, 2, 2, 3 ),
 ( 0.8022388059701494045, 0.8034825870646766788, 0.8047263681592041751, 0.8059701492537315604 ),
 .UNSPECIFIED. ) 
 CURVE ( )  GEOMETRIC_REPRESENTATION_ITEM ( )  RATIONAL_B_SPLINE_CURVE ( ( 0.9999999999999880096, 0.8660254037844506980, 1.000000000000000000, 0.8660254037844387076, 1.000000000000000000, 0.8660254037844148378, 1.000000000000023981 ) ) 
 REPRESENTATION_ITEM ( '' )  );
#36981 = CARTESIAN_POINT ( 'NONE',  ( 5.405949406249992428, -9.363379034771808662, -189.0937500020483810 ) ) ;
#36982 = CARTESIAN_POINT ( 'NONE',  ( -10.81189881249999729, 6.242252689847871849, -36.71875000204835970 ) ) ;
#36983 = CARTESIAN_POINT ( 'NONE',  ( -8.461552159095841574, -5.381368393490791213, 7.703719777548943412E-31 ) ) ;
#36984 = CARTESIAN_POINT ( 'NONE',  ( 9.999999999999998224, 0.000000000000000000, -152.3750000040967905 ) ) ;
#36985 = CARTESIAN_POINT ( 'NONE',  ( 5.405949406249999534, 9.363379034771803333, -179.5937500020484094 ) ) ;
#36986 = CARTESIAN_POINT ( 'NONE',  ( -5.405949406250003975, -9.363379034771801557, -160.8437500020484094 ) ) ;
#36987 = CARTESIAN_POINT ( 'NONE',  ( -10.81189881249999729, 1.324075727343319199E-15, -138.5937500020483810 ) ) ;
#36988 = CARTESIAN_POINT ( 'NONE',  ( 10.81189881249999729, 6.242252689847867408, -158.7187500020484094 ) ) ;
#36989 = CARTESIAN_POINT ( 'NONE',  ( -5.000000000000003553, -8.660254037844383745, -42.99999999999998579 ) ) ;
#36990 =( BOUNDED_CURVE ( )  B_SPLINE_CURVE ( 2, ( #5045, #18190, #14294, #11069, #31382, #7639, #24911 ),
 .UNSPECIFIED., .F., .F. ) 
 B_SPLINE_CURVE_WITH_KNOTS ( ( 3, 2, 2, 3 ),
 ( 0.6082089552238807428, 0.6094527363184080171, 0.6106965174129354024, 0.6119402985074627876 ),
 .UNSPECIFIED. ) 
 CURVE ( )  GEOMETRIC_REPRESENTATION_ITEM ( )  RATIONAL_B_SPLINE_CURVE ( ( 0.9999999999999880096, 0.8660254037844506980, 1.000000000000000000, 0.8660254037844387076, 1.000000000000000000, 0.8660254037844267172, 1.000000000000011990 ) ) 
 REPRESENTATION_ITEM ( '' )  );
#36991 = CARTESIAN_POINT ( 'NONE',  ( -9.999999999999998224, 1.224646799147353059E-15, -187.6250000040967905 ) ) ;
#36992 = CARTESIAN_POINT ( 'NONE',  ( 10.00000000000000000, 5.773502691896255534, -180.3750000000000284 ) ) ;
#36993 = CARTESIAN_POINT ( 'NONE',  ( 10.81189881249999551, -6.242252689847874514, -92.96875000204838102 ) ) ;
#36994 = CARTESIAN_POINT ( 'NONE',  ( -9.999999999999998224, 1.224646799147353059E-15, -200.0000000000000000 ) ) ;
#36995 = CARTESIAN_POINT ( 'NONE',  ( -10.81189881249999729, 1.324075727343319199E-15, -65.28125000204838102 ) ) ;
#36996 = CARTESIAN_POINT ( 'NONE',  ( -9.999999999999998224, 1.224646799147353059E-15, -124.6250000040967763 ) ) ;
#36997 = CARTESIAN_POINT ( 'NONE',  ( -2.293366432827344421E-15, -12.48450537969573659, -180.2187500020484094 ) ) ;
#36998 = CARTESIAN_POINT ( 'NONE',  ( -10.81189881249999729, 1.324075727343319199E-15, -122.2812500020483952 ) ) ;
#36999 = CARTESIAN_POINT ( 'NONE',  ( 10.81189881249999729, 6.242252689847867408, -164.9062500020484094 ) ) ;
#37000 = CARTESIAN_POINT ( 'NONE',  ( 10.81189881249999907, 6.242252689847868297, -49.40625000204837391 ) ) ;
#37001 = CARTESIAN_POINT ( 'NONE',  ( -10.00000000000000000, -5.773502691896251982, -127.5000000040967905 ) ) ;
#37002 = CARTESIAN_POINT ( 'NONE',  ( 10.00000000000000000, 5.773502691896255534, -111.3749999999999858 ) ) ;
#37003 = ORIENTED_EDGE ( 'NONE', *, *, #27372, .T. ) ;
#37004 = CARTESIAN_POINT ( 'NONE',  ( -10.81189881249999729, -6.242252689847864744, -132.6562500020483810 ) ) ;
#37005 = CARTESIAN_POINT ( 'NONE',  ( 9.999999999999996447, -5.773502691896262640, -155.5000000040968189 ) ) ;
#37006 = CARTESIAN_POINT ( 'NONE',  ( 7.644554776091147741E-16, 12.48450537969573659, -151.1562500020484094 ) ) ;
#37007 = CARTESIAN_POINT ( 'NONE',  ( -5.405949406249996869, 9.363379034771805109, -185.5312500020484094 ) ) ;
#37008 = CARTESIAN_POINT ( 'NONE',  ( 10.81189881249999907, 6.242252689847868297, -85.21875000204836681 ) ) ;
#37009 = ORIENTED_EDGE ( 'NONE', *, *, #7325, .F. ) ;
#37010 = CARTESIAN_POINT ( 'NONE',  ( -4.999999999999996447, 8.660254037844387298, -47.99999999999998579 ) ) ;
#37011 = CARTESIAN_POINT ( 'NONE',  ( 10.81189881249999729, 0.000000000000000000, -181.3437500020483810 ) ) ;
#37012 = CARTESIAN_POINT ( 'NONE',  ( 9.999999999999998224, 0.000000000000000000, -68.37500000409677625 ) ) ;
#37013 = CARTESIAN_POINT ( 'NONE',  ( -9.999999999999998224, 1.224646799147353059E-15, -179.7500000000000284 ) ) ;
#37014 = CARTESIAN_POINT ( 'NONE',  ( -9.999999999999998224, 1.224646799147353059E-15, -133.2499999999999716 ) ) ;
#37015 = CARTESIAN_POINT ( 'NONE',  ( 10.81189881249999907, 6.242252689847868297, -77.90625000204836681 ) ) ;
#37016 = CARTESIAN_POINT ( 'NONE',  ( 10.81189881249999729, 0.000000000000000000, -63.03125000204837391 ) ) ;
#37017 = CARTESIAN_POINT ( 'NONE',  ( -9.999999999999998224, 1.224646799147353059E-15, -52.62500000409675494 ) ) ;
#37018 = CARTESIAN_POINT ( 'NONE',  ( 5.405949406249999534, 9.363379034771803333, -7.093750002048371250 ) ) ;
#37019 = CARTESIAN_POINT ( 'NONE',  ( 9.999999999999998224, 0.000000000000000000, -158.3750000040967905 ) ) ;
#37020 = CARTESIAN_POINT ( 'NONE',  ( 10.81189881249999729, 0.000000000000000000, -174.0312500020484094 ) ) ;
#37021 = CARTESIAN_POINT ( 'NONE',  ( 10.81189881249999907, 6.242252689847868297, -4.406250002048361480 ) ) ;
#37022 = DIRECTION ( 'NONE',  ( -0.000000000000000000, -0.000000000000000000, 1.000000000000000000 ) ) ;
#37024 = EDGE_CURVE ( 'NONE', #38572, #5967, #5541, .T. ) ;
#37023 = CARTESIAN_POINT ( 'NONE',  ( -9.999999999999998224, 1.224646799147353059E-15, -161.7500000000000000 ) ) ;
#37025 = CARTESIAN_POINT ( 'NONE',  ( -9.999999999999479527, -5.773502691896549521, -89.62499999999997158 ) ) ;
#37026 = FACE_OUTER_BOUND ( 'NONE', #2967, .T. ) ;
#37027 = ADVANCED_FACE ( 'NONE', ( #29265 ), #36371, .T. ) ;
#37028 = LINE ( 'NONE', #14118, #14453 ) ;
#37029 = ADVANCED_FACE ( 'NONE', ( #35541 ), #1062, .F. ) ;
#37031 = EDGE_LOOP ( 'NONE', ( #27163, #2699, #37177, #41649 ) ) ;
#37030 = CARTESIAN_POINT ( 'NONE',  ( 10.81189881249999729, 0.000000000000000000, -82.53125000204838102 ) ) ;
#37033 = ORIENTED_EDGE ( 'NONE', *, *, #15152, .T. ) ;
#37032 = LINE ( 'NONE', #21266, #11637 ) ;
#37034 = APPROVAL ( #15942, 'UNSPECIFIED' ) ;
#37035 = ORIENTED_EDGE ( 'NONE', *, *, #25204, .T. ) ;
#37036 = CARTESIAN_POINT ( 'NONE',  ( 10.81189881249999907, 6.242252689847868297, -23.71875000204836326 ) ) ;
#37037 = CARTESIAN_POINT ( 'NONE',  ( 10.81189881249999907, 6.242252689847868297, -10.40625000204838102 ) ) ;
#37038 = CARTESIAN_POINT ( 'NONE',  ( 5.405949406249992428, -9.363379034771808662, -67.59375000204836681 ) ) ;
#37039 = CARTESIAN_POINT ( 'NONE',  ( -9.999999999999998224, 1.224646799147353059E-15, -122.7500000000000000 ) ) ;
#37040 = CARTESIAN_POINT ( 'NONE',  ( 9.999999999999996447, -5.773502691896262640, -45.62499999999996447 ) ) ;
#37041 = CARTESIAN_POINT ( 'NONE',  ( 10.81189881249999907, 6.242252689847868297, -184.2187500020483810 ) ) ;
#37042 = CARTESIAN_POINT ( 'NONE',  ( -5.405949406250003975, -9.363379034771801557, -165.3437500020484094 ) ) ;
#37043 = CARTESIAN_POINT ( 'NONE',  ( -5.405949406249996869, 9.363379034771805109, -0.8437500020483656993 ) ) ;
#37044 = CARTESIAN_POINT ( 'NONE',  ( -10.00000000000154188, 5.773502691895366468, -58.75000000409671941 ) ) ;
#37045 = CARTESIAN_POINT ( 'NONE',  ( 7.070501591499376803E-16, 11.54700538379251284, -147.1250000000000000 ) ) ;
#37046 = CARTESIAN_POINT ( 'NONE',  ( -4.999999999999996447, 8.660254037844387298, -126.0000000000000000 ) ) ;
#37047 = EDGE_CURVE ( 'NONE', #25274, #18020, #3239, .T. ) ;
#37048 = CARTESIAN_POINT ( 'NONE',  ( -10.81189881249999729, 6.242252689847871849, -111.7187500020483810 ) ) ;
#37049 = CARTESIAN_POINT ( 'NONE',  ( 9.999999999999998224, 0.000000000000000000, -161.3750000040967905 ) ) ;
#37050 = CARTESIAN_POINT ( 'NONE',  ( -10.81189881249999729, 1.324075727343319199E-15, -93.78125000204838102 ) ) ;
#37051 = CARTESIAN_POINT ( 'NONE',  ( 7.644554776091147741E-16, 12.48450537969573659, -102.9687500020483668 ) ) ;
#37052 = CARTESIAN_POINT ( 'NONE',  ( 10.81189881249999551, -6.242252689847874514, -65.96875000204838102 ) ) ;
#37053 = CARTESIAN_POINT ( 'NONE',  ( 5.405949406249999534, 9.363379034771803333, -76.28125000204838102 ) ) ;
#37054 = CARTESIAN_POINT ( 'NONE',  ( -9.999999999999998224, 1.224646799147353059E-15, -159.1250000040967905 ) ) ;
#37055 = CARTESIAN_POINT ( 'NONE',  ( 10.81189881249999729, 6.242252689847867408, -157.4062500020483810 ) ) ;
#37056 = CARTESIAN_POINT ( 'NONE',  ( -10.81189881249999729, 6.242252689847871849, -168.9062500020483810 ) ) ;
#37057 = CARTESIAN_POINT ( 'NONE',  ( 9.999999999999998224, 0.000000000000000000, -144.8750000040967905 ) ) ;
#37058 = CARTESIAN_POINT ( 'NONE',  ( -5.405949406250003975, -9.363379034771801557, -102.3437500020483810 ) ) ;
#37059 = CARTESIAN_POINT ( 'NONE',  ( 0.000000000000000000, 0.000000000000000000, -200.0000000000000000 ) ) ;
#37060 = CARTESIAN_POINT ( 'NONE',  ( -9.999999999999998224, 5.773502691896259087, -71.87500000000000000 ) ) ;
#37061 = CARTESIAN_POINT ( 'NONE',  ( -10.81189881249999729, 1.324075727343319199E-15, -5.281250002048376579 ) ) ;
#37062 = CARTESIAN_POINT ( 'NONE',  ( 9.999999999999996447, -5.773502691896262640, -91.00000000409677625 ) ) ;
#37063 =( BOUNDED_CURVE ( )  B_SPLINE_CURVE ( 2, ( #17887, #10778, #36692, #31085, #40546, #1085, #7985 ),
 .UNSPECIFIED., .F., .F. ) 
 B_SPLINE_CURVE_WITH_KNOTS ( ( 3, 2, 2, 3 ),
 ( 0.8544776119402988090, 0.8557213930348261943, 0.8569651741293534686, 0.8582089552238808539 ),
 .UNSPECIFIED. ) 
 CURVE ( )  GEOMETRIC_REPRESENTATION_ITEM ( )  RATIONAL_B_SPLINE_CURVE ( ( 0.9999999999999641398, 0.8660254037844745678, 1.000000000000000000, 0.8660254037844387076, 1.000000000000000000, 0.8660254037844148378, 1.000000000000023981 ) ) 
 REPRESENTATION_ITEM ( '' )  );
#37064 = CARTESIAN_POINT ( 'NONE',  ( 5.405949406249992428, -9.363379034771808662, -100.7812500020483952 ) ) ;
#37065 = CARTESIAN_POINT ( 'NONE',  ( 10.81189881249999729, 0.000000000000000000, -82.53125000204838102 ) ) ;
#37066 = CARTESIAN_POINT ( 'NONE',  ( -2.121150477449813534E-15, -11.54700538379251284, -74.75000000409677625 ) ) ;
#37067 = CARTESIAN_POINT ( 'NONE',  ( 9.999999999998969713, 5.773502691896851502, -19.87499999999994316 ) ) ;
#37068 = CARTESIAN_POINT ( 'NONE',  ( -10.81189881249999729, 6.242252689847871849, -36.71875000204835260 ) ) ;
#37069 = VERTEX_POINT ( 'NONE', #20630 ) ;
#37070 = CARTESIAN_POINT ( 'NONE',  ( 5.000000000000000000, 8.660254037844385522, -0.2499999999999724665 ) ) ;
#37071 = CARTESIAN_POINT ( 'NONE',  ( -5.405949406249996869, 9.363379034771805109, -29.53125000204837036 ) ) ;
#37072 = CARTESIAN_POINT ( 'NONE',  ( -10.81189881249999729, 1.324075727343319199E-15, -14.09375000204834905 ) ) ;
#37073 = CARTESIAN_POINT ( 'NONE',  ( 9.999999999999998224, 0.000000000000000000, -14.37500000409674961 ) ) ;
#37074 = CARTESIAN_POINT ( 'NONE',  ( -9.999999999999998224, 5.773502691896259087, -3.250000004096753603 ) ) ;
#37075 = CARTESIAN_POINT ( 'NONE',  ( -10.81189881249999729, 1.324075727343319199E-15, -135.7812500020483810 ) ) ;
#37076 = CARTESIAN_POINT ( 'NONE',  ( -2.121150477449813534E-15, -11.54700538379251284, -186.8750000000000284 ) ) ;
#37078 = VERTEX_POINT ( 'NONE', #12708 ) ;
#37077 = CARTESIAN_POINT ( 'NONE',  ( -10.81189881249999729, 6.242252689847871849, -110.4062500020483810 ) ) ;
#37079 = DIRECTION ( 'NONE',  ( -0.000000000000000000, -0.000000000000000000, 1.000000000000000000 ) ) ;
#37080 = VECTOR ( 'NONE', #3495, 1000.000000000000000 ) ;
#37081 = ORIENTED_EDGE ( 'NONE', *, *, #4042, .T. ) ;
#37082 = EDGE_LOOP ( 'NONE', ( #33009, #35827, #8447, #23002 ) ) ;
#37083 = CARTESIAN_POINT ( 'NONE',  ( 7.644554776091147741E-16, 12.48450537969573659, -44.65625000204836681 ) ) ;
#37084 = APPROVAL_DATE_TIME ( #16789, #21199 ) ;
#37085 = EDGE_CURVE ( 'NONE', #16098, #17857, #16365, .T. ) ;
#37086 = CARTESIAN_POINT ( 'NONE',  ( 10.81189881249999907, 6.242252689847868297, -97.21875000204836681 ) ) ;
#37087 = PLANE ( 'NONE',  #36018 ) ;
#37088 = CARTESIAN_POINT ( 'NONE',  ( 10.00000000000012790, 5.773502691896179151, -174.3750000000000000 ) ) ;
#37089 = CARTESIAN_POINT ( 'NONE',  ( 10.81189881249999551, -6.242252689847874514, -194.9687500020484094 ) ) ;
#37090 = CARTESIAN_POINT ( 'NONE',  ( 10.81189881249999907, 6.242252689847868297, -170.9062500020484094 ) ) ;
#37091 = DIRECTION ( 'NONE',  ( -0.000000000000000000, -0.000000000000000000, 1.000000000000000000 ) ) ;
#37092 = CARTESIAN_POINT ( 'NONE',  ( 7.644554776091147741E-16, 12.48450537969573659, -123.9687500020483952 ) ) ;
#37093 = CARTESIAN_POINT ( 'NONE',  ( 10.81189881249999729, 0.000000000000000000, -91.34375000204838102 ) ) ;
#37094 = CARTESIAN_POINT ( 'NONE',  ( -9.999999999998969713, -5.773502691896847949, -44.62499999999995737 ) ) ;
#37095 = CARTESIAN_POINT ( 'NONE',  ( 7.644554776091147741E-16, 12.48450537969573659, -103.1562500020483952 ) ) ;
#37096 = CARTESIAN_POINT ( 'NONE',  ( -2.121150477449813534E-15, -11.54700538379251284, -185.7500000040967905 ) ) ;
#37097 = CARTESIAN_POINT ( 'NONE',  ( -10.81189881249999729, -6.242252689847864744, -108.4687500020483810 ) ) ;
#37098 = CARTESIAN_POINT ( 'NONE',  ( 7.644554776091147741E-16, 12.48450537969573659, -176.6562500020484094 ) ) ;
#37099 =( BOUNDED_CURVE ( )  B_SPLINE_CURVE ( 2, ( #10142, #27405, #244, #14206, #33260, #10985, #20491 ),
 .UNSPECIFIED., .F., .F. ) 
 B_SPLINE_CURVE_WITH_KNOTS ( ( 3, 2, 2, 3 ),
 ( 0.3694029850746269883, 0.3706467661691543181, 0.3718905472636816478, 0.3731343283582090331 ),
 .UNSPECIFIED. ) 
 CURVE ( )  GEOMETRIC_REPRESENTATION_ITEM ( )  RATIONAL_B_SPLINE_CURVE ( ( 0.9999999999999880096, 0.8660254037844506980, 1.000000000000000000, 0.8660254037844387076, 1.000000000000000000, 0.8660254037844327124, 1.000000000000005995 ) ) 
 REPRESENTATION_ITEM ( '' )  );
#37100 = CARTESIAN_POINT ( 'NONE',  ( -9.999999999999998224, 1.224646799147353059E-15, -200.0000000000000000 ) ) ;
#37101 = CARTESIAN_POINT ( 'NONE',  ( -5.405949406250003975, -9.363379034771801557, -198.5312500020484094 ) ) ;
#37102 = CARTESIAN_POINT ( 'NONE',  ( 5.405949406249992428, -9.363379034771808662, -52.59375000204835260 ) ) ;
#37103 = CARTESIAN_POINT ( 'NONE',  ( 7.644554776091147741E-16, 12.48450537969573659, -41.46875000204835260 ) ) ;
#37104 = CARTESIAN_POINT ( 'NONE',  ( -5.000000000000003553, -8.660254037844383745, -170.8750000040968189 ) ) ;
#37105 = CARTESIAN_POINT ( 'NONE',  ( -5.405949406250003975, -9.363379034771801557, -11.03125000204835438 ) ) ;
#37106 = CARTESIAN_POINT ( 'NONE',  ( 5.405949406249992428, -9.363379034771808662, -18.09375000204835260 ) ) ;
#37107 = CARTESIAN_POINT ( 'NONE',  ( 0.000000000000000000, 0.000000000000000000, -99.99999999999998579 ) ) ;
#37108 = CARTESIAN_POINT ( 'NONE',  ( -2.293366432827344421E-15, -12.48450537969573659, -129.2187500020483810 ) ) ;
#37109 = CARTESIAN_POINT ( 'NONE',  ( -10.00000000000000000, -5.773502691896251982, -94.12499999999998579 ) ) ;
#37110 = CARTESIAN_POINT ( 'NONE',  ( 10.81189881249999551, -6.242252689847874514, -28.65625000204838102 ) ) ;
#37111 = VECTOR ( 'NONE', #30270, 1000.000000000000000 ) ;
#37112 = CARTESIAN_POINT ( 'NONE',  ( 4.999999999999992006, -8.660254037844389075, -49.12500000409678336 ) ) ;
#37113 = CARTESIAN_POINT ( 'NONE',  ( -2.121150477449813534E-15, -11.54700538379251284, -60.87499999999998579 ) ) ;
#37114 = CARTESIAN_POINT ( 'NONE',  ( 5.405949406249999534, 9.363379034771803333, -125.7812500020483668 ) ) ;
#37115 = CARTESIAN_POINT ( 'NONE',  ( -5.405949406249996869, 9.363379034771805109, -104.5312500020483810 ) ) ;
#37116 = VERTEX_POINT ( 'NONE', #17385 ) ;
#37117 = DIRECTION ( 'NONE',  ( -0.000000000000000000, -0.000000000000000000, 1.000000000000000000 ) ) ;
#37118 = CARTESIAN_POINT ( 'NONE',  ( -9.999999999999998224, 1.224646799147353059E-15, -97.62500000409677625 ) ) ;
#37119 = CARTESIAN_POINT ( 'NONE',  ( 9.999999999999998224, 0.000000000000000000, -75.87500000409677625 ) ) ;
#37120 = CARTESIAN_POINT ( 'NONE',  ( -5.405949406250003975, -9.363379034771801557, -61.84375000204836681 ) ) ;
#37121 = ORIENTED_EDGE ( 'NONE', *, *, #19564, .F. ) ;
#37122 = CARTESIAN_POINT ( 'NONE',  ( -10.00000000000000000, -5.773502691896251982, -34.12499999999997158 ) ) ;
#37123 = CARTESIAN_POINT ( 'NONE',  ( 10.81189881249999729, 6.242252689847867408, -38.90625000204835970 ) ) ;
#37124 = CARTESIAN_POINT ( 'NONE',  ( 9.999999999999479527, 5.773502691896553074, -35.25000000409674072 ) ) ;
#37125 = CARTESIAN_POINT ( 'NONE',  ( -10.00000000000000000, -5.773502691896251982, -28.50000000409674783 ) ) ;
#37126 = CARTESIAN_POINT ( 'NONE',  ( 10.81189881249999907, 6.242252689847868297, -131.9062500020484094 ) ) ;
#37127 = CARTESIAN_POINT ( 'NONE',  ( 9.999999999999998224, 0.000000000000000000, -146.3750000040967905 ) ) ;
#37128 = ORIENTED_EDGE ( 'NONE', *, *, #17476, .F. ) ;
#37130 = ORIENTED_EDGE ( 'NONE', *, *, #7454, .F. ) ;
#37129 = EDGE_LOOP ( 'NONE', ( #28464, #2679, #31968, #17162 ) ) ;
#37131 = AXIS2_PLACEMENT_3D ( 'NONE', #33470, #17031, #670 ) ;
#37132 = DIRECTION ( 'NONE',  ( -0.000000000000000000, -0.000000000000000000, -1.000000000000000000 ) ) ;
#37133 = CYLINDRICAL_SURFACE ( 'NONE', #24243, 9.999999999999998224 ) ;
#37134 = CARTESIAN_POINT ( 'NONE',  ( 10.81189881249999907, 6.242252689847868297, -166.2187500020484094 ) ) ;
#37135 = CARTESIAN_POINT ( 'NONE',  ( 10.81189881249999729, 0.000000000000000000, -196.5312500020484094 ) ) ;
#37136 = CARTESIAN_POINT ( 'NONE',  ( 5.405949406249992428, -9.363379034771808662, -13.59375000204834905 ) ) ;
#37137 = CARTESIAN_POINT ( 'NONE',  ( 4.999999999999992006, -8.660254037844389075, -157.1250000040967905 ) ) ;
#37138 = CARTESIAN_POINT ( 'NONE',  ( -5.405949406250003975, -9.363379034771801557, -150.3437500020483810 ) ) ;
#37139 = CARTESIAN_POINT ( 'NONE',  ( -10.81189881249999907, -6.242252689847864744, -136.9687500020483810 ) ) ;
#37140 = CARTESIAN_POINT ( 'NONE',  ( 10.81189881249999907, 6.242252689847868297, -104.9062500020483952 ) ) ;
#37141 = CARTESIAN_POINT ( 'NONE',  ( 7.644554776091147741E-16, 12.48450537969573659, -120.9687500020483952 ) ) ;
#37142 = CARTESIAN_POINT ( 'NONE',  ( -9.999999999999998224, 5.773502691896259087, -196.7500000040968189 ) ) ;
#37143 = CARTESIAN_POINT ( 'NONE',  ( 5.405949406249999534, 9.363379034771803333, -121.2812500020483952 ) ) ;
#37144 = CARTESIAN_POINT ( 'NONE',  ( 7.644554776091147741E-16, 12.48450537969573659, -11.46875000204836859 ) ) ;
#37146 = EDGE_CURVE ( 'NONE', #19338, #14871, #32218, .T. ) ;
#37145 = CARTESIAN_POINT ( 'NONE',  ( -10.81189881249999729, 1.324075727343319199E-15, -131.0937500020483810 ) ) ;
#37147 = CARTESIAN_POINT ( 'NONE',  ( 9.999999999999998224, 0.000000000000000000, -164.0000000000000000 ) ) ;
#37148 = VECTOR ( 'NONE', #21393, 1000.000000000000000 ) ;
#37149 = CARTESIAN_POINT ( 'NONE',  ( 9.999999999999998224, 0.000000000000000000, -179.3750000040967905 ) ) ;
#37150 = CARTESIAN_POINT ( 'NONE',  ( -9.999999999999998224, 1.224646799147353059E-15, -157.2500000000000000 ) ) ;
#37151 = CARTESIAN_POINT ( 'NONE',  ( 7.070501591499377789E-16, 11.54700538379251284, -18.12499999999997513 ) ) ;
#37152 = CARTESIAN_POINT ( 'NONE',  ( 7.644554776091147741E-16, 12.48450537969573659, -72.96875000204836681 ) ) ;
#37153 = CARTESIAN_POINT ( 'NONE',  ( -10.81189881249999729, 1.324075727343319199E-15, -65.09375000204836681 ) ) ;
#37154 = CARTESIAN_POINT ( 'NONE',  ( -5.405949406249996869, 9.363379034771805109, -34.03125000204837391 ) ) ;
#37155 = CARTESIAN_POINT ( 'NONE',  ( -10.81189881249999907, -6.242252689847864744, -42.46875000204835970 ) ) ;
#37156 = CARTESIAN_POINT ( 'NONE',  ( 10.00000000000025402, -5.773502691896113426, -139.0000000040967905 ) ) ;
#37157 = CARTESIAN_POINT ( 'NONE',  ( 5.405949406249992428, -9.363379034771808662, -151.5937500020483810 ) ) ;
#37158 = CARTESIAN_POINT ( 'NONE',  ( -5.000000000000003553, -8.660254037844383745, -127.0000000000000000 ) ) ;
#37159 = CARTESIAN_POINT ( 'NONE',  ( 10.81189881249999729, 0.000000000000000000, -133.5312500020484094 ) ) ;
#37160 = CARTESIAN_POINT ( 'NONE',  ( -10.00000000000051337, 5.773502691895962435, -94.37499999999997158 ) ) ;
#37161 = CARTESIAN_POINT ( 'NONE',  ( -5.000000000000003553, -8.660254037844383745, -80.49999999999998579 ) ) ;
#37162 = CARTESIAN_POINT ( 'NONE',  ( 5.405949406249999534, 9.363379034771803333, -16.28125000204835970 ) ) ;
#37163 = ORIENTED_EDGE ( 'NONE', *, *, #3272, .T. ) ;
#37164 = CARTESIAN_POINT ( 'NONE',  ( 10.81189881249999729, 0.000000000000000000, -108.0312500020483810 ) ) ;
#37165 = CARTESIAN_POINT ( 'NONE',  ( -5.000000000000003553, -8.660254037844383745, -127.3750000040967905 ) ) ;
#37166 = FACE_OUTER_BOUND ( 'NONE', #35512, .T. ) ;
#37167 = CARTESIAN_POINT ( 'NONE',  ( -10.00000000000000000, -5.773502691896251982, -31.50000000409674783 ) ) ;
#37168 = CYLINDRICAL_SURFACE ( 'NONE', #4216, 9.999999999999998224 ) ;
#37169 = CARTESIAN_POINT ( 'NONE',  ( 7.644554776091147741E-16, 12.48450537969573659, -53.65625000204838102 ) ) ;
#37170 = CARTESIAN_POINT ( 'NONE',  ( -4.999999999999996447, 8.660254037844387298, -76.49999999999998579 ) ) ;
#37171 = CARTESIAN_POINT ( 'NONE',  ( -5.405949406249996869, 9.363379034771805109, -149.5312500020483810 ) ) ;
#37172 = AXIS2_PLACEMENT_3D ( 'NONE', #27323, #7902, #37674 ) ;
#37173 = CARTESIAN_POINT ( 'NONE',  ( -10.81189881249999907, -6.242252689847864744, -136.9687500020483810 ) ) ;
#37174 = CARTESIAN_POINT ( 'NONE',  ( 9.999999999999998224, 0.000000000000000000, -120.8750000040967905 ) ) ;
#37175 = ORIENTED_EDGE ( 'NONE', *, *, #10650, .F. ) ;
#37176 = CARTESIAN_POINT ( 'NONE',  ( -10.00000000000012434, 5.773502691896184480, -163.7500000040967905 ) ) ;
#37177 = ORIENTED_EDGE ( 'NONE', *, *, #17957, .F. ) ;
#37178 = VECTOR ( 'NONE', #16439, 1000.000000000000000 ) ;
#37179 = ORIENTED_EDGE ( 'NONE', *, *, #33285, .F. ) ;
#37181 = ORIENTED_EDGE ( 'NONE', *, *, #13936, .T. ) ;
#37180 = CARTESIAN_POINT ( 'NONE',  ( 10.81189881249999729, 0.000000000000000000, -109.3437500020483810 ) ) ;
#37182 =( BOUNDED_CURVE ( )  B_SPLINE_CURVE ( 2, ( #37615, #20560, #13858, #14718, #24038, #21420, #27692 ),
 .UNSPECIFIED., .F., .F. ) 
 B_SPLINE_CURVE_WITH_KNOTS ( ( 3, 2, 2, 3 ),
 ( 0.1119402985074627876, 0.1131840796019901035, 0.1144278606965174333, 0.1156716417910447492 ),
 .UNSPECIFIED. ) 
 CURVE ( )  GEOMETRIC_REPRESENTATION_ITEM ( )  RATIONAL_B_SPLINE_CURVE ( ( 0.9999999999999894529, 0.8660254037844491437, 1.000000000000000000, 0.8660254037844387076, 1.000000000000000000, 0.8660254037844417052, 0.9999999999999970024 ) ) 
 REPRESENTATION_ITEM ( '' )  );
#37183 = CARTESIAN_POINT ( 'NONE',  ( 5.000000000000000000, 8.660254037844385522, -129.6250000040967620 ) ) ;
#37184 = CARTESIAN_POINT ( 'NONE',  ( 10.81189881249999907, 6.242252689847868297, -190.2187500020484094 ) ) ;
#37185 = CARTESIAN_POINT ( 'NONE',  ( 10.81189881249999729, 0.000000000000000000, -38.84375000204837391 ) ) ;
#37186 = CARTESIAN_POINT ( 'NONE',  ( -0.8693057687019801749, -10.36909276259400237, -5.090678961559013491E-15 ) ) ;
#37187 = DIRECTION ( 'NONE',  ( 1.000000000000000000, 0.000000000000000000, 0.000000000000000000 ) ) ;
#37188 = CARTESIAN_POINT ( 'NONE',  ( 10.81189881249999729, 0.000000000000000000, -170.8437500020484094 ) ) ;
#37189 = CARTESIAN_POINT ( 'NONE',  ( -5.405949406249996869, 9.363379034771805109, -158.3437500020483810 ) ) ;
#37190 = CARTESIAN_POINT ( 'NONE',  ( -9.999999999999998224, 1.224646799147353059E-15, -66.12500000409676204 ) ) ;
#37191 = CARTESIAN_POINT ( 'NONE',  ( 5.405949406249999534, 9.363379034771803333, -140.5937500020483810 ) ) ;
#37192 = CARTESIAN_POINT ( 'NONE',  ( -5.405949406249996869, 9.363379034771805109, -156.8437500020483810 ) ) ;
#37193 = CARTESIAN_POINT ( 'NONE',  ( 4.999999999999992006, -8.660254037844389075, -155.2500000000000000 ) ) ;
#37194 = CARTESIAN_POINT ( 'NONE',  ( -9.999999999999998224, 1.224646799147353059E-15, -139.6250000040967905 ) ) ;
#37195 = CARTESIAN_POINT ( 'NONE',  ( -9.999999999999998224, 5.773502691896259087, -182.8750000000000000 ) ) ;
#37196 = VECTOR ( 'NONE', #4702, 1000.000000000000000 ) ;
#37197 = CARTESIAN_POINT ( 'NONE',  ( -10.81189881249999907, -6.242252689847864744, -85.96875000204836681 ) ) ;
#37198 = CARTESIAN_POINT ( 'NONE',  ( -4.208742559982952436, 9.984557306008309041, -99.99999999999995737 ) ) ;
#37199 = CARTESIAN_POINT ( 'NONE',  ( -10.81189881249999907, -6.242252689847864744, -57.65625000204838102 ) ) ;
#37200 = CARTESIAN_POINT ( 'NONE',  ( 9.999999999998969713, 5.773502691896851502, -87.75000000409674783 ) ) ;
#37201 = EDGE_CURVE ( 'NONE', #22477, #34879, #7269, .T. ) ;
#37202 = CARTESIAN_POINT ( 'NONE',  ( -10.81189881249999729, 6.242252689847871849, -179.2187500020483810 ) ) ;
#37203 = CARTESIAN_POINT ( 'NONE',  ( -10.81189881249999907, -6.242252689847864744, -125.1562500020483810 ) ) ;
#37204 = CARTESIAN_POINT ( 'NONE',  ( 5.405949406249999534, 9.363379034771803333, -152.7812500020484094 ) ) ;
#37205 = CARTESIAN_POINT ( 'NONE',  ( 0.000000000000000000, 0.000000000000000000, -200.0000000000000000 ) ) ;
#37206 = CARTESIAN_POINT ( 'NONE',  ( 5.405949406249999534, 9.363379034771803333, -52.28125000204835970 ) ) ;
#37207 = CARTESIAN_POINT ( 'NONE',  ( -10.00000000000000000, -5.773502691896251982, -129.0000000040967905 ) ) ;
#37208 = CARTESIAN_POINT ( 'NONE',  ( -2.121150477449813534E-15, -11.54700538379251284, -104.3749999999999716 ) ) ;
#37209 = VERTEX_POINT ( 'NONE', #804 ) ;
#37210 = CARTESIAN_POINT ( 'NONE',  ( -5.405949406249996869, 9.363379034771805109, -136.0312500020484094 ) ) ;
#37211 = CARTESIAN_POINT ( 'NONE',  ( -10.00000000000000000, -5.773502691896251982, -145.5000000040967905 ) ) ;
#37212 = CARTESIAN_POINT ( 'NONE',  ( 7.644554776091147741E-16, 12.48450537969573659, -146.6562500020484379 ) ) ;
#37213 = CARTESIAN_POINT ( 'NONE',  ( 5.405949406249992428, -9.363379034771808662, -192.2812500020484094 ) ) ;
#37214 = VERTEX_POINT ( 'NONE', #33610 ) ;
#37215 = CARTESIAN_POINT ( 'NONE',  ( 9.999999999999998224, 0.000000000000000000, -52.99999999999996447 ) ) ;
#37216 = CARTESIAN_POINT ( 'NONE',  ( 10.81189881249999551, -6.242252689847874514, -184.4687500020483810 ) ) ;
#37217 = CARTESIAN_POINT ( 'NONE',  ( -5.000000000000003553, -8.660254037844383745, -61.37500000409676204 ) ) ;
#37218 = CARTESIAN_POINT ( 'NONE',  ( 5.000000000000000000, 8.660254037844385522, -153.2500000000000000 ) ) ;
#37219 = CARTESIAN_POINT ( 'NONE',  ( 9.999999999999998224, 0.000000000000000000, -200.0000000000000000 ) ) ;
#37220 = CARTESIAN_POINT ( 'NONE',  ( -10.81189881249999907, -6.242252689847864744, -78.65625000204839523 ) ) ;
#37221 = CARTESIAN_POINT ( 'NONE',  ( -5.405949406249996869, 9.363379034771805109, -49.03125000204838813 ) ) ;
#37222 = CARTESIAN_POINT ( 'NONE',  ( -10.00000000000000000, -5.773502691896251982, -51.00000000409676915 ) ) ;
#37223 = CARTESIAN_POINT ( 'NONE',  ( -2.293366432827344421E-15, -12.48450537969573659, -12.21875000204836148 ) ) ;
#37224 = CARTESIAN_POINT ( 'NONE',  ( -99.99999999999994316, -20.00000000000000355, -160.0000000000000000 ) ) ;
#37225 = CARTESIAN_POINT ( 'NONE',  ( -10.81189881249999729, 6.242252689847871849, -180.9062500020484094 ) ) ;
#37226 = CARTESIAN_POINT ( 'NONE',  ( -5.405949406250003975, -9.363379034771801557, -8.031250002048350822 ) ) ;
#37227 = DIRECTION ( 'NONE',  ( -0.000000000000000000, -0.000000000000000000, 1.000000000000000000 ) ) ;
#37228 = CYLINDRICAL_SURFACE ( 'NONE', #2756, 9.999999999999998224 ) ;
#37229 = CARTESIAN_POINT ( 'NONE',  ( -5.000000000000003553, -8.660254037844383745, -89.49999999999998579 ) ) ;
#37230 = CARTESIAN_POINT ( 'NONE',  ( -2.121150477449813534E-15, -11.54700538379251284, -60.87499999999998579 ) ) ;
#37231 =( BOUNDED_CURVE ( )  B_SPLINE_CURVE ( 2, ( #28441, #41577, #42626, #19330, #22798, #35549, #32315 ),
 .UNSPECIFIED., .F., .F. ) 
 B_SPLINE_CURVE_WITH_KNOTS ( ( 3, 2, 2, 3 ),
 ( 0.3768656716417911334, 0.3781094527363185187, 0.3793532338308459040, 0.3805970149253732338 ),
 .UNSPECIFIED. ) 
 CURVE ( )  GEOMETRIC_REPRESENTATION_ITEM ( )  RATIONAL_B_SPLINE_CURVE ( ( 0.9999999999999880096, 0.8660254037844506980, 1.000000000000000000, 0.8660254037844387076, 1.000000000000000000, 0.8660254037844267172, 1.000000000000011990 ) ) 
 REPRESENTATION_ITEM ( '' )  );
#37232 = CARTESIAN_POINT ( 'NONE',  ( -9.999999999998456346, -5.773502691897145489, -20.62499999999993250 ) ) ;
#37234 = ORIENTED_EDGE ( 'NONE', *, *, #42108, .T. ) ;
#37233 = CARTESIAN_POINT ( 'NONE',  ( -5.405949406249996869, 9.363379034771805109, -83.53125000204838102 ) ) ;
#37235 = CYLINDRICAL_SURFACE ( 'NONE', #23482, 9.999999999999998224 ) ;
#37237 = ORIENTED_EDGE ( 'NONE', *, *, #19158, .F. ) ;
#37236 = CARTESIAN_POINT ( 'NONE',  ( -9.999999999999998224, 1.224646799147353059E-15, -123.1250000040967905 ) ) ;
#37238 = EDGE_LOOP ( 'NONE', ( #9151, #28403, #40355, #42120 ) ) ;
#37239 = CARTESIAN_POINT ( 'NONE',  ( -5.405949406250003975, -9.363379034771801557, -39.34375000204837391 ) ) ;
#37240 = CARTESIAN_POINT ( 'NONE',  ( -10.81189881249999729, 1.324075727343319199E-15, -29.09375000204836326 ) ) ;
#37241 = CARTESIAN_POINT ( 'NONE',  ( -10.81189881249999907, -6.242252689847864744, -15.65625000204837569 ) ) ;
#37242 =( BOUNDED_CURVE ( )  B_SPLINE_CURVE ( 2, ( #6610, #30138, #576, #32947, #19550, #23446, #32734 ),
 .UNSPECIFIED., .F., .F. ) 
 B_SPLINE_CURVE_WITH_KNOTS ( ( 3, 2, 2, 3 ),
 ( 0.5671641791044778058, 0.5684079601990051911, 0.5696517412935325764, 0.5708955223880599616 ),
 .UNSPECIFIED. ) 
 CURVE ( )  GEOMETRIC_REPRESENTATION_ITEM ( )  RATIONAL_B_SPLINE_CURVE ( ( 0.9999999999999761302, 0.8660254037844625774, 1.000000000000000000, 0.8660254037844387076, 1.000000000000000000, 0.8660254037844148378, 1.000000000000023981 ) ) 
 REPRESENTATION_ITEM ( '' )  );
#37243 = CARTESIAN_POINT ( 'NONE',  ( 10.81189881249999907, 6.242252689847868297, -62.71875000204838813 ) ) ;
#37244 = CARTESIAN_POINT ( 'NONE',  ( -2.121150477449813534E-15, -11.54700538379251284, -131.3750000000000000 ) ) ;
#37245 = CARTESIAN_POINT ( 'NONE',  ( 10.00000000000000000, 5.773502691896255534, -48.37499999999997158 ) ) ;
#37246 = CARTESIAN_POINT ( 'NONE',  ( 10.81189881249999729, 0.000000000000000000, -184.3437500020483810 ) ) ;
#37247 = CARTESIAN_POINT ( 'NONE',  ( 7.644554776091147741E-16, 12.48450537969573659, -168.9687500020483810 ) ) ;
#37248 = CARTESIAN_POINT ( 'NONE',  ( -10.81189881249999729, 6.242252689847871849, -176.2187500020483810 ) ) ;
#37249 = LINE ( 'NONE', #37471, #8814 ) ;
#37250 = CARTESIAN_POINT ( 'NONE',  ( -10.00000000000000000, -5.773502691896252870, -168.0000000040968189 ) ) ;
#37251 = CARTESIAN_POINT ( 'NONE',  ( 7.070501591499377789E-16, 11.54700538379251284, -199.6250000000000000 ) ) ;
#37252 = CARTESIAN_POINT ( 'NONE',  ( 5.405949406249992428, -9.363379034771808662, -112.5937500020483810 ) ) ;
#37253 = CARTESIAN_POINT ( 'NONE',  ( -10.00000000000102496, 5.773502691895664007, -14.87499999999994671 ) ) ;
#37254 = CARTESIAN_POINT ( 'NONE',  ( 7.644554776091147741E-16, 12.48450537969573659, -88.15625000204838102 ) ) ;
#37255 = EDGE_CURVE ( 'NONE', #4745, #982, #8501, .T. ) ;
#37256 = CARTESIAN_POINT ( 'NONE',  ( 10.81189881249999729, 0.000000000000000000, -101.8437500020483810 ) ) ;
#37257 = ADVANCED_FACE ( 'NONE', ( #22663 ), #6269, .F. ) ;
#37258 = CARTESIAN_POINT ( 'NONE',  ( 10.81189881249999729, 0.000000000000000000, -73.34375000204838102 ) ) ;
#37259 = EDGE_CURVE ( 'NONE', #18128, #2019, #4453, .T. ) ;
#37260 = CARTESIAN_POINT ( 'NONE',  ( 10.81189881249999907, 6.242252689847868297, -79.40625000204839523 ) ) ;
#37261 = CARTESIAN_POINT ( 'NONE',  ( -9.999999999999998224, 1.224646799147353059E-15, -154.6250000040967905 ) ) ;
#37262 = CARTESIAN_POINT ( 'NONE',  ( -9.999999999999998224, 5.773502691896259087, -134.8750000000000000 ) ) ;
#37263 = EDGE_CURVE ( 'NONE', #684, #1542, #16154, .T. ) ;
#37264 = CARTESIAN_POINT ( 'NONE',  ( -10.81189881249999729, 1.324075727343319199E-15, -155.2812500020484094 ) ) ;
#37265 = CARTESIAN_POINT ( 'NONE',  ( 10.81189881249999551, -6.242252689847874514, -171.1562500020484094 ) ) ;
#37266 = LOCAL_TIME ( 11, 57, 6.000000000000000000, #950 ) ;
#37267 = CARTESIAN_POINT ( 'NONE',  ( 9.999999999999742428, 5.773502691896404748, -153.7500000040967620 ) ) ;
#37268 = CARTESIAN_POINT ( 'NONE',  ( -9.999999999999998224, 1.224646799147353059E-15, -182.7500000000000000 ) ) ;
#37269 = CARTESIAN_POINT ( 'NONE',  ( -10.81189881249999729, 1.324075727343319199E-15, -105.5937500020483810 ) ) ;
#37270 = CARTESIAN_POINT ( 'NONE',  ( -4.999999999999996447, 8.660254037844387298, -156.0000000000000000 ) ) ;
#37271 = CARTESIAN_POINT ( 'NONE',  ( -10.00000000000000000, -5.773502691896251982, -70.12500000000000000 ) ) ;
#37272 = CARTESIAN_POINT ( 'NONE',  ( 5.405949406249992428, -9.363379034771808662, -1.781250002048373471 ) ) ;
#37273 = CARTESIAN_POINT ( 'NONE',  ( 10.00000000000000000, 5.773502691896255534, -80.25000000409679046 ) ) ;
#37274 = CARTESIAN_POINT ( 'NONE',  ( 9.999999999999998224, 0.000000000000000000, -95.37500000409677625 ) ) ;
#37275 = CC_DESIGN_PERSON_AND_ORGANIZATION_ASSIGNMENT ( #33603, #19778, ( #16278 ) ) ;
#37276 = CARTESIAN_POINT ( 'NONE',  ( -10.81189881249999907, -6.242252689847864744, -102.6562500020483952 ) ) ;
#37277 = CARTESIAN_POINT ( 'NONE',  ( -10.81189881249999729, 1.324075727343319199E-15, -83.28125000204838102 ) ) ;
#37278 = CARTESIAN_POINT ( 'NONE',  ( -9.999999999999998224, 5.773502691896259087, -72.25000000409676204 ) ) ;
#37279 = CARTESIAN_POINT ( 'NONE',  ( -10.00000000000012434, 5.773502691896184480, -167.8749999999999716 ) ) ;
#37280 = CARTESIAN_POINT ( 'NONE',  ( 5.405949406249999534, 9.363379034771803333, -35.59375000204836681 ) ) ;
#37281 = ORIENTED_EDGE ( 'NONE', *, *, #34824, .T. ) ;
#37282 = CARTESIAN_POINT ( 'NONE',  ( -2.121150477449813534E-15, -11.54700538379251284, -5.374999999999960920 ) ) ;
#37283 = CARTESIAN_POINT ( 'NONE',  ( -10.81189881249999729, 6.242252689847871849, -30.90625000204835615 ) ) ;
#37284 = CARTESIAN_POINT ( 'NONE',  ( -2.293366432827344421E-15, -12.48450537969573659, -12.21875000204837391 ) ) ;
#37285 = CARTESIAN_POINT ( 'NONE',  ( -4.999999999999996447, 8.660254037844387298, -142.5000000000000000 ) ) ;
#37286 = EDGE_CURVE ( 'NONE', #14564, #16918, #21061, .T. ) ;
#37287 = CARTESIAN_POINT ( 'NONE',  ( 9.999999999999998224, 0.000000000000000000, -2.375000004096766482 ) ) ;
#37288 = CARTESIAN_POINT ( 'NONE',  ( -2.293366432827344421E-15, -12.48450537969573659, -132.4062500020483810 ) ) ;
#37289 = EDGE_CURVE ( 'NONE', #35300, #5570, #13131, .T. ) ;
#37290 = CARTESIAN_POINT ( 'NONE',  ( -10.00000000000000000, -5.773502691896251982, -182.6250000000000284 ) ) ;
#37291 = CARTESIAN_POINT ( 'NONE',  ( -9.999999999999998224, 1.224646799147353059E-15, -184.6250000040967905 ) ) ;
#37293 = ORIENTED_EDGE ( 'NONE', *, *, #9486, .T. ) ;
#37292 = CARTESIAN_POINT ( 'NONE',  ( 10.81189881249999907, 6.242252689847868297, -109.4062500020483952 ) ) ;
#37294 = CARTESIAN_POINT ( 'NONE',  ( -10.00000000000012434, 5.773502691896184480, -194.8750000000000000 ) ) ;
#37295 = EDGE_CURVE ( 'NONE', #18719, #32801, #6140, .T. ) ;
#37296 = EDGE_LOOP ( 'NONE', ( #39361, #4874, #21963, #11812 ) ) ;
#37297 = ORIENTED_EDGE ( 'NONE', *, *, #16335, .T. ) ;
#37298 = VECTOR ( 'NONE', #13383, 1000.000000000000000 ) ;
#37299 = CARTESIAN_POINT ( 'NONE',  ( -5.405949406250003975, -9.363379034771801557, -36.53125000204837391 ) ) ;
#37300 = CALENDAR_DATE ( 2026, 28, 9 ) ;
#37301 = LOCAL_TIME ( 11, 57, 6.000000000000000000, #22237 ) ;
#37302 = CARTESIAN_POINT ( 'NONE',  ( -10.81189881249999729, 6.242252689847871849, -90.71875000204838102 ) ) ;
#37303 = LINE ( 'NONE', #24160, #35314 ) ;
#37304 = ADVANCED_FACE ( 'NONE', ( #42645 ), #13703, .T. ) ;
#37305 = CARTESIAN_POINT ( 'NONE',  ( -9.999999999999998224, 1.224646799147353059E-15, -200.0000000000000000 ) ) ;
#37306 = CARTESIAN_POINT ( 'NONE',  ( 5.000000000000000000, 8.660254037844385522, -156.6250000040967905 ) ) ;
#37307 = CARTESIAN_POINT ( 'NONE',  ( -10.81189881249999907, -6.242252689847864744, -173.1562500020484094 ) ) ;
#37308 = VECTOR ( 'NONE', #2960, 1000.000000000000114 ) ;
#37309 = CARTESIAN_POINT ( 'NONE',  ( 7.070501591499376803E-16, 11.54700538379251284, -58.62499999999999289 ) ) ;
#37310 = CARTESIAN_POINT ( 'NONE',  ( 7.644554776091147741E-16, 12.48450537969573659, -122.4687500020483952 ) ) ;
#37311 =( BOUNDED_CURVE ( )  B_SPLINE_CURVE ( 2, ( #25033, #27829, #5589, #15284, #31934, #5378, #18529 ),
 .UNSPECIFIED., .F., .F. ) 
 B_SPLINE_CURVE_WITH_KNOTS ( ( 3, 2, 2, 3 ),
 ( 0.6492537313432837909, 0.6504975124378111762, 0.6517412935323385614, 0.6529850746268659467 ),
 .UNSPECIFIED. ) 
 CURVE ( )  GEOMETRIC_REPRESENTATION_ITEM ( )  RATIONAL_B_SPLINE_CURVE ( ( 0.9999999999999761302, 0.8660254037844625774, 1.000000000000000000, 0.8660254037844387076, 1.000000000000000000, 0.8660254037844148378, 1.000000000000023981 ) ) 
 REPRESENTATION_ITEM ( '' )  );
#37312 = CARTESIAN_POINT ( 'NONE',  ( 7.644554776091147741E-16, 12.48450537969573659, -93.96875000204838102 ) ) ;
#37313 = CARTESIAN_POINT ( 'NONE',  ( -5.405949406249996869, 9.363379034771805109, -4.031250002048375691 ) ) ;
#37314 = DIRECTION ( 'NONE',  ( 1.000000000000000000, 0.000000000000000000, 0.000000000000000000 ) ) ;
#37315 = CARTESIAN_POINT ( 'NONE',  ( 10.81189881249999729, 0.000000000000000000, -97.53125000204839523 ) ) ;
#37316 = CARTESIAN_POINT ( 'NONE',  ( -9.999999999999998224, 5.773502691896259087, -174.2500000040967905 ) ) ;
#37317 = CARTESIAN_POINT ( 'NONE',  ( 10.81189881249999729, 0.000000000000000000, -106.3437500020483810 ) ) ;
#37318 = CARTESIAN_POINT ( 'NONE',  ( -10.81189881249999729, -6.242252689847864744, -177.6562500020484094 ) ) ;
#37319 = CYLINDRICAL_SURFACE ( 'NONE', #32379, 9.999999999999998224 ) ;
#37320 = DIRECTION ( 'NONE',  ( -0.000000000000000000, -0.000000000000000000, 1.000000000000000000 ) ) ;
#37321 = CARTESIAN_POINT ( 'NONE',  ( 10.00000000000000000, 5.773502691896255534, -0.3749999999999586997 ) ) ;
#37322 = CARTESIAN_POINT ( 'NONE',  ( -5.405949406249996869, 9.363379034771805109, -50.34375000204835260 ) ) ;
#37323 = CARTESIAN_POINT ( 'NONE',  ( -5.405949406250003975, -9.363379034771801557, -42.34375000204837391 ) ) ;
#37324 = CARTESIAN_POINT ( 'NONE',  ( -9.999999999999998224, 1.224646799147353059E-15, -174.1250000040968189 ) ) ;
#37325 = CARTESIAN_POINT ( 'NONE',  ( -10.81189881249999729, 6.242252689847871849, -14.40625000204836859 ) ) ;
#37326 = CARTESIAN_POINT ( 'NONE',  ( -10.81189881249999729, 6.242252689847871849, -23.21875000204837036 ) ) ;
#37327 = CARTESIAN_POINT ( 'NONE',  ( -4.999999999999996447, 8.660254037844387298, -145.5000000000000000 ) ) ;
#37328 = CARTESIAN_POINT ( 'NONE',  ( -5.405949406249996869, 9.363379034771805109, -128.3437500020484094 ) ) ;
#37329 = CARTESIAN_POINT ( 'NONE',  ( 4.999999999999992006, -8.660254037844389075, -99.74999999999998579 ) ) ;
#37330 = CARTESIAN_POINT ( 'NONE',  ( -5.405949406249996869, 9.363379034771805109, -28.03125000204837036 ) ) ;
#37331 = CARTESIAN_POINT ( 'NONE',  ( -4.999999999999996447, 8.660254037844387298, -115.8750000040967905 ) ) ;
#37332 = CARTESIAN_POINT ( 'NONE',  ( -4.999999999999996447, 8.660254037844387298, -157.8750000040967905 ) ) ;
#37333 = CARTESIAN_POINT ( 'NONE',  ( -5.000000000000003553, -8.660254037844383745, -59.49999999999997158 ) ) ;
#37334 = CARTESIAN_POINT ( 'NONE',  ( -10.81189881249999907, -6.242252689847864744, -125.1562500020483810 ) ) ;
#37335 = CARTESIAN_POINT ( 'NONE',  ( 7.644554776091147741E-16, 12.48450537969573659, -109.1562500020483810 ) ) ;
#37336 = ORIENTED_EDGE ( 'NONE', *, *, #22114, .F. ) ;
#37337 = AXIS2_PLACEMENT_3D ( 'NONE', #16089, #17797, #40042 ) ;
#37338 = DIRECTION ( 'NONE',  ( -0.000000000000000000, -0.000000000000000000, -1.000000000000000000 ) ) ;
#37339 = CARTESIAN_POINT ( 'NONE',  ( 7.070501591499377789E-16, 11.54700538379251284, -99.50000000409677625 ) ) ;
#37340 = CARTESIAN_POINT ( 'NONE',  ( 9.999999999999479527, 5.773502691896553074, -141.7500000040967620 ) ) ;
#37341 = CARTESIAN_POINT ( 'NONE',  ( -2.293366432827344421E-15, -12.48450537969573659, -166.9062500020483810 ) ) ;
#37342 = CARTESIAN_POINT ( 'NONE',  ( -2.293366432827344421E-15, -12.48450537969573659, -58.71875000204837391 ) ) ;
#37343 = ORIENTED_EDGE ( 'NONE', *, *, #5638, .F. ) ;
#37344 = CARTESIAN_POINT ( 'NONE',  ( -9.999999999999998224, 5.773502691896259087, -26.87499999999998579 ) ) ;
#37345 = SECURITY_CLASSIFICATION ( '', '', #2973 ) ;
#37346 = CARTESIAN_POINT ( 'NONE',  ( -10.81189881249999729, 1.324075727343319199E-15, -35.28125000204837391 ) ) ;
#37347 = CARTESIAN_POINT ( 'NONE',  ( -5.000000000000003553, -8.660254037844383745, -163.0000000000000000 ) ) ;
#37348 = DIRECTION ( 'NONE',  ( -1.000000000000000000, 0.000000000000000000, 0.000000000000000000 ) ) ;
#37349 = CARTESIAN_POINT ( 'NONE',  ( 10.00000000000000000, 5.773502691896255534, -26.25000000409677270 ) ) ;
#37350 = AXIS2_PLACEMENT_3D ( 'NONE', #14880, #28075, #11644 ) ;
#37351 = CARTESIAN_POINT ( 'NONE',  ( -10.81189881249999729, 6.242252689847871849, -131.4062500020484094 ) ) ;
#37352 = CARTESIAN_POINT ( 'NONE',  ( 9.999999999999998224, 0.000000000000000000, -46.99999999999998579 ) ) ;
#37353 = CARTESIAN_POINT ( 'NONE',  ( -9.999999999999998224, 0.000000000000000000, -99.99999999999998579 ) ) ;
#37354 = ORIENTED_EDGE ( 'NONE', *, *, #41980, .F. ) ;
#37356 = ORIENTED_EDGE ( 'NONE', *, *, #23075, .T. ) ;
#37355 = ORIENTED_EDGE ( 'NONE', *, *, #27774, .T. ) ;
#37357 = CARTESIAN_POINT ( 'NONE',  ( 9.999999999999998224, 0.000000000000000000, -182.3750000040967905 ) ) ;
#37358 = AXIS2_PLACEMENT_3D ( 'NONE', #35362, #38579, #6216 ) ;
#37359 = CARTESIAN_POINT ( 'NONE',  ( 0.000000000000000000, 0.000000000000000000, -200.0000000000000000 ) ) ;
#37360 =( BOUNDED_CURVE ( )  B_SPLINE_CURVE ( 2, ( #7868, #37200, #20799, #33987, #4408, #17547, #27502 ),
 .UNSPECIFIED., .F., .F. ) 
 B_SPLINE_CURVE_WITH_KNOTS ( ( 3, 2, 2, 3 ),
 ( 0.5522388059701495155, 0.5534825870646767898, 0.5547263681592041751, 0.5559701492537315604 ),
 .UNSPECIFIED. ) 
 CURVE ( )  GEOMETRIC_REPRESENTATION_ITEM ( )  RATIONAL_B_SPLINE_CURVE ( ( 0.9999999999999761302, 0.8660254037844625774, 1.000000000000000000, 0.8660254037844387076, 1.000000000000000000, 0.8660254037844148378, 1.000000000000023981 ) ) 
 REPRESENTATION_ITEM ( '' )  );
#37361 = CARTESIAN_POINT ( 'NONE',  ( 7.644554776091147741E-16, 12.48450537969573659, -167.4687500020483810 ) ) ;
#37362 = CARTESIAN_POINT ( 'NONE',  ( -2.293366432827344421E-15, -12.48450537969573659, -196.9062500020484094 ) ) ;
#37363 = CARTESIAN_POINT ( 'NONE',  ( -5.405949406249996869, 9.363379034771805109, -17.34375000204835260 ) ) ;
#37364 = CARTESIAN_POINT ( 'NONE',  ( -4.999999999999996447, 8.660254037844387298, -150.0000000000000000 ) ) ;
#37365 = CARTESIAN_POINT ( 'NONE',  ( -10.81189881249999729, -6.242252689847864744, -147.4687500020484094 ) ) ;
#37366 = CARTESIAN_POINT ( 'NONE',  ( -10.81189881249999729, 6.242252689847871849, -138.7187500020483810 ) ) ;
#37367 = CARTESIAN_POINT ( 'NONE',  ( -10.81189881249999729, 6.242252689847871849, -105.9062500020483810 ) ) ;
#37368 = CARTESIAN_POINT ( 'NONE',  ( -2.293366432827344421E-15, -12.48450537969573659, -115.7187500020483952 ) ) ;
#37369 = CARTESIAN_POINT ( 'NONE',  ( 10.81189881249999907, 6.242252689847868297, 0.2812499979516491777 ) ) ;
#37370 = CARTESIAN_POINT ( 'NONE',  ( 7.644554776091147741E-16, 12.48450537969573659, -127.1562500020483952 ) ) ;
#37371 = CARTESIAN_POINT ( 'NONE',  ( 10.81189881249999907, 6.242252689847868297, -11.71875000204837214 ) ) ;
#37372 = CARTESIAN_POINT ( 'NONE',  ( 5.405949406249992428, -9.363379034771808662, -129.0937500020483810 ) ) ;
#37373 = CARTESIAN_POINT ( 'NONE',  ( -5.405949406250003975, -9.363379034771801557, -198.5312500020484094 ) ) ;
#37374 = CARTESIAN_POINT ( 'NONE',  ( -4.999999999999996447, 8.660254037844387298, -109.8750000040967763 ) ) ;
#37375 = CARTESIAN_POINT ( 'NONE',  ( 5.000000000000000000, 8.660254037844385522, -156.2500000000000000 ) ) ;
#37376 = CARTESIAN_POINT ( 'NONE',  ( -5.000000000000003553, -8.660254037844383745, -17.49999999999996092 ) ) ;
#37377 = AXIS2_PLACEMENT_3D ( 'NONE', #36436, #36224, #10519 ) ;
#37378 = CARTESIAN_POINT ( 'NONE',  ( 5.405949406249999534, 9.363379034771803333, -77.59375000204838102 ) ) ;
#37379 = CARTESIAN_POINT ( 'NONE',  ( -5.405949406249996869, 9.363379034771805109, -66.84375000204836681 ) ) ;
#37380 = CARTESIAN_POINT ( 'NONE',  ( 9.999999999999998224, 0.000000000000000000, -158.3750000040967905 ) ) ;
#37381 = CARTESIAN_POINT ( 'NONE',  ( -10.81189881249999907, -6.242252689847864744, -33.65625000204836681 ) ) ;
#37382 = CARTESIAN_POINT ( 'NONE',  ( 10.81189881249999907, 6.242252689847868297, -46.21875000204837391 ) ) ;
#37383 = CARTESIAN_POINT ( 'NONE',  ( -5.000000000000003553, -8.660254037844383745, -110.8750000040967763 ) ) ;
#37384 = CARTESIAN_POINT ( 'NONE',  ( -10.81189881249999907, -6.242252689847864744, -150.4687500020484094 ) ) ;
#37385 = CARTESIAN_POINT ( 'NONE',  ( 10.00000000000000000, 5.773502691896255534, -124.8750000000000000 ) ) ;
#37386 = CARTESIAN_POINT ( 'NONE',  ( -10.81189881249999729, 6.242252689847871849, -131.4062500020483810 ) ) ;
#37387 = FACE_OUTER_BOUND ( 'NONE', #3388, .T. ) ;
#37388 = CARTESIAN_POINT ( 'NONE',  ( 4.999999999999992006, -8.660254037844389075, -80.24999999999998579 ) ) ;
#37389 = CARTESIAN_POINT ( 'NONE',  ( 5.405949406249999534, 9.363379034771803333, -14.78125000204835793 ) ) ;
#37390 = VERTEX_POINT ( 'NONE', #36817 ) ;
#37391 = CARTESIAN_POINT ( 'NONE',  ( 5.405949406249992428, -9.363379034771808662, -105.2812500020483810 ) ) ;
#37392 = CARTESIAN_POINT ( 'NONE',  ( 10.00000000000000000, 5.773502691896255534, -126.7500000040967905 ) ) ;
#37393 = CARTESIAN_POINT ( 'NONE',  ( -2.121150477449813534E-15, -11.54700538379251284, -154.2500000040968189 ) ) ;
#37394 = EDGE_CURVE ( 'NONE', #17641, #32014, #5476, .T. ) ;
#37395 = CARTESIAN_POINT ( 'NONE',  ( 4.999999999999992006, -8.660254037844389075, -32.62500000409676915 ) ) ;
#37396 = CARTESIAN_POINT ( 'NONE',  ( 9.999999999999479527, 5.773502691896553074, -148.8749999999999432 ) ) ;
#37397 = CARTESIAN_POINT ( 'NONE',  ( -10.81189881249999729, 1.324075727343319199E-15, -44.28125000204838102 ) ) ;
#37398 = DIRECTION ( 'NONE',  ( 1.000000000000000000, 0.000000000000000000, 0.000000000000000000 ) ) ;
#37399 = CARTESIAN_POINT ( 'NONE',  ( -5.405949406249996869, 9.363379034771805109, -155.5312500020484094 ) ) ;
#37400 = CARTESIAN_POINT ( 'NONE',  ( -10.81189881249999729, 1.324075727343319199E-15, -129.5937500020483810 ) ) ;
#37401 = CARTESIAN_POINT ( 'NONE',  ( 9.999999999999776179, 5.773502691896386985, -190.8750000000000000 ) ) ;
#37402 = EDGE_LOOP ( 'NONE', ( #11733, #17745, #17012, #42540 ) ) ;
#37403 = CARTESIAN_POINT ( 'NONE',  ( 9.999999999999998224, 0.000000000000000000, -31.99999999999997158 ) ) ;
#37405 = EDGE_CURVE ( 'NONE', #10629, #21806, #22819, .T. ) ;
#37404 = ORIENTED_EDGE ( 'NONE', *, *, #27555, .F. ) ;
#37406 = EDGE_LOOP ( 'NONE', ( #373, #737, #20293, #38686 ) ) ;
#37408 = VERTEX_POINT ( 'NONE', #6621 ) ;
#37407 = CARTESIAN_POINT ( 'NONE',  ( 10.81189881249999551, -6.242252689847874514, -110.9687500020483810 ) ) ;
#37409 = CARTESIAN_POINT ( 'NONE',  ( 4.999999999999992006, -8.660254037844389075, -41.62500000409677625 ) ) ;
#37410 = CARTESIAN_POINT ( 'NONE',  ( 5.405949406249999534, 9.363379034771803333, -191.5937500020484094 ) ) ;
#37411 = CARTESIAN_POINT ( 'NONE',  ( -5.405949406250003975, -9.363379034771801557, -40.84375000204837391 ) ) ;
#37412 = CARTESIAN_POINT ( 'NONE',  ( 9.999999999999742428, 5.773502691896404748, -153.7500000040967620 ) ) ;
#37413 = FACE_OUTER_BOUND ( 'NONE', #40785, .T. ) ;
#37414 = CARTESIAN_POINT ( 'NONE',  ( 10.81189881249999551, -6.242252689847874514, -169.4687500020483810 ) ) ;
#37415 = CARTESIAN_POINT ( 'NONE',  ( -10.81189881249999907, -6.242252689847864744, -162.4687500020483526 ) ) ;
#37416 = CARTESIAN_POINT ( 'NONE',  ( -9.999999999999998224, 1.224646799147353059E-15, -25.62500000409675849 ) ) ;
#37417 = CARTESIAN_POINT ( 'NONE',  ( -5.405949406249996869, 9.363379034771805109, -141.8437500020483810 ) ) ;
#37418 = CARTESIAN_POINT ( 'NONE',  ( -2.293366432827344421E-15, -12.48450537969573659, -145.9062500020484094 ) ) ;
#37419 = CARTESIAN_POINT ( 'NONE',  ( 10.81189881249999551, -6.242252689847874514, -152.9687500020484094 ) ) ;
#37420 = CARTESIAN_POINT ( 'NONE',  ( 9.999999999998969713, 5.773502691896851502, -87.37499999999997158 ) ) ;
#37421 = CARTESIAN_POINT ( 'NONE',  ( 7.070501591499377789E-16, 11.54700538379251284, -180.1250000000000000 ) ) ;
#37422 = CARTESIAN_POINT ( 'NONE',  ( -10.81189881249999729, 6.242252689847871849, -86.21875000204838102 ) ) ;
#37423 = CARTESIAN_POINT ( 'NONE',  ( 9.999999999999998224, 0.000000000000000000, -36.49999999999997868 ) ) ;
#37424 = CARTESIAN_POINT ( 'NONE',  ( -5.405949406249996869, 9.363379034771805109, -59.53125000204836681 ) ) ;
#37425 = CARTESIAN_POINT ( 'NONE',  ( 9.999999999999998224, 0.000000000000000000, -13.99999999999995737 ) ) ;
#37426 = CARTESIAN_POINT ( 'NONE',  ( -2.293366432827344421E-15, -12.48450537969573659, -181.7187500020484094 ) ) ;
#37427 = CARTESIAN_POINT ( 'NONE',  ( 10.81189881249999729, 0.000000000000000000, -114.0312500020483952 ) ) ;
#37428 = CARTESIAN_POINT ( 'NONE',  ( -2.293366432827344421E-15, -12.48450537969573659, -154.9062500020483810 ) ) ;
#37429 = DIRECTION ( 'NONE',  ( 0.000000000000000000, 0.000000000000000000, -1.000000000000000000 ) ) ;
#37430 = CARTESIAN_POINT ( 'NONE',  ( 10.81189881249999907, 6.242252689847868297, -44.90625000204836681 ) ) ;
#37431 = CARTESIAN_POINT ( 'NONE',  ( 5.000000000000000000, 8.660254037844385522, -128.1250000040967620 ) ) ;
#37432 = CARTESIAN_POINT ( 'NONE',  ( 7.070501591499377789E-16, 11.54700538379251284, -105.1249999999999858 ) ) ;
#37433 = EDGE_CURVE ( 'NONE', #14344, #20834, #35492, .T. ) ;
#37434 = ORIENTED_EDGE ( 'NONE', *, *, #25926, .F. ) ;
#37435 = CARTESIAN_POINT ( 'NONE',  ( -10.81189881249999729, -6.242252689847864744, -129.6562500020483810 ) ) ;
#37436 = CARTESIAN_POINT ( 'NONE',  ( 7.070501591499377789E-16, 11.54700538379251284, -150.5000000040968189 ) ) ;
#37437 = CARTESIAN_POINT ( 'NONE',  ( -5.405949406250003975, -9.363379034771801557, -179.0312500020483810 ) ) ;
#37438 = ORIENTED_EDGE ( 'NONE', *, *, #25324, .F. ) ;
#37439 = CARTESIAN_POINT ( 'NONE',  ( 4.999999999999992006, -8.660254037844389075, -48.74999999999998579 ) ) ;
#37440 = CARTESIAN_POINT ( 'NONE',  ( 10.81189881249999729, 0.000000000000000000, -184.3437500020483810 ) ) ;
#37441 = CARTESIAN_POINT ( 'NONE',  ( 4.999999999999992006, -8.660254037844389075, -58.12500000409676204 ) ) ;
#37442 = DIRECTION ( 'NONE',  ( 1.000000000000000000, 0.000000000000000000, -0.000000000000000000 ) ) ;
#37443 = CARTESIAN_POINT ( 'NONE',  ( 9.999999999999998224, 0.000000000000000000, -170.3750000040968189 ) ) ;
#37444 = CARTESIAN_POINT ( 'NONE',  ( -2.293366432827344421E-15, -12.48450537969573659, -78.40625000204838102 ) ) ;
#37445 = CARTESIAN_POINT ( 'NONE',  ( 10.81189881249999729, 6.242252689847867408, -47.90625000204836681 ) ) ;
#37446 = CARTESIAN_POINT ( 'NONE',  ( -9.999999999999998224, 5.773502691896259087, -48.25000000409676915 ) ) ;
#37447 = CARTESIAN_POINT ( 'NONE',  ( 5.405949406249999534, 9.363379034771803333, -8.593750002048345493 ) ) ;
#37448 = CARTESIAN_POINT ( 'NONE',  ( -5.000000000000003553, -8.660254037844383745, -134.8750000040967905 ) ) ;
#37449 = CARTESIAN_POINT ( 'NONE',  ( -2.293366432827344421E-15, -12.48450537969573659, -178.9062500020484379 ) ) ;
#37450 = CARTESIAN_POINT ( 'NONE',  ( -10.81189881249999729, 1.324075727343319199E-15, -5.281250002048376579 ) ) ;
#37451 = CARTESIAN_POINT ( 'NONE',  ( 0.000000000000000000, 0.000000000000000000, -99.99999999999998579 ) ) ;
#37452 = CARTESIAN_POINT ( 'NONE',  ( -9.999999999999998224, 1.224646799147353059E-15, -82.24999999999998579 ) ) ;
#37453 = CARTESIAN_POINT ( 'NONE',  ( 7.070501591499376803E-16, 11.54700538379251284, -154.6250000000000284 ) ) ;
#37454 = DIRECTION ( 'NONE',  ( -0.000000000000000000, -0.000000000000000000, -1.000000000000000000 ) ) ;
#37455 = CYLINDRICAL_SURFACE ( 'NONE', #6233, 9.999999999999998224 ) ;
#37457 = ORIENTED_EDGE ( 'NONE', *, *, #11998, .T. ) ;
#37456 = CARTESIAN_POINT ( 'NONE',  ( -10.81189881249999907, -6.242252689847864744, -86.15625000204836681 ) ) ;
#37458 = EDGE_CURVE ( 'NONE', #6661, #10829, #38251, .T. ) ;
#37460 = ORIENTED_EDGE ( 'NONE', *, *, #18388, .F. ) ;
#37459 = FACE_OUTER_BOUND ( 'NONE', #18925, .T. ) ;
#37461 = ORIENTED_EDGE ( 'NONE', *, *, #36863, .F. ) ;
#37462 = CARTESIAN_POINT ( 'NONE',  ( -10.81189881249999729, -6.242252689847864744, -37.96875000204837391 ) ) ;
#37463 = CARTESIAN_POINT ( 'NONE',  ( -10.81189881249999729, 1.324075727343319199E-15, -23.09375000204835615 ) ) ;
#37464 = CARTESIAN_POINT ( 'NONE',  ( -5.405949406249996869, 9.363379034771805109, -14.53125000204835615 ) ) ;
#37465 = CARTESIAN_POINT ( 'NONE',  ( 5.405949406249992428, -9.363379034771808662, -60.09375000204835970 ) ) ;
#37466 = CARTESIAN_POINT ( 'NONE',  ( -9.999999999999998224, 1.224646799147353059E-15, -163.6250000040967905 ) ) ;
#37467 = CARTESIAN_POINT ( 'NONE',  ( 5.000000000000000000, 8.660254037844385522, -40.74999999999997868 ) ) ;
#37468 = CARTESIAN_POINT ( 'NONE',  ( -10.81189881249999729, 1.324075727343319199E-15, -188.0937500020483810 ) ) ;
#37469 = CARTESIAN_POINT ( 'NONE',  ( 10.81189881249999551, -6.242252689847874514, -169.4687500020483810 ) ) ;
#37470 = CARTESIAN_POINT ( 'NONE',  ( -2.293366432827344421E-15, -12.48450537969573659, -175.7187500020483810 ) ) ;
#37471 = CARTESIAN_POINT ( 'NONE',  ( -9.999999999999998224, 1.224646799147353059E-15, -200.0000000000000000 ) ) ;
#37472 = CARTESIAN_POINT ( 'NONE',  ( 0.000000000000000000, 0.000000000000000000, -200.0000000000000000 ) ) ;
#37473 = CARTESIAN_POINT ( 'NONE',  ( -9.999999999998969713, -5.773502691896847949, -21.00000000409676204 ) ) ;
#37474 = DIRECTION ( 'NONE',  ( -0.000000000000000000, -0.000000000000000000, 1.000000000000000000 ) ) ;
#37475 = CARTESIAN_POINT ( 'NONE',  ( 7.644554776091147741E-16, 12.48450537969573659, -114.9687500020483668 ) ) ;
#37476 = CYLINDRICAL_SURFACE ( 'NONE', #19716, 9.999999999999998224 ) ;
#37477 = CARTESIAN_POINT ( 'NONE',  ( -5.405949406249996869, 9.363379034771805109, -85.03125000204838102 ) ) ;
#37478 = CARTESIAN_POINT ( 'NONE',  ( 10.81189881249999729, 6.242252689847867408, -101.7187500020483810 ) ) ;
#37479 = CARTESIAN_POINT ( 'NONE',  ( 5.405949406249999534, 9.363379034771803333, -61.09375000204836681 ) ) ;
#37480 = CARTESIAN_POINT ( 'NONE',  ( 10.81189881249999907, 6.242252689847868297, -65.90625000204839523 ) ) ;
#37481 = CARTESIAN_POINT ( 'NONE',  ( -5.000000000000003553, -8.660254037844383745, -151.3750000040967905 ) ) ;
#37482 = CARTESIAN_POINT ( 'NONE',  ( -10.00000000000000000, -5.773502691896251982, -131.6250000000000000 ) ) ;
#37483 =( BOUNDED_CURVE ( )  B_SPLINE_CURVE ( 2, ( #13496, #33596, #6417, #29502, #19557, #16306, #10060 ),
 .UNSPECIFIED., .F., .F. ) 
 B_SPLINE_CURVE_WITH_KNOTS ( ( 3, 2, 2, 3 ),
 ( 0.08582089552238814090, 0.08706467661691551230, 0.08830845771144288370, 0.08955223880597024122 ),
 .UNSPECIFIED. ) 
 CURVE ( )  GEOMETRIC_REPRESENTATION_ITEM ( )  RATIONAL_B_SPLINE_CURVE ( ( 0.9999999999999910072, 0.8660254037844477004, 1.000000000000000000, 0.8660254037844387076, 1.000000000000000000, 0.8660254037844282715, 1.000000000000010436 ) ) 
 REPRESENTATION_ITEM ( '' )  );
#37484 = CARTESIAN_POINT ( 'NONE',  ( 5.405949406249999534, 9.363379034771803333, -160.2812500020484094 ) ) ;
#37485 = CARTESIAN_POINT ( 'NONE',  ( 7.644554776091147741E-16, 12.48450537969573659, -169.1562500020484094 ) ) ;
#37486 = CARTESIAN_POINT ( 'NONE',  ( 5.405949406249999534, 9.363379034771803333, -1.093750002048365921 ) ) ;
#37487 = CARTESIAN_POINT ( 'NONE',  ( -5.405949406250003975, -9.363379034771801557, -106.8437500020483810 ) ) ;
#37488 = FACE_OUTER_BOUND ( 'NONE', #8598, .T. ) ;
#37489 = CARTESIAN_POINT ( 'NONE',  ( -2.121150477449813534E-15, -11.54700538379251284, -69.87500000000000000 ) ) ;
#37490 = CARTESIAN_POINT ( 'NONE',  ( 10.81189881249999551, -6.242252689847874514, -7.656250002048365921 ) ) ;
#37491 = CARTESIAN_POINT ( 'NONE',  ( 9.999999999999996447, -5.773502691896262640, -83.50000000409676204 ) ) ;
#37492 = CARTESIAN_POINT ( 'NONE',  ( -9.999999999999998224, 1.224646799147353059E-15, -133.6250000040967620 ) ) ;
#37493 = CARTESIAN_POINT ( 'NONE',  ( 5.405949406249999534, 9.363379034771803333, -97.28125000204839523 ) ) ;
#37494 = CARTESIAN_POINT ( 'NONE',  ( 10.81189881249999729, 0.000000000000000000, -75.03125000204838102 ) ) ;
#37495 =( BOUNDED_CURVE ( )  B_SPLINE_CURVE ( 2, ( #37049, #20430, #20002, #4250, #23474, #4034, #33408 ),
 .UNSPECIFIED., .F., .F. ) 
 B_SPLINE_CURVE_WITH_KNOTS ( ( 3, 2, 2, 3 ),
 ( 0.1865671641791045166, 0.1878109452736318741, 0.1890547263681592594, 0.1902985074626866169 ),
 .UNSPECIFIED. ) 
 CURVE ( )  GEOMETRIC_REPRESENTATION_ITEM ( )  RATIONAL_B_SPLINE_CURVE ( ( 0.9999999999999970024, 0.8660254037844417052, 1.000000000000000000, 0.8660254037844387076, 1.000000000000000000, 0.8660254037844327124, 1.000000000000005995 ) ) 
 REPRESENTATION_ITEM ( '' )  );
#37496 = CARTESIAN_POINT ( 'NONE',  ( 5.000000000000000000, 8.660254037844385522, -78.62500000409677625 ) ) ;
#37497 = CARTESIAN_POINT ( 'NONE',  ( 5.000000000000000000, 8.660254037844385522, -135.2499999999999716 ) ) ;
#37498 = CARTESIAN_POINT ( 'NONE',  ( -5.405949406250003975, -9.363379034771801557, -36.34375000204836681 ) ) ;
#37499 = VERTEX_POINT ( 'NONE', #18019 ) ;
#37500 = CARTESIAN_POINT ( 'NONE',  ( 10.00000000000000000, 5.773502691896255534, -0.3749999999999697464 ) ) ;
#37501 = CARTESIAN_POINT ( 'NONE',  ( -10.81189881249999729, 1.324075727343319199E-15, -24.78125000204836681 ) ) ;
#37502 = CARTESIAN_POINT ( 'NONE',  ( 5.405949406249999534, 9.363379034771803333, -13.09375000204834905 ) ) ;
#37503 = CARTESIAN_POINT ( 'NONE',  ( -9.999999999999998224, 1.224646799147353059E-15, -94.62500000409677625 ) ) ;
#37504 = CARTESIAN_POINT ( 'NONE',  ( 9.999999999999996447, -5.773502691896262640, -7.000000004096756712 ) ) ;
#37505 = CARTESIAN_POINT ( 'NONE',  ( 7.644554776091147741E-16, 12.48450537969573659, -127.1562500020483952 ) ) ;
#37506 =( BOUNDED_CURVE ( )  B_SPLINE_CURVE ( 2, ( #21813, #36039, #22661, #39055, #225, #13347, #26537 ),
 .UNSPECIFIED., .F., .F. ) 
 B_SPLINE_CURVE_WITH_KNOTS ( ( 3, 2, 2, 3 ),
 ( 0.4141791044776120256, 0.4154228855721394109, 0.4166666666666667962, 0.4179104477611941260 ),
 .UNSPECIFIED. ) 
 CURVE ( )  GEOMETRIC_REPRESENTATION_ITEM ( )  RATIONAL_B_SPLINE_CURVE ( ( 0.9999999999999880096, 0.8660254037844506980, 1.000000000000000000, 0.8660254037844387076, 1.000000000000000000, 0.8660254037844267172, 1.000000000000011990 ) ) 
 REPRESENTATION_ITEM ( '' )  );
#37507 = CARTESIAN_POINT ( 'NONE',  ( -9.999999999999998224, 5.773502691896259087, -184.3750000000000000 ) ) ;
#37508 = CARTESIAN_POINT ( 'NONE',  ( 9.999999999999998224, 0.000000000000000000, -120.5000000000000000 ) ) ;
#37510 = ORIENTED_EDGE ( 'NONE', *, *, #36192, .F. ) ;
#37509 = CARTESIAN_POINT ( 'NONE',  ( -10.81189881249999907, -6.242252689847864744, -108.6562500020483952 ) ) ;
#37511 = DIRECTION ( 'NONE',  ( -1.000000000000000000, 0.000000000000000000, 0.000000000000000000 ) ) ;
#37512 = EDGE_CURVE ( 'NONE', #19666, #2132, #37032, .T. ) ;
#37513 = ORIENTED_EDGE ( 'NONE', *, *, #12588, .T. ) ;
#37514 = EDGE_CURVE ( 'NONE', #35669, #134, #13744, .T. ) ;
#37515 = ORIENTED_EDGE ( 'NONE', *, *, #9473, .F. ) ;
#37516 = CARTESIAN_POINT ( 'NONE',  ( -10.81189881249999729, 1.324075727343319199E-15, -38.28125000204838102 ) ) ;
#37517 = APPROVAL_DATE_TIME ( #20893, #7210 ) ;
#37518 = CARTESIAN_POINT ( 'NONE',  ( -5.405949406250003975, -9.363379034771801557, -85.84375000204836681 ) ) ;
#37519 = DIRECTION ( 'NONE',  ( 1.000000000000000000, 0.000000000000000000, 0.000000000000000000 ) ) ;
#37520 = CARTESIAN_POINT ( 'NONE',  ( -5.000000000000003553, -8.660254037844383745, -128.8750000040967905 ) ) ;
#37521 = CARTESIAN_POINT ( 'NONE',  ( 5.000000000000000000, 8.660254037844385522, -105.6250000040967763 ) ) ;
#37522 = CARTESIAN_POINT ( 'NONE',  ( 10.81189881249999907, 6.242252689847868297, -161.9062500020484094 ) ) ;
#37523 = CARTESIAN_POINT ( 'NONE',  ( 9.999999999999998224, 0.000000000000000000, -200.0000000000000000 ) ) ;
#37524 = EDGE_CURVE ( 'NONE', #41727, #5730, #33592, .T. ) ;
#37525 = CARTESIAN_POINT ( 'NONE',  ( 10.81189881249999551, -6.242252689847874514, -125.9687500020483810 ) ) ;
#37526 = CARTESIAN_POINT ( 'NONE',  ( 10.81189881249999907, 6.242252689847868297, -94.21875000204838102 ) ) ;
#37527 = CARTESIAN_POINT ( 'NONE',  ( 10.81189881249999551, -6.242252689847874514, -1.656250002048371917 ) ) ;
#37528 = CARTESIAN_POINT ( 'NONE',  ( -2.293366432827344421E-15, -12.48450537969573659, -190.7187500020484094 ) ) ;
#37529 = CARTESIAN_POINT ( 'NONE',  ( 5.405949406249992428, -9.363379034771808662, -97.78125000204839523 ) ) ;
#37530 = CARTESIAN_POINT ( 'NONE',  ( -5.000000000000003553, -8.660254037844383745, -175.3750000040967905 ) ) ;
#37531 = CARTESIAN_POINT ( 'NONE',  ( -10.81189881249999729, 1.324075727343319199E-15, -108.5937500020483810 ) ) ;
#37532 = CARTESIAN_POINT ( 'NONE',  ( -5.405949406249996869, 9.363379034771805109, -175.0312500020484094 ) ) ;
#37533 = CARTESIAN_POINT ( 'NONE',  ( -9.999999999999998224, 1.224646799147353059E-15, -151.6250000040967905 ) ) ;
#37534 = CARTESIAN_POINT ( 'NONE',  ( -9.999999999999998224, 1.224646799147353059E-15, -121.6250000040967905 ) ) ;
#37535 = CARTESIAN_POINT ( 'NONE',  ( 5.000000000000000000, 8.660254037844385522, -0.2499999999999724665 ) ) ;
#37536 = CARTESIAN_POINT ( 'NONE',  ( -10.81189881249999729, 1.324075727343319199E-15, -48.59375000204838102 ) ) ;
#37537 = CARTESIAN_POINT ( 'NONE',  ( -2.121150477449813534E-15, -11.54700538379251284, -172.2500000040968189 ) ) ;
#37538 = CARTESIAN_POINT ( 'NONE',  ( 10.81189881249999907, 6.242252689847868297, -8.906250002048375691 ) ) ;
#37539 = CARTESIAN_POINT ( 'NONE',  ( 5.405949406249999534, 9.363379034771803333, -23.59375000204835970 ) ) ;
#37540 = CARTESIAN_POINT ( 'NONE',  ( -9.999999999999998224, 1.224646799147353059E-15, -193.6250000040967905 ) ) ;
#37541 = CARTESIAN_POINT ( 'NONE',  ( 10.81189881249999551, -6.242252689847874514, -131.9687500020483810 ) ) ;
#37542 = CARTESIAN_POINT ( 'NONE',  ( 9.999999999999996447, -5.773502691896262640, -95.12499999999998579 ) ) ;
#37543 = CARTESIAN_POINT ( 'NONE',  ( -10.81189881249999907, -6.242252689847864744, -32.15625000204835970 ) ) ;
#37544 = CARTESIAN_POINT ( 'NONE',  ( 10.00000000000000000, 5.773502691896255534, -107.2500000040967763 ) ) ;
#37545 = EDGE_CURVE ( 'NONE', #8658, #40301, #26400, .T. ) ;
#37546 = CARTESIAN_POINT ( 'NONE',  ( 0.000000000000000000, 0.000000000000000000, -200.0000000000000000 ) ) ;
#37547 = CARTESIAN_POINT ( 'NONE',  ( -10.00000000000000000, -5.773502691896251982, -53.62499999999997868 ) ) ;
#37548 = CARTESIAN_POINT ( 'NONE',  ( -10.81189881249999729, 6.242252689847871849, -126.9062500020483810 ) ) ;
#37549 = CARTESIAN_POINT ( 'NONE',  ( 10.81189881249999551, -6.242252689847874514, -97.65625000204839523 ) ) ;
#37550 = ORIENTED_EDGE ( 'NONE', *, *, #9834, .T. ) ;
#37551 = CARTESIAN_POINT ( 'NONE',  ( -4.999999999999996447, 8.660254037844387298, -97.87500000409677625 ) ) ;
#37552 = CARTESIAN_POINT ( 'NONE',  ( -10.00000000000051337, 5.773502691895962435, -91.37499999999997158 ) ) ;
#37553 = CARTESIAN_POINT ( 'NONE',  ( -10.81189881249999729, 6.242252689847871849, -161.4062500020483810 ) ) ;
#37554 = CARTESIAN_POINT ( 'NONE',  ( 10.81189881249999907, 6.242252689847868297, -55.21875000204836681 ) ) ;
#37555 = ORIENTED_EDGE ( 'NONE', *, *, #32223, .F. ) ;
#37556 = CARTESIAN_POINT ( 'NONE',  ( 9.999999999999998224, 0.000000000000000000, -25.99999999999996803 ) ) ;
#37557 = CARTESIAN_POINT ( 'NONE',  ( 5.405949406249992428, -9.363379034771808662, -37.78125000204838102 ) ) ;
#37558 = CARTESIAN_POINT ( 'NONE',  ( -5.000000000000003553, -8.660254037844383745, -158.5000000000000000 ) ) ;
#37559 = CARTESIAN_POINT ( 'NONE',  ( 10.00000000000051159, -5.773502691895965988, -92.12499999999997158 ) ) ;
#37560 = CARTESIAN_POINT ( 'NONE',  ( -4.999999999999996447, 8.660254037844387298, -24.37500000409675849 ) ) ;
#37561 = LINE ( 'NONE', #31533, #7745 ) ;
#37562 = CARTESIAN_POINT ( 'NONE',  ( 5.405949406249999534, 9.363379034771803333, -136.2812500020483810 ) ) ;
#37563 = DIRECTION ( 'NONE',  ( -0.000000000000000000, -0.000000000000000000, 1.000000000000000000 ) ) ;
#37564 = EDGE_CURVE ( 'NONE', #18570, #6727, #23883, .T. ) ;
#37565 = EDGE_LOOP ( 'NONE', ( #1915, #2697, #9796, #14455 ) ) ;
#37566 = EDGE_CURVE ( 'NONE', #6715, #7196, #34452, .T. ) ;
#37567 = EDGE_CURVE ( 'NONE', #29817, #35407, #23381, .T. ) ;
#37569 = ORIENTED_EDGE ( 'NONE', *, *, #18388, .T. ) ;
#37568 = ORIENTED_EDGE ( 'NONE', *, *, #39352, .F. ) ;
#37570 =( BOUNDED_CURVE ( )  B_SPLINE_CURVE ( 2, ( #9657, #22830, #36196, #10075, #33188, #26905, #40061 ),
 .UNSPECIFIED., .F., .F. ) 
 B_SPLINE_CURVE_WITH_KNOTS ( ( 3, 2, 2, 3 ),
 ( 0.1343283582089551953, 0.1355721393034825528, 0.1368159203980099381, 0.1380597014925373234 ),
 .UNSPECIFIED. ) 
 CURVE ( )  GEOMETRIC_REPRESENTATION_ITEM ( )  RATIONAL_B_SPLINE_CURVE ( ( 1.000000000000003109, 0.8660254037844358210, 1.000000000000000000, 0.8660254037844387076, 1.000000000000000000, 0.8660254037844387076, 1.000000000000000000 ) ) 
 REPRESENTATION_ITEM ( '' )  );
#37571 = CARTESIAN_POINT ( 'NONE',  ( 9.999999999999998224, 0.000000000000000000, -200.0000000000000000 ) ) ;
#37572 = CARTESIAN_POINT ( 'NONE',  ( 7.070501591499376803E-16, 11.54700538379251284, -174.5000000040967905 ) ) ;
#37573 = CARTESIAN_POINT ( 'NONE',  ( -5.405949406250003975, -9.363379034771801557, -165.3437500020484094 ) ) ;
#37574 = CARTESIAN_POINT ( 'NONE',  ( 7.644554776091147741E-16, 12.48450537969573659, -193.1562500020484094 ) ) ;
#37575 = CARTESIAN_POINT ( 'NONE',  ( 10.81189881249999551, -6.242252689847874514, -11.96875000204837214 ) ) ;
#37576 = DIRECTION ( 'NONE',  ( -0.4999999999999998890, -0.8660254037844387076, 0.000000000000000000 ) ) ;
#37577 = CARTESIAN_POINT ( 'NONE',  ( 7.644554776091147741E-16, 12.48450537969573659, -144.9687500020484094 ) ) ;
#37578 = CARTESIAN_POINT ( 'NONE',  ( 10.81189881249999907, 6.242252689847868297, -137.7187500020484094 ) ) ;
#37579 = CARTESIAN_POINT ( 'NONE',  ( -5.405949406250003975, -9.363379034771801557, -108.5312500020483810 ) ) ;
#37580 = CARTESIAN_POINT ( 'NONE',  ( 5.405949406249999534, 9.363379034771803333, -116.5937500020483810 ) ) ;
#37581 = CARTESIAN_POINT ( 'NONE',  ( 4.999999999999992006, -8.660254037844389075, -194.6250000040967905 ) ) ;
#37582 = CARTESIAN_POINT ( 'NONE',  ( -10.81189881249999729, 1.324075727343319199E-15, -120.7812500020483952 ) ) ;
#37583 = CARTESIAN_POINT ( 'NONE',  ( 5.405949406249992428, -9.363379034771808662, -6.093750002048370362 ) ) ;
#37585 = ADVANCED_FACE ( 'NONE', ( #37459 ), #24315, .F. ) ;
#37584 = CARTESIAN_POINT ( 'NONE',  ( 5.405949406249999534, 9.363379034771803333, -128.5937500020483810 ) ) ;
#37586 = CARTESIAN_POINT ( 'NONE',  ( -9.999999999999998224, 1.224646799147353059E-15, -55.24999999999996447 ) ) ;
#37587 = CARTESIAN_POINT ( 'NONE',  ( 7.071067811865472841, -7.071067811865472841, -200.0000000000000000 ) ) ;
#37588 = CARTESIAN_POINT ( 'NONE',  ( -9.999999999999998224, 5.773502691896259087, -149.8750000000000000 ) ) ;
#37589 = CARTESIAN_POINT ( 'NONE',  ( 9.999999999999998224, 0.000000000000000000, -22.99999999999996447 ) ) ;
#37590 = CARTESIAN_POINT ( 'NONE',  ( 10.81189881249999551, -6.242252689847874514, -73.46875000204836681 ) ) ;
#37591 = CARTESIAN_POINT ( 'NONE',  ( 5.405949406249999534, 9.363379034771803333, -64.09375000204836681 ) ) ;
#37592 = CARTESIAN_POINT ( 'NONE',  ( -5.000000000000003553, -8.660254037844383745, -19.37500000409675494 ) ) ;
#37593 = CARTESIAN_POINT ( 'NONE',  ( -10.81189881249999907, -6.242252689847864744, -30.65625000204835260 ) ) ;
#37594 = CARTESIAN_POINT ( 'NONE',  ( -5.405949406250003975, -9.363379034771801557, -48.34375000204838102 ) ) ;
#37595 = CARTESIAN_POINT ( 'NONE',  ( 4.999999999999992006, -8.660254037844389075, -163.1250000040967905 ) ) ;
#37596 = CARTESIAN_POINT ( 'NONE',  ( -10.81189881249999907, -6.242252689847864744, -156.4687500020484379 ) ) ;
#37597 = CARTESIAN_POINT ( 'NONE',  ( 9.999999999999996447, -5.773502691896262640, -117.6250000000000000 ) ) ;
#37598 = CARTESIAN_POINT ( 'NONE',  ( -10.81189881249999729, 1.324075727343319199E-15, -132.7812500020483810 ) ) ;
#37599 = CARTESIAN_POINT ( 'NONE',  ( -1.877755174760191048, 9.997121275661758233, -180.0000000000000284 ) ) ;
#37600 = VECTOR ( 'NONE', #37338, 1000.000000000000000 ) ;
#37601 = CARTESIAN_POINT ( 'NONE',  ( 10.00000000000000000, 5.773502691896255534, -87.37499999999998579 ) ) ;
#37602 = CARTESIAN_POINT ( 'NONE',  ( 10.81189881249999551, -6.242252689847874514, -16.65625000204838102 ) ) ;
#37603 = EDGE_LOOP ( 'NONE', ( #18665, #6245, #2131, #13464 ) ) ;
#37604 = CARTESIAN_POINT ( 'NONE',  ( -10.81189881249999729, -6.242252689847864744, -102.6562500020483952 ) ) ;
#37605 = CARTESIAN_POINT ( 'NONE',  ( 4.999999999999992006, -8.660254037844389075, -125.6250000040967620 ) ) ;
#37606 = CARTESIAN_POINT ( 'NONE',  ( 10.00000000000051159, -5.773502691895965988, -143.5000000040967905 ) ) ;
#37607 = CARTESIAN_POINT ( 'NONE',  ( 5.000000000000000000, 8.660254037844385522, -36.62500000409676915 ) ) ;
#37608 = CARTESIAN_POINT ( 'NONE',  ( 7.070501591499376803E-16, 11.54700538379251284, -130.6250000000000000 ) ) ;
#37609 = CARTESIAN_POINT ( 'NONE',  ( 7.644554776091147741E-16, 12.48450537969573659, -46.15625000204837391 ) ) ;
#37610 = CARTESIAN_POINT ( 'NONE',  ( -10.00000000000025580, 5.773502691896109873, -100.7500000040968047 ) ) ;
#37611 = CARTESIAN_POINT ( 'NONE',  ( 5.405949406249999534, 9.363379034771803333, -152.7812500020484094 ) ) ;
#37612 = CARTESIAN_POINT ( 'NONE',  ( -5.405949406250003975, -9.363379034771801557, -130.8437500020484094 ) ) ;
#37613 = CARTESIAN_POINT ( 'NONE',  ( -10.00000000000051337, 5.773502691895962435, -143.8750000000000000 ) ) ;
#37614 = ORIENTED_EDGE ( 'NONE', *, *, #24444, .F. ) ;
#37615 = CARTESIAN_POINT ( 'NONE',  ( 9.999999999999998224, 0.000000000000000000, -177.5000000000000000 ) ) ;
#37616 = ORIENTED_EDGE ( 'NONE', *, *, #29248, .F. ) ;
#37617 =( BOUNDED_CURVE ( )  B_SPLINE_CURVE ( 2, ( #26645, #23631, #13243, #26225, #36776, #13449, #6788 ),
 .UNSPECIFIED., .F., .F. ) 
 B_SPLINE_CURVE_WITH_KNOTS ( ( 3, 2, 2, 3 ),
 ( 0.3992537313432836799, 0.4004975124378110651, 0.4017412935323383949, 0.4029850746268657802 ),
 .UNSPECIFIED. ) 
 CURVE ( )  GEOMETRIC_REPRESENTATION_ITEM ( )  RATIONAL_B_SPLINE_CURVE ( ( 0.9999999999999880096, 0.8660254037844506980, 1.000000000000000000, 0.8660254037844387076, 1.000000000000000000, 0.8660254037844267172, 1.000000000000011990 ) ) 
 REPRESENTATION_ITEM ( '' )  );
#37618 = ORIENTED_EDGE ( 'NONE', *, *, #6976, .T. ) ;
#37619 = ORIENTED_EDGE ( 'NONE', *, *, #27535, .F. ) ;
#37620 = AXIS2_PLACEMENT_3D ( 'NONE', #19296, #2917, #16047 ) ;
#37621 = CARTESIAN_POINT ( 'NONE',  ( 9.999999999999998224, 0.000000000000000000, -144.8750000040967905 ) ) ;
#37622 = CARTESIAN_POINT ( 'NONE',  ( -10.81189881249999907, -6.242252689847864744, -189.4687500020484094 ) ) ;
#37623 = VECTOR ( 'NONE', #26154, 1000.000000000000114 ) ;
#37625 = EDGE_CURVE ( 'NONE', #933, #5984, #14772, .T. ) ;
#37624 = CARTESIAN_POINT ( 'NONE',  ( 10.81189881249999729, 0.000000000000000000, -37.34375000204836681 ) ) ;
#37626 = CARTESIAN_POINT ( 'NONE',  ( -2.544246206568858693, -10.01717225130982492, 6.879861566378983540E-16 ) ) ;
#37627 = CARTESIAN_POINT ( 'NONE',  ( 9.999999999999998224, 0.000000000000000000, -73.99999999999998579 ) ) ;
#37628 = CARTESIAN_POINT ( 'NONE',  ( 7.644554776091147741E-16, 12.48450537969573659, -170.4687500020483810 ) ) ;
#37629 = AXIS2_PLACEMENT_3D ( 'NONE', #23303, #39269, #33242 ) ;
#37630 = CARTESIAN_POINT ( 'NONE',  ( 5.405949406249999534, 9.363379034771803333, -158.5937500020483810 ) ) ;
#37631 = DIRECTION ( 'NONE',  ( -0.000000000000000000, -0.000000000000000000, 1.000000000000000000 ) ) ;
#37632 = CARTESIAN_POINT ( 'NONE',  ( -5.405949406249996869, 9.363379034771805109, -144.8437500020483810 ) ) ;
#37633 = CARTESIAN_POINT ( 'NONE',  ( 10.81189881249999551, -6.242252689847874514, -150.1562500020484094 ) ) ;
#37634 = CARTESIAN_POINT ( 'NONE',  ( 10.81189881249999729, 0.000000000000000000, -152.8437500020483810 ) ) ;
#37635 = CARTESIAN_POINT ( 'NONE',  ( 5.000000000000000000, 8.660254037844385522, -134.1250000040967620 ) ) ;
#37636 = CARTESIAN_POINT ( 'NONE',  ( 9.999999999998969713, 5.773502691896851502, -66.75000000409674783 ) ) ;
#37637 = CARTESIAN_POINT ( 'NONE',  ( -10.00000000000000000, -5.773502691896251982, -167.6249999999999716 ) ) ;
#37638 = CARTESIAN_POINT ( 'NONE',  ( -5.405949406250003975, -9.363379034771801557, -88.84375000204838102 ) ) ;
#37639 = CARTESIAN_POINT ( 'NONE',  ( -9.999999999999998224, 1.224646799147353059E-15, -113.7499999999999858 ) ) ;
#37640 = CARTESIAN_POINT ( 'NONE',  ( -10.81189881249999907, -6.242252689847864744, -60.65625000204840234 ) ) ;
#37641 = DIRECTION ( 'NONE',  ( -1.000000000000000000, 0.000000000000000000, 0.000000000000000000 ) ) ;
#37642 = CARTESIAN_POINT ( 'NONE',  ( 10.81189881249999551, -6.242252689847874514, -178.4687500020484094 ) ) ;
#37643 = CARTESIAN_POINT ( 'NONE',  ( -10.81189881249999729, 6.242252689847871849, -113.4062500020483810 ) ) ;
#37644 = CARTESIAN_POINT ( 'NONE',  ( -5.405949406249996869, 9.363379034771805109, -155.5312500020484094 ) ) ;
#37645 = CARTESIAN_POINT ( 'NONE',  ( -5.000000000000003553, -8.660254037844383745, -11.49999999999995381 ) ) ;
#37646 = CARTESIAN_POINT ( 'NONE',  ( -10.81189881249999729, 6.242252689847871849, -42.90625000204836681 ) ) ;
#37647 = CARTESIAN_POINT ( 'NONE',  ( -10.00000000000000000, -5.773502691896251982, -130.5000000040967905 ) ) ;
#37648 = CARTESIAN_POINT ( 'NONE',  ( 5.000000000000000000, 8.660254037844385522, -106.7499999999999858 ) ) ;
#37649 = ORIENTED_EDGE ( 'NONE', *, *, #15271, .T. ) ;
#37650 = CARTESIAN_POINT ( 'NONE',  ( 7.644554776091147741E-16, 12.48450537969573659, -128.6562500020483810 ) ) ;
#37651 = CARTESIAN_POINT ( 'NONE',  ( -5.000000000000003553, -8.660254037844383745, -148.3750000040967905 ) ) ;
#37652 = CARTESIAN_POINT ( 'NONE',  ( -1.040834085586084257E-14, 125.0000000000000000, 22.49999999999999289 ) ) ;
#37653 = CARTESIAN_POINT ( 'NONE',  ( -10.81189881249999907, -6.242252689847864744, -177.6562500020484094 ) ) ;
#37654 = VERTEX_POINT ( 'NONE', #34665 ) ;
#37655 = CARTESIAN_POINT ( 'NONE',  ( 7.644554776091147741E-16, 12.48450537969573659, -173.4687500020483810 ) ) ;
#37656 = CARTESIAN_POINT ( 'NONE',  ( 7.070501591499377789E-16, 11.54700538379251284, -62.00000000409678336 ) ) ;
#37657 = CARTESIAN_POINT ( 'NONE',  ( -9.999999999999998224, 0.000000000000000000, -99.99999999999998579 ) ) ;
#37658 = CARTESIAN_POINT ( 'NONE',  ( 10.00000000000000000, 5.773502691896255534, -135.7500000040967905 ) ) ;
#37659 = CARTESIAN_POINT ( 'NONE',  ( 10.81189881249999907, 6.242252689847868297, -64.40625000204839523 ) ) ;
#37660 = CONICAL_SURFACE ( 'NONE', #32832, 22.00000000000000711, 0.7853981633974466137 ) ;
#37661 = CARTESIAN_POINT ( 'NONE',  ( -10.81189881249999729, 6.242252689847871849, -50.40625000204837391 ) ) ;
#37662 = CARTESIAN_POINT ( 'NONE',  ( 7.070501591499377789E-16, 11.54700538379251284, -42.50000000409676204 ) ) ;
#37663 = CARTESIAN_POINT ( 'NONE',  ( 5.405949406249999534, 9.363379034771803333, -4.093750002048368586 ) ) ;
#37664 = CARTESIAN_POINT ( 'NONE',  ( -10.00000000000012434, 5.773502691896184480, -157.7500000040967905 ) ) ;
#37665 = CARTESIAN_POINT ( 'NONE',  ( 10.81189881249999729, 0.000000000000000000, -177.0312500020483810 ) ) ;
#37666 = CARTESIAN_POINT ( 'NONE',  ( 10.00000000000051159, -5.773502691895965988, -73.00000000409676204 ) ) ;
#37667 = CARTESIAN_POINT ( 'NONE',  ( 9.999999999999998224, 0.000000000000000000, -81.49999999999998579 ) ) ;
#37668 = VERTEX_POINT ( 'NONE', #4654 ) ;
#37669 = DIRECTION ( 'NONE',  ( -0.000000000000000000, -0.000000000000000000, 1.000000000000000000 ) ) ;
#37670 = CARTESIAN_POINT ( 'NONE',  ( 9.999999999999227285, 5.773502691896701400, -105.7500000040967620 ) ) ;
#37671 = LINE ( 'NONE', #21263, #4126 ) ;
#37673 = VERTEX_POINT ( 'NONE', #14342 ) ;
#37672 = CARTESIAN_POINT ( 'NONE',  ( 7.644554776091147741E-16, 12.48450537969573659, -86.65625000204838102 ) ) ;
#37675 = VERTEX_POINT ( 'NONE', #37890 ) ;
#37674 = DIRECTION ( 'NONE',  ( 1.000000000000000000, 0.000000000000000000, 0.000000000000000000 ) ) ;
#37676 = ORIENTED_EDGE ( 'NONE', *, *, #5844, .F. ) ;
#37677 = CARTESIAN_POINT ( 'NONE',  ( 10.81189881249999729, 6.242252689847867408, -38.71875000204835970 ) ) ;
#37678 = CARTESIAN_POINT ( 'NONE',  ( -2.293366432827344421E-15, -12.48450537969573659, -24.21875000204836326 ) ) ;
#37679 = CARTESIAN_POINT ( 'NONE',  ( -10.81189881249999907, -6.242252689847864744, -17.15625000204838102 ) ) ;
#37681 = ORIENTED_EDGE ( 'NONE', *, *, #17752, .F. ) ;
#37680 = CARTESIAN_POINT ( 'NONE',  ( -5.405949406250003975, -9.363379034771801557, -64.84375000204836681 ) ) ;
#37682 = CARTESIAN_POINT ( 'NONE',  ( 4.999999999999992006, -8.660254037844389075, -17.62500000409675138 ) ) ;
#37683 = CARTESIAN_POINT ( 'NONE',  ( -9.999999999999998224, 1.224646799147353059E-15, -32.74999999999997158 ) ) ;
#37684 = CARTESIAN_POINT ( 'NONE',  ( -5.405949406249996869, 9.363379034771805109, -188.3437500020483810 ) ) ;
#37685 = CARTESIAN_POINT ( 'NONE',  ( 10.81189881249999729, 0.000000000000000000, -166.3437500020484094 ) ) ;
#37686 = CARTESIAN_POINT ( 'NONE',  ( 10.81189881249999729, 6.242252689847867408, -176.7187500020484094 ) ) ;
#37687 = CARTESIAN_POINT ( 'NONE',  ( -9.999999999999998224, 1.224646799147353059E-15, -193.2500000000000000 ) ) ;
#37688 = ORGANIZATION ( 'NAUO-ORG6', 'UNSPECIFIED', 'UNSPECIFIED' ) ;
#37689 = CARTESIAN_POINT ( 'NONE',  ( 9.999999999999994671, -5.773502691896262640, -167.5000000040967905 ) ) ;
#37690 = CARTESIAN_POINT ( 'NONE',  ( 10.00000000000102318, -5.773502691895667560, -104.1249999999999432 ) ) ;
#37691 = CARTESIAN_POINT ( 'NONE',  ( 9.999999999999998224, 0.000000000000000000, -200.0000000000000000 ) ) ;
#37692 = CARTESIAN_POINT ( 'NONE',  ( 5.405949406249999534, 9.363379034771803333, -116.5937500020483810 ) ) ;
#37693 = CARTESIAN_POINT ( 'NONE',  ( 0.000000000000000000, 20.00000000000000000, -232.0000000000000000 ) ) ;
#37694 = CARTESIAN_POINT ( 'NONE',  ( 10.81189881249999729, 0.000000000000000000, -82.53125000204838102 ) ) ;
#37695 = CARTESIAN_POINT ( 'NONE',  ( -10.81189881249999729, -6.242252689847864744, -97.96875000204838102 ) ) ;
#37696 = EDGE_CURVE ( 'NONE', #2592, #24037, #24096, .T. ) ;
#37697 = CARTESIAN_POINT ( 'NONE',  ( -10.81189881249999729, 6.242252689847871849, -65.21875000204838102 ) ) ;
#37698 = CARTESIAN_POINT ( 'NONE',  ( -10.81189881249999907, -6.242252689847864744, -65.15625000204838102 ) ) ;
#37699 = CARTESIAN_POINT ( 'NONE',  ( -4.999999999999996447, 8.660254037844387298, -154.8750000040967905 ) ) ;
#37700 = CARTESIAN_POINT ( 'NONE',  ( 4.999999999999992006, -8.660254037844389075, -134.2499999999999716 ) ) ;
#37701 = CARTESIAN_POINT ( 'NONE',  ( 10.81189881249999729, 0.000000000000000000, -150.0312500020483810 ) ) ;
#37702 = CARTESIAN_POINT ( 'NONE',  ( 5.405949406249999534, 9.363379034771803333, -163.2812500020484094 ) ) ;
#37703 = FACE_OUTER_BOUND ( 'NONE', #6832, .T. ) ;
#37704 = DIRECTION ( 'NONE',  ( -1.000000000000000000, 0.000000000000000000, -0.000000000000000000 ) ) ;
#37705 = CARTESIAN_POINT ( 'NONE',  ( -10.81189881249999907, -6.242252689847864744, -99.46875000204838102 ) ) ;
#37706 = CARTESIAN_POINT ( 'NONE',  ( -10.00000000000102496, 5.773502691895664007, -62.87499999999994316 ) ) ;
#37707 = CARTESIAN_POINT ( 'NONE',  ( -10.00000000000000000, -5.773502691896251982, -76.12499999999997158 ) ) ;
#37708 = CARTESIAN_POINT ( 'NONE',  ( 10.81189881249999551, -6.242252689847874514, -194.9687500020484094 ) ) ;
#37709 = CARTESIAN_POINT ( 'NONE',  ( 4.999999999999992006, -8.660254037844389075, -79.12500000409677625 ) ) ;
#37710 = CARTESIAN_POINT ( 'NONE',  ( 11.54700538379253416, -19.99999999999999289, 49.99999999999998579 ) ) ;
#37711 = CARTESIAN_POINT ( 'NONE',  ( 10.81189881249999907, 6.242252689847868297, -91.40625000204836681 ) ) ;
#37712 = CARTESIAN_POINT ( 'NONE',  ( 7.644554776091147741E-16, 12.48450537969573659, -77.65625000204838102 ) ) ;
#37713 = CARTESIAN_POINT ( 'NONE',  ( 9.999999999999998224, 0.000000000000000000, -74.37500000409677625 ) ) ;
#37714 = CARTESIAN_POINT ( 'NONE',  ( -4.999999999999996447, 8.660254037844387298, -168.0000000000000000 ) ) ;
#37715 = CARTESIAN_POINT ( 'NONE',  ( -10.81189881249999729, 1.324075727343319199E-15, -29.09375000204836326 ) ) ;
#37716 = VERTEX_POINT ( 'NONE', #1217 ) ;
#37717 = CARTESIAN_POINT ( 'NONE',  ( -10.00000000000000000, -5.773502691896251982, -1.124999999999973355 ) ) ;
#37718 = CARTESIAN_POINT ( 'NONE',  ( -5.405949406250003975, -9.363379034771801557, -24.53125000204836681 ) ) ;
#37719 = CARTESIAN_POINT ( 'NONE',  ( -10.81189881249999729, -6.242252689847864744, -16.96875000204836681 ) ) ;
#37720 = DIRECTION ( 'NONE',  ( -0.000000000000000000, -0.000000000000000000, 1.000000000000000000 ) ) ;
#37721 = CARTESIAN_POINT ( 'NONE',  ( 5.000000000000000000, 8.660254037844385522, -8.125000004096744277 ) ) ;
#37722 = DIRECTION ( 'NONE',  ( 0.000000000000000000, 0.08715574274765837404, -0.9961946980917455452 ) ) ;
#37723 = CARTESIAN_POINT ( 'NONE',  ( 10.81189881249999907, 6.242252689847868297, -127.4062500020483810 ) ) ;
#37724 = CARTESIAN_POINT ( 'NONE',  ( -4.999999999999996447, 8.660254037844387298, -184.5000000000000000 ) ) ;
#37725 = CARTESIAN_POINT ( 'NONE',  ( 0.000000000000000000, 0.000000000000000000, -200.0000000000000000 ) ) ;
#37727 = ORIENTED_EDGE ( 'NONE', *, *, #10791, .F. ) ;
#37726 = CARTESIAN_POINT ( 'NONE',  ( 10.81189881249999729, 0.000000000000000000, -108.0312500020483810 ) ) ;
#37728 = CARTESIAN_POINT ( 'NONE',  ( -9.999999999999998224, 1.224646799147353059E-15, -138.1250000040967620 ) ) ;
#37729 = ORIENTED_EDGE ( 'NONE', *, *, #30982, .T. ) ;
#37730 = EDGE_LOOP ( 'NONE', ( #16134, #22076, #29658, #33968 ) ) ;
#37731 = CARTESIAN_POINT ( 'NONE',  ( 10.81189881249999551, -6.242252689847874514, -34.65625000204836681 ) ) ;
#37732 = COORDINATED_UNIVERSAL_TIME_OFFSET ( 6, 0, .AHEAD. ) ;
#37733 = CARTESIAN_POINT ( 'NONE',  ( -5.405949406250003975, -9.363379034771801557, -90.34375000204838102 ) ) ;
#37734 = CYLINDRICAL_SURFACE ( 'NONE', #33920, 9.999999999999998224 ) ;
#37735 = CARTESIAN_POINT ( 'NONE',  ( 9.999999999999998224, 0.000000000000000000, -128.3750000040967905 ) ) ;
#37736 =( BOUNDED_CURVE ( )  B_SPLINE_CURVE ( 2, ( #5937, #19085, #28822, #32271, #8749, #5509, #35084 ),
 .UNSPECIFIED., .F., .F. ) 
 B_SPLINE_CURVE_WITH_KNOTS ( ( 3, 2, 2, 3 ),
 ( 0.3059701492537313383, 0.3072139303482587791, 0.3084577114427861644, 0.3097014925373136052 ),
 .UNSPECIFIED. ) 
 CURVE ( )  GEOMETRIC_REPRESENTATION_ITEM ( )  RATIONAL_B_SPLINE_CURVE ( ( 1.000000000000000000, 0.8660254037844387076, 1.000000000000000000, 0.8660254037844387076, 1.000000000000000000, 0.8660254037844207220, 1.000000000000017986 ) ) 
 REPRESENTATION_ITEM ( '' )  );
#37737 = CARTESIAN_POINT ( 'NONE',  ( 7.070501591499376803E-16, 11.54700538379251284, -123.1249999999999858 ) ) ;
#37738 = CARTESIAN_POINT ( 'NONE',  ( 5.405949406249992428, -9.363379034771808662, -163.7812500020484094 ) ) ;
#37739 = CARTESIAN_POINT ( 'NONE',  ( 9.999999999999994671, -5.773502691896262640, -138.6250000000000000 ) ) ;
#37740 = CARTESIAN_POINT ( 'NONE',  ( -5.405949406250003975, -9.363379034771801557, -124.8437500020483810 ) ) ;
#37741 = CARTESIAN_POINT ( 'NONE',  ( -2.293366432827344421E-15, -12.48450537969573659, -84.21875000204835260 ) ) ;
#37742 = CARTESIAN_POINT ( 'NONE',  ( -9.999999999999998224, 1.224646799147353059E-15, -171.1250000040968189 ) ) ;
#37743 = CARTESIAN_POINT ( 'NONE',  ( -5.405949406249996869, 9.363379034771805109, -194.3437500020484094 ) ) ;
#37744 = CARTESIAN_POINT ( 'NONE',  ( 10.81189881249999907, 6.242252689847868297, -95.90625000204839523 ) ) ;
#37745 = CARTESIAN_POINT ( 'NONE',  ( -10.00000000000000000, -5.773502691896251982, -175.5000000040967905 ) ) ;
#37746 = CARTESIAN_POINT ( 'NONE',  ( 10.81189881249999551, -6.242252689847874514, -171.1562500020484094 ) ) ;
#37747 = CARTESIAN_POINT ( 'NONE',  ( -5.000000000000003553, -8.660254037844383745, -1.375000004096765815 ) ) ;
#37748 = CARTESIAN_POINT ( 'NONE',  ( -10.81189881249999729, 1.324075727343319199E-15, -173.2812500020484094 ) ) ;
#37749 = CARTESIAN_POINT ( 'NONE',  ( -10.81189881249999729, 6.242252689847871849, -189.9062500020484379 ) ) ;
#37750 = CARTESIAN_POINT ( 'NONE',  ( -10.81189881249999729, -6.242252689847864744, -51.46875000204837391 ) ) ;
#37751 = CARTESIAN_POINT ( 'NONE',  ( -9.999999999999998224, 1.224646799147353059E-15, -162.1250000040967905 ) ) ;
#37752 = CARTESIAN_POINT ( 'NONE',  ( -10.81189881249999729, 1.324075727343319199E-15, -11.28125000204835438 ) ) ;
#37753 = CARTESIAN_POINT ( 'NONE',  ( -5.405949406250003975, -9.363379034771801557, -10.84375000204834727 ) ) ;
#37754 = CARTESIAN_POINT ( 'NONE',  ( 5.405949406249992428, -9.363379034771808662, -126.0937500020483668 ) ) ;
#37755 = ADVANCED_FACE ( 'NONE', ( #27539 ), #17803, .F. ) ;
#37756 = CARTESIAN_POINT ( 'NONE',  ( -4.999999999999996447, 8.660254037844387298, -100.4999999999999858 ) ) ;
#37757 = CARTESIAN_POINT ( 'NONE',  ( -2.293366432827344421E-15, -12.48450537969573659, -19.90625000204837391 ) ) ;
#37758 = CARTESIAN_POINT ( 'NONE',  ( -5.000000000000003553, -8.660254037844383745, -104.8750000040967763 ) ) ;
#37759 = CARTESIAN_POINT ( 'NONE',  ( -5.000000000000003553, -8.660254037844383745, -136.3750000040967905 ) ) ;
#37760 = EDGE_CURVE ( 'NONE', #33065, #35463, #8114, .T. ) ;
#37761 = CARTESIAN_POINT ( 'NONE',  ( -9.999999999999998224, 5.773502691896259087, -55.37499999999998579 ) ) ;
#37762 = CARTESIAN_POINT ( 'NONE',  ( -2.293366432827344421E-15, -12.48450537969573659, -120.4062500020483952 ) ) ;
#37763 = CARTESIAN_POINT ( 'NONE',  ( 5.405949406249992428, -9.363379034771808662, -96.28125000204838102 ) ) ;
#37764 = EDGE_LOOP ( 'NONE', ( #33748, #1189, #20470, #9820 ) ) ;
#37765 = CARTESIAN_POINT ( 'NONE',  ( 9.999999999999998224, 0.000000000000000000, -96.87500000409677625 ) ) ;
#37766 = CARTESIAN_POINT ( 'NONE',  ( 4.999999999999992006, -8.660254037844389075, -166.1250000040967905 ) ) ;
#37767 = CARTESIAN_POINT ( 'NONE',  ( -5.405949406250003975, -9.363379034771801557, -167.0312500020484094 ) ) ;
#37768 = CARTESIAN_POINT ( 'NONE',  ( -2.293366432827344421E-15, -12.48450537969573659, -60.21875000204837391 ) ) ;
#37769 = ORIENTED_EDGE ( 'NONE', *, *, #37524, .T. ) ;
#37770 = CARTESIAN_POINT ( 'NONE',  ( -10.00000000000000000, -5.773502691896251982, -22.12499999999997868 ) ) ;
#37771 = AXIS2_PLACEMENT_3D ( 'NONE', #3719, #20738, #36930 ) ;
#37772 = CARTESIAN_POINT ( 'NONE',  ( -5.405949406250003975, -9.363379034771801557, -29.03125000204837036 ) ) ;
#37773 = CARTESIAN_POINT ( 'NONE',  ( -5.000000000000003553, -8.660254037844383745, -161.5000000000000000 ) ) ;
#37774 = CARTESIAN_POINT ( 'NONE',  ( 4.999999999999992006, -8.660254037844389075, -92.24999999999998579 ) ) ;
#37775 = CARTESIAN_POINT ( 'NONE',  ( 7.070501591499377789E-16, 11.54700538379251284, -27.50000000409677270 ) ) ;
#37776 = CARTESIAN_POINT ( 'NONE',  ( 0.000000000000000000, 0.000000000000000000, -200.0000000000000000 ) ) ;
#37777 = CARTESIAN_POINT ( 'NONE',  ( -5.405949406249996869, 9.363379034771805109, -131.5312500020484094 ) ) ;
#37778 = CARTESIAN_POINT ( 'NONE',  ( 1.915001621468759074, 10.12637373387462780, 1.028787474604546119E-14 ) ) ;
#37779 = CARTESIAN_POINT ( 'NONE',  ( -2.121150477449813534E-15, -11.54700538379251284, -188.3750000000000284 ) ) ;
#37780 = ORIENTED_EDGE ( 'NONE', *, *, #15145, .T. ) ;
#37781 = CARTESIAN_POINT ( 'NONE',  ( 10.81189881249999551, -6.242252689847874514, -61.65625000204838813 ) ) ;
#37782 = CALENDAR_DATE ( 2026, 28, 9 ) ;
#37784 = EDGE_LOOP ( 'NONE', ( #28406, #37569, #13121, #26526 ) ) ;
#37783 = ORIENTED_EDGE ( 'NONE', *, *, #10764, .T. ) ;
#37785 = CYLINDRICAL_SURFACE ( 'NONE', #9340, 9.999999999999998224 ) ;
#37786 = CARTESIAN_POINT ( 'NONE',  ( 9.999999999999998224, 0.000000000000000000, -54.87500000409675494 ) ) ;
#37787 = CARTESIAN_POINT ( 'NONE',  ( 10.81189881249999551, -6.242252689847874514, -158.9687500020484094 ) ) ;
#37788 = CARTESIAN_POINT ( 'NONE',  ( 10.81189881249999551, -6.242252689847874514, -187.6562500020484379 ) ) ;
#37789 = CARTESIAN_POINT ( 'NONE',  ( -10.81189881249999729, 1.324075727343319199E-15, -17.09375000204835260 ) ) ;
#37790 = CYLINDRICAL_SURFACE ( 'NONE', #6732, 9.999999999999998224 ) ;
#37791 = CARTESIAN_POINT ( 'NONE',  ( 10.81189881249999551, -6.242252689847874514, -148.4687500020484094 ) ) ;
#37792 = CARTESIAN_POINT ( 'NONE',  ( 10.81189881249999729, 0.000000000000000000, -125.8437500020483952 ) ) ;
#37793 = CARTESIAN_POINT ( 'NONE',  ( 10.81189881249999729, 0.000000000000000000, -103.5312500020483810 ) ) ;
#37794 = CARTESIAN_POINT ( 'NONE',  ( 10.81189881249999551, -6.242252689847874514, -112.4687500020483810 ) ) ;
#37795 = DIRECTION ( 'NONE',  ( -0.000000000000000000, -0.000000000000000000, 1.000000000000000000 ) ) ;
#37796 = CARTESIAN_POINT ( 'NONE',  ( -2.293366432827344421E-15, -12.48450537969573659, -112.9062500020483952 ) ) ;
#37797 = CARTESIAN_POINT ( 'NONE',  ( 7.644554776091147741E-16, 12.48450537969573659, -2.468750002048359704 ) ) ;
#37798 = CARTESIAN_POINT ( 'NONE',  ( -10.81189881249999729, 6.242252689847871849, -132.7187500020483810 ) ) ;
#37799 = CARTESIAN_POINT ( 'NONE',  ( 10.81189881249999729, 6.242252689847867408, -191.9062500020484094 ) ) ;
#37800 = CARTESIAN_POINT ( 'NONE',  ( 9.999999999999998224, 0.000000000000000000, -12.49999999999995559 ) ) ;
#37801 = CARTESIAN_POINT ( 'NONE',  ( 7.070501591499377789E-16, 11.54700538379251284, -147.1250000000000000 ) ) ;
#37802 = CARTESIAN_POINT ( 'NONE',  ( 9.999999999999998224, 0.000000000000000000, -19.99999999999996092 ) ) ;
#37803 = CARTESIAN_POINT ( 'NONE',  ( -5.405949406250003975, -9.363379034771801557, -79.84375000204838102 ) ) ;
#37804 = CARTESIAN_POINT ( 'NONE',  ( 5.405949406249992428, -9.363379034771808662, -54.09375000204835970 ) ) ;
#37805 = CARTESIAN_POINT ( 'NONE',  ( -5.000000000000003553, -8.660254037844383745, -116.8750000040967905 ) ) ;
#37806 = CARTESIAN_POINT ( 'NONE',  ( -10.81189881249999907, -6.242252689847864744, -35.15625000204837391 ) ) ;
#37807 = CARTESIAN_POINT ( 'NONE',  ( -5.405949406250003975, -9.363379034771801557, -45.34375000204838102 ) ) ;
#37808 = CARTESIAN_POINT ( 'NONE',  ( 10.00000000000000000, 5.773502691896255534, -136.8750000000000000 ) ) ;
#37809 = EDGE_CURVE ( 'NONE', #27414, #21209, #15205, .T. ) ;
#37810 = CARTESIAN_POINT ( 'NONE',  ( 5.405949406249992428, -9.363379034771808662, -145.5937500020483810 ) ) ;
#37811 = EDGE_CURVE ( 'NONE', #7087, #19666, #42169, .T. ) ;
#37812 = CARTESIAN_POINT ( 'NONE',  ( -2.121150477449813534E-15, -11.54700538379251284, -125.3749999999999858 ) ) ;
#37813 = EDGE_CURVE ( 'NONE', #22008, #23394, #1321, .T. ) ;
#37814 = CARTESIAN_POINT ( 'NONE',  ( 9.988285040850783503, 3.942477841776621084, -180.0000000000000568 ) ) ;
#37815 = CARTESIAN_POINT ( 'NONE',  ( 10.00000000000000000, 5.773502691896255534, -72.37499999999997158 ) ) ;
#37816 = CARTESIAN_POINT ( 'NONE',  ( 5.405949406249992428, -9.363379034771808662, -9.281250002048352599 ) ) ;
#37817 = EDGE_CURVE ( 'NONE', #5974, #38843, #27792, .T. ) ;
#37818 = ORIENTED_EDGE ( 'NONE', *, *, #35439, .T. ) ;
#37819 = CARTESIAN_POINT ( 'NONE',  ( -10.81189881249999729, -6.242252689847864744, -104.1562500020483952 ) ) ;
#37820 = CARTESIAN_POINT ( 'NONE',  ( -9.999999999999998224, 1.224646799147353059E-15, -123.1250000040967905 ) ) ;
#37821 = CARTESIAN_POINT ( 'NONE',  ( -9.999999999999998224, 1.224646799147353059E-15, -200.0000000000000000 ) ) ;
#37822 = CARTESIAN_POINT ( 'NONE',  ( -10.81189881249999907, -6.242252689847864744, -81.46875000204838102 ) ) ;
#37823 = CARTESIAN_POINT ( 'NONE',  ( 10.00000000000000000, 5.773502691896255534, -30.75000000409674428 ) ) ;
#37824 = CARTESIAN_POINT ( 'NONE',  ( 5.000000000000000000, 8.660254037844385522, -61.74999999999997158 ) ) ;
#37825 = CC_DESIGN_PERSON_AND_ORGANIZATION_ASSIGNMENT ( #2911, #16042, ( #20040 ) ) ;
#37826 = CARTESIAN_POINT ( 'NONE',  ( 10.81189881249999551, -6.242252689847874514, -45.15625000204836681 ) ) ;
#37827 = CARTESIAN_POINT ( 'NONE',  ( 0.000000000000000000, 0.000000000000000000, -200.0000000000000000 ) ) ;
#37828 = CARTESIAN_POINT ( 'NONE',  ( 10.81189881249999729, 0.000000000000000000, -142.5312500020483810 ) ) ;
#37829 = CARTESIAN_POINT ( 'NONE',  ( 7.644554776091147741E-16, 12.48450537969573659, -123.9687500020483952 ) ) ;
#37830 = CARTESIAN_POINT ( 'NONE',  ( -4.999999999999996447, 8.660254037844387298, -3.375000004096767370 ) ) ;
#37831 = AXIS2_PLACEMENT_3D ( 'NONE', #15291, #21130, #18536 ) ;
#37832 =( BOUNDED_CURVE ( )  B_SPLINE_CURVE ( 2, ( #6308, #23347, #36500, #266, #25950, #19454, #39098 ),
 .UNSPECIFIED., .F., .F. ) 
 B_SPLINE_CURVE_WITH_KNOTS ( ( 3, 2, 2, 3 ),
 ( 0.4440298507462688282, 0.4452736318407962135, 0.4465174129353234878, 0.4477611940298508730 ),
 .UNSPECIFIED. ) 
 CURVE ( )  GEOMETRIC_REPRESENTATION_ITEM ( )  RATIONAL_B_SPLINE_CURVE ( ( 0.9999999999999820144, 0.8660254037844566932, 1.000000000000000000, 0.8660254037844387076, 1.000000000000000000, 0.8660254037844267172, 1.000000000000011990 ) ) 
 REPRESENTATION_ITEM ( '' )  );
#37833 = LINE ( 'NONE', #17103, #25236 ) ;
#37834 = VERTEX_POINT ( 'NONE', #31860 ) ;
#37835 = EDGE_CURVE ( 'NONE', #36368, #14677, #10373, .T. ) ;
#37836 = ORIENTED_EDGE ( 'NONE', *, *, #28393, .F. ) ;
#37837 = ORIENTED_EDGE ( 'NONE', *, *, #31800, .T. ) ;
#37838 = CARTESIAN_POINT ( 'NONE',  ( 10.00000000000012257, -5.773502691896187144, -165.6250000000000000 ) ) ;
#37839 = CARTESIAN_POINT ( 'NONE',  ( 5.405949406249992428, -9.363379034771808662, -193.5937500020484094 ) ) ;
#37840 = CARTESIAN_POINT ( 'NONE',  ( -5.405949406249996869, 9.363379034771805109, -36.84375000204836681 ) ) ;
#37841 = CARTESIAN_POINT ( 'NONE',  ( 9.999999999999998224, 0.000000000000000000, -200.0000000000000000 ) ) ;
#37842 = CARTESIAN_POINT ( 'NONE',  ( 9.999999999999998224, 0.000000000000000000, -140.0000000000000000 ) ) ;
#37843 = CARTESIAN_POINT ( 'NONE',  ( 5.405949406249999534, 9.363379034771803333, -172.0937500020484094 ) ) ;
#37844 = CARTESIAN_POINT ( 'NONE',  ( -10.81189881249999907, -6.242252689847864744, -154.9687500020484094 ) ) ;
#37845 = EDGE_CURVE ( 'NONE', #25379, #37675, #25032, .T. ) ;
#37846 = CARTESIAN_POINT ( 'NONE',  ( -5.405949406249996869, 9.363379034771805109, -140.3437500020484094 ) ) ;
#37847 = CARTESIAN_POINT ( 'NONE',  ( -2.293366432827344421E-15, -12.48450537969573659, -150.4062500020483810 ) ) ;
#37848 = CARTESIAN_POINT ( 'NONE',  ( 10.81189881249999551, -6.242252689847874514, -155.9687500020484094 ) ) ;
#37849 = CARTESIAN_POINT ( 'NONE',  ( 9.999999999999998224, 0.000000000000000000, -165.8750000040967905 ) ) ;
#37850 = CARTESIAN_POINT ( 'NONE',  ( -4.999999999999996447, 8.660254037844387298, -70.49999999999998579 ) ) ;
#37851 = CARTESIAN_POINT ( 'NONE',  ( -2.121150477449813534E-15, -11.54700538379251284, -171.8750000000000284 ) ) ;
#37852 = CARTESIAN_POINT ( 'NONE',  ( 10.81189881249999551, -6.242252689847874514, -86.96875000204838102 ) ) ;
#37853 = CARTESIAN_POINT ( 'NONE',  ( 4.999999999999992006, -8.660254037844389075, -113.2499999999999858 ) ) ;
#37854 = CARTESIAN_POINT ( 'NONE',  ( -5.405949406250003975, -9.363379034771801557, -54.53125000204836681 ) ) ;
#37855 = CARTESIAN_POINT ( 'NONE',  ( -10.36423010611328799, -0.9417504169010495474, -99.99999999999998579 ) ) ;
#37856 = CARTESIAN_POINT ( 'NONE',  ( -10.81189881249999729, 1.324075727343319199E-15, -177.5937500020484094 ) ) ;
#37857 = CARTESIAN_POINT ( 'NONE',  ( -5.405949406249996869, 9.363379034771805109, -113.5312500020483952 ) ) ;
#37858 = CARTESIAN_POINT ( 'NONE',  ( -10.81189881249999729, 6.242252689847871849, -156.9062500020483526 ) ) ;
#37859 = CARTESIAN_POINT ( 'NONE',  ( 0.000000000000000000, 0.000000000000000000, -99.99999999999998579 ) ) ;
#37860 = CARTESIAN_POINT ( 'NONE',  ( 10.81189881249999729, 0.000000000000000000, -42.03125000204838102 ) ) ;
#37861 = CARTESIAN_POINT ( 'NONE',  ( -4.999999999999996447, 8.660254037844387298, -129.3750000040967905 ) ) ;
#37862 = CARTESIAN_POINT ( 'NONE',  ( 4.999999999999992006, -8.660254037844389075, -99.74999999999998579 ) ) ;
#37863 = ORIENTED_EDGE ( 'NONE', *, *, #15782, .F. ) ;
#37864 = CARTESIAN_POINT ( 'NONE',  ( -2.293366432827344421E-15, -12.48450537969573659, -123.4062500020483952 ) ) ;
#37865 = CARTESIAN_POINT ( 'NONE',  ( -10.00000000000000000, -5.773502691896251982, -151.5000000040967905 ) ) ;
#37866 = VECTOR ( 'NONE', #8988, 1000.000000000000000 ) ;
#37867 = CARTESIAN_POINT ( 'NONE',  ( 5.405949406249992428, -9.363379034771808662, -178.7812500020484094 ) ) ;
#37868 = EDGE_LOOP ( 'NONE', ( #25111, #22926, #28165, #28561 ) ) ;
#37869 = CARTESIAN_POINT ( 'NONE',  ( 7.644554776091147741E-16, 12.48450537969573659, -174.9687500020484094 ) ) ;
#37870 = CARTESIAN_POINT ( 'NONE',  ( 5.000000000000000000, 8.660254037844385522, -60.62500000409676204 ) ) ;
#37871 = LINE ( 'NONE', #30983, #21710 ) ;
#37872 = FACE_OUTER_BOUND ( 'NONE', #16946, .T. ) ;
#37873 = CARTESIAN_POINT ( 'NONE',  ( 5.405949406249999534, 9.363379034771803333, -68.78125000204838102 ) ) ;
#37874 = CARTESIAN_POINT ( 'NONE',  ( -10.81189881249999729, -6.242252689847864744, -53.15625000204838102 ) ) ;
#37875 =( BOUNDED_CURVE ( )  B_SPLINE_CURVE ( 2, ( #16104, #15273, #25439, #25646, #5792, #15893, #32344 ),
 .UNSPECIFIED., .F., .F. ) 
 B_SPLINE_CURVE_WITH_KNOTS ( ( 3, 2, 2, 3 ),
 ( 0.3395522388059703522, 0.3407960199004976820, 0.3420398009950250118, 0.3432835820895522860 ),
 .UNSPECIFIED. ) 
 CURVE ( )  GEOMETRIC_REPRESENTATION_ITEM ( )  RATIONAL_B_SPLINE_CURVE ( ( 0.9999999999999761302, 0.8660254037844625774, 1.000000000000000000, 0.8660254037844387076, 1.000000000000000000, 0.8660254037844327124, 1.000000000000005995 ) ) 
 REPRESENTATION_ITEM ( '' )  );
#37876 = CARTESIAN_POINT ( 'NONE',  ( -5.000000000000003553, -8.660254037844383745, -47.87500000409677625 ) ) ;
#37877 = AXIS2_PLACEMENT_3D ( 'NONE', #15908, #4840, #27722 ) ;
#37878 = CARTESIAN_POINT ( 'NONE',  ( -10.81189881249999729, 6.242252689847871849, -5.218750002048355263 ) ) ;
#37879 = CARTESIAN_POINT ( 'NONE',  ( 9.999999999999998224, 0.000000000000000000, -88.99999999999998579 ) ) ;
#37880 = CARTESIAN_POINT ( 'NONE',  ( -2.293366432827344421E-15, -12.48450537969573659, -175.9062500020483810 ) ) ;
#37881 = EDGE_CURVE ( 'NONE', #7438, #38628, #40994, .T. ) ;
#37882 = CARTESIAN_POINT ( 'NONE',  ( 5.000000000000000000, 8.660254037844385522, -198.2500000000000000 ) ) ;
#37883 = ORIENTED_EDGE ( 'NONE', *, *, #39352, .T. ) ;
#37884 = CARTESIAN_POINT ( 'NONE',  ( 5.000000000000000000, 8.660254037844385522, -84.62500000409677625 ) ) ;
#37885 = FACE_OUTER_BOUND ( 'NONE', #2652, .T. ) ;
#37886 = CARTESIAN_POINT ( 'NONE',  ( -2.121150477449813534E-15, -11.54700538379251284, -20.37499999999996803 ) ) ;
#37888 = ORIENTED_EDGE ( 'NONE', *, *, #9191, .F. ) ;
#37887 = CARTESIAN_POINT ( 'NONE',  ( -5.405949406250003975, -9.363379034771801557, -75.53125000204838102 ) ) ;
#37889 = DIRECTION ( 'NONE',  ( 1.000000000000000000, 0.000000000000000000, 0.000000000000000000 ) ) ;
#37891 = ORIENTED_EDGE ( 'NONE', *, *, #14409, .T. ) ;
#37890 = CARTESIAN_POINT ( 'NONE',  ( -9.999999999999998224, 1.224646799147353059E-15, -29.74999999999997158 ) ) ;
#37892 = EDGE_LOOP ( 'NONE', ( #7847, #18118, #15149, #31324 ) ) ;
#37893 = CARTESIAN_POINT ( 'NONE',  ( -5.405949406250003975, -9.363379034771801557, -40.84375000204837391 ) ) ;
#37894 = DIRECTION ( 'NONE',  ( 0.000000000000000000, 0.000000000000000000, 1.000000000000000000 ) ) ;
#37895 = CARTESIAN_POINT ( 'NONE',  ( 7.644554776091147741E-16, 12.48450537969573659, -14.65625000204836859 ) ) ;
#37896 = VECTOR ( 'NONE', #18177, 1000.000000000000000 ) ;
#37898 = VERTEX_POINT ( 'NONE', #2292 ) ;
#37897 = CARTESIAN_POINT ( 'NONE',  ( 10.81189881249999729, 0.000000000000000000, -59.84375000204835970 ) ) ;
#37899 = CYLINDRICAL_SURFACE ( 'NONE', #33249, 9.999999999999998224 ) ;
#37900 = CARTESIAN_POINT ( 'NONE',  ( 5.000000000000000000, 8.660254037844385522, -34.74999999999997868 ) ) ;
#37901 = CARTESIAN_POINT ( 'NONE',  ( -10.81189881249999729, -6.242252689847864744, -192.4687500020484094 ) ) ;
#37902 = CARTESIAN_POINT ( 'NONE',  ( 10.81189881249999907, 6.242252689847868297, -173.7187500020484094 ) ) ;
#37903 = CARTESIAN_POINT ( 'NONE',  ( -10.81189881249999907, -6.242252689847864744, -168.4687500020483526 ) ) ;
#37904 = CARTESIAN_POINT ( 'NONE',  ( 10.81189881249999729, 6.242252689847867408, -178.2187500020484094 ) ) ;
#37905 = CARTESIAN_POINT ( 'NONE',  ( -9.999999999999834799, -5.773502691896343464, -193.1250000000000000 ) ) ;
#37906 = DIRECTION ( 'NONE',  ( -0.000000000000000000, -0.000000000000000000, -1.000000000000000000 ) ) ;
#37907 = CARTESIAN_POINT ( 'NONE',  ( -10.00000000000000000, -5.773502691896251982, -199.1250000000000284 ) ) ;
#37908 = CARTESIAN_POINT ( 'NONE',  ( -10.81189881249999907, -6.242252689847864744, -109.9687500020483668 ) ) ;
#37909 = CARTESIAN_POINT ( 'NONE',  ( -9.999999999999998224, 1.224646799147353059E-15, -87.12500000409677625 ) ) ;
#37910 = CARTESIAN_POINT ( 'NONE',  ( -5.405949406249996869, 9.363379034771805109, -83.53125000204838102 ) ) ;
#37911 = CARTESIAN_POINT ( 'NONE',  ( 10.81189881249999551, -6.242252689847874514, -92.96875000204838102 ) ) ;
#37912 = CARTESIAN_POINT ( 'NONE',  ( -10.81189881249999729, 6.242252689847871849, -60.71875000204838102 ) ) ;
#37913 = CARTESIAN_POINT ( 'NONE',  ( -5.405949406250003975, -9.363379034771801557, -72.53125000204838102 ) ) ;
#37914 = CARTESIAN_POINT ( 'NONE',  ( -4.999999999999996447, 8.660254037844387298, -157.8750000040967905 ) ) ;
#37915 = CARTESIAN_POINT ( 'NONE',  ( -5.000000000000003553, -8.660254037844383745, -121.0000000000000000 ) ) ;
#37916 = CARTESIAN_POINT ( 'NONE',  ( -10.81189881249999729, 6.242252689847871849, -150.9062500020484094 ) ) ;
#37917 = CARTESIAN_POINT ( 'NONE',  ( 10.81189881249999729, 0.000000000000000000, -162.0312500020484094 ) ) ;
#37918 = CARTESIAN_POINT ( 'NONE',  ( -5.000000000000003553, -8.660254037844383745, -13.37500000409674783 ) ) ;
#37919 = DIRECTION ( 'NONE',  ( -0.000000000000000000, -0.000000000000000000, 1.000000000000000000 ) ) ;
#37920 = CARTESIAN_POINT ( 'NONE',  ( 10.81189881249999907, 6.242252689847868297, -94.21875000204838102 ) ) ;
#37921 = ORIENTED_EDGE ( 'NONE', *, *, #31149, .T. ) ;
#37922 = CARTESIAN_POINT ( 'NONE',  ( -2.121150477449813534E-15, -11.54700538379251284, -77.37499999999997158 ) ) ;
#37923 = CARTESIAN_POINT ( 'NONE',  ( -5.405949406250003975, -9.363379034771801557, -198.3437500020484094 ) ) ;
#37924 = CARTESIAN_POINT ( 'NONE',  ( 9.999999999999998224, 0.000000000000000000, -84.87500000409677625 ) ) ;
#37925 = CARTESIAN_POINT ( 'NONE',  ( -5.604939563500185962, -8.526197496611898075, -180.0000000000000000 ) ) ;
#37926 = CARTESIAN_POINT ( 'NONE',  ( -5.405949406250003975, -9.363379034771801557, -90.53125000204838102 ) ) ;
#37927 = CARTESIAN_POINT ( 'NONE',  ( -10.81189881249999729, 1.324075727343319199E-15, -72.78125000204838102 ) ) ;
#37928 = CARTESIAN_POINT ( 'NONE',  ( -5.000000000000003553, -8.660254037844383745, -71.87500000409677625 ) ) ;
#37929 = CARTESIAN_POINT ( 'NONE',  ( 10.00000000000102318, -5.773502691895667560, -59.12499999999996447 ) ) ;
#37930 = CARTESIAN_POINT ( 'NONE',  ( -10.81189881249999729, 6.242252689847871849, -29.21875000204834905 ) ) ;
#37931 = ORIENTED_EDGE ( 'NONE', *, *, #4965, .T. ) ;
#37932 = CARTESIAN_POINT ( 'NONE',  ( -2.121150477449813534E-15, -11.54700538379251284, -0.8749999999999721334 ) ) ;
#37933 = EDGE_CURVE ( 'NONE', #39083, #342, #42639, .T. ) ;
#37934 = CARTESIAN_POINT ( 'NONE',  ( -2.293366432827344421E-15, -12.48450537969573659, -21.40625000204837747 ) ) ;
#37935 = CARTESIAN_POINT ( 'NONE',  ( -10.81189881249999729, -6.242252689847864744, -10.96875000204836859 ) ) ;
#37936 = CARTESIAN_POINT ( 'NONE',  ( -9.999999999999998224, 1.224646799147353059E-15, -118.6250000040967905 ) ) ;
#37937 = CARTESIAN_POINT ( 'NONE',  ( -10.81189881249999729, 6.242252689847871849, -143.2187500020484094 ) ) ;
#37938 = CARTESIAN_POINT ( 'NONE',  ( -9.999999999999998224, 1.224646799147353059E-15, -0.1250000040967647053 ) ) ;
#37939 = CARTESIAN_POINT ( 'NONE',  ( -9.999999999999998224, 1.224646799147353059E-15, -151.6250000040967905 ) ) ;
#37940 = CARTESIAN_POINT ( 'NONE',  ( 10.81189881249999551, -6.242252689847874514, -132.1562500020484094 ) ) ;
#37941 = CARTESIAN_POINT ( 'NONE',  ( -10.00000000000000000, -5.773502691896251982, -185.6250000000000284 ) ) ;
#37942 = CYLINDRICAL_SURFACE ( 'NONE', #18610, 9.999999999999998224 ) ;
#37944 = VERTEX_POINT ( 'NONE', #41746 ) ;
#37943 = CARTESIAN_POINT ( 'NONE',  ( 10.81189881249999907, 6.242252689847868297, -107.9062500020483668 ) ) ;
#37945 = CARTESIAN_POINT ( 'NONE',  ( 0.000000000000000000, 0.000000000000000000, -200.0000000000000000 ) ) ;
#37946 = ORIENTED_EDGE ( 'NONE', *, *, #18751, .T. ) ;
#37947 = ORIENTED_EDGE ( 'NONE', *, *, #16683, .F. ) ;
#37948 = EDGE_CURVE ( 'NONE', #22601, #36180, #36599, .T. ) ;
#37949 = CARTESIAN_POINT ( 'NONE',  ( 5.405949406249992428, -9.363379034771808662, -40.78125000204838102 ) ) ;
#37950 = APPROVAL_DATE_TIME ( #21545, #40954 ) ;
#37951 = CARTESIAN_POINT ( 'NONE',  ( 5.405949406249992428, -9.363379034771808662, -84.09375000204836681 ) ) ;
#37952 = FACE_OUTER_BOUND ( 'NONE', #33544, .T. ) ;
#37953 = CARTESIAN_POINT ( 'NONE',  ( 42.00000000000001421, 5.327213576290987622E-15, -200.0000000000000000 ) ) ;
#37954 = CARTESIAN_POINT ( 'NONE',  ( -10.81189881249999907, -6.242252689847864744, -167.1562500020483810 ) ) ;
#37955 = CARTESIAN_POINT ( 'NONE',  ( 4.999999999999992006, -8.660254037844389075, -86.24999999999998579 ) ) ;
#37956 = VECTOR ( 'NONE', #33860, 1000.000000000000000 ) ;
#37957 = VECTOR ( 'NONE', #10624, 1000.000000000000000 ) ;
#37958 = CARTESIAN_POINT ( 'NONE',  ( 10.81189881249999551, -6.242252689847874514, -118.4687500020483810 ) ) ;
#37959 = CARTESIAN_POINT ( 'NONE',  ( -10.81189881249999729, 6.242252689847871849, -89.21875000204836681 ) ) ;
#37960 = CARTESIAN_POINT ( 'NONE',  ( -5.405949406249996869, 9.363379034771805109, -5.531250002048376579 ) ) ;
#37961 = CARTESIAN_POINT ( 'NONE',  ( 5.405949406249992428, -9.363379034771808662, -192.0937500020484094 ) ) ;
#37962 = CARTESIAN_POINT ( 'NONE',  ( -5.405949406249996869, 9.363379034771805109, -92.53125000204838102 ) ) ;
#37963 = CARTESIAN_POINT ( 'NONE',  ( 7.070501591499377789E-16, 11.54700538379251284, -179.0000000040967905 ) ) ;
#37964 = CARTESIAN_POINT ( 'NONE',  ( 5.405949406249992428, -9.363379034771808662, -169.7812500020484094 ) ) ;
#37965 = CARTESIAN_POINT ( 'NONE',  ( -2.121150477449813534E-15, -11.54700538379251284, -150.8750000000000000 ) ) ;
#37966 = CARTESIAN_POINT ( 'NONE',  ( 7.644554776091147741E-16, 12.48450537969573659, -173.6562500020483810 ) ) ;
#37967 = CARTESIAN_POINT ( 'NONE',  ( -2.293366432827344421E-15, -12.48450537969573659, -190.9062500020483810 ) ) ;
#37968 = CARTESIAN_POINT ( 'NONE',  ( 10.81189881249999729, 6.242252689847867408, -55.21875000204836681 ) ) ;
#37969 = EDGE_CURVE ( 'NONE', #24099, #1756, #33845, .T. ) ;
#37970 = CARTESIAN_POINT ( 'NONE',  ( -4.999999999999996447, 8.660254037844387298, -162.3750000040967905 ) ) ;
#37971 = CARTESIAN_POINT ( 'NONE',  ( -10.81189881249999729, 1.324075727343319199E-15, -5.281250002048376579 ) ) ;
#37972 = CARTESIAN_POINT ( 'NONE',  ( 10.81189881249999729, 0.000000000000000000, -10.34375000204834549 ) ) ;
#37973 = CARTESIAN_POINT ( 'NONE',  ( 9.999999999999998224, 0.000000000000000000, -122.3750000040967905 ) ) ;
#37974 = CARTESIAN_POINT ( 'NONE',  ( 10.81189881249999551, -6.242252689847874514, -121.4687500020484094 ) ) ;
#37975 = CARTESIAN_POINT ( 'NONE',  ( -5.000000000000003553, -8.660254037844383745, -101.5000000000000000 ) ) ;
#37976 = CARTESIAN_POINT ( 'NONE',  ( 10.81189881249999551, -6.242252689847874514, -21.15625000204837391 ) ) ;
#37977 = CARTESIAN_POINT ( 'NONE',  ( 4.999999999999992006, -8.660254037844389075, -103.1250000040967763 ) ) ;
#37978 = CARTESIAN_POINT ( 'NONE',  ( -9.999999999999998224, 1.224646799147353059E-15, -50.74999999999996447 ) ) ;
#37979 = CARTESIAN_POINT ( 'NONE',  ( -5.405949406249996869, 9.363379034771805109, -119.5312500020483952 ) ) ;
#37980 = CARTESIAN_POINT ( 'NONE',  ( -5.405949406250003975, -9.363379034771801557, -98.03125000204839523 ) ) ;
#37981 = ORIENTED_EDGE ( 'NONE', *, *, #26060, .F. ) ;
#37982 = EDGE_CURVE ( 'NONE', #36710, #1760, #26466, .T. ) ;
#37983 = CARTESIAN_POINT ( 'NONE',  ( -9.999999999999998224, 1.224646799147353059E-15, -96.12500000409677625 ) ) ;
#37984 = FACE_OUTER_BOUND ( 'NONE', #19323, .T. ) ;
#37985 = CARTESIAN_POINT ( 'NONE',  ( -2.293366432827344421E-15, -12.48450537969573659, -157.9062500020483810 ) ) ;
#37986 = CARTESIAN_POINT ( 'NONE',  ( 10.81189881249999729, 0.000000000000000000, -46.34375000204838102 ) ) ;
#37987 = VERTEX_POINT ( 'NONE', #36596 ) ;
#37988 = CARTESIAN_POINT ( 'NONE',  ( -5.000000000000003553, -8.660254037844383745, -29.49999999999997158 ) ) ;
#37989 = CARTESIAN_POINT ( 'NONE',  ( -10.81189881249999729, -6.242252689847864744, -30.65625000204835260 ) ) ;
#37990 = CARTESIAN_POINT ( 'NONE',  ( -9.999999999999998224, 1.224646799147353059E-15, -161.7500000000000000 ) ) ;
#37991 = CARTESIAN_POINT ( 'NONE',  ( -9.999999999999479527, -5.773502691896549521, -103.1249999999999858 ) ) ;
#37992 = CARTESIAN_POINT ( 'NONE',  ( -2.121150477449813534E-15, -11.54700538379251284, -25.25000000409676915 ) ) ;
#37993 = DIRECTION ( 'NONE',  ( -0.000000000000000000, -0.000000000000000000, 1.000000000000000000 ) ) ;
#37994 = CARTESIAN_POINT ( 'NONE',  ( 10.81189881249999907, 6.242252689847868297, -137.9062500020483810 ) ) ;
#37995 = CARTESIAN_POINT ( 'NONE',  ( 10.55761814654026232, 2.340415281005872039, -2.775557561562896400E-14 ) ) ;
#37996 = CARTESIAN_POINT ( 'NONE',  ( 10.00000000000025402, -5.773502691896113426, -188.1250000000000284 ) ) ;
#37997 = VERTEX_POINT ( 'NONE', #23875 ) ;
#37998 =( BOUNDED_CURVE ( )  B_SPLINE_CURVE ( 2, ( #41775, #15446, #8145, #1458, #21293, #11567, #8364 ),
 .UNSPECIFIED., .F., .F. ) 
 B_SPLINE_CURVE_WITH_KNOTS ( ( 3, 2, 2, 3 ),
 ( 0.1231343283582089221, 0.1243781094527362935, 0.1256218905472636649, 0.1268656716417910224 ),
 .UNSPECIFIED. ) 
 CURVE ( )  GEOMETRIC_REPRESENTATION_ITEM ( )  RATIONAL_B_SPLINE_CURVE ( ( 1.000000000000002887, 0.8660254037844355990, 1.000000000000000000, 0.8660254037844387076, 1.000000000000000000, 0.8660254037844417052, 0.9999999999999970024 ) ) 
 REPRESENTATION_ITEM ( '' )  );
#37999 = CARTESIAN_POINT ( 'NONE',  ( 5.405949406249999534, 9.363379034771803333, -64.28125000204836681 ) ) ;
#38000 = CALENDAR_DATE ( 2026, 28, 9 ) ;
#38001 = ADVANCED_FACE ( 'NONE', ( #29712 ), #39828, .F. ) ;
#38003 = ORIENTED_EDGE ( 'NONE', *, *, #20808, .T. ) ;
#38002 = ORIENTED_EDGE ( 'NONE', *, *, #32327, .F. ) ;
#38004 = CARTESIAN_POINT ( 'NONE',  ( 0.000000000000000000, 0.000000000000000000, -99.99999999999998579 ) ) ;
#38005 = FACE_OUTER_BOUND ( 'NONE', #18886, .T. ) ;
#38006 = CARTESIAN_POINT ( 'NONE',  ( 7.644554776091147741E-16, 12.48450537969573659, -158.4687500020483810 ) ) ;
#38007 = CARTESIAN_POINT ( 'NONE',  ( -10.81189881249999907, -6.242252689847864744, -189.6562500020484094 ) ) ;
#38008 = CARTESIAN_POINT ( 'NONE',  ( -10.81189881249999729, 6.242252689847871849, -6.718750002048347270 ) ) ;
#38009 = CARTESIAN_POINT ( 'NONE',  ( -5.405949406250003975, -9.363379034771801557, -145.8437500020483810 ) ) ;
#38010 = CARTESIAN_POINT ( 'NONE',  ( -5.405949406250003975, -9.363379034771801557, -95.03125000204838102 ) ) ;
#38011 = CARTESIAN_POINT ( 'NONE',  ( 10.81189881249999907, 6.242252689847868297, -113.7187500020483810 ) ) ;
#38012 = DIRECTION ( 'NONE',  ( 1.000000000000000000, 0.000000000000000000, 0.000000000000000000 ) ) ;
#38013 = CARTESIAN_POINT ( 'NONE',  ( -5.405949406249996869, 9.363379034771805109, -118.0312500020483952 ) ) ;
#38014 = CARTESIAN_POINT ( 'NONE',  ( 7.644554776091147741E-16, 12.48450537969573659, -5.468750002048341941 ) ) ;
#38015 = CARTESIAN_POINT ( 'NONE',  ( 10.81189881249999729, 0.000000000000000000, -124.3437500020483952 ) ) ;
#38016 = CIRCLE ( 'NONE', #28350, 9.999999999999998224 ) ;
#38017 = CARTESIAN_POINT ( 'NONE',  ( -10.81189881249999729, -6.242252689847864744, -191.1562500020484094 ) ) ;
#38018 = CARTESIAN_POINT ( 'NONE',  ( 9.999999999999998224, 0.000000000000000000, -165.8750000040967905 ) ) ;
#38019 = CARTESIAN_POINT ( 'NONE',  ( -5.000000000000003553, -8.660254037844383745, -145.0000000000000000 ) ) ;
#38020 = CARTESIAN_POINT ( 'NONE',  ( 10.00000000000000000, 5.773502691896255534, -10.87499999999996625 ) ) ;
#38021 = LOCAL_TIME ( 11, 57, 6.000000000000000000, #22872 ) ;
#38022 = CARTESIAN_POINT ( 'NONE',  ( -5.405949406250003975, -9.363379034771801557, -73.84375000204838102 ) ) ;
#38023 = CARTESIAN_POINT ( 'NONE',  ( -5.405949406249996869, 9.363379034771805109, -57.84375000204835970 ) ) ;
#38024 = CARTESIAN_POINT ( 'NONE',  ( 10.00000000000000000, 5.773502691896255534, -191.2500000040968189 ) ) ;
#38025 = CARTESIAN_POINT ( 'NONE',  ( -10.81189881249999729, 6.242252689847871849, -30.90625000204834905 ) ) ;
#38026 = CARTESIAN_POINT ( 'NONE',  ( 10.81189881249999907, 6.242252689847868297, -34.21875000204835260 ) ) ;
#38027 = FACE_OUTER_BOUND ( 'NONE', #19881, .T. ) ;
#38028 = CARTESIAN_POINT ( 'NONE',  ( 7.644554776091147741E-16, 12.48450537969573659, -147.9687500020484094 ) ) ;
#38029 = CARTESIAN_POINT ( 'NONE',  ( -9.999999999999998224, 1.224646799147353059E-15, -121.2500000000000000 ) ) ;
#38030 = CARTESIAN_POINT ( 'NONE',  ( -9.999999999999998224, 1.224646799147353059E-15, -71.74999999999998579 ) ) ;
#38031 = CARTESIAN_POINT ( 'NONE',  ( 10.81189881249999729, 0.000000000000000000, -144.0312500020483810 ) ) ;
#38032 = CARTESIAN_POINT ( 'NONE',  ( -10.81189881249999729, -6.242252689847864744, -12.65625000204835970 ) ) ;
#38033 = ORIENTED_EDGE ( 'NONE', *, *, #23486, .F. ) ;
#38034 = CARTESIAN_POINT ( 'NONE',  ( -10.81189881249999729, 6.242252689847871849, -104.4062500020483810 ) ) ;
#38035 = CARTESIAN_POINT ( 'NONE',  ( -10.00000000000000000, -5.773502691896251982, -114.0000000040967905 ) ) ;
#38036 = DIRECTION ( 'NONE',  ( -0.000000000000000000, -0.000000000000000000, 1.000000000000000000 ) ) ;
#38037 = CARTESIAN_POINT ( 'NONE',  ( 10.81189881249999729, 0.000000000000000000, -71.84375000204836681 ) ) ;
#38038 = AXIS2_PLACEMENT_3D ( 'NONE', #10376, #33921, #30475 ) ;
#38039 = CARTESIAN_POINT ( 'NONE',  ( 5.000000000000000000, 8.660254037844385522, -24.62500000409675849 ) ) ;
#38040 = CARTESIAN_POINT ( 'NONE',  ( -2.121150477449813534E-15, -11.54700538379251284, -14.37499999999997335 ) ) ;
#38041 = CARTESIAN_POINT ( 'NONE',  ( -2.293366432827344421E-15, -12.48450537969573659, -42.40625000204836681 ) ) ;
#38042 = DIRECTION ( 'NONE',  ( -0.000000000000000000, -0.000000000000000000, 1.000000000000000000 ) ) ;
#38043 = CARTESIAN_POINT ( 'NONE',  ( 10.81189881249999729, 0.000000000000000000, -147.0312500020483810 ) ) ;
#38044 = CARTESIAN_POINT ( 'NONE',  ( 5.405949406249992428, -9.363379034771808662, -129.0937500020483810 ) ) ;
#38045 = CARTESIAN_POINT ( 'NONE',  ( -4.999999999999996447, 8.660254037844387298, -50.99999999999996447 ) ) ;
#38046 = CARTESIAN_POINT ( 'NONE',  ( -9.999999999999227285, -5.773502691896698735, -127.5000000040967763 ) ) ;
#38047 = ORIENTED_EDGE ( 'NONE', *, *, #29337, .T. ) ;
#38048 = EDGE_LOOP ( 'NONE', ( #18384, #9223, #12593, #39813 ) ) ;
#38049 = EDGE_CURVE ( 'NONE', #5023, #26528, #29184, .T. ) ;
#38050 = ORIENTED_EDGE ( 'NONE', *, *, #4231, .F. ) ;
#38051 = EDGE_CURVE ( 'NONE', #23180, #26892, #30569, .T. ) ;
#38052 = LINE ( 'NONE', #21645, #9766 ) ;
#38053 = CARTESIAN_POINT ( 'NONE',  ( -10.81189881249999729, 1.324075727343319199E-15, -180.5937500020484094 ) ) ;
#38054 = CARTESIAN_POINT ( 'NONE',  ( 10.81189881249999729, 0.000000000000000000, -32.84375000204836681 ) ) ;
#38055 = DIRECTION ( 'NONE',  ( -0.000000000000000000, -0.000000000000000000, 1.000000000000000000 ) ) ;
#38056 = CARTESIAN_POINT ( 'NONE',  ( -5.405949406249996869, 9.363379034771805109, -171.8437500020484094 ) ) ;
#38057 = CARTESIAN_POINT ( 'NONE',  ( -10.81189881249999729, 6.242252689847871849, -152.2187500020483526 ) ) ;
#38058 = CARTESIAN_POINT ( 'NONE',  ( 5.405949406249992428, -9.363379034771808662, -130.5937500020483810 ) ) ;
#38059 = CARTESIAN_POINT ( 'NONE',  ( -10.81189881249999729, 1.324075727343319199E-15, -141.7812500020483810 ) ) ;
#38060 = CARTESIAN_POINT ( 'NONE',  ( -10.81189881249999729, -6.242252689847864744, -156.4687500020484094 ) ) ;
#38061 = DIRECTION ( 'NONE',  ( -0.000000000000000000, -0.000000000000000000, 1.000000000000000000 ) ) ;
#38062 = CARTESIAN_POINT ( 'NONE',  ( 9.999999999999998224, 0.000000000000000000, -183.5000000000000000 ) ) ;
#38063 = CARTESIAN_POINT ( 'NONE',  ( -10.00000000000000000, -5.773502691896251982, -175.1249999999999716 ) ) ;
#38064 = CARTESIAN_POINT ( 'NONE',  ( 7.644554776091147741E-16, 12.48450537969573659, -78.96875000204839523 ) ) ;
#38065 = CARTESIAN_POINT ( 'NONE',  ( 0.000000000000000000, 0.000000000000000000, -200.0000000000000000 ) ) ;
#38066 = CARTESIAN_POINT ( 'NONE',  ( 10.81189881249999551, -6.242252689847874514, -58.65625000204838813 ) ) ;
#38067 = CARTESIAN_POINT ( 'NONE',  ( -10.12150904654152761, -2.198084950377523050, -100.0000000000000142 ) ) ;
#38068 = CARTESIAN_POINT ( 'NONE',  ( 7.644554776091147741E-16, 12.48450537969573659, -170.4687500020483810 ) ) ;
#38069 = EDGE_CURVE ( 'NONE', #23937, #38155, #29495, .T. ) ;
#38070 = CARTESIAN_POINT ( 'NONE',  ( -5.405949406250003975, -9.363379034771801557, -117.5312500020483952 ) ) ;
#38071 = CARTESIAN_POINT ( 'NONE',  ( -10.81189881249999729, -6.242252689847864744, -147.6562500020483810 ) ) ;
#38072 = CYLINDRICAL_SURFACE ( 'NONE', #3433, 9.999999999999998224 ) ;
#38073 = CARTESIAN_POINT ( 'NONE',  ( -10.81189881249999729, 6.242252689847871849, -45.90625000204836681 ) ) ;
#38074 = CARTESIAN_POINT ( 'NONE',  ( -5.000000000000003553, -8.660254037844383745, -118.3750000040967905 ) ) ;
#38075 = CARTESIAN_POINT ( 'NONE',  ( 4.999999999999992006, -8.660254037844389075, -96.74999999999998579 ) ) ;
#38076 = ORIENTED_EDGE ( 'NONE', *, *, #20022, .F. ) ;
#38077 = CARTESIAN_POINT ( 'NONE',  ( 5.405949406249992428, -9.363379034771808662, -123.2812500020483952 ) ) ;
#38078 = CARTESIAN_POINT ( 'NONE',  ( 9.999999999999996447, -5.773502691896262640, -148.0000000040968189 ) ) ;
#38079 = CARTESIAN_POINT ( 'NONE',  ( -10.81189881249999729, 6.242252689847871849, -183.9062500020484094 ) ) ;
#38080 = ORIENTED_EDGE ( 'NONE', *, *, #25981, .T. ) ;
#38081 = CARTESIAN_POINT ( 'NONE',  ( 10.81189881249999907, 6.242252689847868297, -170.7187500020483810 ) ) ;
#38082 = CARTESIAN_POINT ( 'NONE',  ( -10.00000000000000000, -5.773502691896251982, -57.00000000409676915 ) ) ;
#38083 = EDGE_CURVE ( 'NONE', #31273, #12182, #36810, .T. ) ;
#38084 =( BOUNDED_CURVE ( )  B_SPLINE_CURVE ( 2, ( #8442, #15315, #18127, #37779, #8861, #37996, #31962 ),
 .UNSPECIFIED., .F., .F. ) 
 B_SPLINE_CURVE_WITH_KNOTS ( ( 3, 2, 2, 3 ),
 ( 0.05597014925373139382, 0.05721393034825875828, 0.05845771144278612275, 0.05970149253731348721 ),
 .UNSPECIFIED. ) 
 CURVE ( )  GEOMETRIC_REPRESENTATION_ITEM ( )  RATIONAL_B_SPLINE_CURVE ( ( 0.9999999999999947820, 0.8660254037844439257, 1.000000000000000000, 0.8660254037844387076, 1.000000000000000000, 0.8660254037844327124, 1.000000000000005995 ) ) 
 REPRESENTATION_ITEM ( '' )  );
#38085 = CARTESIAN_POINT ( 'NONE',  ( 0.000000000000000000, 0.000000000000000000, -200.0000000000000000 ) ) ;
#38086 = CARTESIAN_POINT ( 'NONE',  ( -5.405949406250003975, -9.363379034771801557, -66.53125000204838102 ) ) ;
#38087 = CARTESIAN_POINT ( 'NONE',  ( -2.121150477449813534E-15, -11.54700538379251284, -40.25000000409676204 ) ) ;
#38088 = CARTESIAN_POINT ( 'NONE',  ( 10.81189881249999907, 6.242252689847868297, -4.218750002048355263 ) ) ;
#38089 = DIRECTION ( 'NONE',  ( 1.000000000000000000, 0.000000000000000000, 0.000000000000000000 ) ) ;
#38090 = CARTESIAN_POINT ( 'NONE',  ( 10.81189881249999551, -6.242252689847874514, -172.6562500020484379 ) ) ;
#38091 = CARTESIAN_POINT ( 'NONE',  ( 9.999999999999998224, 0.000000000000000000, -107.3750000040967763 ) ) ;
#38092 = CARTESIAN_POINT ( 'NONE',  ( -10.00000000000051337, 5.773502691895962435, -148.3749999999999716 ) ) ;
#38093 = ORIENTED_EDGE ( 'NONE', *, *, #31491, .F. ) ;
#38094 = CARTESIAN_POINT ( 'NONE',  ( -4.999999999999996447, 8.660254037844387298, -16.87500000409675138 ) ) ;
#38095 = DIRECTION ( 'NONE',  ( 0.4999999999999998335, 0.8660254037844387076, 0.000000000000000000 ) ) ;
#38096 = CARTESIAN_POINT ( 'NONE',  ( 4.999999999999992006, -8.660254037844389075, -163.1250000040967905 ) ) ;
#38098 = VERTEX_POINT ( 'NONE', #27103 ) ;
#38097 = CARTESIAN_POINT ( 'NONE',  ( -5.405949406250003975, -9.363379034771801557, -74.03125000204838102 ) ) ;
#38099 = SHAPE_REPRESENTATION_RELATIONSHIP ( 'NONE' , 'NONE' ,  #36293, #29436 ) ;
#38100 = ORIENTED_EDGE ( 'NONE', *, *, #33639, .F. ) ;
#38101 = ORIENTED_EDGE ( 'NONE', *, *, #23406, .T. ) ;
#38102 = EDGE_CURVE ( 'NONE', #32122, #14673, #1583, .T. ) ;
#38103 = CARTESIAN_POINT ( 'NONE',  ( 5.405949406249999534, 9.363379034771803333, -35.59375000204836681 ) ) ;
#38104 = CARTESIAN_POINT ( 'NONE',  ( -9.999999999999998224, 1.224646799147353059E-15, -171.1250000040968189 ) ) ;
#38105 = CARTESIAN_POINT ( 'NONE',  ( -5.405949406250003975, -9.363379034771801557, -9.531250002048352599 ) ) ;
#38108 = EDGE_CURVE ( 'NONE', #21458, #25114, #2701, .T. ) ;
#38107 = EDGE_LOOP ( 'NONE', ( #28188, #4072, #29910, #41483 ) ) ;
#38106 = CARTESIAN_POINT ( 'NONE',  ( 5.405949406249992428, -9.363379034771808662, -64.59375000204836681 ) ) ;
#38109 = CARTESIAN_POINT ( 'NONE',  ( -9.999999999999998224, 1.224646799147353059E-15, -109.6250000040967763 ) ) ;
#38110 = CARTESIAN_POINT ( 'NONE',  ( -5.000000000000003553, -8.660254037844383745, -39.99999999999997868 ) ) ;
#38111 = CARTESIAN_POINT ( 'NONE',  ( -10.81189881249999729, -6.242252689847864744, -198.4687500020484094 ) ) ;
#38112 = CARTESIAN_POINT ( 'NONE',  ( -2.293366432827344421E-15, -12.48450537969573659, -177.2187500020484094 ) ) ;
#38113 = CARTESIAN_POINT ( 'NONE',  ( 5.405949406249999534, 9.363379034771803333, -158.5937500020483810 ) ) ;
#38114 = CARTESIAN_POINT ( 'NONE',  ( 10.81189881249999551, -6.242252689847874514, -175.4687500020484094 ) ) ;
#38115 = CARTESIAN_POINT ( 'NONE',  ( 10.00000000000051159, -5.773502691895965988, -75.62499999999998579 ) ) ;
#38116 = DIRECTION ( 'NONE',  ( -0.08682659386424779191, 0.08682659386424779191, 0.9924325091389669673 ) ) ;
#38117 = CARTESIAN_POINT ( 'NONE',  ( 5.000000000000000000, 8.660254037844385522, -193.7500000000000000 ) ) ;
#38118 = CARTESIAN_POINT ( 'NONE',  ( 7.644554776091147741E-16, 12.48450537969573659, -102.9687500020483952 ) ) ;
#38119 = DIRECTION ( 'NONE',  ( 0.000000000000000000, 0.000000000000000000, 1.000000000000000000 ) ) ;
#38120 = CARTESIAN_POINT ( 'NONE',  ( -10.81189881249999907, -6.242252689847864744, -86.15625000204836681 ) ) ;
#38121 = CARTESIAN_POINT ( 'NONE',  ( -10.81189881249999729, 1.324075727343319199E-15, -90.59375000204838102 ) ) ;
#38122 = CARTESIAN_POINT ( 'NONE',  ( -2.293366432827344421E-15, -12.48450537969573659, -72.40625000204836681 ) ) ;
#38123 = CARTESIAN_POINT ( 'NONE',  ( -10.00000000000000000, -5.773502691896251982, -156.0000000040967905 ) ) ;
#38124 = CARTESIAN_POINT ( 'NONE',  ( -10.00000000000000000, -5.773502691896251982, -127.1249999999999858 ) ) ;
#38125 = ADVANCED_FACE ( 'NONE', ( #3378 ), #13276, .T. ) ;
#38126 =( BOUNDED_CURVE ( )  B_SPLINE_CURVE ( 2, ( #23950, #37094, #445, #26753, #24167, #3672, #10336 ),
 .UNSPECIFIED., .F., .F. ) 
 B_SPLINE_CURVE_WITH_KNOTS ( ( 3, 2, 2, 3 ),
 ( 0.7723880597014927130, 0.7736318407960200982, 0.7748756218905473725, 0.7761194029850747578 ),
 .UNSPECIFIED. ) 
 CURVE ( )  GEOMETRIC_REPRESENTATION_ITEM ( )  RATIONAL_B_SPLINE_CURVE ( ( 0.9999999999999761302, 0.8660254037844625774, 1.000000000000000000, 0.8660254037844387076, 1.000000000000000000, 0.8660254037844267172, 1.000000000000011990 ) ) 
 REPRESENTATION_ITEM ( '' )  );
#38127 = CARTESIAN_POINT ( 'NONE',  ( -10.81189881249999729, -6.242252689847864744, -153.6562500020484094 ) ) ;
#38128 = CARTESIAN_POINT ( 'NONE',  ( 10.81189881249999551, -6.242252689847874514, -162.1562500020484379 ) ) ;
#38129 = CARTESIAN_POINT ( 'NONE',  ( -5.000000000000003553, -8.660254037844383745, -39.99999999999997868 ) ) ;
#38130 = CARTESIAN_POINT ( 'NONE',  ( 4.999999999999992006, -8.660254037844389075, -182.2500000000000000 ) ) ;
#38131 = CARTESIAN_POINT ( 'NONE',  ( -2.293366432827344421E-15, -12.48450537969573659, -94.71875000204838102 ) ) ;
#38132 = ORIENTED_EDGE ( 'NONE', *, *, #36313, .F. ) ;
#38133 = CARTESIAN_POINT ( 'NONE',  ( 9.999999999999998224, 0.000000000000000000, -66.49999999999997158 ) ) ;
#38134 = CARTESIAN_POINT ( 'NONE',  ( -10.81189881249999729, 1.324075727343319199E-15, -197.0937500020484094 ) ) ;
#38135 = CARTESIAN_POINT ( 'NONE',  ( 7.070501591499377789E-16, 11.54700538379251284, -80.00000000409679046 ) ) ;
#38136 = CARTESIAN_POINT ( 'NONE',  ( -9.999999999999998224, 1.224646799147353059E-15, -142.6250000040967905 ) ) ;
#38137 = CARTESIAN_POINT ( 'NONE',  ( -9.999999999999998224, 1.224646799147353059E-15, -157.2500000000000000 ) ) ;
#38138 = CARTESIAN_POINT ( 'NONE',  ( -5.405949406249996869, 9.363379034771805109, -94.03125000204838102 ) ) ;
#38139 = CARTESIAN_POINT ( 'NONE',  ( -5.405949406249996869, 9.363379034771805109, -76.03125000204838102 ) ) ;
#38140 =( BOUNDED_CURVE ( )  B_SPLINE_CURVE ( 2, ( #37416, #11496, #7858, #4399, #28143, #34196, #24699 ),
 .UNSPECIFIED., .F., .F. ) 
 B_SPLINE_CURVE_WITH_KNOTS ( ( 3, 2, 2, 3 ),
 ( 0.8619402985074630097, 0.8631840796019903950, 0.8644278606965177802, 0.8656716417910450545 ),
 .UNSPECIFIED. ) 
 CURVE ( )  GEOMETRIC_REPRESENTATION_ITEM ( )  RATIONAL_B_SPLINE_CURVE ( ( 0.9999999999999641398, 0.8660254037844745678, 1.000000000000000000, 0.8660254037844387076, 1.000000000000000000, 0.8660254037844028474, 1.000000000000035971 ) ) 
 REPRESENTATION_ITEM ( '' )  );
#38141 = CARTESIAN_POINT ( 'NONE',  ( 10.00000000000000000, 5.773502691896255534, -71.25000000409676204 ) ) ;
#38142 = CARTESIAN_POINT ( 'NONE',  ( -9.999999999999998224, 1.224646799147353059E-15, -200.0000000000000000 ) ) ;
#38143 = CARTESIAN_POINT ( 'NONE',  ( 10.81189881249999729, 0.000000000000000000, -23.84375000204835970 ) ) ;
#38144 = ORIENTED_EDGE ( 'NONE', *, *, #16628, .F. ) ;
#38145 = CARTESIAN_POINT ( 'NONE',  ( -10.81189881249999729, 6.242252689847871849, -189.9062500020484379 ) ) ;
#38146 = CARTESIAN_POINT ( 'NONE',  ( -5.405949406249996869, 9.363379034771805109, -20.53125000204836326 ) ) ;
#38147 = CARTESIAN_POINT ( 'NONE',  ( 5.405949406249999534, 9.363379034771803333, -7.093750002048371250 ) ) ;
#38148 = CARTESIAN_POINT ( 'NONE',  ( 7.070501591499376803E-16, 11.54700538379251284, -142.6250000000000000 ) ) ;
#38149 = CARTESIAN_POINT ( 'NONE',  ( 5.405949406249999534, 9.363379034771803333, -145.0937500020483810 ) ) ;
#38150 = CARTESIAN_POINT ( 'NONE',  ( 5.500000000000000888, -20.00000000000000000, -220.0000000000000000 ) ) ;
#38151 = DIRECTION ( 'NONE',  ( -0.000000000000000000, -0.000000000000000000, 1.000000000000000000 ) ) ;
#38152 = CARTESIAN_POINT ( 'NONE',  ( -9.999999999999998224, 1.224646799147353059E-15, -179.7500000000000284 ) ) ;
#38153 = CARTESIAN_POINT ( 'NONE',  ( -9.999999999999998224, 1.224646799147353059E-15, -106.2499999999999858 ) ) ;
#38155 = VERTEX_POINT ( 'NONE', #1636 ) ;
#38154 = CARTESIAN_POINT ( 'NONE',  ( 10.81189881249999729, 0.000000000000000000, -105.0312500020483810 ) ) ;
#38156 = CARTESIAN_POINT ( 'NONE',  ( 9.999999999999998224, 0.000000000000000000, -161.3750000040967905 ) ) ;
#38157 = ORIENTED_EDGE ( 'NONE', *, *, #15107, .F. ) ;
#38158 = ORIENTED_EDGE ( 'NONE', *, *, #33597, .F. ) ;
#38159 = CARTESIAN_POINT ( 'NONE',  ( 5.405949406249999534, 9.363379034771803333, -28.28125000204837036 ) ) ;
#38160 = DATE_AND_TIME ( #37300, #40736 ) ;
#38161 = CARTESIAN_POINT ( 'NONE',  ( 10.81189881249999907, 6.242252689847868297, -83.71875000204836681 ) ) ;
#38162 = CARTESIAN_POINT ( 'NONE',  ( -9.999999999999998224, 1.224646799147353059E-15, -127.6250000040967620 ) ) ;
#38163 = CARTESIAN_POINT ( 'NONE',  ( 7.644554776091147741E-16, 12.48450537969573659, -198.9687500020484094 ) ) ;
#38164 = CARTESIAN_POINT ( 'NONE',  ( 7.644554776091147741E-16, 12.48450537969573659, -166.1562500020483810 ) ) ;
#38165 = CARTESIAN_POINT ( 'NONE',  ( -5.000000000000003553, -8.660254037844383745, -11.87500000409674783 ) ) ;
#38166 = CARTESIAN_POINT ( 'NONE',  ( -9.999999999999998224, 1.224646799147353059E-15, -199.2500000000000000 ) ) ;
#38167 = EDGE_CURVE ( 'NONE', #6210, #1756, #1420, .T. ) ;
#38168 = CARTESIAN_POINT ( 'NONE',  ( 10.81189881249999729, 6.242252689847867408, -115.2187500020483810 ) ) ;
#38169 = CARTESIAN_POINT ( 'NONE',  ( -10.81189881249999729, 6.242252689847871849, -87.71875000204838102 ) ) ;
#38170 = CARTESIAN_POINT ( 'NONE',  ( -5.405949406250003975, -9.363379034771801557, -2.031250002048373915 ) ) ;
#38171 = CARTESIAN_POINT ( 'NONE',  ( 10.81189881249999729, 0.000000000000000000, -196.3437500020484094 ) ) ;
#38172 = CARTESIAN_POINT ( 'NONE',  ( 10.81189881249999551, -6.242252689847874514, -96.15625000204838102 ) ) ;
#38173 = CARTESIAN_POINT ( 'NONE',  ( 9.999999999999998224, 0.000000000000000000, -174.8750000040967905 ) ) ;
#38174 = CARTESIAN_POINT ( 'NONE',  ( -5.405949406249996869, 9.363379034771805109, -169.0312500020484094 ) ) ;
#38175 = CARTESIAN_POINT ( 'NONE',  ( 9.999999999999998224, 0.000000000000000000, -164.3750000040967905 ) ) ;
#38176 = CARTESIAN_POINT ( 'NONE',  ( -10.81189881249999729, 1.324075727343319199E-15, -176.2812500020484094 ) ) ;
#38177 = CARTESIAN_POINT ( 'NONE',  ( -10.81189881249999729, 1.324075727343319199E-15, -185.2812500020484094 ) ) ;
#38178 = CARTESIAN_POINT ( 'NONE',  ( 10.81189881249999551, -6.242252689847874514, -46.46875000204838102 ) ) ;
#38179 = CARTESIAN_POINT ( 'NONE',  ( 9.999999999999998224, 0.000000000000000000, -165.8750000040967905 ) ) ;
#38180 = CARTESIAN_POINT ( 'NONE',  ( 10.81189881249999907, 6.242252689847868297, -5.906250002048359704 ) ) ;
#38181 = CARTESIAN_POINT ( 'NONE',  ( -10.81189881249999907, -6.242252689847864744, -13.96875000204836326 ) ) ;
#38182 = CARTESIAN_POINT ( 'NONE',  ( 7.070501591499376803E-16, 11.54700538379251284, -54.12499999999997158 ) ) ;
#38183 = CARTESIAN_POINT ( 'NONE',  ( 10.81189881249999907, 6.242252689847868297, -125.7187500020483810 ) ) ;
#38184 = CARTESIAN_POINT ( 'NONE',  ( -9.999999999999998224, 1.224646799147353059E-15, -88.24999999999998579 ) ) ;
#38185 = CARTESIAN_POINT ( 'NONE',  ( 7.644554776091147741E-16, 12.48450537969573659, -17.65625000204837391 ) ) ;
#38186 = CARTESIAN_POINT ( 'NONE',  ( -10.00000000000000000, -5.773502691896251982, -106.5000000040967763 ) ) ;
#38187 = CARTESIAN_POINT ( 'NONE',  ( 9.999999999999998224, 0.000000000000000000, -143.3750000040967905 ) ) ;
#38188 = CARTESIAN_POINT ( 'NONE',  ( 5.000000000000000000, 8.660254037844385522, -52.74999999999996447 ) ) ;
#38189 = CARTESIAN_POINT ( 'NONE',  ( 10.81189881249999551, -6.242252689847874514, -114.1562500020483952 ) ) ;
#38190 = CARTESIAN_POINT ( 'NONE',  ( 10.81189881249999551, -6.242252689847874514, -103.6562500020483810 ) ) ;
#38191 = EDGE_CURVE ( 'NONE', #1644, #29774, #17301, .T. ) ;
#38192 = VERTEX_POINT ( 'NONE', #21472 ) ;
#38193 = CARTESIAN_POINT ( 'NONE',  ( -2.121150477449813534E-15, -11.54700538379251284, -91.25000000409677625 ) ) ;
#38194 = LINE ( 'NONE', #12687, #32589 ) ;
#38195 = CARTESIAN_POINT ( 'NONE',  ( 10.81189881249999729, 0.000000000000000000, -157.5312500020484094 ) ) ;
#38196 = CARTESIAN_POINT ( 'NONE',  ( -10.81189881249999729, 1.324075727343319199E-15, -48.59375000204838102 ) ) ;
#38197 = ORIENTED_EDGE ( 'NONE', *, *, #3804, .F. ) ;
#38198 = CARTESIAN_POINT ( 'NONE',  ( 10.00000000000000000, 5.773502691896255534, -28.87499999999997868 ) ) ;
#38199 = CARTESIAN_POINT ( 'NONE',  ( 10.81189881249999729, 6.242252689847867408, -28.40625000204838813 ) ) ;
#38200 = CARTESIAN_POINT ( 'NONE',  ( -9.999999999999998224, 1.224646799147353059E-15, -152.7500000000000000 ) ) ;
#38201 = CARTESIAN_POINT ( 'NONE',  ( -2.121150477449813534E-15, -11.54700538379251284, -22.25000000409676915 ) ) ;
#38202 = CARTESIAN_POINT ( 'NONE',  ( 4.999999999999992006, -8.660254037844389075, -80.62500000409677625 ) ) ;
#38203 = CARTESIAN_POINT ( 'NONE',  ( 10.81189881249999907, 6.242252689847868297, -122.9062500020484094 ) ) ;
#38204 = CARTESIAN_POINT ( 'NONE',  ( 9.999999999999227285, 5.773502691896701400, -111.3749999999999432 ) ) ;
#38205 =( BOUNDED_CURVE ( )  B_SPLINE_CURVE ( 2, ( #29700, #38981, #9417, #146, #8995, #15659, #40032 ),
 .UNSPECIFIED., .F., .F. ) 
 B_SPLINE_CURVE_WITH_KNOTS ( ( 3, 2, 2, 3 ),
 ( 0.4850746268656717652, 0.4863184079601990950, 0.4875621890547264248, 0.4888059701492538101 ),
 .UNSPECIFIED. ) 
 CURVE ( )  GEOMETRIC_REPRESENTATION_ITEM ( )  RATIONAL_B_SPLINE_CURVE ( ( 0.9999999999999880096, 0.8660254037844506980, 1.000000000000000000, 0.8660254037844387076, 1.000000000000000000, 0.8660254037844327124, 1.000000000000005995 ) ) 
 REPRESENTATION_ITEM ( '' )  );
#38206 = CARTESIAN_POINT ( 'NONE',  ( -9.999999999999479527, -5.773502691896549521, -45.00000000409674783 ) ) ;
#38207 = ORIENTED_EDGE ( 'NONE', *, *, #18057, .T. ) ;
#38208 = CARTESIAN_POINT ( 'NONE',  ( -5.405949406249996869, 9.363379034771805109, -64.03125000204836681 ) ) ;
#38209 = CALENDAR_DATE ( 2026, 28, 9 ) ;
#38210 = CARTESIAN_POINT ( 'NONE',  ( 10.81189881249999907, 6.242252689847868297, -107.7187500020483810 ) ) ;
#38212 = ORIENTED_EDGE ( 'NONE', *, *, #41656, .T. ) ;
#38211 = VERTEX_POINT ( 'NONE', #40452 ) ;
#38213 = CARTESIAN_POINT ( 'NONE',  ( -79.99999999999995737, -40.00000000000000711, -170.0000000000000000 ) ) ;
#38214 = CARTESIAN_POINT ( 'NONE',  ( 10.00000000000031619, -5.773502691896077010, -183.6249999999999716 ) ) ;
#38216 = ADVANCED_FACE ( 'NONE', ( #14334 ), #34445, .T. ) ;
#38215 = CARTESIAN_POINT ( 'NONE',  ( 10.81189881249999729, 0.000000000000000000, -154.3437500020483810 ) ) ;
#38217 = CARTESIAN_POINT ( 'NONE',  ( -10.81189881249999907, -6.242252689847864744, -191.1562500020484094 ) ) ;
#38218 = CARTESIAN_POINT ( 'NONE',  ( 10.81189881249999551, -6.242252689847874514, -8.968750002048359704 ) ) ;
#38219 = CARTESIAN_POINT ( 'NONE',  ( 10.81189881249999729, 0.000000000000000000, -136.3437500020484094 ) ) ;
#38220 = CARTESIAN_POINT ( 'NONE',  ( 5.405949406249999534, 9.363379034771803333, -100.2812500020483952 ) ) ;
#38221 = CARTESIAN_POINT ( 'NONE',  ( 7.644554776091147741E-16, 12.48450537969573659, -107.4687500020483668 ) ) ;
#38222 = CARTESIAN_POINT ( 'NONE',  ( -10.00000000000025580, 5.773502691896109873, -187.3750000000000284 ) ) ;
#38223 = CARTESIAN_POINT ( 'NONE',  ( 7.644554776091147741E-16, 12.48450537969573659, -116.6562500020483952 ) ) ;
#38224 = CARTESIAN_POINT ( 'NONE',  ( 9.999999999999998224, 0.000000000000000000, -198.8750000040967905 ) ) ;
#38225 = CARTESIAN_POINT ( 'NONE',  ( 5.405949406249992428, -9.363379034771808662, -121.5937500020483952 ) ) ;
#38226 = CARTESIAN_POINT ( 'NONE',  ( 5.405949406249992428, -9.363379034771808662, -190.7812500020484094 ) ) ;
#38227 = CARTESIAN_POINT ( 'NONE',  ( 9.999999999999998224, 0.000000000000000000, -158.0000000000000000 ) ) ;
#38228 = CARTESIAN_POINT ( 'NONE',  ( -2.121150477449813534E-15, -11.54700538379251284, -146.3750000000000000 ) ) ;
#38229 = CARTESIAN_POINT ( 'NONE',  ( -4.999999999999996447, 8.660254037844387298, -8.999999999999952038 ) ) ;
#38230 = CARTESIAN_POINT ( 'NONE',  ( -5.405949406250003975, -9.363379034771801557, -70.84375000204836681 ) ) ;
#38231 = CARTESIAN_POINT ( 'NONE',  ( 10.81189881249999551, -6.242252689847874514, -55.46875000204837391 ) ) ;
#38232 = CARTESIAN_POINT ( 'NONE',  ( 10.00000000000000000, 5.773502691896255534, -185.2500000040967905 ) ) ;
#38233 = CARTESIAN_POINT ( 'NONE',  ( -10.81189881249999729, 1.324075727343319199E-15, -26.28125000204836681 ) ) ;
#38234 = CARTESIAN_POINT ( 'NONE',  ( 10.81189881249999907, 6.242252689847868297, -38.71875000204835260 ) ) ;
#38235 = CARTESIAN_POINT ( 'NONE',  ( -9.999999999999998224, 1.224646799147353059E-15, -94.62500000409677625 ) ) ;
#38236 = CARTESIAN_POINT ( 'NONE',  ( -10.81189881249999729, 1.324075727343319199E-15, -149.0937500020483810 ) ) ;
#38237 = CARTESIAN_POINT ( 'NONE',  ( 5.000000000000000000, 8.660254037844385522, -118.7500000000000000 ) ) ;
#38238 = EDGE_CURVE ( 'NONE', #15716, #8658, #20574, .T. ) ;
#38239 = CARTESIAN_POINT ( 'NONE',  ( -9.999999999999479527, -5.773502691896549521, -148.1249999999999716 ) ) ;
#38240 = CARTESIAN_POINT ( 'NONE',  ( -5.000000000000003553, -8.660254037844383745, -71.49999999999998579 ) ) ;
#38241 = CARTESIAN_POINT ( 'NONE',  ( 10.81189881249999551, -6.242252689847874514, -139.6562500020484094 ) ) ;
#38242 = CARTESIAN_POINT ( 'NONE',  ( -5.405949406250003975, -9.363379034771801557, -12.53125000204835615 ) ) ;
#38243 = VERTEX_POINT ( 'NONE', #30567 ) ;
#38244 = CARTESIAN_POINT ( 'NONE',  ( -5.405949406250003975, -9.363379034771801557, -102.5312500020483952 ) ) ;
#38245 = CARTESIAN_POINT ( 'NONE',  ( 5.000000000000000000, 8.660254037844385522, -114.6250000040967763 ) ) ;
#38246 = CARTESIAN_POINT ( 'NONE',  ( 9.999999999999998224, 0.000000000000000000, -140.0000000000000000 ) ) ;
#38247 = CARTESIAN_POINT ( 'NONE',  ( -2.293366432827344421E-15, -12.48450537969573659, -72.21875000204835260 ) ) ;
#38248 = CARTESIAN_POINT ( 'NONE',  ( -4.999999999999996447, 8.660254037844387298, -49.49999999999998579 ) ) ;
#38249 = CARTESIAN_POINT ( 'NONE',  ( -9.999999999999998224, 1.224646799147353059E-15, -24.12500000409675849 ) ) ;
#38250 = CARTESIAN_POINT ( 'NONE',  ( -5.405949406250003975, -9.363379034771801557, -41.03125000204838102 ) ) ;
#38251 =( BOUNDED_CURVE ( )  B_SPLINE_CURVE ( 2, ( #10270, #3607, #7051, #17373, #14988, #4232, #20836 ),
 .UNSPECIFIED., .F., .F. ) 
 B_SPLINE_CURVE_WITH_KNOTS ( ( 3, 2, 2, 3 ),
 ( 0.6455223880597016350, 0.6467661691542290203, 0.6480099502487564056, 0.6492537313432837909 ),
 .UNSPECIFIED. ) 
 CURVE ( )  GEOMETRIC_REPRESENTATION_ITEM ( )  RATIONAL_B_SPLINE_CURVE ( ( 0.9999999999999880096, 0.8660254037844506980, 1.000000000000000000, 0.8660254037844387076, 1.000000000000000000, 0.8660254037844148378, 1.000000000000023981 ) ) 
 REPRESENTATION_ITEM ( '' )  );
#38252 = CARTESIAN_POINT ( 'NONE',  ( -10.00000000000102496, 5.773502691895664007, -23.87499999999995381 ) ) ;
#38253 = CARTESIAN_POINT ( 'NONE',  ( 7.644554776091147741E-16, 12.48450537969573659, -142.1562500020483810 ) ) ;
#38254 = CARTESIAN_POINT ( 'NONE',  ( -10.81189881249999907, -6.242252689847864744, -129.4687500020483810 ) ) ;
#38255 = DIRECTION ( 'NONE',  ( 0.000000000000000000, 0.000000000000000000, 1.000000000000000000 ) ) ;
#38256 = EDGE_LOOP ( 'NONE', ( #16140, #34869, #35199, #4707 ) ) ;
#38257 = AXIS2_PLACEMENT_3D ( 'NONE', #23062, #13321, #42679 ) ;
#38258 = VERTEX_POINT ( 'NONE', #24735 ) ;
#38259 = ORIENTED_EDGE ( 'NONE', *, *, #34944, .T. ) ;
#38260 = CARTESIAN_POINT ( 'NONE',  ( 0.000000000000000000, 0.000000000000000000, -200.0000000000000000 ) ) ;
#38261 = CARTESIAN_POINT ( 'NONE',  ( -5.405949406250003975, -9.363379034771801557, -178.8437500020483810 ) ) ;
#38262 = CARTESIAN_POINT ( 'NONE',  ( -5.405949406250003975, -9.363379034771801557, -30.34375000204836326 ) ) ;
#38263 = CARTESIAN_POINT ( 'NONE',  ( -9.999999999999998224, 1.224646799147353059E-15, -109.6250000040967763 ) ) ;
#38264 = CARTESIAN_POINT ( 'NONE',  ( -5.405949406250003975, -9.363379034771801557, -160.8437500020484094 ) ) ;
#38265 = CARTESIAN_POINT ( 'NONE',  ( 5.405949406249999534, 9.363379034771803333, -157.0937500020483810 ) ) ;
#38266 = CARTESIAN_POINT ( 'NONE',  ( -9.999999999999998224, 1.224646799147353059E-15, -200.0000000000000000 ) ) ;
#38267 = CARTESIAN_POINT ( 'NONE',  ( -10.81189881249999729, 6.242252689847871849, -135.7187500020483810 ) ) ;
#38268 = AXIS2_PLACEMENT_3D ( 'NONE', #33028, #32034, #16593 ) ;
#38269 = CARTESIAN_POINT ( 'NONE',  ( 10.81189881249999907, 6.242252689847868297, -142.4062500020484094 ) ) ;
#38270 = CARTESIAN_POINT ( 'NONE',  ( 7.644554776091147741E-16, 12.48450537969573659, -143.4687500020484094 ) ) ;
#38271 = CARTESIAN_POINT ( 'NONE',  ( 9.999999999999742428, 5.773502691896404748, -135.3750000000000000 ) ) ;
#38272 = CARTESIAN_POINT ( 'NONE',  ( -4.999999999999996447, 8.660254037844387298, -10.87500000409674605 ) ) ;
#38273 = CARTESIAN_POINT ( 'NONE',  ( -5.000000000000003553, -8.660254037844383745, -175.0000000000000284 ) ) ;
#38274 = CARTESIAN_POINT ( 'NONE',  ( -10.81189881249999729, 6.242252689847871849, -78.71875000204838102 ) ) ;
#38275 = CARTESIAN_POINT ( 'NONE',  ( -5.000000000000003553, -8.660254037844383745, -113.8750000040967763 ) ) ;
#38276 = CARTESIAN_POINT ( 'NONE',  ( 10.81189881249999907, 6.242252689847868297, -49.40625000204837391 ) ) ;
#38277 = CARTESIAN_POINT ( 'NONE',  ( 0.000000000000000000, 0.000000000000000000, -200.0000000000000000 ) ) ;
#38278 = CARTESIAN_POINT ( 'NONE',  ( 10.81189881249999729, 0.000000000000000000, -170.8437500020484094 ) ) ;
#38279 = CARTESIAN_POINT ( 'NONE',  ( 10.81189881249999729, 0.000000000000000000, -117.0312500020483952 ) ) ;
#38280 = CARTESIAN_POINT ( 'NONE',  ( 5.405949406249999534, 9.363379034771803333, -143.7812500020483810 ) ) ;
#38281 = CARTESIAN_POINT ( 'NONE',  ( 9.999999999999998224, 0.000000000000000000, -138.5000000000000000 ) ) ;
#38282 = CARTESIAN_POINT ( 'NONE',  ( 5.405949406249999534, 9.363379034771803333, -43.28125000204838102 ) ) ;
#38283 = CARTESIAN_POINT ( 'NONE',  ( 9.999999999999998224, 0.000000000000000000, -122.3750000040967905 ) ) ;
#38284 = CARTESIAN_POINT ( 'NONE',  ( -2.121150477449813534E-15, -11.54700538379251284, -101.3750000000000000 ) ) ;
#38285 = ORIENTED_EDGE ( 'NONE', *, *, #38893, .F. ) ;
#38286 = AXIS2_PLACEMENT_3D ( 'NONE', #25516, #32204, #2633 ) ;
#38287 = CARTESIAN_POINT ( 'NONE',  ( -5.405949406249996869, 9.363379034771805109, -130.0312500020484094 ) ) ;
#38288 = CARTESIAN_POINT ( 'NONE',  ( 9.999999999999998224, 0.000000000000000000, -137.3750000040967905 ) ) ;
#38289 = CARTESIAN_POINT ( 'NONE',  ( 9.999999999999998224, 0.000000000000000000, -147.5000000000000000 ) ) ;
#38290 = CARTESIAN_POINT ( 'NONE',  ( 5.405949406249999534, 9.363379034771803333, -176.7812500020484094 ) ) ;
#38291 = ORIENTED_EDGE ( 'NONE', *, *, #27809, .F. ) ;
#38292 = CARTESIAN_POINT ( 'NONE',  ( -10.81189881249999729, 1.324075727343319199E-15, -174.5937500020484094 ) ) ;
#38293 = CARTESIAN_POINT ( 'NONE',  ( -5.000000000000003553, -8.660254037844383745, -53.87500000409675494 ) ) ;
#38294 = EDGE_CURVE ( 'NONE', #33541, #16838, #35243, .T. ) ;
#38295 = CYLINDRICAL_SURFACE ( 'NONE', #9729, 9.999999999999998224 ) ;
#38296 = CARTESIAN_POINT ( 'NONE',  ( 10.81189881249999907, 6.242252689847868297, -71.90625000204836681 ) ) ;
#38297 = CARTESIAN_POINT ( 'NONE',  ( 5.000000000000000000, 8.660254037844385522, -47.12500000409677625 ) ) ;
#38298 = CARTESIAN_POINT ( 'NONE',  ( 7.070501591499376803E-16, 11.54700538379251284, -84.12499999999997158 ) ) ;
#38299 = CARTESIAN_POINT ( 'NONE',  ( -5.405949406249996869, 9.363379034771805109, -167.5312500020484094 ) ) ;
#38300 = CARTESIAN_POINT ( 'NONE',  ( -10.00000000000102496, 5.773502691895664007, -1.750000004096726069 ) ) ;
#38301 = CARTESIAN_POINT ( 'NONE',  ( 9.999999999998969713, 5.773502691896851502, -64.87499999999997158 ) ) ;
#38302 = ORIENTED_EDGE ( 'NONE', *, *, #42405, .F. ) ;
#38303 = DIRECTION ( 'NONE',  ( -0.000000000000000000, -0.000000000000000000, 1.000000000000000000 ) ) ;
#38304 = CARTESIAN_POINT ( 'NONE',  ( -9.999999999999998224, 1.224646799147353059E-15, -137.7499999999999716 ) ) ;
#38305 = VECTOR ( 'NONE', #21379, 1000.000000000000000 ) ;
#38306 = AXIS2_PLACEMENT_3D ( 'NONE', #4650, #7679, #34016 ) ;
#38307 = DIRECTION ( 'NONE',  ( -0.000000000000000000, -0.000000000000000000, 1.000000000000000000 ) ) ;
#38309 = ORIENTED_EDGE ( 'NONE', *, *, #382, .F. ) ;
#38308 = CARTESIAN_POINT ( 'NONE',  ( -10.81189881249999729, 6.242252689847871849, -81.90625000204838102 ) ) ;
#38311 = ORIENTED_EDGE ( 'NONE', *, *, #13771, .T. ) ;
#38310 = CARTESIAN_POINT ( 'NONE',  ( 10.00000000000025402, -5.773502691896113426, -188.5000000040968473 ) ) ;
#38312 = AXIS2_PLACEMENT_3D ( 'NONE', #7465, #20615, #33802 ) ;
#38313 = ORIENTED_EDGE ( 'NONE', *, *, #34824, .F. ) ;
#38314 = CARTESIAN_POINT ( 'NONE',  ( 5.405949406249992428, -9.363379034771808662, -33.09375000204836681 ) ) ;
#38315 = CARTESIAN_POINT ( 'NONE',  ( 10.00000000000102318, -5.773502691895667560, -53.12499999999995737 ) ) ;
#38316 = CARTESIAN_POINT ( 'NONE',  ( -10.81189881249999729, 6.242252689847871849, -3.906250002048350822 ) ) ;
#38318 = ORIENTED_EDGE ( 'NONE', *, *, #42273, .T. ) ;
#38317 = CARTESIAN_POINT ( 'NONE',  ( -2.293366432827344421E-15, -12.48450537969573659, -54.21875000204838102 ) ) ;
#38319 = CARTESIAN_POINT ( 'NONE',  ( -9.999999999999998224, 1.224646799147353059E-15, -28.24999999999996803 ) ) ;
#38320 = CARTESIAN_POINT ( 'NONE',  ( -9.999999999999998224, 5.773502691896259087, -35.87499999999995737 ) ) ;
#38321 = CARTESIAN_POINT ( 'NONE',  ( -5.405949406250003975, -9.363379034771801557, -198.3437500020484094 ) ) ;
#38322 = CARTESIAN_POINT ( 'NONE',  ( 7.644554776091147741E-16, 12.48450537969573659, -177.9687500020483810 ) ) ;
#38323 = CARTESIAN_POINT ( 'NONE',  ( 7.644554776091147741E-16, 12.48450537969573659, -161.4687500020484094 ) ) ;
#38324 = CARTESIAN_POINT ( 'NONE',  ( -5.405949406250003975, -9.363379034771801557, -166.8437500020484094 ) ) ;
#38325 = CARTESIAN_POINT ( 'NONE',  ( 9.999999999999998224, 0.000000000000000000, -200.0000000000000000 ) ) ;
#38326 = CARTESIAN_POINT ( 'NONE',  ( 9.999999999999996447, -5.773502691896262640, -195.6250000000000284 ) ) ;
#38327 = CARTESIAN_POINT ( 'NONE',  ( -10.81189881249999907, -6.242252689847864744, -102.4687500020483810 ) ) ;
#38328 = DIRECTION ( 'NONE',  ( -0.000000000000000000, -0.000000000000000000, 1.000000000000000000 ) ) ;
#38329 = CARTESIAN_POINT ( 'NONE',  ( 5.405949406249992428, -9.363379034771808662, -82.78125000204838102 ) ) ;
#38330 = CARTESIAN_POINT ( 'NONE',  ( -5.405949406250003975, -9.363379034771801557, -88.84375000204838102 ) ) ;
#38331 =( BOUNDED_CURVE ( )  B_SPLINE_CURVE ( 2, ( #10221, #3974, #36556, #10855, #7420 ),
 .UNSPECIFIED., .F., .F. ) 
 B_SPLINE_CURVE_WITH_KNOTS ( ( 3, 2, 3 ),
 ( 0.9925373134328360214, 0.9937810945273632957, 0.9950248756218905699 ),
 .UNSPECIFIED. ) 
 CURVE ( )  GEOMETRIC_REPRESENTATION_ITEM ( )  RATIONAL_B_SPLINE_CURVE ( ( 0.9999999999999761302, 0.8660254037844625774, 1.000000000000000000, 0.8660254037844387076, 1.000000000000000000 ) ) 
 REPRESENTATION_ITEM ( '' )  );
#38332 = CARTESIAN_POINT ( 'NONE',  ( -10.81189881249999729, 1.324075727343319199E-15, -71.28125000204838102 ) ) ;
#38333 = CARTESIAN_POINT ( 'NONE',  ( -2.121150477449813534E-15, -11.54700538379251284, -146.7500000040968189 ) ) ;
#38334 = CARTESIAN_POINT ( 'NONE',  ( 9.999999999999996447, -5.773502691896262640, -126.6250000000000000 ) ) ;
#38335 = ORIENTED_EDGE ( 'NONE', *, *, #32988, .T. ) ;
#38336 = CARTESIAN_POINT ( 'NONE',  ( 10.81189881249999729, 0.000000000000000000, -153.0312500020484094 ) ) ;
#38337 = CARTESIAN_POINT ( 'NONE',  ( 10.81189881249999729, 0.000000000000000000, -166.5312500020484094 ) ) ;
#38338 = CARTESIAN_POINT ( 'NONE',  ( -9.999999999999998224, 1.224646799147353059E-15, -147.1250000040967905 ) ) ;
#38339 = DIRECTION ( 'NONE',  ( -0.000000000000000000, -0.000000000000000000, 1.000000000000000000 ) ) ;
#38340 = CARTESIAN_POINT ( 'NONE',  ( 5.405949406249999534, 9.363379034771803333, -100.0937500020483810 ) ) ;
#38341 = ORIENTED_EDGE ( 'NONE', *, *, #42513, .T. ) ;
#38342 = CARTESIAN_POINT ( 'NONE',  ( 4.999999999999992006, -8.660254037844389075, -63.74999999999997158 ) ) ;
#38343 = CARTESIAN_POINT ( 'NONE',  ( -10.81189881249999729, 6.242252689847871849, -197.2187500020484379 ) ) ;
#38344 = CARTESIAN_POINT ( 'NONE',  ( -9.999999999999998224, 5.773502691896259087, -75.25000000409677625 ) ) ;
#38345 = ADVANCED_FACE ( 'NONE', ( #7896 ), #41311, .T. ) ;
#38346 = CARTESIAN_POINT ( 'NONE',  ( 9.999999999999998224, 0.000000000000000000, -141.8750000040967905 ) ) ;
#38347 = LINE ( 'NONE', #1090, #37600 ) ;
#38348 = CARTESIAN_POINT ( 'NONE',  ( 10.81189881249999907, 6.242252689847868297, -89.90625000204839523 ) ) ;
#38349 = CARTESIAN_POINT ( 'NONE',  ( -10.81189881249999729, -6.242252689847864744, -75.65625000204836681 ) ) ;
#38350 = EDGE_CURVE ( 'NONE', #12651, #37668, #8326, .T. ) ;
#38351 = CARTESIAN_POINT ( 'NONE',  ( 4.999999999999992006, -8.660254037844389075, -70.12500000409677625 ) ) ;
#38352 = DIRECTION ( 'NONE',  ( -0.000000000000000000, -0.000000000000000000, 1.000000000000000000 ) ) ;
#38353 = CARTESIAN_POINT ( 'NONE',  ( -10.81189881249999729, 1.324075727343319199E-15, -27.59375000204836326 ) ) ;
#38354 = VERTEX_POINT ( 'NONE', #27745 ) ;
#38355 = CARTESIAN_POINT ( 'NONE',  ( 10.81189881249999729, 0.000000000000000000, -196.5312500020484094 ) ) ;
#38356 = EDGE_CURVE ( 'NONE', #19091, #18719, #28177, .T. ) ;
#38357 = CARTESIAN_POINT ( 'NONE',  ( -5.405949406250003975, -9.363379034771801557, -17.03125000204835970 ) ) ;
#38358 = CARTESIAN_POINT ( 'NONE',  ( 5.405949406249999534, 9.363379034771803333, -4.093750002048368586 ) ) ;
#38359 = DIRECTION ( 'NONE',  ( -1.000000000000000000, 0.000000000000000000, 0.000000000000000000 ) ) ;
#38360 = CARTESIAN_POINT ( 'NONE',  ( -2.121150477449813534E-15, -11.54700538379251284, -50.37499999999998579 ) ) ;
#38361 = APPROVAL ( #9906, 'UNSPECIFIED' ) ;
#38362 = DIRECTION ( 'NONE',  ( -0.5000000000000003331, 0.8660254037844383745, 0.000000000000000000 ) ) ;
#38363 = CARTESIAN_POINT ( 'NONE',  ( -5.000000000000003553, -8.660254037844383745, -175.0000000000000284 ) ) ;
#38364 = FACE_OUTER_BOUND ( 'NONE', #35924, .T. ) ;
#38366 = VERTEX_POINT ( 'NONE', #31416 ) ;
#38365 = CARTESIAN_POINT ( 'NONE',  ( 7.644554776091147741E-16, 12.48450537969573659, -101.6562500020483952 ) ) ;
#38367 = CARTESIAN_POINT ( 'NONE',  ( 10.00000000000025402, -5.773502691896113426, -164.1250000000000284 ) ) ;
#38368 = ORIENTED_EDGE ( 'NONE', *, *, #35354, .F. ) ;
#38369 = ORIENTED_EDGE ( 'NONE', *, *, #13936, .F. ) ;
#38370 = CARTESIAN_POINT ( 'NONE',  ( 5.405949406249992428, -9.363379034771808662, -28.78125000204837036 ) ) ;
#38371 = CALENDAR_DATE ( 2026, 28, 9 ) ;
#38372 = EDGE_CURVE ( 'NONE', #21752, #6776, #4085, .T. ) ;
#38373 = CARTESIAN_POINT ( 'NONE',  ( -10.81189881249999729, 1.324075727343319199E-15, -78.59375000204838102 ) ) ;
#38374 = LINE ( 'NONE', #28470, #41484 ) ;
#38375 = CARTESIAN_POINT ( 'NONE',  ( 9.999999999999998224, 0.000000000000000000, -173.3750000040968189 ) ) ;
#38376 =( BOUNDED_CURVE ( )  B_SPLINE_CURVE ( 2, ( #1068, #33245, #11189, #17440, #27175, #40528, #16800 ),
 .UNSPECIFIED., .F., .F. ) 
 B_SPLINE_CURVE_WITH_KNOTS ( ( 3, 2, 2, 3 ),
 ( 0.4626865671641792743, 0.4639303482587066596, 0.4651741293532339339, 0.4664179104477613191 ),
 .UNSPECIFIED. ) 
 CURVE ( )  GEOMETRIC_REPRESENTATION_ITEM ( )  RATIONAL_B_SPLINE_CURVE ( ( 0.9999999999999820144, 0.8660254037844566932, 1.000000000000000000, 0.8660254037844387076, 1.000000000000000000, 0.8660254037844267172, 1.000000000000011990 ) ) 
 REPRESENTATION_ITEM ( '' )  );
#38377 = DIRECTION ( 'NONE',  ( 0.000000000000000000, 0.000000000000000000, -1.000000000000000000 ) ) ;
#38378 = CARTESIAN_POINT ( 'NONE',  ( 10.81189881249999907, 6.242252689847868297, -163.4062500020484094 ) ) ;
#38379 = CARTESIAN_POINT ( 'NONE',  ( 5.000000000000000000, 8.660254037844385522, -14.12500000409674961 ) ) ;
#38380 = DIRECTION ( 'NONE',  ( -0.000000000000000000, -0.000000000000000000, -1.000000000000000000 ) ) ;
#38381 = CARTESIAN_POINT ( 'NONE',  ( 5.405949406249999534, 9.363379034771803333, -118.0937500020483810 ) ) ;
#38382 = CARTESIAN_POINT ( 'NONE',  ( -5.405949406249996869, 9.363379034771805109, -89.34375000204838102 ) ) ;
#38383 = CARTESIAN_POINT ( 'NONE',  ( -5.405949406250003975, -9.363379034771801557, -193.8437500020484094 ) ) ;
#38384 = CARTESIAN_POINT ( 'NONE',  ( 5.405949406249999534, 9.363379034771803333, -89.78125000204838102 ) ) ;
#38385 = CARTESIAN_POINT ( 'NONE',  ( -4.999999999999996447, 8.660254037844387298, -166.8750000040967905 ) ) ;
#38386 = CARTESIAN_POINT ( 'NONE',  ( 10.81189881249999551, -6.242252689847874514, -174.1562500020484094 ) ) ;
#38387 =( BOUNDED_CURVE ( )  B_SPLINE_CURVE ( 2, ( #40498, #37067, #13953, #7509, #27362, #31038, #17412 ),
 .UNSPECIFIED., .F., .F. ) 
 B_SPLINE_CURVE_WITH_KNOTS ( ( 3, 2, 2, 3 ),
 ( 0.8955223880597017461, 0.8967661691542291313, 0.8980099502487565166, 0.8992537313432839019 ),
 .UNSPECIFIED. ) 
 CURVE ( )  GEOMETRIC_REPRESENTATION_ITEM ( )  RATIONAL_B_SPLINE_CURVE ( ( 0.9999999999999761302, 0.8660254037844625774, 1.000000000000000000, 0.8660254037844387076, 1.000000000000000000, 0.8660254037844028474, 1.000000000000035971 ) ) 
 REPRESENTATION_ITEM ( '' )  );
#38388 = CARTESIAN_POINT ( 'NONE',  ( 9.999999999999998224, 0.000000000000000000, -69.87500000409677625 ) ) ;
#38389 = CARTESIAN_POINT ( 'NONE',  ( -10.81189881249999729, 6.242252689847871849, -171.9062500020484094 ) ) ;
#38390 = CARTESIAN_POINT ( 'NONE',  ( -10.81189881249999907, -6.242252689847864744, -189.6562500020484094 ) ) ;
#38391 = CARTESIAN_POINT ( 'NONE',  ( -10.81189881249999729, 6.242252689847871849, -44.21875000204835970 ) ) ;
#38392 = CARTESIAN_POINT ( 'NONE',  ( 4.999999999999992006, -8.660254037844389075, -164.6250000040967905 ) ) ;
#38393 = CARTESIAN_POINT ( 'NONE',  ( 7.644554776091147741E-16, 12.48450537969573659, -1.156250002048369474 ) ) ;
#38394 = CARTESIAN_POINT ( 'NONE',  ( 5.405949406249999534, 9.363379034771803333, -11.59375000204834727 ) ) ;
#38395 = CARTESIAN_POINT ( 'NONE',  ( 10.00000000000038369, -5.773502691896038819, -152.5000000040967620 ) ) ;
#38396 = CARTESIAN_POINT ( 'NONE',  ( 7.644554776091147741E-16, 12.48450537969573659, -119.4687500020483952 ) ) ;
#38397 = CARTESIAN_POINT ( 'NONE',  ( -9.999999999999998224, 1.224646799147353059E-15, -86.74999999999998579 ) ) ;
#38398 = CARTESIAN_POINT ( 'NONE',  ( 10.81189881249999551, -6.242252689847874514, -19.65625000204837747 ) ) ;
#38399 = CARTESIAN_POINT ( 'NONE',  ( -9.999999999999998224, 5.773502691896259087, -103.7500000040967620 ) ) ;
#38400 = DIRECTION ( 'NONE',  ( -0.000000000000000000, -0.000000000000000000, -1.000000000000000000 ) ) ;
#38401 = CARTESIAN_POINT ( 'NONE',  ( -10.81189881249999729, 1.324075727343319199E-15, -114.7812500020483952 ) ) ;
#38402 = CARTESIAN_POINT ( 'NONE',  ( 10.81189881249999729, 0.000000000000000000, -103.5312500020483810 ) ) ;
#38403 = ORIENTED_EDGE ( 'NONE', *, *, #19995, .T. ) ;
#38404 = CARTESIAN_POINT ( 'NONE',  ( -9.999999999999998224, 1.224646799147353059E-15, -88.62500000409677625 ) ) ;
#38405 = CARTESIAN_POINT ( 'NONE',  ( -9.999999999999998224, 1.224646799147353059E-15, -71.74999999999998579 ) ) ;
#38406 = CARTESIAN_POINT ( 'NONE',  ( 5.405949406249999534, 9.363379034771803333, -154.2812500020484094 ) ) ;
#38407 = CARTESIAN_POINT ( 'NONE',  ( -2.293366432827344421E-15, -12.48450537969573659, -48.21875000204836681 ) ) ;
#38408 = ORIENTED_EDGE ( 'NONE', *, *, #32845, .F. ) ;
#38409 = CARTESIAN_POINT ( 'NONE',  ( 10.00000000000000000, 5.773502691896255534, -21.37499999999997513 ) ) ;
#38410 = CLOSED_SHELL ( 'NONE', ( #16408, #17058, #21132, #27122, #36228, #3984, #3027, #25445, #21070, #27156, #6917, #41268, #35145, #27272, #182, #24201, #38415, #35959, #25875, #39532, #8274, #1424, #3496, #28983, #29625, #36715, #6741, #31536, #25154, #16839, #32268, #12610, #39671, #24682, #14997, #4647, #26695, #8488, #42541, #5406, #39960, #38754, #3808, #40896, #28321, #27531, #12062, #19354, #41853, #40837, #14571, #778, #21002, #40435, #6206, #40404, #19495, #26208, #19460, #11712, #27215, #10094, #17289, #1173, #23316, #22225, #29334, #25692, #10675, #21680, #18319, #29657, #17731, #26743, #32925, #1794, #20964, #33477, #23238, #13224, #35965, #22286, #35962, #28685, #21553, #31796, #10249, #10740, #36803, #12090, #39884, #34726, #30415, #35219, #29827, #6057, #37304, #6202, #34391, #9221, #38583, #14367, #29795, #2737, #54, #649, #38125, #7366, #4817, #21971, #40524, #25158, #18940, #137, #26577, #29019, #25751, #1368, #14544, #21321, #14837, #11681, #6695, #42034, #6682, #6988, #22398, #29620, #4881, #23053, #30994, #17417, #15806, #24691, #4201, #3559, #12872, #33164, #8013, #41492, #11621, #39640, #38624, #42014, #29013, #21803, #16158, #10363, #33043, #42690, #10126, #18130, #22783, #16096, #10362, #19732, #33088, #12449, #16928, #6803, #359, #12485, #39347, #36028, #7619, #905, #15750, #39368, #12642, #42570, #24379, #23543, #34008, #16386, #2333, #16190, #41221, #594, #35460, #678, #3777, #12452, #25185, #33756, #42438, #15141, #13811, #40198, #8833, #41258, #19885, #22334, #34776, #32809, #30172, #32687, #3537, #5728, #38503, #40950, #5363, #30472, #37027, #18810, #28270, #14231, #25392, #23876, #6310, #10843, #13456, #24508, #2977, #14335, #24132, #9438, #31275, #4899, #24623, #32507, #30855, #30166, #40606, #3013, #14459, #5074, #22503, #1490, #2467, #11138, #13297, #13993, #5132, #26812, #30197, #5670, #5019, #25292, #25639, #31604, #42464, #33940, #35443, #28612, #20642, #13280, #10718, #7694, #39902, #12398, #28616, #19870, #13047, #9617, #20583, #25178, #6040, #40719, #21358, #34480, #11263, #10118, #8774, #40178, #23426, #17472, #20028, #114, #29226, #24794, #6383, #27107, #12489, #2442, #894, #3055, #9540, #36758, #41738, #13869, #28813, #37029, #16574, #21889, #18879, #15032, #38216, #27803, #24640, #11194, #14602, #6719, #18006, #3329, #15690, #39382, #26047 ) ) ;
#38411 = CARTESIAN_POINT ( 'NONE',  ( 10.81189881249999551, -6.242252689847874514, -27.15625000204838102 ) ) ;
#38412 = CARTESIAN_POINT ( 'NONE',  ( 10.00000000000000000, 5.773502691896255534, -153.3750000000000000 ) ) ;
#38413 = CARTESIAN_POINT ( 'NONE',  ( 9.999999999999996447, -5.773502691896262640, -17.50000000409676559 ) ) ;
#38414 = CARTESIAN_POINT ( 'NONE',  ( 5.000000000000000000, 8.660254037844385522, -198.2500000000000000 ) ) ;
#38415 = ADVANCED_FACE ( 'NONE', ( #1853 ), #37228, .T. ) ;
#38417 = ORIENTED_EDGE ( 'NONE', *, *, #34413, .F. ) ;
#38416 = CARTESIAN_POINT ( 'NONE',  ( 5.405949406249992428, -9.363379034771808662, -123.2812500020483952 ) ) ;
#38418 = LINE ( 'NONE', #29775, #5557 ) ;
#38419 = CARTESIAN_POINT ( 'NONE',  ( -9.999999999999998224, 1.224646799147353059E-15, -45.12500000409677625 ) ) ;
#38420 = ORIENTED_EDGE ( 'NONE', *, *, #41768, .T. ) ;
#38421 = CARTESIAN_POINT ( 'NONE',  ( -10.81189881249999907, -6.242252689847864744, -56.15625000204837391 ) ) ;
#38422 = PERSON_AND_ORGANIZATION ( #11915, #17965 ) ;
#38423 = CARTESIAN_POINT ( 'NONE',  ( -10.81189881249999729, 6.242252689847871849, -110.2187500020483810 ) ) ;
#38425 = ORIENTED_EDGE ( 'NONE', *, *, #24323, .F. ) ;
#38424 = ORIENTED_EDGE ( 'NONE', *, *, #38102, .T. ) ;
#38426 = CARTESIAN_POINT ( 'NONE',  ( 9.999999999999998224, 0.000000000000000000, -83.37500000409677625 ) ) ;
#38427 = DIRECTION ( 'NONE',  ( 1.000000000000000000, 0.000000000000000000, 0.000000000000000000 ) ) ;
#38428 = CARTESIAN_POINT ( 'NONE',  ( -10.81189881249999907, -6.242252689847864744, -159.4687500020484094 ) ) ;
#38429 = CARTESIAN_POINT ( 'NONE',  ( -2.293366432827344421E-15, -12.48450537969573659, -187.9062500020484094 ) ) ;
#38430 = CARTESIAN_POINT ( 'NONE',  ( -5.405949406249996869, 9.363379034771805109, -6.843750002048371250 ) ) ;
#38431 = CARTESIAN_POINT ( 'NONE',  ( 5.405949406249992428, -9.363379034771808662, -142.5937500020483810 ) ) ;
#38432 = CARTESIAN_POINT ( 'NONE',  ( -5.405949406250003975, -9.363379034771801557, -108.3437500020483810 ) ) ;
#38433 = CARTESIAN_POINT ( 'NONE',  ( -9.999999999999998224, 1.224646799147353059E-15, -150.1250000040967905 ) ) ;
#38434 = CARTESIAN_POINT ( 'NONE',  ( 10.81189881249999729, 0.000000000000000000, -114.0312500020483952 ) ) ;
#38435 = CARTESIAN_POINT ( 'NONE',  ( 5.000000000000000000, 8.660254037844385522, -198.6250000040967905 ) ) ;
#38436 = CARTESIAN_POINT ( 'NONE',  ( 5.405949406249992428, -9.363379034771808662, -126.0937500020483668 ) ) ;
#38437 = CARTESIAN_POINT ( 'NONE',  ( 5.405949406249992428, -9.363379034771808662, -198.2812500020484094 ) ) ;
#38438 = CARTESIAN_POINT ( 'NONE',  ( -4.999999999999996447, 8.660254037844387298, -148.5000000000000000 ) ) ;
#38439 = CARTESIAN_POINT ( 'NONE',  ( 5.000000000000000000, 8.660254037844385522, -12.24999999999995559 ) ) ;
#38440 = CARTESIAN_POINT ( 'NONE',  ( -5.405949406250003975, -9.363379034771801557, -67.84375000204836681 ) ) ;
#38441 = CARTESIAN_POINT ( 'NONE',  ( -2.293366432827344421E-15, -12.48450537969573659, -60.21875000204837391 ) ) ;
#38442 = CARTESIAN_POINT ( 'NONE',  ( -2.121150477449813534E-15, -11.54700538379251284, -187.2500000040967905 ) ) ;
#38443 = CARTESIAN_POINT ( 'NONE',  ( 5.405949406249999534, 9.363379034771803333, -25.28125000204836681 ) ) ;
#38444 = AXIS2_PLACEMENT_3D ( 'NONE', #23254, #19786, #3623 ) ;
#38445 = CARTESIAN_POINT ( 'NONE',  ( 7.644554776091147741E-16, 12.48450537969573659, -36.96875000204835260 ) ) ;
#38446 = CARTESIAN_POINT ( 'NONE',  ( -4.999999999999996447, 8.660254037844387298, -31.87500000409676559 ) ) ;
#38447 = CARTESIAN_POINT ( 'NONE',  ( 5.405949406249999534, 9.363379034771803333, -145.0937500020483810 ) ) ;
#38448 = CARTESIAN_POINT ( 'NONE',  ( 9.999999999999996447, -5.773502691896262640, -113.1250000000000000 ) ) ;
#38449 = VECTOR ( 'NONE', #2090, 1000.000000000000000 ) ;
#38450 = CARTESIAN_POINT ( 'NONE',  ( -4.999999999999996447, 8.660254037844387298, -136.5000000000000000 ) ) ;
#38451 = CARTESIAN_POINT ( 'NONE',  ( -9.999999999999998224, 5.773502691896259087, -76.37499999999998579 ) ) ;
#38452 = CARTESIAN_POINT ( 'NONE',  ( -10.81189881249999907, -6.242252689847864744, -141.6562500020483810 ) ) ;
#38453 = CARTESIAN_POINT ( 'NONE',  ( -10.81189881249999729, 6.242252689847871849, -9.906250002048379244 ) ) ;
#38454 = ORIENTED_EDGE ( 'NONE', *, *, #13812, .F. ) ;
#38455 = CARTESIAN_POINT ( 'NONE',  ( -9.999999999999998224, 1.224646799147353059E-15, -50.74999999999996447 ) ) ;
#38456 = CARTESIAN_POINT ( 'NONE',  ( 10.00000000000000000, 5.773502691896255534, -117.7500000040967905 ) ) ;
#38457 = CARTESIAN_POINT ( 'NONE',  ( -2.121150477449813534E-15, -11.54700538379251284, -128.3750000000000000 ) ) ;
#38458 = CARTESIAN_POINT ( 'NONE',  ( -10.81189881249999729, 6.242252689847871849, -74.21875000204836681 ) ) ;
#38459 = CARTESIAN_POINT ( 'NONE',  ( -5.000000000000003553, -8.660254037844383745, -41.49999999999997868 ) ) ;
#38460 = CARTESIAN_POINT ( 'NONE',  ( 5.000000000000000000, 8.660254037844385522, -26.12500000409675849 ) ) ;
#38461 =( BOUNDED_CURVE ( )  B_SPLINE_CURVE ( 2, ( #2866, #15997, #2246, #8916, #5250, #29192, #28567 ),
 .UNSPECIFIED., .F., .F. ) 
 B_SPLINE_CURVE_WITH_KNOTS ( ( 3, 2, 2, 3 ),
 ( 0.3134328358208955390, 0.3146766169154229242, 0.3159203980099503650, 0.3171641791044778058 ),
 .UNSPECIFIED. ) 
 CURVE ( )  GEOMETRIC_REPRESENTATION_ITEM ( )  RATIONAL_B_SPLINE_CURVE ( ( 1.000000000000000000, 0.8660254037844387076, 1.000000000000000000, 0.8660254037844387076, 1.000000000000000000, 0.8660254037844207220, 1.000000000000017986 ) ) 
 REPRESENTATION_ITEM ( '' )  );
#38462 = CARTESIAN_POINT ( 'NONE',  ( -9.999999999999872102, -5.773502691896326589, -157.5000000040968189 ) ) ;
#38463 = CARTESIAN_POINT ( 'NONE',  ( 10.81189881249999551, -6.242252689847874514, -37.65625000204836681 ) ) ;
#38464 = CARTESIAN_POINT ( 'NONE',  ( 9.999999999999998224, 0.000000000000000000, -80.37500000409677625 ) ) ;
#38465 = CARTESIAN_POINT ( 'NONE',  ( -10.81189881249999907, -6.242252689847864744, -144.6562500020484094 ) ) ;
#38466 = CARTESIAN_POINT ( 'NONE',  ( 10.81189881249999729, 0.000000000000000000, -147.0312500020483810 ) ) ;
#38467 = CARTESIAN_POINT ( 'NONE',  ( 9.999999999999998224, 0.000000000000000000, -126.8750000040967905 ) ) ;
#38468 = ORIENTED_EDGE ( 'NONE', *, *, #34188, .F. ) ;
#38469 = VERTEX_POINT ( 'NONE', #11532 ) ;
#38470 = AXIS2_PLACEMENT_3D ( 'NONE', #34682, #20851, #21280 ) ;
#38471 = ORIENTED_EDGE ( 'NONE', *, *, #30471, .F. ) ;
#38472 = EDGE_CURVE ( 'NONE', #17679, #107, #2963, .T. ) ;
#38473 = CYLINDRICAL_SURFACE ( 'NONE', #29076, 9.999999999999998224 ) ;
#38474 = CARTESIAN_POINT ( 'NONE',  ( 7.644554776091147741E-16, 12.48450537969573659, -177.9687500020483810 ) ) ;
#38475 = CARTESIAN_POINT ( 'NONE',  ( 7.644554776091147741E-16, 12.48450537969573659, -32.46875000204835970 ) ) ;
#38476 = CYLINDRICAL_SURFACE ( 'NONE', #28135, 9.999999999999998224 ) ;
#38477 = CARTESIAN_POINT ( 'NONE',  ( -5.405949406249996869, 9.363379034771805109, -164.3437500020484094 ) ) ;
#38478 = CARTESIAN_POINT ( 'NONE',  ( -10.81189881249999729, 1.324075727343319199E-15, -155.0937500020483810 ) ) ;
#38479 = DIRECTION ( 'NONE',  ( -0.000000000000000000, -0.000000000000000000, 1.000000000000000000 ) ) ;
#38480 = CARTESIAN_POINT ( 'NONE',  ( -5.405949406249996869, 9.363379034771805109, -134.3437500020484094 ) ) ;
#38481 = CARTESIAN_POINT ( 'NONE',  ( 10.81189881249999551, -6.242252689847874514, -136.6562500020484094 ) ) ;
#38482 = CARTESIAN_POINT ( 'NONE',  ( 9.999999999999998224, 0.000000000000000000, -3.499999999999975131 ) ) ;
#38483 = CARTESIAN_POINT ( 'NONE',  ( 10.81189881249999729, 0.000000000000000000, -146.8437500020483810 ) ) ;
#38484 = LINE ( 'NONE', #18849, #28168 ) ;
#38485 = CARTESIAN_POINT ( 'NONE',  ( 9.999999999999479527, 5.773502691896553074, -33.75000000409673362 ) ) ;
#38486 = CARTESIAN_POINT ( 'NONE',  ( 5.000000000000000000, 8.660254037844385522, -172.7500000000000284 ) ) ;
#38487 = CARTESIAN_POINT ( 'NONE',  ( 5.405949406249999534, 9.363379034771803333, -77.59375000204838102 ) ) ;
#38488 = CARTESIAN_POINT ( 'NONE',  ( 9.999999999999998224, 1.224646799147353059E-15, -99.99999999999998579 ) ) ;
#38489 = CARTESIAN_POINT ( 'NONE',  ( -5.405949406249996869, 9.363379034771805109, -52.03125000204835970 ) ) ;
#38490 = DIRECTION ( 'NONE',  ( -0.000000000000000000, -0.000000000000000000, 1.000000000000000000 ) ) ;
#38491 = CARTESIAN_POINT ( 'NONE',  ( -10.81189881249999729, 6.242252689847871849, -173.2187500020483810 ) ) ;
#38492 = CARTESIAN_POINT ( 'NONE',  ( 9.999999999999998224, 0.000000000000000000, -140.0000000000000000 ) ) ;
#38493 = CARTESIAN_POINT ( 'NONE',  ( -10.81189881249999729, 6.242252689847871849, -143.4062500020484094 ) ) ;
#38494 = CYLINDRICAL_SURFACE ( 'NONE', #20632, 9.999999999999998224 ) ;
#38495 = CARTESIAN_POINT ( 'NONE',  ( 5.405949406249992428, -9.363379034771808662, -34.78125000204837391 ) ) ;
#38496 = CARTESIAN_POINT ( 'NONE',  ( 9.999999999999998224, 0.000000000000000000, -120.8750000040967905 ) ) ;
#38497 = CARTESIAN_POINT ( 'NONE',  ( 7.070501591499377789E-16, 11.54700538379251284, -99.12500000000000000 ) ) ;
#38498 =( BOUNDED_CURVE ( )  B_SPLINE_CURVE ( 2, ( #6649, #7079, #36633, #16979, #3844, #9883, #36844 ),
 .UNSPECIFIED., .F., .F. ) 
 B_SPLINE_CURVE_WITH_KNOTS ( ( 3, 2, 2, 3 ),
 ( 0.7201492537313435305, 0.7213930348258709158, 0.7226368159203983010, 0.7238805970149256863 ),
 .UNSPECIFIED. ) 
 CURVE ( )  GEOMETRIC_REPRESENTATION_ITEM ( )  RATIONAL_B_SPLINE_CURVE ( ( 0.9999999999999761302, 0.8660254037844625774, 1.000000000000000000, 0.8660254037844387076, 1.000000000000000000, 0.8660254037844028474, 1.000000000000035971 ) ) 
 REPRESENTATION_ITEM ( '' )  );
#38499 = EDGE_LOOP ( 'NONE', ( #42260, #35721, #17134, #32715 ) ) ;
#38500 = CARTESIAN_POINT ( 'NONE',  ( -10.81189881249999729, -6.242252689847864744, -116.1562500020483952 ) ) ;
#38501 = CARTESIAN_POINT ( 'NONE',  ( 7.070501591499377789E-16, 11.54700538379251284, -140.0000000040968189 ) ) ;
#38502 = DIRECTION ( 'NONE',  ( -0.000000000000000000, -0.000000000000000000, 1.000000000000000000 ) ) ;
#38503 = ADVANCED_FACE ( 'NONE', ( #25997 ), #42370, .T. ) ;
#38504 = CARTESIAN_POINT ( 'NONE',  ( 5.405949406249999534, 9.363379034771803333, -170.7812500020484094 ) ) ;
#38505 = CARTESIAN_POINT ( 'NONE',  ( 9.999999999999996447, -5.773502691896262640, -52.00000000409676915 ) ) ;
#38506 = AXIS2_PLACEMENT_3D ( 'NONE', #10774, #17453, #23963 ) ;
#38507 = CARTESIAN_POINT ( 'NONE',  ( -10.81189881249999907, -6.242252689847864744, -65.15625000204838102 ) ) ;
#38508 = CARTESIAN_POINT ( 'NONE',  ( 7.070501591499376803E-16, 11.54700538379251284, -9.500000004096756712 ) ) ;
#38509 = CARTESIAN_POINT ( 'NONE',  ( -10.81189881249999907, -6.242252689847864744, -167.1562500020483810 ) ) ;
#38510 = CARTESIAN_POINT ( 'NONE',  ( 9.999999999999998224, 0.000000000000000000, -7.999999999999952038 ) ) ;
#38511 = CARTESIAN_POINT ( 'NONE',  ( 9.999999999999998224, 0.000000000000000000, -33.87500000409676915 ) ) ;
#38512 = VERTEX_POINT ( 'NONE', #9579 ) ;
#38513 = CARTESIAN_POINT ( 'NONE',  ( 80.00000000000002842, 39.99999999999999289, -160.0000000000000000 ) ) ;
#38514 = CARTESIAN_POINT ( 'NONE',  ( 7.070501591499376803E-16, 11.54700538379251284, -123.5000000040967905 ) ) ;
#38515 = FACE_OUTER_BOUND ( 'NONE', #33238, .T. ) ;
#38517 = ORIENTED_EDGE ( 'NONE', *, *, #16442, .F. ) ;
#38516 = CARTESIAN_POINT ( 'NONE',  ( -10.81189881249999729, 1.324075727343319199E-15, -81.78125000204839523 ) ) ;
#38518 = CARTESIAN_POINT ( 'NONE',  ( 0.000000000000000000, 0.000000000000000000, 0.000000000000000000 ) ) ;
#38520 = ORIENTED_EDGE ( 'NONE', *, *, #15084, .F. ) ;
#38519 = CARTESIAN_POINT ( 'NONE',  ( -9.999999999999998224, 1.224646799147353059E-15, -143.7500000000000000 ) ) ;
#38521 = ORIENTED_EDGE ( 'NONE', *, *, #9018, .T. ) ;
#38522 = CARTESIAN_POINT ( 'NONE',  ( 5.405949406249999534, 9.363379034771803333, -31.09375000204836326 ) ) ;
#38523 = CARTESIAN_POINT ( 'NONE',  ( 9.999999999999998224, 0.000000000000000000, -52.99999999999996447 ) ) ;
#38524 = CARTESIAN_POINT ( 'NONE',  ( -2.293366432827344421E-15, -12.48450537969573659, -6.406250002048362369 ) ) ;
#38526 = ORIENTED_EDGE ( 'NONE', *, *, #9068, .F. ) ;
#38525 = CARTESIAN_POINT ( 'NONE',  ( 10.81189881249999551, -6.242252689847874514, -53.96875000204838102 ) ) ;
#38527 = EDGE_CURVE ( 'NONE', #17561, #17891, #34987, .T. ) ;
#38528 = CARTESIAN_POINT ( 'NONE',  ( 9.999999999999996447, -5.773502691896262640, -33.62499999999995737 ) ) ;
#38529 = CARTESIAN_POINT ( 'NONE',  ( -10.81189881249999729, 6.242252689847871849, -189.7187500020484379 ) ) ;
#38530 = CARTESIAN_POINT ( 'NONE',  ( -5.405949406250003975, -9.363379034771801557, -178.8437500020483810 ) ) ;
#38531 = CARTESIAN_POINT ( 'NONE',  ( 5.405949406249992428, -9.363379034771808662, -157.5937500020483810 ) ) ;
#38532 = CARTESIAN_POINT ( 'NONE',  ( 10.81189881249999551, -6.242252689847874514, -166.4687500020483810 ) ) ;
#38533 = CARTESIAN_POINT ( 'NONE',  ( -9.999999999999998224, 1.224646799147353059E-15, -72.12500000409677625 ) ) ;
#38534 = CARTESIAN_POINT ( 'NONE',  ( -6.964452268037473637, 6.964452268037472749, -201.2186212422413689 ) ) ;
#38535 = CARTESIAN_POINT ( 'NONE',  ( -2.121150477449813534E-15, -11.54700538379251284, -195.8750000000000284 ) ) ;
#38536 = VECTOR ( 'NONE', #39599, 1000.000000000000000 ) ;
#38537 = CARTESIAN_POINT ( 'NONE',  ( -5.405949406249996869, 9.363379034771805109, -101.3437500020483810 ) ) ;
#38538 = CARTESIAN_POINT ( 'NONE',  ( 9.999999999998969713, 5.773502691896851502, -18.37499999999995026 ) ) ;
#38539 = CARTESIAN_POINT ( 'NONE',  ( -10.81189881249999729, 1.324075727343319199E-15, -75.78125000204838102 ) ) ;
#38540 = CARTESIAN_POINT ( 'NONE',  ( -5.405949406249996869, 9.363379034771805109, -90.84375000204838102 ) ) ;
#38541 = CARTESIAN_POINT ( 'NONE',  ( 10.81189881249999907, 6.242252689847868297, -64.40625000204839523 ) ) ;
#38542 = CARTESIAN_POINT ( 'NONE',  ( 5.000000000000000000, 8.660254037844385522, -149.1250000040967905 ) ) ;
#38543 = CARTESIAN_POINT ( 'NONE',  ( 4.999999999999992006, -8.660254037844389075, -120.7500000000000000 ) ) ;
#38544 = ORIENTED_EDGE ( 'NONE', *, *, #32330, .F. ) ;
#38545 = CARTESIAN_POINT ( 'NONE',  ( -10.81189881249999729, 1.324075727343319199E-15, -141.7812500020483810 ) ) ;
#38546 = CARTESIAN_POINT ( 'NONE',  ( 7.644554776091147741E-16, 12.48450537969573659, -164.6562500020484094 ) ) ;
#38547 = CARTESIAN_POINT ( 'NONE',  ( 22.00000000000000711, 2.877919977996280320E-15, -99.99999999999998579 ) ) ;
#38548 = CARTESIAN_POINT ( 'NONE',  ( 10.00000000000102318, -5.773502691895667560, -51.62499999999995737 ) ) ;
#38549 = CARTESIAN_POINT ( 'NONE',  ( 10.81189881249999729, 0.000000000000000000, -88.34375000204838102 ) ) ;
#38550 = EDGE_LOOP ( 'NONE', ( #21630, #32071, #12292, #26985, #7468, #31217, #36503, #28614, #8652, #7181, #24956, #15320, #20514, #25049, #40152, #29937, #297, #13756, #26581, #887, #3101, #35831, #20945, #22425, #33442, #5621, #41957, #21696, #32841, #7256, #18277, #30887, #34556, #37729, #34919, #28641, #24524, #28497, #14765, #42329, #34392, #2389, #23287, #31639, #10582, #31621, #38899, #26371, #8214, #38900, #10908, #39840, #26477, #637, #21597, #17844, #25404, #34673, #40977, #42228, #37457, #31948, #30287, #11648, #42212, #24515, #19185, #37163, #20777, #14394, #14177, #26320, #37921, #9999, #38335, #11273, #3119, #17467, #946, #21697, #18479, #18655, #29085, #41643, #36975, #31666, #1051, #36162, #13433, #36236, #9256, #8476, #19823, #1699, #34762, #5400, #8367, #17693, #13436, #34346, #19410, #16342, #25791, #13018, #18882, #1576, #14827, #18133, #142, #1745 ) ) ;
#38551 = CARTESIAN_POINT ( 'NONE',  ( 9.999999999999998224, 0.000000000000000000, -61.99999999999997158 ) ) ;
#38552 = CARTESIAN_POINT ( 'NONE',  ( 10.81189881249999907, 6.242252689847868297, -193.2187500020484094 ) ) ;
#38553 = CARTESIAN_POINT ( 'NONE',  ( -5.000000000000003553, -8.660254037844383745, -71.87500000409677625 ) ) ;
#38554 = DIRECTION ( 'NONE',  ( -0.000000000000000000, -0.000000000000000000, -1.000000000000000000 ) ) ;
#38555 = CYLINDRICAL_SURFACE ( 'NONE', #4503, 9.999999999999998224 ) ;
#38556 = CARTESIAN_POINT ( 'NONE',  ( 10.81189881249999729, 0.000000000000000000, -96.03125000204838102 ) ) ;
#38557 = CARTESIAN_POINT ( 'NONE',  ( 5.405949406249999534, 9.363379034771803333, -67.28125000204838102 ) ) ;
#38558 = CARTESIAN_POINT ( 'NONE',  ( -9.999999999999998224, 1.224646799147353059E-15, -67.62500000409676204 ) ) ;
#38559 = CARTESIAN_POINT ( 'NONE',  ( -2.121150477449813534E-15, -11.54700538379251284, -77.75000000409677625 ) ) ;
#38560 = CARTESIAN_POINT ( 'NONE',  ( -10.81189881249999729, 1.324075727343319199E-15, -23.09375000204835615 ) ) ;
#38561 = VERTEX_POINT ( 'NONE', #34868 ) ;
#38562 = CARTESIAN_POINT ( 'NONE',  ( 10.81189881249999729, 0.000000000000000000, -193.5312500020484094 ) ) ;
#38563 = CARTESIAN_POINT ( 'NONE',  ( -10.81189881249999729, 6.242252689847871849, -20.40625000204837391 ) ) ;
#38564 = CARTESIAN_POINT ( 'NONE',  ( -5.405949406250003975, -9.363379034771801557, -9.343750002048345493 ) ) ;
#38565 = CARTESIAN_POINT ( 'NONE',  ( -10.00000000000076916, 5.773502691895813221, -136.7500000040967620 ) ) ;
#38566 = CARTESIAN_POINT ( 'NONE',  ( -9.999999999999998224, 1.224646799147353059E-15, -37.62500000409676915 ) ) ;
#38567 = CARTESIAN_POINT ( 'NONE',  ( 9.999999999999998224, 0.000000000000000000, -147.5000000000000000 ) ) ;
#38568 = CARTESIAN_POINT ( 'NONE',  ( 9.999999999999996447, -5.773502691896262640, -173.1250000000000000 ) ) ;
#38569 = DIRECTION ( 'NONE',  ( 1.000000000000000000, 0.000000000000000000, 0.000000000000000000 ) ) ;
#38570 = VECTOR ( 'NONE', #14173, 1000.000000000000000 ) ;
#38572 = VERTEX_POINT ( 'NONE', #2067 ) ;
#38571 = CARTESIAN_POINT ( 'NONE',  ( 10.81189881249999551, -6.242252689847874514, -105.1562500020483810 ) ) ;
#38573 = DIRECTION ( 'NONE',  ( -0.000000000000000000, -0.000000000000000000, 1.000000000000000000 ) ) ;
#38574 = ORIENTED_EDGE ( 'NONE', *, *, #42648, .T. ) ;
#38575 = ORIENTED_EDGE ( 'NONE', *, *, #8798, .T. ) ;
#38576 = AXIS2_PLACEMENT_3D ( 'NONE', #14528, #34847, #9147 ) ;
#38577 = CARTESIAN_POINT ( 'NONE',  ( -5.405949406250003975, -9.363379034771801557, -27.53125000204836681 ) ) ;
#38578 = CARTESIAN_POINT ( 'NONE',  ( 7.644554776091147741E-16, 12.48450537969573659, -80.46875000204838102 ) ) ;
#38579 = DIRECTION ( 'NONE',  ( -0.000000000000000000, -0.000000000000000000, 1.000000000000000000 ) ) ;
#38580 = EDGE_CURVE ( 'NONE', #27810, #17561, #41734, .T. ) ;
#38581 = CARTESIAN_POINT ( 'NONE',  ( 6.703084383986223749, 8.205311082841122428, -100.0000000000000000 ) ) ;
#38582 =( BOUNDED_CURVE ( )  B_SPLINE_CURVE ( 2, ( #20772, #33961, #17734, #17310, #40392, #36752, #940 ),
 .UNSPECIFIED., .F., .F. ) 
 B_SPLINE_CURVE_WITH_KNOTS ( ( 3, 2, 2, 3 ),
 ( 0.2649253731343284568, 0.2661691542288558421, 0.2674129353233831718, 0.2686567164179105571 ),
 .UNSPECIFIED. ) 
 CURVE ( )  GEOMETRIC_REPRESENTATION_ITEM ( )  RATIONAL_B_SPLINE_CURVE ( ( 0.9999999999999880096, 0.8660254037844506980, 1.000000000000000000, 0.8660254037844387076, 1.000000000000000000, 0.8660254037844267172, 1.000000000000011990 ) ) 
 REPRESENTATION_ITEM ( '' )  );
#38583 = ADVANCED_FACE ( 'NONE', ( #15407 ), #12173, .T. ) ;
#38584 = EDGE_CURVE ( 'NONE', #5784, #5415, #32057, .T. ) ;
#38585 = DIRECTION ( 'NONE',  ( -0.000000000000000000, -1.000000000000000000, -0.000000000000000000 ) ) ;
#38586 = CARTESIAN_POINT ( 'NONE',  ( -4.999999999999996447, 8.660254037844387298, -30.37500000409676204 ) ) ;
#38587 = CARTESIAN_POINT ( 'NONE',  ( 5.405949406249999534, 9.363379034771803333, -152.7812500020484094 ) ) ;
#38588 = CARTESIAN_POINT ( 'NONE',  ( 4.999999999999992006, -8.660254037844389075, -8.625000004096744277 ) ) ;
#38589 = CARTESIAN_POINT ( 'NONE',  ( -9.999999999998969713, -5.773502691896847949, -86.62499999999995737 ) ) ;
#38590 = CARTESIAN_POINT ( 'NONE',  ( -10.81189881249999907, -6.242252689847864744, -129.4687500020483810 ) ) ;
#38591 = CARTESIAN_POINT ( 'NONE',  ( 10.81189881249999729, 0.000000000000000000, -119.8437500020483810 ) ) ;
#38592 = CC_DESIGN_PERSON_AND_ORGANIZATION_ASSIGNMENT ( #1488, #31703, ( #36620 ) ) ;
#38593 = CARTESIAN_POINT ( 'NONE',  ( 5.405949406249999534, 9.363379034771803333, -82.09375000204836681 ) ) ;
#38594 = CARTESIAN_POINT ( 'NONE',  ( -10.81189881249999729, 6.242252689847871849, -95.40625000204838102 ) ) ;
#38595 = CARTESIAN_POINT ( 'NONE',  ( -9.999999999999998224, 5.773502691896259087, -171.2500000040967905 ) ) ;
#38596 = CARTESIAN_POINT ( 'NONE',  ( -2.293366432827344421E-15, -12.48450537969573659, -171.4062500020484379 ) ) ;
#38597 = CARTESIAN_POINT ( 'NONE',  ( 9.999999999999998224, 0.000000000000000000, -132.8750000040967905 ) ) ;
#38598 = CARTESIAN_POINT ( 'NONE',  ( -2.293366432827344421E-15, -12.48450537969573659, -175.9062500020484379 ) ) ;
#38599 = CARTESIAN_POINT ( 'NONE',  ( 7.644554776091147741E-16, 12.48450537969573659, -190.1562500020484094 ) ) ;
#38600 = CARTESIAN_POINT ( 'NONE',  ( -10.81189881249999729, -6.242252689847864744, -45.46875000204837391 ) ) ;
#38601 = VECTOR ( 'NONE', #13912, 1000.000000000000000 ) ;
#38602 = CARTESIAN_POINT ( 'NONE',  ( 9.999999999999996447, -5.773502691896262640, -164.5000000040967905 ) ) ;
#38603 = CARTESIAN_POINT ( 'NONE',  ( -10.00000000000102496, 5.773502691895664007, -85.75000000409671941 ) ) ;
#38604 = CARTESIAN_POINT ( 'NONE',  ( 7.644554776091147741E-16, 12.48450537969573659, -12.96875000204836503 ) ) ;
#38605 = CARTESIAN_POINT ( 'NONE',  ( 9.999999999999742428, 5.773502691896404748, -162.7500000040968189 ) ) ;
#38606 = CARTESIAN_POINT ( 'NONE',  ( -5.405949406250003975, -9.363379034771801557, -118.8437500020483810 ) ) ;
#38607 = CARTESIAN_POINT ( 'NONE',  ( 4.999999999999992006, -8.660254037844389075, -87.74999999999998579 ) ) ;
#38608 = CARTESIAN_POINT ( 'NONE',  ( -10.81189881249999907, -6.242252689847864744, -17.15625000204837391 ) ) ;
#38609 = CARTESIAN_POINT ( 'NONE',  ( 9.999999999999998224, 0.000000000000000000, -99.87500000409679046 ) ) ;
#38610 = EDGE_CURVE ( 'NONE', #3867, #5197, #14775, .T. ) ;
#38611 = DIRECTION ( 'NONE',  ( -1.000000000000000000, 0.000000000000000000, 0.000000000000000000 ) ) ;
#38612 = CARTESIAN_POINT ( 'NONE',  ( -10.81189881249999729, 1.324075727343319199E-15, -119.2812500020483952 ) ) ;
#38613 = CARTESIAN_POINT ( 'NONE',  ( -10.81189881249999729, 1.324075727343319199E-15, -87.78125000204838102 ) ) ;
#38614 = ORIENTED_EDGE ( 'NONE', *, *, #37259, .F. ) ;
#38615 = CARTESIAN_POINT ( 'NONE',  ( -9.999999999999998224, 5.773502691896259087, -90.25000000409676204 ) ) ;
#38616 = CARTESIAN_POINT ( 'NONE',  ( 9.999999999998969713, 5.773502691896851502, -4.874999999999934275 ) ) ;
#38617 = CARTESIAN_POINT ( 'NONE',  ( -10.81189881249999729, 1.324075727343319199E-15, -159.7812500020484094 ) ) ;
#38618 = CARTESIAN_POINT ( 'NONE',  ( 10.81189881249999907, 6.242252689847868297, -47.71875000204835970 ) ) ;
#38620 = EDGE_CURVE ( 'NONE', #34021, #35538, #26153, .T. ) ;
#38619 = ORIENTED_EDGE ( 'NONE', *, *, #19334, .T. ) ;
#38621 = CARTESIAN_POINT ( 'NONE',  ( 7.070501591499377789E-16, 11.54700538379251284, -13.62499999999996803 ) ) ;
#38622 = CARTESIAN_POINT ( 'NONE',  ( 7.644554776091147741E-16, 12.48450537969573659, -25.15625000204838813 ) ) ;
#38623 = CARTESIAN_POINT ( 'NONE',  ( 10.00000000000000000, 5.773502691896255534, -150.3750000000000000 ) ) ;
#38624 = ADVANCED_FACE ( 'NONE', ( #5932 ), #15825, .T. ) ;
#38625 = CARTESIAN_POINT ( 'NONE',  ( -2.121150477449813534E-15, -11.54700538379251284, -23.75000000409676915 ) ) ;
#38626 = CARTESIAN_POINT ( 'NONE',  ( -9.999999999999998224, 1.224646799147353059E-15, -197.7500000000000000 ) ) ;
#38628 = VERTEX_POINT ( 'NONE', #29022 ) ;
#38627 = CARTESIAN_POINT ( 'NONE',  ( 5.405949406249999534, 9.363379034771803333, -127.2812500020483810 ) ) ;
#38629 = CARTESIAN_POINT ( 'NONE',  ( 7.070501591499376803E-16, 11.54700538379251284, -65.00000000409677625 ) ) ;
#38630 = EDGE_CURVE ( 'NONE', #1539, #16629, #11760, .T. ) ;
#38631 = ORIENTED_EDGE ( 'NONE', *, *, #19278, .F. ) ;
#38632 =( BOUNDED_CURVE ( )  B_SPLINE_CURVE ( 2, ( #21414, #35028, #28124, #40607, #5457, #31579, #18607 ),
 .UNSPECIFIED., .F., .F. ) 
 B_SPLINE_CURVE_WITH_KNOTS ( ( 3, 2, 2, 3 ),
 ( 0.9738805970149255753, 0.9751243781094529606, 0.9763681592039802348, 0.9776119402985076201 ),
 .UNSPECIFIED. ) 
 CURVE ( )  GEOMETRIC_REPRESENTATION_ITEM ( )  RATIONAL_B_SPLINE_CURVE ( ( 0.9999999999999761302, 0.8660254037844625774, 1.000000000000000000, 0.8660254037844387076, 1.000000000000000000, 0.8660254037844267172, 1.000000000000011990 ) ) 
 REPRESENTATION_ITEM ( '' )  );
#38633 = CARTESIAN_POINT ( 'NONE',  ( -5.405949406250003975, -9.363379034771801557, -51.53125000204835970 ) ) ;
#38634 = DATE_AND_TIME ( #35197, #38021 ) ;
#38635 = CIRCLE ( 'NONE', #33804, 20.00000000000000355 ) ;
#38636 = CARTESIAN_POINT ( 'NONE',  ( 7.644554776091147741E-16, 12.48450537969573659, -104.4687500020483668 ) ) ;
#38638 = VERTEX_POINT ( 'NONE', #19713 ) ;
#38637 = ORIENTED_EDGE ( 'NONE', *, *, #33743, .F. ) ;
#38639 = CARTESIAN_POINT ( 'NONE',  ( 9.999999999999998224, 0.000000000000000000, -125.3750000040967905 ) ) ;
#38640 = CARTESIAN_POINT ( 'NONE',  ( -9.999999999999982236, -5.773502691896262640, -198.0000000040968473 ) ) ;
#38642 = EDGE_CURVE ( 'NONE', #4750, #27209, #6557, .T. ) ;
#38641 = CARTESIAN_POINT ( 'NONE',  ( -10.81189881249999729, 1.324075727343319199E-15, -156.5937500020483810 ) ) ;
#38643 =( BOUNDED_CURVE ( )  B_SPLINE_CURVE ( 2, ( #19285, #42369, #32684, #29868, #22752, #12801, #309 ),
 .UNSPECIFIED., .F., .F. ) 
 B_SPLINE_CURVE_WITH_KNOTS ( ( 3, 2, 2, 3 ),
 ( 0.4925373134328359104, 0.4937810945273632957, 0.4950248756218906809, 0.4962686567164180107 ),
 .UNSPECIFIED. ) 
 CURVE ( )  GEOMETRIC_REPRESENTATION_ITEM ( )  RATIONAL_B_SPLINE_CURVE ( ( 0.9999999999999880096, 0.8660254037844506980, 1.000000000000000000, 0.8660254037844387076, 1.000000000000000000, 0.8660254037844267172, 1.000000000000011990 ) ) 
 REPRESENTATION_ITEM ( '' )  );
#38644 = CARTESIAN_POINT ( 'NONE',  ( -2.293366432827344421E-15, -12.48450537969573659, -190.9062500020483810 ) ) ;
#38645 = CARTESIAN_POINT ( 'NONE',  ( -5.405949406249996869, 9.363379034771805109, -3.843750002048368586 ) ) ;
#38646 = CARTESIAN_POINT ( 'NONE',  ( 10.81189881249999551, -6.242252689847874514, -139.4687500020483810 ) ) ;
#38647 = CARTESIAN_POINT ( 'NONE',  ( -2.293366432827344421E-15, -12.48450537969573659, -111.2187500020483668 ) ) ;
#38648 = DIRECTION ( 'NONE',  ( -0.08682659386424779191, -0.08682659386424779191, 0.9924325091389669673 ) ) ;
#38649 = CARTESIAN_POINT ( 'NONE',  ( -5.405949406250003975, -9.363379034771801557, -116.0312500020483952 ) ) ;
#38650 = CARTESIAN_POINT ( 'NONE',  ( 10.00000000000000000, 5.773502691896255534, -195.7500000040968189 ) ) ;
#38651 = CARTESIAN_POINT ( 'NONE',  ( -5.405949406250003975, -9.363379034771801557, -120.3437500020483952 ) ) ;
#38652 = CARTESIAN_POINT ( 'NONE',  ( 10.81189881249999551, -6.242252689847874514, -198.1562500020484379 ) ) ;
#38653 = DIRECTION ( 'NONE',  ( 1.000000000000000000, 0.000000000000000000, 0.000000000000000000 ) ) ;
#38654 = CARTESIAN_POINT ( 'NONE',  ( -10.00000000000000000, -5.773502691896251982, -137.6250000000000000 ) ) ;
#38655 = CARTESIAN_POINT ( 'NONE',  ( -10.00000000000000000, -5.773502691896251982, -14.62499999999996980 ) ) ;
#38656 = CARTESIAN_POINT ( 'NONE',  ( 10.81189881249999551, -6.242252689847874514, -71.96875000204836681 ) ) ;
#38657 = CARTESIAN_POINT ( 'NONE',  ( -10.81189881249999729, 1.324075727343319199E-15, -56.09375000204835970 ) ) ;
#38658 = CARTESIAN_POINT ( 'NONE',  ( -5.000000000000003553, -8.660254037844383745, -191.8750000040967905 ) ) ;
#38659 = CARTESIAN_POINT ( 'NONE',  ( 7.644554776091147741E-16, 12.48450537969573659, -28.15625000204838457 ) ) ;
#38660 = CARTESIAN_POINT ( 'NONE',  ( 7.644554776091147741E-16, 12.48450537969573659, -35.46875000204835260 ) ) ;
#38661 = CARTESIAN_POINT ( 'NONE',  ( 9.999999999999998224, 0.000000000000000000, -111.8750000040967763 ) ) ;
#38662 = CARTESIAN_POINT ( 'NONE',  ( -10.81189881249999729, 6.242252689847871849, -144.7187500020483810 ) ) ;
#38663 = CARTESIAN_POINT ( 'NONE',  ( 10.00000000000000000, 5.773502691896255534, -111.3749999999999858 ) ) ;
#38664 = CARTESIAN_POINT ( 'NONE',  ( 9.999999999999998224, 0.000000000000000000, -146.0000000000000000 ) ) ;
#38665 = CARTESIAN_POINT ( 'NONE',  ( -10.00000000000000000, -5.773502691896251982, -65.62499999999998579 ) ) ;
#38666 = CARTESIAN_POINT ( 'NONE',  ( 7.644554776091147741E-16, 12.48450537969573659, -139.1562500020483810 ) ) ;
#38667 = CARTESIAN_POINT ( 'NONE',  ( -10.81189881249999729, 1.324075727343319199E-15, -8.281250002048350822 ) ) ;
#38668 = EDGE_CURVE ( 'NONE', #22389, #2291, #39617, .T. ) ;
#38669 = ORIENTED_EDGE ( 'NONE', *, *, #40135, .F. ) ;
#38670 = CARTESIAN_POINT ( 'NONE',  ( 7.071067811865472841, -7.071067811865472841, -200.0000000000000000 ) ) ;
#38671 = CARTESIAN_POINT ( 'NONE',  ( -10.00000000000000000, -5.773502691896251982, -115.5000000040967905 ) ) ;
#38672 = DIRECTION ( 'NONE',  ( 0.000000000000000000, 0.000000000000000000, -1.000000000000000000 ) ) ;
#38673 = CARTESIAN_POINT ( 'NONE',  ( 10.81189881249999729, 0.000000000000000000, -73.34375000204838102 ) ) ;
#38674 = CARTESIAN_POINT ( 'NONE',  ( -9.999999999999998224, 1.224646799147353059E-15, -38.74999999999997868 ) ) ;
#38675 = LOCAL_TIME ( 11, 57, 6.000000000000000000, #36131 ) ;
#38676 = CARTESIAN_POINT ( 'NONE',  ( 10.00000000000000000, 5.773502691896255534, -24.75000000409676559 ) ) ;
#38677 = CARTESIAN_POINT ( 'NONE',  ( 10.81189881249999729, 6.242252689847867408, -55.40625000204837391 ) ) ;
#38678 = CARTESIAN_POINT ( 'NONE',  ( 4.999999999999992006, -8.660254037844389075, -131.6250000040967620 ) ) ;
#38679 = CARTESIAN_POINT ( 'NONE',  ( 10.81189881249999907, 6.242252689847868297, -38.90625000204836681 ) ) ;
#38680 = CARTESIAN_POINT ( 'NONE',  ( 10.00000000000051159, -5.773502691895965988, -105.6249999999999858 ) ) ;
#38681 = CARTESIAN_POINT ( 'NONE',  ( 5.405949406249999534, 9.363379034771803333, -146.7812500020483810 ) ) ;
#38682 = CARTESIAN_POINT ( 'NONE',  ( 10.81189881249999551, -6.242252689847874514, -150.1562500020484094 ) ) ;
#38683 = CARTESIAN_POINT ( 'NONE',  ( -9.999999999999998224, 1.224646799147353059E-15, -78.12500000409677625 ) ) ;
#38684 = CARTESIAN_POINT ( 'NONE',  ( -9.999999999999998224, 1.224646799147353059E-15, -58.24999999999997158 ) ) ;
#38685 = ORIENTED_EDGE ( 'NONE', *, *, #19874, .T. ) ;
#38686 = ORIENTED_EDGE ( 'NONE', *, *, #18971, .F. ) ;
#38687 = VERTEX_POINT ( 'NONE', #3325 ) ;
#38688 = VECTOR ( 'NONE', #6979, 1000.000000000000000 ) ;
#38689 = DIRECTION ( 'NONE',  ( -0.000000000000000000, -0.000000000000000000, 1.000000000000000000 ) ) ;
#38690 = CARTESIAN_POINT ( 'NONE',  ( -5.405949406250003975, -9.363379034771801557, -184.8437500020483810 ) ) ;
#38691 = LOCAL_TIME ( 11, 57, 6.000000000000000000, #35619 ) ;
#38692 = CARTESIAN_POINT ( 'NONE',  ( -10.81189881249999729, 6.242252689847871849, -29.21875000204835615 ) ) ;
#38693 = CARTESIAN_POINT ( 'NONE',  ( 0.000000000000000000, 0.000000000000000000, -200.0000000000000000 ) ) ;
#38694 = CARTESIAN_POINT ( 'NONE',  ( 10.81189881249999551, -6.242252689847874514, -161.9687500020484094 ) ) ;
#38695 = CARTESIAN_POINT ( 'NONE',  ( -10.81189881249999729, 1.324075727343319199E-15, -152.0937500020483810 ) ) ;
#38696 = CARTESIAN_POINT ( 'NONE',  ( 10.82102786788851212, -1.350150063679357304, 1.152242674263551442E-14 ) ) ;
#38697 = CARTESIAN_POINT ( 'NONE',  ( 7.644554776091147741E-16, 12.48450537969573659, -132.9687500020483810 ) ) ;
#38698 = CARTESIAN_POINT ( 'NONE',  ( 10.81189881249999551, -6.242252689847874514, -139.6562500020484094 ) ) ;
#38699 = CARTESIAN_POINT ( 'NONE',  ( -10.81189881249999907, -6.242252689847864744, -16.96875000204836681 ) ) ;
#38700 = CARTESIAN_POINT ( 'NONE',  ( -10.81189881249999729, 1.324075727343319199E-15, -146.0937500020483810 ) ) ;
#38701 = FACE_OUTER_BOUND ( 'NONE', #33861, .T. ) ;
#38702 = CARTESIAN_POINT ( 'NONE',  ( -9.999999999999998224, 1.224646799147353059E-15, -10.62500000409674605 ) ) ;
#38703 = CARTESIAN_POINT ( 'NONE',  ( 10.00000000000000000, 5.773502691896255534, -165.3749999999999716 ) ) ;
#38704 = EDGE_CURVE ( 'NONE', #17267, #5246, #16458, .T. ) ;
#38705 = CARTESIAN_POINT ( 'NONE',  ( 7.644554776091147741E-16, 12.48450537969573659, -83.46875000204838102 ) ) ;
#38706 = CARTESIAN_POINT ( 'NONE',  ( -9.999999999999998224, 1.224646799147353059E-15, -114.1250000040967763 ) ) ;
#38707 = CARTESIAN_POINT ( 'NONE',  ( 10.81189881249999907, 6.242252689847868297, -52.40625000204838813 ) ) ;
#38708 = CARTESIAN_POINT ( 'NONE',  ( -5.405949406249996869, 9.363379034771805109, -65.34375000204836681 ) ) ;
#38709 = CARTESIAN_POINT ( 'NONE',  ( -9.999999999999998224, 1.224646799147353059E-15, -16.62500000409675138 ) ) ;
#38710 = CARTESIAN_POINT ( 'NONE',  ( 10.81189881249999907, 6.242252689847868297, -172.2187500020483810 ) ) ;
#38711 = CARTESIAN_POINT ( 'NONE',  ( 7.070501591499377789E-16, 11.54700538379251284, -139.6250000000000000 ) ) ;
#38712 = CARTESIAN_POINT ( 'NONE',  ( -5.405949406249996869, 9.363379034771805109, -146.5312500020483810 ) ) ;
#38713 =( BOUNDED_CURVE ( )  B_SPLINE_CURVE ( 2, ( #36062, #35856, #16605, #42308, #32831, #2838, #12730 ),
 .UNSPECIFIED., .F., .F. ) 
 B_SPLINE_CURVE_WITH_KNOTS ( ( 3, 2, 2, 3 ),
 ( 0.1791044776119403437, 0.1803482587064677289, 0.1815920398009950587, 0.1828358208955224162 ),
 .UNSPECIFIED. ) 
 CURVE ( )  GEOMETRIC_REPRESENTATION_ITEM ( )  RATIONAL_B_SPLINE_CURVE ( ( 0.9999999999999940048, 0.8660254037844447028, 1.000000000000000000, 0.8660254037844387076, 1.000000000000000000, 0.8660254037844357100, 1.000000000000003109 ) ) 
 REPRESENTATION_ITEM ( '' )  );
#38714 = CYLINDRICAL_SURFACE ( 'NONE', #10995, 9.999999999999998224 ) ;
#38715 = CARTESIAN_POINT ( 'NONE',  ( 5.405949406249992428, -9.363379034771808662, -39.28125000204838102 ) ) ;
#38716 = CARTESIAN_POINT ( 'NONE',  ( -9.999999999999998224, 5.773502691896259087, -121.7500000040967905 ) ) ;
#38717 = CARTESIAN_POINT ( 'NONE',  ( 5.000000000000000000, 8.660254037844385522, -99.24999999999998579 ) ) ;
#38718 = ORIENTED_EDGE ( 'NONE', *, *, #42040, .T. ) ;
#38719 = CARTESIAN_POINT ( 'NONE',  ( 10.81189881249999551, -6.242252689847874514, -118.6562500020483952 ) ) ;
#38720 = CARTESIAN_POINT ( 'NONE',  ( -2.121150477449813534E-15, -11.54700538379251284, -139.2500000040967905 ) ) ;
#38721 = CYLINDRICAL_SURFACE ( 'NONE', #27743, 9.999999999999998224 ) ;
#38722 = CARTESIAN_POINT ( 'NONE',  ( 10.81189881249999729, 0.000000000000000000, -169.5312500020484094 ) ) ;
#38723 = CARTESIAN_POINT ( 'NONE',  ( -4.999999999999996447, 8.660254037844387298, -48.37500000409677625 ) ) ;
#38724 = CARTESIAN_POINT ( 'NONE',  ( -9.999999999999742428, -5.773502691896402084, -160.1250000000000284 ) ) ;
#38725 = CARTESIAN_POINT ( 'NONE',  ( 10.81189881249999729, 0.000000000000000000, -60.03125000204836681 ) ) ;
#38726 = EDGE_CURVE ( 'NONE', #12739, #41070, #7365, .T. ) ;
#38727 = VECTOR ( 'NONE', #39202, 1000.000000000000000 ) ;
#38728 = FACE_OUTER_BOUND ( 'NONE', #15831, .T. ) ;
#38729 = CARTESIAN_POINT ( 'NONE',  ( -10.81189881249999729, 6.242252689847871849, -171.9062500020484094 ) ) ;
#38730 = CARTESIAN_POINT ( 'NONE',  ( -9.999999999999998224, 1.224646799147353059E-15, -7.249999999999978684 ) ) ;
#38731 = DIRECTION ( 'NONE',  ( -0.000000000000000000, -0.000000000000000000, 1.000000000000000000 ) ) ;
#38732 = ORIENTED_EDGE ( 'NONE', *, *, #8828, .F. ) ;
#38733 = CYLINDRICAL_SURFACE ( 'NONE', #5914, 9.999999999999998224 ) ;
#38734 = CARTESIAN_POINT ( 'NONE',  ( -4.999999999999996447, 8.660254037844387298, -26.99999999999996803 ) ) ;
#38736 = VERTEX_POINT ( 'NONE', #17099 ) ;
#38735 = CARTESIAN_POINT ( 'NONE',  ( 7.644554776091147741E-16, 12.48450537969573659, -80.65625000204839523 ) ) ;
#38737 =( NAMED_UNIT ( * ) PLANE_ANGLE_UNIT ( ) SI_UNIT ( $, .RADIAN. ) );
#38739 = ORIENTED_EDGE ( 'NONE', *, *, #25430, .T. ) ;
#38738 = CARTESIAN_POINT ( 'NONE',  ( -2.121150477449813534E-15, -11.54700538379251284, -100.2500000040967905 ) ) ;
#38740 = VERTEX_POINT ( 'NONE', #26626 ) ;
#38741 = CARTESIAN_POINT ( 'NONE',  ( -2.293366432827344421E-15, -12.48450537969573659, -28.71875000204835615 ) ) ;
#38742 = LINE ( 'NONE', #11976, #14836 ) ;
#38743 = CARTESIAN_POINT ( 'NONE',  ( -5.405949406250003975, -9.363379034771801557, -8.031250002048350822 ) ) ;
#38745 = ORIENTED_EDGE ( 'NONE', *, *, #18147, .T. ) ;
#38744 = CARTESIAN_POINT ( 'NONE',  ( -10.81189881249999907, -6.242252689847864744, -54.46875000204838102 ) ) ;
#38746 = FACE_OUTER_BOUND ( 'NONE', #6128, .T. ) ;
#38747 = CARTESIAN_POINT ( 'NONE',  ( -5.000000000000003553, -8.660254037844383745, -30.99999999999997158 ) ) ;
#38748 = CARTESIAN_POINT ( 'NONE',  ( 10.81189881249999551, -6.242252689847874514, -188.9687500020484094 ) ) ;
#38749 = CARTESIAN_POINT ( 'NONE',  ( 10.81189881249999551, -6.242252689847874514, -173.9687500020484094 ) ) ;
#38750 = CARTESIAN_POINT ( 'NONE',  ( 10.81189881249999551, -6.242252689847874514, -155.9687500020484094 ) ) ;
#38751 = AXIS2_PLACEMENT_3D ( 'NONE', #30790, #4661, #4024 ) ;
#38752 =( BOUNDED_CURVE ( )  B_SPLINE_CURVE ( 2, ( #18804, #21183, #31781, #25302, #38446, #31992, #34373 ),
 .UNSPECIFIED., .F., .F. ) 
 B_SPLINE_CURVE_WITH_KNOTS ( ( 3, 2, 2, 3 ),
 ( 0.8283582089552240513, 0.8296019900497514366, 0.8308457711442787108, 0.8320895522388060961 ),
 .UNSPECIFIED. ) 
 CURVE ( )  GEOMETRIC_REPRESENTATION_ITEM ( )  RATIONAL_B_SPLINE_CURVE ( ( 0.9999999999999761302, 0.8660254037844625774, 1.000000000000000000, 0.8660254037844387076, 1.000000000000000000, 0.8660254037844267172, 1.000000000000011990 ) ) 
 REPRESENTATION_ITEM ( '' )  );
#38754 = ADVANCED_FACE ( 'NONE', ( #22753 ), #13009, .T. ) ;
#38753 = CARTESIAN_POINT ( 'NONE',  ( 10.81189881249999729, 0.000000000000000000, -170.8437500020484094 ) ) ;
#38755 = CARTESIAN_POINT ( 'NONE',  ( 5.000000000000000000, 8.660254037844385522, -41.12500000409677625 ) ) ;
#38756 = CARTESIAN_POINT ( 'NONE',  ( 9.999999999999998224, 0.000000000000000000, -126.5000000000000000 ) ) ;
#38757 = CARTESIAN_POINT ( 'NONE',  ( -5.000000000000003553, -8.660254037844383745, -199.0000000000000000 ) ) ;
#38758 = CARTESIAN_POINT ( 'NONE',  ( -10.81189881249999907, -6.242252689847864744, -103.9687500020483668 ) ) ;
#38759 = CARTESIAN_POINT ( 'NONE',  ( -9.999999999999998224, 1.224646799147353059E-15, -200.0000000000000000 ) ) ;
#38760 = CARTESIAN_POINT ( 'NONE',  ( -10.81189881249999729, 1.324075727343319199E-15, -72.78125000204838102 ) ) ;
#38761 = CARTESIAN_POINT ( 'NONE',  ( 5.405949406249999534, 9.363379034771803333, -95.59375000204838102 ) ) ;
#38762 = CARTESIAN_POINT ( 'NONE',  ( -2.293366432827344421E-15, -12.48450537969573659, -63.40625000204838813 ) ) ;
#38763 = CARTESIAN_POINT ( 'NONE',  ( 9.999999999999996447, -5.773502691896262640, -148.0000000040968189 ) ) ;
#38764 = CARTESIAN_POINT ( 'NONE',  ( 9.999999999999996447, -5.773502691896262640, -125.1249999999999858 ) ) ;
#38765 = ORIENTED_EDGE ( 'NONE', *, *, #34438, .T. ) ;
#38766 = CARTESIAN_POINT ( 'NONE',  ( -5.405949406250003975, -9.363379034771801557, -144.5312500020483810 ) ) ;
#38767 = CARTESIAN_POINT ( 'NONE',  ( 5.405949406249992428, -9.363379034771808662, -156.2812500020484094 ) ) ;
#38768 = VECTOR ( 'NONE', #14708, 1000.000000000000000 ) ;
#38769 = DIRECTION ( 'NONE',  ( 1.000000000000000000, 0.000000000000000000, 0.000000000000000000 ) ) ;
#38770 = CARTESIAN_POINT ( 'NONE',  ( 8.660254119780192994, -4.999999858083012505, -99.99999999999998579 ) ) ;
#38771 = CARTESIAN_POINT ( 'NONE',  ( 10.81189881249999551, -6.242252689847874514, -89.96875000204838102 ) ) ;
#38772 = VERTEX_POINT ( 'NONE', #26413 ) ;
#38773 = CARTESIAN_POINT ( 'NONE',  ( 10.00000000000000000, 5.773502691896255534, -69.37499999999998579 ) ) ;
#38774 = CARTESIAN_POINT ( 'NONE',  ( 7.644554776091147741E-16, 12.48450537969573659, -186.9687500020483810 ) ) ;
#38775 = CARTESIAN_POINT ( 'NONE',  ( 5.000000000000000000, 8.660254037844385522, -74.12500000409677625 ) ) ;
#38776 = CARTESIAN_POINT ( 'NONE',  ( -9.999999999999998224, 1.224646799147353059E-15, -122.7500000000000000 ) ) ;
#38777 = CARTESIAN_POINT ( 'NONE',  ( -4.999999999999996447, 8.660254037844387298, -12.37500000409674783 ) ) ;
#38778 = CARTESIAN_POINT ( 'NONE',  ( -5.405949406249996869, 9.363379034771805109, -85.03125000204838102 ) ) ;
#38779 = CARTESIAN_POINT ( 'NONE',  ( -5.405949406250003975, -9.363379034771801557, -69.53125000204838102 ) ) ;
#38780 = CARTESIAN_POINT ( 'NONE',  ( 9.999999999999996447, -5.773502691896262640, -56.50000000409677625 ) ) ;
#38781 = CARTESIAN_POINT ( 'NONE',  ( -4.999999999999996447, 8.660254037844387298, -93.37500000409677625 ) ) ;
#38782 = CARTESIAN_POINT ( 'NONE',  ( -2.293366432827344421E-15, -12.48450537969573659, -16.71875000204836681 ) ) ;
#38783 = CARTESIAN_POINT ( 'NONE',  ( -9.999999999999998224, 1.224646799147353059E-15, -46.62500000409677625 ) ) ;
#38784 = CARTESIAN_POINT ( 'NONE',  ( -5.405949406249996869, 9.363379034771805109, -190.0312500020484094 ) ) ;
#38785 = CARTESIAN_POINT ( 'NONE',  ( 5.405949406249992428, -9.363379034771808662, -18.28125000204835970 ) ) ;
#38786 = EDGE_CURVE ( 'NONE', #2188, #35877, #24783, .T. ) ;
#38787 = CARTESIAN_POINT ( 'NONE',  ( 5.405949406249992428, -9.363379034771808662, -4.593750002048368586 ) ) ;
#38788 = CYLINDRICAL_SURFACE ( 'NONE', #14490, 9.999999999999998224 ) ;
#38789 = FACE_OUTER_BOUND ( 'NONE', #21688, .T. ) ;
#38790 = CARTESIAN_POINT ( 'NONE',  ( -9.999999999999998224, 1.224646799147353059E-15, -200.0000000000000000 ) ) ;
#38791 = CARTESIAN_POINT ( 'NONE',  ( 5.000000000000000000, 8.660254037844385522, -171.2500000000000000 ) ) ;
#38792 = DIRECTION ( 'NONE',  ( -0.000000000000000000, -0.000000000000000000, 1.000000000000000000 ) ) ;
#38794 = ORIENTED_EDGE ( 'NONE', *, *, #22573, .T. ) ;
#38793 = CARTESIAN_POINT ( 'NONE',  ( 5.405949406249999534, 9.363379034771803333, -98.78125000204839523 ) ) ;
#38795 = CARTESIAN_POINT ( 'NONE',  ( 9.999999999998969713, 5.773502691896851502, -37.87499999999992895 ) ) ;
#38796 = ORIENTED_EDGE ( 'NONE', *, *, #33231, .F. ) ;
#38797 = EDGE_LOOP ( 'NONE', ( #28778, #27196, #23668, #20091 ) ) ;
#38798 = CARTESIAN_POINT ( 'NONE',  ( -2.293366432827344421E-15, -12.48450537969573659, -30.40625000204834905 ) ) ;
#38799 = COORDINATED_UNIVERSAL_TIME_OFFSET ( 6, 0, .AHEAD. ) ;
#38800 = CARTESIAN_POINT ( 'NONE',  ( -5.405949406250003975, -9.363379034771801557, -78.34375000204838102 ) ) ;
#38801 = DIRECTION ( 'NONE',  ( -0.000000000000000000, -0.000000000000000000, -1.000000000000000000 ) ) ;
#38802 = CARTESIAN_POINT ( 'NONE',  ( 9.865189697491926424, 3.226167097173905152, -100.0000000000000000 ) ) ;
#38803 = CARTESIAN_POINT ( 'NONE',  ( -9.999999999999998224, 1.224646799147353059E-15, -127.6250000040967620 ) ) ;
#38804 = LINE ( 'NONE', #19365, #39106 ) ;
#38805 = CARTESIAN_POINT ( 'NONE',  ( 10.81189881249999729, 0.000000000000000000, -159.0312500020484094 ) ) ;
#38806 = CARTESIAN_POINT ( 'NONE',  ( -5.000000000000003553, -8.660254037844383745, -7.375000004096743389 ) ) ;
#38807 = CARTESIAN_POINT ( 'NONE',  ( -9.999999999999998224, 1.224646799147353059E-15, -150.1250000040967905 ) ) ;
#38808 = CARTESIAN_POINT ( 'NONE',  ( 5.405949406249999534, 9.363379034771803333, -133.0937500020483810 ) ) ;
#38809 = CARTESIAN_POINT ( 'NONE',  ( 10.81189881249999729, 6.242252689847867408, -113.7187500020483952 ) ) ;
#38810 = CARTESIAN_POINT ( 'NONE',  ( 5.405949406249999534, 9.363379034771803333, -76.09375000204838102 ) ) ;
#38811 = CARTESIAN_POINT ( 'NONE',  ( -10.81189881249999907, -6.242252689847864744, -83.15625000204836681 ) ) ;
#38812 = CARTESIAN_POINT ( 'NONE',  ( -9.999999999999998224, 1.224646799147353059E-15, -166.6250000040967905 ) ) ;
#38813 = CARTESIAN_POINT ( 'NONE',  ( -9.999999999999998224, 1.224646799147353059E-15, -133.6250000040967620 ) ) ;
#38814 = CARTESIAN_POINT ( 'NONE',  ( 10.81189881249999729, 6.242252689847867408, -164.9062500020484094 ) ) ;
#38815 = CARTESIAN_POINT ( 'NONE',  ( -10.81189881249999729, 1.324075727343319199E-15, -179.2812500020484094 ) ) ;
#38816 = CARTESIAN_POINT ( 'NONE',  ( 5.405949406249999534, 9.363379034771803333, -47.59375000204838102 ) ) ;
#38817 = CARTESIAN_POINT ( 'NONE',  ( -5.000000000000003553, -8.660254037844383745, -155.8750000040967905 ) ) ;
#38818 = CARTESIAN_POINT ( 'NONE',  ( -10.81189881249999907, -6.242252689847864744, -0.6562500020483670315 ) ) ;
#38819 = CARTESIAN_POINT ( 'NONE',  ( 10.81189881249999907, 6.242252689847868297, -4.218750002048355263 ) ) ;
#38820 = CARTESIAN_POINT ( 'NONE',  ( -5.405949406250003975, -9.363379034771801557, -111.3437500020483810 ) ) ;
#38821 = CARTESIAN_POINT ( 'NONE',  ( 5.000000000000000000, 8.660254037844385522, -91.74999999999998579 ) ) ;
#38822 = CARTESIAN_POINT ( 'NONE',  ( 10.81189881249999907, 6.242252689847868297, -8.906250002048366810 ) ) ;
#38823 = CARTESIAN_POINT ( 'NONE',  ( -10.00000000000000000, -5.773502691896251982, -94.50000000409677625 ) ) ;
#38824 = CARTESIAN_POINT ( 'NONE',  ( -9.999999999999998224, 1.224646799147353059E-15, -94.24999999999998579 ) ) ;
#38825 = CARTESIAN_POINT ( 'NONE',  ( 5.405949406249992428, -9.363379034771808662, -112.7812500020483952 ) ) ;
#38826 = CARTESIAN_POINT ( 'NONE',  ( -10.81189881249999729, -6.242252689847864744, -90.65625000204836681 ) ) ;
#38827 = ORIENTED_EDGE ( 'NONE', *, *, #37201, .T. ) ;
#38828 = CARTESIAN_POINT ( 'NONE',  ( -2.121150477449813534E-15, -11.54700538379251284, -89.75000000409677625 ) ) ;
#38829 = CARTESIAN_POINT ( 'NONE',  ( 10.00000000000051159, -5.773502691895965988, -101.1249999999999858 ) ) ;
#38830 = CARTESIAN_POINT ( 'NONE',  ( -5.405949406249996869, 9.363379034771805109, -47.34375000204838102 ) ) ;
#38831 = ORIENTED_EDGE ( 'NONE', *, *, #31492, .T. ) ;
#38832 = CARTESIAN_POINT ( 'NONE',  ( 4.999999999999992006, -8.660254037844389075, -15.74999999999995914 ) ) ;
#38833 = EDGE_CURVE ( 'NONE', #3790, #34380, #11499, .T. ) ;
#38834 = CARTESIAN_POINT ( 'NONE',  ( -5.405949406250003975, -9.363379034771801557, -23.03125000204836326 ) ) ;
#38835 = CARTESIAN_POINT ( 'NONE',  ( -10.00000000000000000, -5.773502691896251982, -149.6250000000000284 ) ) ;
#38836 = CARTESIAN_POINT ( 'NONE',  ( 9.999999999999998224, 0.000000000000000000, -17.37500000409675138 ) ) ;
#38837 = EDGE_CURVE ( 'NONE', #7311, #10904, #20334, .T. ) ;
#38838 = CARTESIAN_POINT ( 'NONE',  ( 10.00000000000000000, 5.773502691896255534, -195.3750000000000284 ) ) ;
#38840 = ORIENTED_EDGE ( 'NONE', *, *, #34933, .T. ) ;
#38839 = CARTESIAN_POINT ( 'NONE',  ( -5.405949406250003975, -9.363379034771801557, -123.5312500020483952 ) ) ;
#38841 = CARTESIAN_POINT ( 'NONE',  ( -9.999999999999998224, 1.224646799147353059E-15, -89.74999999999998579 ) ) ;
#38842 =( BOUNDED_CURVE ( )  B_SPLINE_CURVE ( 2, ( #4867, #31419, #14117, #1857, #14983, #10684, #23878 ),
 .UNSPECIFIED., .F., .F. ) 
 B_SPLINE_CURVE_WITH_KNOTS ( ( 3, 2, 2, 3 ),
 ( 0.2276119402985075368, 0.2288557213930349221, 0.2300995024875622796, 0.2313432835820896372 ),
 .UNSPECIFIED. ) 
 CURVE ( )  GEOMETRIC_REPRESENTATION_ITEM ( )  RATIONAL_B_SPLINE_CURVE ( ( 0.9999999999999910072, 0.8660254037844477004, 1.000000000000000000, 0.8660254037844387076, 1.000000000000000000, 0.8660254037844297148, 1.000000000000008882 ) ) 
 REPRESENTATION_ITEM ( '' )  );
#38843 = VERTEX_POINT ( 'NONE', #39774 ) ;
#38844 = CARTESIAN_POINT ( 'NONE',  ( -10.81189881249999729, 1.324075727343319199E-15, -53.28125000204836681 ) ) ;
#38845 = APPROVAL_STATUS ( 'not_yet_approved' ) ;
#38846 = CARTESIAN_POINT ( 'NONE',  ( -5.405949406250003975, -9.363379034771801557, -102.3437500020483810 ) ) ;
#38848 = ORIENTED_EDGE ( 'NONE', *, *, #23044, .F. ) ;
#38847 = ORIENTED_EDGE ( 'NONE', *, *, #25204, .F. ) ;
#38849 = DIRECTION ( 'NONE',  ( -1.000000000000000000, -0.000000000000000000, -0.000000000000000000 ) ) ;
#38850 = CYLINDRICAL_SURFACE ( 'NONE', #3551, 9.999999999999998224 ) ;
#38851 = CARTESIAN_POINT ( 'NONE',  ( 10.81189881249999907, 6.242252689847868297, -148.2187500020484094 ) ) ;
#38852 = CARTESIAN_POINT ( 'NONE',  ( 10.81189881249999729, 0.000000000000000000, -180.0312500020483810 ) ) ;
#38853 = CARTESIAN_POINT ( 'NONE',  ( -5.405949406249996869, 9.363379034771805109, -9.843750002048345493 ) ) ;
#38854 = CARTESIAN_POINT ( 'NONE',  ( 9.999999999999742428, 5.773502691896404748, -139.8749999999999716 ) ) ;
#38855 = EDGE_CURVE ( 'NONE', #27592, #12865, #42380, .T. ) ;
#38856 = CARTESIAN_POINT ( 'NONE',  ( 10.81189881249999729, 0.000000000000000000, -139.3437500020484094 ) ) ;
#38857 = CARTESIAN_POINT ( 'NONE',  ( -5.405949406250003975, -9.363379034771801557, -105.3437500020483810 ) ) ;
#38858 = CARTESIAN_POINT ( 'NONE',  ( -5.405949406250003975, -9.363379034771801557, -111.5312500020483810 ) ) ;
#38859 = CARTESIAN_POINT ( 'NONE',  ( -9.999999999999998224, 5.773502691896259087, -195.2500000040967905 ) ) ;
#38860 = CARTESIAN_POINT ( 'NONE',  ( 5.405949406249999534, 9.363379034771803333, -122.5937500020483952 ) ) ;
#38861 = CARTESIAN_POINT ( 'NONE',  ( -10.81189881249999729, -6.242252689847864744, -183.6562500020484094 ) ) ;
#38862 = CARTESIAN_POINT ( 'NONE',  ( -9.999999999999998224, 1.224646799147353059E-15, -170.7500000000000000 ) ) ;
#38863 = CARTESIAN_POINT ( 'NONE',  ( 7.070501591499377789E-16, 11.54700538379251284, -142.6250000000000000 ) ) ;
#38864 = CARTESIAN_POINT ( 'NONE',  ( -9.999999999999998224, 1.224646799147353059E-15, -2.749999999999974687 ) ) ;
#38865 = CARTESIAN_POINT ( 'NONE',  ( -10.81189881249999729, 1.324075727343319199E-15, -68.09375000204836681 ) ) ;
#38866 = CARTESIAN_POINT ( 'NONE',  ( -2.293366432827344421E-15, -12.48450537969573659, -45.21875000204836681 ) ) ;
#38867 = CARTESIAN_POINT ( 'NONE',  ( 9.999999999999996447, -5.773502691896262640, -188.5000000040968189 ) ) ;
#38868 = CARTESIAN_POINT ( 'NONE',  ( -5.405949406250003975, -9.363379034771801557, -23.03125000204836326 ) ) ;
#38869 = CARTESIAN_POINT ( 'NONE',  ( -5.405949406250003975, -9.363379034771801557, -34.84375000204836681 ) ) ;
#38870 = CARTESIAN_POINT ( 'NONE',  ( 5.000000000000000000, 8.660254037844385522, -149.1250000040967905 ) ) ;
#38871 = CARTESIAN_POINT ( 'NONE',  ( -5.405949406249996869, 9.363379034771805109, -137.3437500020484094 ) ) ;
#38872 = CARTESIAN_POINT ( 'NONE',  ( 5.000000000000000000, 8.660254037844385522, -114.2499999999999858 ) ) ;
#38873 = CARTESIAN_POINT ( 'NONE',  ( -2.121150477449813534E-15, -11.54700538379251284, -147.8750000000000000 ) ) ;
#38874 = CARTESIAN_POINT ( 'NONE',  ( -5.000000000000003553, -8.660254037844383745, -65.49999999999997158 ) ) ;
#38875 = CARTESIAN_POINT ( 'NONE',  ( 5.405949406249992428, -9.363379034771808662, -136.7812500020483810 ) ) ;
#38876 = CARTESIAN_POINT ( 'NONE',  ( 10.81189881249999551, -6.242252689847874514, -114.1562500020483952 ) ) ;
#38877 =( BOUNDED_CURVE ( )  B_SPLINE_CURVE ( 2, ( #36178, #371, #999, #40044, #4014, #20198, #27106 ),
 .UNSPECIFIED., .F., .F. ) 
 B_SPLINE_CURVE_WITH_KNOTS ( ( 3, 2, 2, 3 ),
 ( 0.3843283582089552786, 0.3855721393034826638, 0.3868159203980099936, 0.3880597014925373789 ),
 .UNSPECIFIED. ) 
 CURVE ( )  GEOMETRIC_REPRESENTATION_ITEM ( )  RATIONAL_B_SPLINE_CURVE ( ( 0.9999999999999940048, 0.8660254037844447028, 1.000000000000000000, 0.8660254037844387076, 1.000000000000000000, 0.8660254037844327124, 1.000000000000005995 ) ) 
 REPRESENTATION_ITEM ( '' )  );
#38878 = ORIENTED_EDGE ( 'NONE', *, *, #5501, .T. ) ;
#38879 = CARTESIAN_POINT ( 'NONE',  ( -10.00000000000025580, 5.773502691896109873, -120.2500000040967905 ) ) ;
#38880 = CARTESIAN_POINT ( 'NONE',  ( -9.999999999999998224, 1.224646799147353059E-15, -120.1250000040967905 ) ) ;
#38881 = CARTESIAN_POINT ( 'NONE',  ( -5.000000000000003553, -8.660254037844383745, -86.87500000409677625 ) ) ;
#38882 = CARTESIAN_POINT ( 'NONE',  ( -5.405949406249996869, 9.363379034771805109, -72.84375000204838102 ) ) ;
#38883 = CARTESIAN_POINT ( 'NONE',  ( 7.070501591499377789E-16, 11.54700538379251284, -37.62499999999995737 ) ) ;
#38884 = CARTESIAN_POINT ( 'NONE',  ( -5.000000000000003553, -8.660254037844383745, -29.87500000409676204 ) ) ;
#38885 = EDGE_CURVE ( 'NONE', #5998, #17896, #1588, .T. ) ;
#38886 = CARTESIAN_POINT ( 'NONE',  ( 10.81189881249999551, -6.242252689847874514, -42.15625000204838102 ) ) ;
#38887 = CARTESIAN_POINT ( 'NONE',  ( -22.00000000000000711, 0.000000000000000000, -99.99999999999998579 ) ) ;
#38888 = CARTESIAN_POINT ( 'NONE',  ( -10.81189881249999907, -6.242252689847864744, -38.15625000204835970 ) ) ;
#38889 = EDGE_CURVE ( 'NONE', #16629, #38687, #10840, .T. ) ;
#38890 =( BOUNDED_CURVE ( )  B_SPLINE_CURVE ( 2, ( #27521, #33790, #987, #13686, #16930, #14105, #20185 ),
 .UNSPECIFIED., .F., .F. ) 
 B_SPLINE_CURVE_WITH_KNOTS ( ( 3, 2, 2, 3 ),
 ( 0.2052238805970149627, 0.2064676616915423202, 0.2077114427860697055, 0.2089552238805970630 ),
 .UNSPECIFIED. ) 
 CURVE ( )  GEOMETRIC_REPRESENTATION_ITEM ( )  RATIONAL_B_SPLINE_CURVE ( ( 0.9999999999999970024, 0.8660254037844417052, 1.000000000000000000, 0.8660254037844387076, 1.000000000000000000, 0.8660254037844327124, 1.000000000000005995 ) ) 
 REPRESENTATION_ITEM ( '' )  );
#38891 = CARTESIAN_POINT ( 'NONE',  ( -9.999999999999998224, 1.224646799147353059E-15, -175.6250000040968189 ) ) ;
#38892 = CARTESIAN_POINT ( 'NONE',  ( 10.81189881249999551, -6.242252689847874514, -133.6562500020483810 ) ) ;
#38893 = EDGE_CURVE ( 'NONE', #7682, #6043, #39873, .T. ) ;
#38894 = CARTESIAN_POINT ( 'NONE',  ( 10.81189881249999551, -6.242252689847874514, -151.6562500020484094 ) ) ;
#38895 = CARTESIAN_POINT ( 'NONE',  ( 9.999999999999998224, 0.000000000000000000, -60.49999999999997158 ) ) ;
#38896 = CARTESIAN_POINT ( 'NONE',  ( -9.999999999999998224, 1.224646799147353059E-15, -121.2500000000000000 ) ) ;
#38897 = ORIENTED_EDGE ( 'NONE', *, *, #3505, .F. ) ;
#38898 =( BOUNDED_CURVE ( )  B_SPLINE_CURVE ( 2, ( #1144, #11474, #5026, #37393, #4799, #27684, #14489 ),
 .UNSPECIFIED., .F., .F. ) 
 B_SPLINE_CURVE_WITH_KNOTS ( ( 3, 2, 2, 3 ),
 ( 0.2201492537313433639, 0.2213930348258707215, 0.2226368159203980790, 0.2238805970149254365 ),
 .UNSPECIFIED. ) 
 CURVE ( )  GEOMETRIC_REPRESENTATION_ITEM ( )  RATIONAL_B_SPLINE_CURVE ( ( 0.9999999999999910072, 0.8660254037844477004, 1.000000000000000000, 0.8660254037844387076, 1.000000000000000000, 0.8660254037844327124, 1.000000000000005995 ) ) 
 REPRESENTATION_ITEM ( '' )  );
#38899 = ORIENTED_EDGE ( 'NONE', *, *, #5364, .T. ) ;
#38900 = ORIENTED_EDGE ( 'NONE', *, *, #30852, .T. ) ;
#38901 = EDGE_CURVE ( 'NONE', #9326, #16734, #42689, .T. ) ;
#38902 = CARTESIAN_POINT ( 'NONE',  ( -9.999999999999998224, 1.224646799147353059E-15, -177.1250000040968189 ) ) ;
#38903 = CARTESIAN_POINT ( 'NONE',  ( 10.81189881249999907, 6.242252689847868297, -170.7187500020483810 ) ) ;
#38904 = CARTESIAN_POINT ( 'NONE',  ( 10.81189881249999729, 0.000000000000000000, -29.84375000204836326 ) ) ;
#38905 = CARTESIAN_POINT ( 'NONE',  ( 9.999999999999998224, 0.000000000000000000, -200.0000000000000000 ) ) ;
#38906 = CARTESIAN_POINT ( 'NONE',  ( -10.81189881249999729, -6.242252689847864744, -165.4687500020483526 ) ) ;
#38907 = CARTESIAN_POINT ( 'NONE',  ( 10.81189881249999729, 0.000000000000000000, -142.3437500020483810 ) ) ;
#38908 = CARTESIAN_POINT ( 'NONE',  ( 10.00000000000051159, -5.773502691895965988, -176.1250000000000000 ) ) ;
#38909 = CARTESIAN_POINT ( 'NONE',  ( 7.644554776091147741E-16, 12.48450537969573659, -129.9687500020483810 ) ) ;
#38910 = CARTESIAN_POINT ( 'NONE',  ( -10.81189881249999907, -6.242252689847864744, -141.6562500020483810 ) ) ;
#38911 = CARTESIAN_POINT ( 'NONE',  ( -5.405949406249996869, 9.363379034771805109, -17.34375000204835260 ) ) ;
#38912 = CARTESIAN_POINT ( 'NONE',  ( 10.81189881249999551, -6.242252689847874514, -148.4687500020484094 ) ) ;
#38913 = CARTESIAN_POINT ( 'NONE',  ( 9.999999999999742428, 5.773502691896404748, -129.3750000000000000 ) ) ;
#38914 = CARTESIAN_POINT ( 'NONE',  ( 9.999999999999479527, 5.773502691896553074, -120.3749999999999716 ) ) ;
#38915 = CARTESIAN_POINT ( 'NONE',  ( 4.999999999999992006, -8.660254037844389075, -167.2500000000000000 ) ) ;
#38916 = CARTESIAN_POINT ( 'NONE',  ( 5.405949406249999534, 9.363379034771803333, -82.09375000204836681 ) ) ;
#38917 = CARTESIAN_POINT ( 'NONE',  ( 10.81189881249999729, 0.000000000000000000, -49.53125000204838813 ) ) ;
#38918 = CARTESIAN_POINT ( 'NONE',  ( 5.405949406249999534, 9.363379034771803333, -58.09375000204835970 ) ) ;
#38919 = CARTESIAN_POINT ( 'NONE',  ( 9.999999999999998224, 1.224646799147353059E-15, -99.99999999999998579 ) ) ;
#38920 = CARTESIAN_POINT ( 'NONE',  ( -10.81189881249999729, 6.242252689847871849, -168.7187500020483810 ) ) ;
#38921 = CARTESIAN_POINT ( 'NONE',  ( -9.999999999999998224, 5.773502691896259087, -139.3750000000000000 ) ) ;
#38922 = CARTESIAN_POINT ( 'NONE',  ( -5.405949406250003975, -9.363379034771801557, -149.0312500020483810 ) ) ;
#38923 = CARTESIAN_POINT ( 'NONE',  ( -5.000000000000003553, -8.660254037844383745, -23.87500000409675849 ) ) ;
#38924 = CARTESIAN_POINT ( 'NONE',  ( -4.999999999999996447, 8.660254037844387298, -121.8750000040967905 ) ) ;
#38925 = CARTESIAN_POINT ( 'NONE',  ( -4.999999999999996447, 8.660254037844387298, -94.49999999999998579 ) ) ;
#38926 = EDGE_LOOP ( 'NONE', ( #40431, #9693, #24686, #949 ) ) ;
#38927 = CARTESIAN_POINT ( 'NONE',  ( -5.405949406249996869, 9.363379034771805109, -115.0312500020483952 ) ) ;
#38928 = CARTESIAN_POINT ( 'NONE',  ( -10.00000000000000000, -5.773502691896251982, -144.0000000040967905 ) ) ;
#38929 = CARTESIAN_POINT ( 'NONE',  ( -4.999999999999996447, 8.660254037844387298, -159.0000000000000000 ) ) ;
#38930 = CARTESIAN_POINT ( 'NONE',  ( -10.81189881249999729, 1.324075727343319199E-15, -174.7812500020484094 ) ) ;
#38931 = CARTESIAN_POINT ( 'NONE',  ( -5.000000000000003553, -8.660254037844383745, -50.87500000409675494 ) ) ;
#38932 = LINE ( 'NONE', #2687, #6989 ) ;
#38933 = CARTESIAN_POINT ( 'NONE',  ( -2.293366432827344421E-15, -12.48450537969573659, -58.90625000204838102 ) ) ;
#38934 = AXIS2_PLACEMENT_3D ( 'NONE', #33211, #10514, #23701 ) ;
#38935 = FACE_OUTER_BOUND ( 'NONE', #34971, .T. ) ;
#38936 = CARTESIAN_POINT ( 'NONE',  ( -5.405949406250003975, -9.363379034771801557, -171.5312500020484094 ) ) ;
#38937 = CARTESIAN_POINT ( 'NONE',  ( 10.81189881249999729, 0.000000000000000000, -142.3437500020483810 ) ) ;
#38938 = CARTESIAN_POINT ( 'NONE',  ( 9.999999999999998224, 0.000000000000000000, -20.37500000409675494 ) ) ;
#38939 = CARTESIAN_POINT ( 'NONE',  ( 9.999999999999998224, 0.000000000000000000, -80.37500000409677625 ) ) ;
#38940 = VERTEX_POINT ( 'NONE', #943 ) ;
#38941 = CARTESIAN_POINT ( 'NONE',  ( 4.999999999999992006, -8.660254037844389075, -194.2500000000000000 ) ) ;
#38942 = EDGE_CURVE ( 'NONE', #32646, #28517, #12884, .T. ) ;
#38944 = ORIENTED_EDGE ( 'NONE', *, *, #15445, .T. ) ;
#38943 = CARTESIAN_POINT ( 'NONE',  ( 5.405949406249992428, -9.363379034771808662, -66.28125000204838102 ) ) ;
#38945 =( NAMED_UNIT ( * ) PLANE_ANGLE_UNIT ( ) SI_UNIT ( $, .RADIAN. ) );
#38947 = ORIENTED_EDGE ( 'NONE', *, *, #13590, .T. ) ;
#38946 = CARTESIAN_POINT ( 'NONE',  ( 10.00000000000051159, -5.773502691895965988, -143.1250000000000000 ) ) ;
#38948 = ORIENTED_EDGE ( 'NONE', *, *, #32830, .F. ) ;
#38949 = CARTESIAN_POINT ( 'NONE',  ( -10.81189881249999729, 6.242252689847871849, -32.21875000204835970 ) ) ;
#38950 = CYLINDRICAL_SURFACE ( 'NONE', #3162, 9.999999999999998224 ) ;
#38951 = CARTESIAN_POINT ( 'NONE',  ( 5.405949406249992428, -9.363379034771808662, -4.781250002048375691 ) ) ;
#38953 = EDGE_LOOP ( 'NONE', ( #14311, #20814, #20619, #13857 ) ) ;
#38952 = CARTESIAN_POINT ( 'NONE',  ( -10.81189881249999729, 1.324075727343319199E-15, -51.59375000204835260 ) ) ;
#38954 = CARTESIAN_POINT ( 'NONE',  ( -5.000000000000003553, -8.660254037844383745, -3.999999999999976019 ) ) ;
#38955 = CARTESIAN_POINT ( 'NONE',  ( -10.00000000000000000, -5.773502691896251982, -26.62499999999998224 ) ) ;
#38956 = CARTESIAN_POINT ( 'NONE',  ( 7.644554776091147741E-16, 12.48450537969573659, -185.4687500020484094 ) ) ;
#38957 = CARTESIAN_POINT ( 'NONE',  ( 7.644554776091147741E-16, 12.48450537969573659, -171.9687500020483810 ) ) ;
#38958 =( BOUNDED_CURVE ( )  B_SPLINE_CURVE ( 2, ( #34466, #33822, #30586, #8350, #20633, #40471, #30375 ),
 .UNSPECIFIED., .F., .F. ) 
 B_SPLINE_CURVE_WITH_KNOTS ( ( 3, 2, 2, 3 ),
 ( 0.6343283582089553896, 0.6355721393034826638, 0.6368159203980100491, 0.6380597014925374344 ),
 .UNSPECIFIED. ) 
 CURVE ( )  GEOMETRIC_REPRESENTATION_ITEM ( )  RATIONAL_B_SPLINE_CURVE ( ( 0.9999999999999880096, 0.8660254037844506980, 1.000000000000000000, 0.8660254037844387076, 1.000000000000000000, 0.8660254037844267172, 1.000000000000011990 ) ) 
 REPRESENTATION_ITEM ( '' )  );
#38959 = CARTESIAN_POINT ( 'NONE',  ( 7.644554776091147741E-16, 12.48450537969573659, -155.4687500020484094 ) ) ;
#38960 = CARTESIAN_POINT ( 'NONE',  ( -10.81189881249999729, 6.242252689847871849, -168.7187500020483810 ) ) ;
#38961 = CARTESIAN_POINT ( 'NONE',  ( -10.00000000000154188, 5.773502691895366468, -18.25000000409673007 ) ) ;
#38962 = CARTESIAN_POINT ( 'NONE',  ( -9.999999999999834799, -5.773502691896343464, -192.0000000040968189 ) ) ;
#38963 = CARTESIAN_POINT ( 'NONE',  ( 9.999999999999998224, 0.000000000000000000, -183.5000000000000000 ) ) ;
#38964 = CARTESIAN_POINT ( 'NONE',  ( -2.293366432827344421E-15, -12.48450537969573659, -105.2187500020483952 ) ) ;
#38965 = CARTESIAN_POINT ( 'NONE',  ( 5.405949406249999534, 9.363379034771803333, -74.78125000204838102 ) ) ;
#38966 = CARTESIAN_POINT ( 'NONE',  ( 4.999999999999992006, -8.660254037844389075, -5.249999999999976907 ) ) ;
#38967 = CARTESIAN_POINT ( 'NONE',  ( -10.81189881249999729, 6.242252689847871849, -87.71875000204836681 ) ) ;
#38968 = CARTESIAN_POINT ( 'NONE',  ( -5.405949406249996869, 9.363379034771805109, -58.03125000204836681 ) ) ;
#38969 = CARTESIAN_POINT ( 'NONE',  ( -5.000000000000003553, -8.660254037844383745, -143.8750000040967905 ) ) ;
#38970 = CARTESIAN_POINT ( 'NONE',  ( -4.999999999999996447, 8.660254037844387298, -112.4999999999999858 ) ) ;
#38971 = VERTEX_POINT ( 'NONE', #14498 ) ;
#38972 = CARTESIAN_POINT ( 'NONE',  ( 5.405949406249999534, 9.363379034771803333, -143.7812500020483810 ) ) ;
#38973 = CARTESIAN_POINT ( 'NONE',  ( -5.405949406249996869, 9.363379034771805109, -154.0312500020484094 ) ) ;
#38974 = CARTESIAN_POINT ( 'NONE',  ( -10.81189881249999729, 6.242252689847871849, -194.4062500020484094 ) ) ;
#38975 = CARTESIAN_POINT ( 'NONE',  ( 9.999999999999998224, 0.000000000000000000, -112.9999999999999858 ) ) ;
#38976 = CARTESIAN_POINT ( 'NONE',  ( -10.81189881249999729, 6.242252689847871849, -90.71875000204838102 ) ) ;
#38977 = ORIENTED_EDGE ( 'NONE', *, *, #23293, .F. ) ;
#38978 = CARTESIAN_POINT ( 'NONE',  ( 7.070501591499377789E-16, 11.54700538379251284, -64.62499999999998579 ) ) ;
#38979 = CARTESIAN_POINT ( 'NONE',  ( -10.81189881249999907, -6.242252689847864744, -189.4687500020484094 ) ) ;
#38980 = CARTESIAN_POINT ( 'NONE',  ( -2.121150477449813534E-15, -11.54700538379251284, -77.75000000409677625 ) ) ;
#38981 = CARTESIAN_POINT ( 'NONE',  ( 9.999999999999479527, 5.773502691896553074, -102.3749999999999858 ) ) ;
#38982 = CARTESIAN_POINT ( 'NONE',  ( 10.81189881249999907, 6.242252689847868297, -85.40625000204839523 ) ) ;
#38983 = CIRCLE ( 'NONE', #37620, 20.00000000000000355 ) ;
#38984 = CARTESIAN_POINT ( 'NONE',  ( -10.81189881249999729, 1.324075727343319199E-15, -66.78125000204838102 ) ) ;
#38985 = CARTESIAN_POINT ( 'NONE',  ( -10.00000000000000000, -5.773502691896251982, -63.00000000409677625 ) ) ;
#38986 = CARTESIAN_POINT ( 'NONE',  ( 7.644554776091147741E-16, 12.48450537969573659, -14.46875000204836503 ) ) ;
#38987 = ORIENTED_EDGE ( 'NONE', *, *, #23902, .F. ) ;
#38988 = CARTESIAN_POINT ( 'NONE',  ( -10.81189881249999729, 1.324075727343319199E-15, -195.7812500020484094 ) ) ;
#38989 = CARTESIAN_POINT ( 'NONE',  ( -10.81189881249999729, 1.324075727343319199E-15, -12.78125000204835615 ) ) ;
#38990 = CARTESIAN_POINT ( 'NONE',  ( 10.81189881249999729, 0.000000000000000000, -4.343750002048368586 ) ) ;
#38991 = DIRECTION ( 'NONE',  ( 0.000000000000000000, 0.000000000000000000, 1.000000000000000000 ) ) ;
#38992 = VECTOR ( 'NONE', #99, 1000.000000000000000 ) ;
#38993 = DIRECTION ( 'NONE',  ( -0.000000000000000000, 1.000000000000000000, -0.000000000000000000 ) ) ;
#38994 = CARTESIAN_POINT ( 'NONE',  ( 9.999999999999998224, 0.000000000000000000, -114.8750000040967905 ) ) ;
#38995 = CARTESIAN_POINT ( 'NONE',  ( 7.070501591499377789E-16, 11.54700538379251284, -178.6250000000000000 ) ) ;
#38996 = CARTESIAN_POINT ( 'NONE',  ( 5.000000000000002665, 20.00000000000000000, -235.0000000000000000 ) ) ;
#38998 = EDGE_LOOP ( 'NONE', ( #5997, #11426, #27378, #42595 ) ) ;
#38997 = CARTESIAN_POINT ( 'NONE',  ( -5.405949406249996869, 9.363379034771805109, -104.5312500020483810 ) ) ;
#38999 = CARTESIAN_POINT ( 'NONE',  ( -9.999999999999998224, 1.224646799147353059E-15, -37.24999999999997868 ) ) ;
#39000 = ORIENTED_EDGE ( 'NONE', *, *, #41110, .T. ) ;
#39001 = ORIENTED_EDGE ( 'NONE', *, *, #9860, .T. ) ;
#39002 =( BOUNDED_CURVE ( )  B_SPLINE_CURVE ( 2, ( #40260, #10697, #23891, #4238, #7690, #14130, #37466 ),
 .UNSPECIFIED., .F., .F. ) 
 B_SPLINE_CURVE_WITH_KNOTS ( ( 3, 2, 2, 3 ),
 ( 0.1716417910447761430, 0.1728855721393035005, 0.1741293532338308858, 0.1753731343283582433 ),
 .UNSPECIFIED. ) 
 CURVE ( )  GEOMETRIC_REPRESENTATION_ITEM ( )  RATIONAL_B_SPLINE_CURVE ( ( 0.9999999999999970024, 0.8660254037844417052, 1.000000000000000000, 0.8660254037844387076, 1.000000000000000000, 0.8660254037844357100, 1.000000000000003109 ) ) 
 REPRESENTATION_ITEM ( '' )  );
#39003 = CARTESIAN_POINT ( 'NONE',  ( -10.81189881249999729, 6.242252689847871849, -32.21875000204835970 ) ) ;
#39004 = CARTESIAN_POINT ( 'NONE',  ( -10.81189881249999729, 1.324075727343319199E-15, -27.78125000204837036 ) ) ;
#39005 = DATE_TIME_ROLE ( 'classification_date' ) ;
#39006 = CARTESIAN_POINT ( 'NONE',  ( -5.405949406250003975, -9.363379034771801557, -82.84375000204836681 ) ) ;
#39007 = CARTESIAN_POINT ( 'NONE',  ( -10.00000000000076916, 5.773502691895813221, -127.7500000040967763 ) ) ;
#39008 = CARTESIAN_POINT ( 'NONE',  ( 5.405949406249992428, -9.363379034771808662, -198.0937500020484094 ) ) ;
#39009 = EDGE_CURVE ( 'NONE', #10480, #39684, #21735, .T. ) ;
#39010 = CARTESIAN_POINT ( 'NONE',  ( -9.999999999999998224, 1.224646799147353059E-15, -124.2500000000000000 ) ) ;
#39011 = PLANE ( 'NONE',  #41161 ) ;
#39012 = CARTESIAN_POINT ( 'NONE',  ( 10.81189881249999729, 0.000000000000000000, -156.0312500020484094 ) ) ;
#39013 = CARTESIAN_POINT ( 'NONE',  ( 4.999999999999992006, -8.660254037844389075, -14.62500000409674961 ) ) ;
#39014 = CARTESIAN_POINT ( 'NONE',  ( 9.999999999999998224, 0.000000000000000000, -122.0000000000000000 ) ) ;
#39015 = CARTESIAN_POINT ( 'NONE',  ( -2.293366432827344421E-15, -12.48450537969573659, -126.2187500020483952 ) ) ;
#39016 = CARTESIAN_POINT ( 'NONE',  ( 10.81189881249999551, -6.242252689847874514, -94.65625000204838102 ) ) ;
#39017 = CARTESIAN_POINT ( 'NONE',  ( -10.81189881249999729, 1.324075727343319199E-15, -111.5937500020483810 ) ) ;
#39018 = AXIS2_PLACEMENT_3D ( 'NONE', #29786, #13769, #6894 ) ;
#39019 = CARTESIAN_POINT ( 'NONE',  ( 7.644554776091147741E-16, 12.48450537969573659, -78.96875000204839523 ) ) ;
#39020 = CARTESIAN_POINT ( 'NONE',  ( 7.644554776091147741E-16, 12.48450537969573659, -88.15625000204838102 ) ) ;
#39021 = CARTESIAN_POINT ( 'NONE',  ( 4.999999999999992006, -8.660254037844389075, -172.1250000040968189 ) ) ;
#39022 = CYLINDRICAL_SURFACE ( 'NONE', #19251, 9.999999999999998224 ) ;
#39023 = CARTESIAN_POINT ( 'NONE',  ( -5.405949406250003975, -9.363379034771801557, -165.5312500020484094 ) ) ;
#39024 = CARTESIAN_POINT ( 'NONE',  ( -5.405949406250003975, -9.363379034771801557, -183.5312500020484094 ) ) ;
#39025 = CARTESIAN_POINT ( 'NONE',  ( -9.999999999999998224, 5.773502691896259087, -159.2500000040967905 ) ) ;
#39026 = DIRECTION ( 'NONE',  ( 1.000000000000000000, 0.000000000000000000, 0.000000000000000000 ) ) ;
#39027 = CARTESIAN_POINT ( 'NONE',  ( -10.81189881249999907, -6.242252689847864744, -1.968750002048352599 ) ) ;
#39028 = CARTESIAN_POINT ( 'NONE',  ( -2.121150477449813534E-15, -11.54700538379251284, -126.8749999999999858 ) ) ;
#39029 = CARTESIAN_POINT ( 'NONE',  ( -10.81189881249999907, -6.242252689847864744, -112.9687500020483810 ) ) ;
#39030 = CARTESIAN_POINT ( 'NONE',  ( -9.999999999999998224, 1.224646799147353059E-15, -91.24999999999998579 ) ) ;
#39031 = CARTESIAN_POINT ( 'NONE',  ( -2.293366432827344421E-15, -12.48450537969573659, -15.40625000204837214 ) ) ;
#39032 = CARTESIAN_POINT ( 'NONE',  ( -2.121150477449813534E-15, -11.54700538379251284, -95.75000000409677625 ) ) ;
#39033 = CARTESIAN_POINT ( 'NONE',  ( 0.000000000000000000, 0.000000000000000000, -99.99999999999998579 ) ) ;
#39034 = CARTESIAN_POINT ( 'NONE',  ( -2.293366432827344421E-15, -12.48450537969573659, -111.4062500020483952 ) ) ;
#39035 = CARTESIAN_POINT ( 'NONE',  ( 7.644554776091147741E-16, 12.48450537969573659, -91.15625000204838102 ) ) ;
#39036 = VERTEX_POINT ( 'NONE', #34179 ) ;
#39037 = CARTESIAN_POINT ( 'NONE',  ( -9.999999999999998224, 5.773502691896259087, -81.25000000409677625 ) ) ;
#39038 = FACE_OUTER_BOUND ( 'NONE', #23008, .T. ) ;
#39039 = CARTESIAN_POINT ( 'NONE',  ( -10.81189881249999729, 6.242252689847871849, -42.71875000204835970 ) ) ;
#39040 = VERTEX_POINT ( 'NONE', #34390 ) ;
#39041 = CARTESIAN_POINT ( 'NONE',  ( 7.070501591499377789E-16, 11.54700538379251284, -19.62499999999997868 ) ) ;
#39042 = CARTESIAN_POINT ( 'NONE',  ( 5.000000000000000000, 8.660254037844385522, -154.7500000000000000 ) ) ;
#39043 = CARTESIAN_POINT ( 'NONE',  ( 5.000000000000000000, 8.660254037844385522, -23.12500000409675849 ) ) ;
#39044 = FACE_OUTER_BOUND ( 'NONE', #11738, .T. ) ;
#39046 = ORIENTED_EDGE ( 'NONE', *, *, #31628, .T. ) ;
#39045 = CARTESIAN_POINT ( 'NONE',  ( 5.405949406249992428, -9.363379034771808662, -126.2812500020483668 ) ) ;
#39047 = CARTESIAN_POINT ( 'NONE',  ( -5.000000000000003553, -8.660254037844383745, -12.99999999999995559 ) ) ;
#39048 = ORIENTED_EDGE ( 'NONE', *, *, #15615, .T. ) ;
#39049 = CARTESIAN_POINT ( 'NONE',  ( 10.81189881249999551, -6.242252689847874514, -57.15625000204837391 ) ) ;
#39050 = SHAPE_DEFINITION_REPRESENTATION ( #17307, #10057 ) ;
#39051 = CARTESIAN_POINT ( 'NONE',  ( -10.81189881249999729, 6.242252689847871849, -102.7187500020483810 ) ) ;
#39053 = VERTEX_POINT ( 'NONE', #14716 ) ;
#39052 = EDGE_LOOP ( 'NONE', ( #23292, #26582, #6668, #34992 ) ) ;
#39054 = CYLINDRICAL_SURFACE ( 'NONE', #21801, 9.999999999999998224 ) ;
#39055 = CARTESIAN_POINT ( 'NONE',  ( -2.121150477449813534E-15, -11.54700538379251284, -116.3749999999999858 ) ) ;
#39056 = CARTESIAN_POINT ( 'NONE',  ( 5.405949406249999534, 9.363379034771803333, -181.2812500020483810 ) ) ;
#39057 = CARTESIAN_POINT ( 'NONE',  ( -9.999999999999868550, 5.773502691896333694, -175.3750000000000000 ) ) ;
#39058 = DIRECTION ( 'NONE',  ( 0.5000000000000003331, -0.8660254037844383745, 0.000000000000000000 ) ) ;
#39059 = EDGE_CURVE ( 'NONE', #20204, #5974, #39362, .T. ) ;
#39060 = CARTESIAN_POINT ( 'NONE',  ( -10.81189881249999729, 1.324075727343319199E-15, -137.0937500020483810 ) ) ;
#39061 = CARTESIAN_POINT ( 'NONE',  ( -5.405949406249996869, 9.363379034771805109, -102.8437500020483810 ) ) ;
#39062 = DIRECTION ( 'NONE',  ( -0.000000000000000000, -0.000000000000000000, 1.000000000000000000 ) ) ;
#39063 = CARTESIAN_POINT ( 'NONE',  ( -10.81189881249999907, -6.242252689847864744, -111.6562500020483952 ) ) ;
#39064 = CARTESIAN_POINT ( 'NONE',  ( -4.999999999999996447, 8.660254037844387298, -196.8750000040967905 ) ) ;
#39065 = CARTESIAN_POINT ( 'NONE',  ( -10.81189881249999729, 1.324075727343319199E-15, -111.5937500020483810 ) ) ;
#39066 = CARTESIAN_POINT ( 'NONE',  ( -10.81189881249999729, 6.242252689847871849, -185.4062500020484094 ) ) ;
#39067 = LINE ( 'NONE', #29362, #41271 ) ;
#39068 = CARTESIAN_POINT ( 'NONE',  ( -9.999999999999998224, 1.224646799147353059E-15, -137.7499999999999716 ) ) ;
#39069 = CARTESIAN_POINT ( 'NONE',  ( -9.999999999999998224, 1.224646799147353059E-15, -7.249999999999978684 ) ) ;
#39070 = CARTESIAN_POINT ( 'NONE',  ( 10.81189881249999729, 0.000000000000000000, -70.34375000204836681 ) ) ;
#39071 = CARTESIAN_POINT ( 'NONE',  ( 10.81189881249999729, 0.000000000000000000, -52.34375000204835260 ) ) ;
#39072 = DESIGN_CONTEXT ( 'detailed design', #42159, 'design' ) ;
#39073 = CARTESIAN_POINT ( 'NONE',  ( 4.999999999999992006, -8.660254037844389075, -176.6250000040968189 ) ) ;
#39074 = CARTESIAN_POINT ( 'NONE',  ( 10.81189881249999907, 6.242252689847868297, -25.40625000204838813 ) ) ;
#39075 = CARTESIAN_POINT ( 'NONE',  ( 7.644554776091147741E-16, 12.48450537969573659, -26.46875000204837391 ) ) ;
#39076 = CARTESIAN_POINT ( 'NONE',  ( -10.00000000000051337, 5.773502691895962435, -116.8749999999999858 ) ) ;
#39077 = CARTESIAN_POINT ( 'NONE',  ( 7.644554776091147741E-16, 12.48450537969573659, -134.4687500020483810 ) ) ;
#39078 = CARTESIAN_POINT ( 'NONE',  ( 9.999999999999998224, 0.000000000000000000, -111.4999999999999858 ) ) ;
#39079 = CARTESIAN_POINT ( 'NONE',  ( 7.070501591499376803E-16, 11.54700538379251284, -111.1249999999999858 ) ) ;
#39080 = CARTESIAN_POINT ( 'NONE',  ( -10.00000000000000000, -5.773502691896251982, -68.62499999999998579 ) ) ;
#39081 = CARTESIAN_POINT ( 'NONE',  ( -10.81189881249999729, 6.242252689847871849, -129.9062500020483810 ) ) ;
#39082 = CARTESIAN_POINT ( 'NONE',  ( -5.405949406249996869, 9.363379034771805109, -116.5312500020483952 ) ) ;
#39083 = VERTEX_POINT ( 'NONE', #1152 ) ;
#39084 = CARTESIAN_POINT ( 'NONE',  ( -9.999999999999998224, 1.224646799147353059E-15, -120.1250000040967905 ) ) ;
#39085 = CARTESIAN_POINT ( 'NONE',  ( 10.00000000000000000, 5.773502691896255534, -104.2500000040967763 ) ) ;
#39086 = CARTESIAN_POINT ( 'NONE',  ( 9.999999999999872102, 5.773502691896329253, -169.8750000000000000 ) ) ;
#39087 = CARTESIAN_POINT ( 'NONE',  ( -10.81189881249999907, -6.242252689847864744, -67.96875000204838102 ) ) ;
#39088 = EDGE_LOOP ( 'NONE', ( #26162, #16309 ) ) ;
#39089 = CARTESIAN_POINT ( 'NONE',  ( -5.000000000000003553, -8.660254037844383745, -42.99999999999998579 ) ) ;
#39090 = CARTESIAN_POINT ( 'NONE',  ( -2.121150477449813534E-15, -11.54700538379251284, -20.75000000409677980 ) ) ;
#39091 = CARTESIAN_POINT ( 'NONE',  ( -10.81189881249999729, 1.324075727343319199E-15, -41.28125000204838102 ) ) ;
#39092 = CARTESIAN_POINT ( 'NONE',  ( -1.040834085586084257E-14, -125.0000000000000000, 22.49999999999999289 ) ) ;
#39093 = CARTESIAN_POINT ( 'NONE',  ( 4.999999999999992006, -8.660254037844389075, -47.62500000409677625 ) ) ;
#39094 = CARTESIAN_POINT ( 'NONE',  ( 7.644554776091147741E-16, 12.48450537969573659, -38.65625000204836681 ) ) ;
#39095 = CARTESIAN_POINT ( 'NONE',  ( -9.999999999999998224, 1.224646799147353059E-15, -156.1250000040967905 ) ) ;
#39096 = CARTESIAN_POINT ( 'NONE',  ( -5.405949406249996869, 9.363379034771805109, -136.0312500020484094 ) ) ;
#39097 = CARTESIAN_POINT ( 'NONE',  ( -5.405949406250003975, -9.363379034771801557, -146.0312500020483810 ) ) ;
#39098 = CARTESIAN_POINT ( 'NONE',  ( 9.999999999999998224, 0.000000000000000000, -109.9999999999999858 ) ) ;
#39099 = ORIENTED_EDGE ( 'NONE', *, *, #29386, .T. ) ;
#39100 = VERTEX_POINT ( 'NONE', #37174 ) ;
#39101 = VERTEX_POINT ( 'NONE', #14275 ) ;
#39102 = DIRECTION ( 'NONE',  ( -1.000000000000000000, 0.000000000000000000, 0.000000000000000000 ) ) ;
#39103 = CARTESIAN_POINT ( 'NONE',  ( -2.293366432827344421E-15, -12.48450537969573659, -171.2187500020484094 ) ) ;
#39104 = CARTESIAN_POINT ( 'NONE',  ( -5.405949406249996869, 9.363379034771805109, -23.34375000204835970 ) ) ;
#39105 = CYLINDRICAL_SURFACE ( 'NONE', #41882, 5.000000000000002665 ) ;
#39106 = VECTOR ( 'NONE', #32551, 1000.000000000000000 ) ;
#39107 = EDGE_CURVE ( 'NONE', #34857, #27421, #26643, .T. ) ;
#39108 = CARTESIAN_POINT ( 'NONE',  ( -2.293366432827344421E-15, -12.48450537969573659, -166.7187500020483810 ) ) ;
#39109 = CARTESIAN_POINT ( 'NONE',  ( -10.81189881249999907, -6.242252689847864744, -142.9687500020484094 ) ) ;
#39110 = EDGE_CURVE ( 'NONE', #11539, #3816, #5734, .T. ) ;
#39111 = LINE ( 'NONE', #32234, #30053 ) ;
#39112 = CARTESIAN_POINT ( 'NONE',  ( -10.81189881249999729, 1.324075727343319199E-15, -126.5937500020483668 ) ) ;
#39113 = CARTESIAN_POINT ( 'NONE',  ( 10.81189881249999907, 6.242252689847868297, -130.4062500020483810 ) ) ;
#39115 = CARTESIAN_POINT ( 'NONE',  ( -10.81189881249999729, 6.242252689847871849, -21.71875000204837036 ) ) ;
#39114 =( BOUNDED_CURVE ( )  B_SPLINE_CURVE ( 2, ( #27161, #13754, #3868, #20461, #847, #16353, #30414 ),
 .UNSPECIFIED., .F., .F. ) 
 B_SPLINE_CURVE_WITH_KNOTS ( ( 3, 2, 2, 3 ),
 ( 0.8059701492537315604, 0.8072139303482589456, 0.8084577114427863309, 0.8097014925373136052 ),
 .UNSPECIFIED. ) 
 CURVE ( )  GEOMETRIC_REPRESENTATION_ITEM ( )  RATIONAL_B_SPLINE_CURVE ( ( 0.9999999999999761302, 0.8660254037844625774, 1.000000000000000000, 0.8660254037844387076, 1.000000000000000000, 0.8660254037844148378, 1.000000000000023981 ) ) 
 REPRESENTATION_ITEM ( '' )  );
#39117 = EDGE_CURVE ( 'NONE', #33917, #1371, #28046, .T. ) ;
#39116 = CARTESIAN_POINT ( 'NONE',  ( -2.293366432827344421E-15, -12.48450537969573659, -145.7187500020484094 ) ) ;
#39118 = CARTESIAN_POINT ( 'NONE',  ( 8.614196012144985204, -6.533971456632194474, -180.0000000000000000 ) ) ;
#39119 = CARTESIAN_POINT ( 'NONE',  ( 5.000000000000000000, 8.660254037844385522, -141.6250000040967905 ) ) ;
#39120 = CARTESIAN_POINT ( 'NONE',  ( -9.999999999999998224, 1.224646799147353059E-15, -166.2500000000000000 ) ) ;
#39121 = CARTESIAN_POINT ( 'NONE',  ( -5.000000000000003553, -8.660254037844383745, -17.49999999999996092 ) ) ;
#39122 = CARTESIAN_POINT ( 'NONE',  ( -10.81189881249999729, 6.242252689847871849, -75.71875000204836681 ) ) ;
#39123 = CARTESIAN_POINT ( 'NONE',  ( -10.81189881249999729, 6.242252689847871849, -47.40625000204835970 ) ) ;
#39124 = CARTESIAN_POINT ( 'NONE',  ( 10.81189881249999907, 6.242252689847868297, -52.21875000204837391 ) ) ;
#39125 = CARTESIAN_POINT ( 'NONE',  ( 0.000000000000000000, 0.000000000000000000, -99.99999999999998579 ) ) ;
#39126 = CARTESIAN_POINT ( 'NONE',  ( 10.81189881249999729, 0.000000000000000000, -161.8437500020484094 ) ) ;
#39127 = CARTESIAN_POINT ( 'NONE',  ( 9.999999999999996447, -5.773502691896262640, -140.1250000000000000 ) ) ;
#39128 = CARTESIAN_POINT ( 'NONE',  ( 10.81189881249999729, 6.242252689847867408, -137.9062500020484094 ) ) ;
#39129 = CC_DESIGN_PERSON_AND_ORGANIZATION_ASSIGNMENT ( #18298, #34295, ( #20655 ) ) ;
#39130 = FACE_OUTER_BOUND ( 'NONE', #18970, .T. ) ;
#39131 = CARTESIAN_POINT ( 'NONE',  ( 9.999999999999998224, 0.000000000000000000, -110.3750000040967763 ) ) ;
#39132 = CARTESIAN_POINT ( 'NONE',  ( -4.999999999999996447, 8.660254037844387298, -92.99999999999998579 ) ) ;
#39133 = ORIENTED_EDGE ( 'NONE', *, *, #20719, .T. ) ;
#39134 =( BOUNDED_CURVE ( )  B_SPLINE_CURVE ( 2, ( #12735, #31789, #15768, #9310, #25310, #19025, #15560 ),
 .UNSPECIFIED., .F., .F. ) 
 B_SPLINE_CURVE_WITH_KNOTS ( ( 3, 2, 2, 3 ),
 ( 0.3880597014925373789, 0.3893034825870647087, 0.3905472636815920939, 0.3917910447761194792 ),
 .UNSPECIFIED. ) 
 CURVE ( )  GEOMETRIC_REPRESENTATION_ITEM ( )  RATIONAL_B_SPLINE_CURVE ( ( 0.9999999999999940048, 0.8660254037844447028, 1.000000000000000000, 0.8660254037844387076, 1.000000000000000000, 0.8660254037844327124, 1.000000000000005995 ) ) 
 REPRESENTATION_ITEM ( '' )  );
#39135 = CARTESIAN_POINT ( 'NONE',  ( -10.81189881249999729, 6.242252689847871849, -120.9062500020483952 ) ) ;
#39136 = CARTESIAN_POINT ( 'NONE',  ( 9.999999999999996447, -5.773502691896262640, -137.5000000040967905 ) ) ;
#39137 = DIRECTION ( 'NONE',  ( 1.000000000000000000, 0.000000000000000000, 0.000000000000000000 ) ) ;
#39138 = CARTESIAN_POINT ( 'NONE',  ( 10.81189881249999907, 6.242252689847868297, -169.4062500020484094 ) ) ;
#39139 = CARTESIAN_POINT ( 'NONE',  ( -10.00000000000000000, -5.773502691896251982, -49.50000000409676915 ) ) ;
#39140 = EDGE_CURVE ( 'NONE', #28517, #9895, #31072, .T. ) ;
#39141 = DIRECTION ( 'NONE',  ( -0.000000000000000000, -0.000000000000000000, 1.000000000000000000 ) ) ;
#39142 = CARTESIAN_POINT ( 'NONE',  ( -5.405949406250003975, -9.363379034771801557, -57.53125000204836681 ) ) ;
#39143 = CARTESIAN_POINT ( 'NONE',  ( 9.999999999999998224, 0.000000000000000000, -200.0000000000000000 ) ) ;
#39144 = CARTESIAN_POINT ( 'NONE',  ( -10.81189881249999729, 6.242252689847871849, -159.9062500020483810 ) ) ;
#39145 = EDGE_CURVE ( 'NONE', #39053, #41888, #31584, .T. ) ;
#39146 = CARTESIAN_POINT ( 'NONE',  ( 10.81189881249999907, 6.242252689847868297, -145.2187500020484094 ) ) ;
#39147 = AXIS2_PLACEMENT_3D ( 'NONE', #10440, #39374, #39794 ) ;
#39148 = CYLINDRICAL_SURFACE ( 'NONE', #10470, 9.999999999999998224 ) ;
#39149 = CARTESIAN_POINT ( 'NONE',  ( 0.000000000000000000, 0.000000000000000000, -200.0000000000000000 ) ) ;
#39150 = ORIENTED_EDGE ( 'NONE', *, *, #37255, .F. ) ;
#39151 = CARTESIAN_POINT ( 'NONE',  ( -9.999999999999998224, 1.224646799147353059E-15, -31.24999999999997158 ) ) ;
#39153 = ORIENTED_EDGE ( 'NONE', *, *, #39350, .F. ) ;
#39152 = CARTESIAN_POINT ( 'NONE',  ( -10.81189881249999729, 1.324075727343319199E-15, -72.78125000204838102 ) ) ;
#39155 = ORIENTED_EDGE ( 'NONE', *, *, #20669, .T. ) ;
#39154 = CARTESIAN_POINT ( 'NONE',  ( -5.405949406249996869, 9.363379034771805109, -119.3437500020483810 ) ) ;
#39156 = EDGE_CURVE ( 'NONE', #7656, #34021, #5991, .T. ) ;
#39157 = EDGE_LOOP ( 'NONE', ( #38718, #22859, #3384, #13207 ) ) ;
#39158 = CARTESIAN_POINT ( 'NONE',  ( -5.405949406249996869, 9.363379034771805109, -27.84375000204836326 ) ) ;
#39159 = CARTESIAN_POINT ( 'NONE',  ( -10.81189881249999729, 6.242252689847871849, -194.2187500020483810 ) ) ;
#39160 = CARTESIAN_POINT ( 'NONE',  ( -10.81189881249999907, -6.242252689847864744, -58.96875000204836681 ) ) ;
#39161 = CARTESIAN_POINT ( 'NONE',  ( 9.999999999999998224, 1.224646799147353059E-15, -99.99999999999998579 ) ) ;
#39162 = CARTESIAN_POINT ( 'NONE',  ( -2.121150477449813534E-15, -11.54700538379251284, -30.87499999999995737 ) ) ;
#39163 = CARTESIAN_POINT ( 'NONE',  ( -5.405949406249996869, 9.363379034771805109, -191.3437500020484094 ) ) ;
#39164 = CARTESIAN_POINT ( 'NONE',  ( -10.81189881249999729, 6.242252689847871849, -171.7187500020483810 ) ) ;
#39165 = CARTESIAN_POINT ( 'NONE',  ( 10.81189881249999907, 6.242252689847868297, -146.7187500020484094 ) ) ;
#39166 = CARTESIAN_POINT ( 'NONE',  ( -5.405949406249996869, 9.363379034771805109, -171.8437500020484094 ) ) ;
#39167 = DIRECTION ( 'NONE',  ( 8.659560562354921765E-17, 0.7071067811865484609, -0.7071067811865465735 ) ) ;
#39168 = CARTESIAN_POINT ( 'NONE',  ( -2.121150477449813534E-15, -11.54700538379251284, -161.7500000040968189 ) ) ;
#39169 = CARTESIAN_POINT ( 'NONE',  ( -2.121150477449813534E-15, -11.54700538379251284, -189.8750000000000000 ) ) ;
#39170 = CARTESIAN_POINT ( 'NONE',  ( 7.644554776091147741E-16, 12.48450537969573659, -98.46875000204839523 ) ) ;
#39171 = CARTESIAN_POINT ( 'NONE',  ( -9.999999999999479527, -5.773502691896549521, -48.00000000409674783 ) ) ;
#39172 = CARTESIAN_POINT ( 'NONE',  ( 10.81189881249999729, 0.000000000000000000, -75.03125000204838102 ) ) ;
#39173 = DIRECTION ( 'NONE',  ( -1.000000000000000000, 0.000000000000000000, 0.000000000000000000 ) ) ;
#39174 = CARTESIAN_POINT ( 'NONE',  ( -2.293366432827344421E-15, -12.48450537969573659, -189.2187500020484094 ) ) ;
#39175 = CARTESIAN_POINT ( 'NONE',  ( 10.81189881249999729, 6.242252689847867408, -82.21875000204836681 ) ) ;
#39176 = VECTOR ( 'NONE', #917, 1000.000000000000000 ) ;
#39177 = CARTESIAN_POINT ( 'NONE',  ( -5.405949406250003975, -9.363379034771801557, -63.53125000204837391 ) ) ;
#39178 = CARTESIAN_POINT ( 'NONE',  ( 4.999999999999992006, -8.660254037844389075, -145.1250000040967905 ) ) ;
#39179 = CARTESIAN_POINT ( 'NONE',  ( -5.000000000000003553, -8.660254037844383745, -113.4999999999999858 ) ) ;
#39180 = ORIENTED_EDGE ( 'NONE', *, *, #38049, .T. ) ;
#39181 = CARTESIAN_POINT ( 'NONE',  ( 10.81189881249999729, 6.242252689847867408, -143.9062500020484094 ) ) ;
#39182 = CARTESIAN_POINT ( 'NONE',  ( 7.644554776091147741E-16, 12.48450537969573659, -158.6562500020484094 ) ) ;
#39183 = EDGE_CURVE ( 'NONE', #32177, #4342, #20624, .T. ) ;
#39184 = DIRECTION ( 'NONE',  ( -0.000000000000000000, -0.000000000000000000, 1.000000000000000000 ) ) ;
#39185 = CARTESIAN_POINT ( 'NONE',  ( -10.00000000000019362, -5.773502691896140959, -179.6250000000000568 ) ) ;
#39186 = CARTESIAN_POINT ( 'NONE',  ( 7.644554776091147741E-16, 12.48450537969573659, -93.96875000204838102 ) ) ;
#39187 = VERTEX_POINT ( 'NONE', #8909 ) ;
#39188 = CARTESIAN_POINT ( 'NONE',  ( 4.999999999999992006, -8.660254037844389075, -57.74999999999997158 ) ) ;
#39189 = CARTESIAN_POINT ( 'NONE',  ( 10.81189881249999907, 6.242252689847868297, -188.7187500020484094 ) ) ;
#39190 = CARTESIAN_POINT ( 'NONE',  ( 9.999999999999998224, 0.000000000000000000, -71.37500000409677625 ) ) ;
#39191 = CARTESIAN_POINT ( 'NONE',  ( 0.000000000000000000, 0.000000000000000000, -200.0000000000000000 ) ) ;
#39192 = LINE ( 'NONE', #16504, #14810 ) ;
#39193 = CARTESIAN_POINT ( 'NONE',  ( 5.405949406249999534, 9.363379034771803333, -86.78125000204838102 ) ) ;
#39194 = CARTESIAN_POINT ( 'NONE',  ( -5.405949406250003975, -9.363379034771801557, -71.03125000204838102 ) ) ;
#39195 = CARTESIAN_POINT ( 'NONE',  ( 10.00000000000000000, 5.773502691896255534, -63.75000000409677625 ) ) ;
#39196 = CARTESIAN_POINT ( 'NONE',  ( -10.81189881249999907, -6.242252689847864744, -18.46875000204836681 ) ) ;
#39197 = CARTESIAN_POINT ( 'NONE',  ( -2.121150477449813534E-15, -11.54700538379251284, -151.2500000040968189 ) ) ;
#39198 = CARTESIAN_POINT ( 'NONE',  ( 10.81189881249999907, 6.242252689847868297, -181.4062500020484379 ) ) ;
#39199 = CARTESIAN_POINT ( 'NONE',  ( -10.81189881249999729, 1.324075727343319199E-15, -9.781250002048352599 ) ) ;
#39200 = CARTESIAN_POINT ( 'NONE',  ( -9.999999999999998224, 1.224646799147353059E-15, -200.0000000000000000 ) ) ;
#39201 = CARTESIAN_POINT ( 'NONE',  ( 10.00000000000000000, 5.773502691896255534, -137.2500000040967905 ) ) ;
#39202 = DIRECTION ( 'NONE',  ( -0.000000000000000000, -0.000000000000000000, 1.000000000000000000 ) ) ;
#39203 = CARTESIAN_POINT ( 'NONE',  ( -2.121150477449813534E-15, -11.54700538379251284, -137.3750000000000000 ) ) ;
#39204 = CARTESIAN_POINT ( 'NONE',  ( -10.00000000000000000, -5.773502691896251982, -176.6250000000000284 ) ) ;
#39205 = CARTESIAN_POINT ( 'NONE',  ( -9.999999999999998224, 1.224646799147353059E-15, -97.24999999999998579 ) ) ;
#39207 = ORIENTED_EDGE ( 'NONE', *, *, #26621, .F. ) ;
#39206 = CARTESIAN_POINT ( 'NONE',  ( 7.644554776091147741E-16, 12.48450537969573659, -94.15625000204839523 ) ) ;
#39208 = CIRCLE ( 'NONE', #40569, 60.00000000000000711 ) ;
#39209 = ORIENTED_EDGE ( 'NONE', *, *, #20300, .F. ) ;
#39210 =( BOUNDED_CURVE ( )  B_SPLINE_CURVE ( 2, ( #28839, #38962, #15004, #5529, #19108, #25598, #35103 ),
 .UNSPECIFIED., .F., .F. ) 
 B_SPLINE_CURVE_WITH_KNOTS ( ( 3, 2, 2, 3 ),
 ( 0.03358208955223884046, 0.03482587064676620492, 0.03606965174129356938, 0.03731343283582092690 ),
 .UNSPECIFIED. ) 
 CURVE ( )  GEOMETRIC_REPRESENTATION_ITEM ( )  RATIONAL_B_SPLINE_CURVE ( ( 0.9999999999999963363, 0.8660254037844424824, 1.000000000000000000, 0.8660254037844387076, 1.000000000000000000, 0.8660254037844349329, 1.000000000000003775 ) ) 
 REPRESENTATION_ITEM ( '' )  );
#39211 = ORIENTED_EDGE ( 'NONE', *, *, #7629, .F. ) ;
#39212 = CARTESIAN_POINT ( 'NONE',  ( -10.81189881249999729, 1.324075727343319199E-15, -35.09375000204836681 ) ) ;
#39213 = CARTESIAN_POINT ( 'NONE',  ( 10.81189881249999729, 0.000000000000000000, -18.03125000204835970 ) ) ;
#39214 = APPROVAL_STATUS ( 'not_yet_approved' ) ;
#39215 = CARTESIAN_POINT ( 'NONE',  ( -5.405949406249996869, 9.363379034771805109, -77.34375000204838102 ) ) ;
#39216 = LINE ( 'NONE', #42654, #23607 ) ;
#39217 = CARTESIAN_POINT ( 'NONE',  ( -2.293366432827344421E-15, -12.48450537969573659, -193.7187500020484094 ) ) ;
#39218 = LINE ( 'NONE', #22191, #9518 ) ;
#39219 = AXIS2_PLACEMENT_3D ( 'NONE', #42087, #19215, #35845 ) ;
#39220 = CARTESIAN_POINT ( 'NONE',  ( 9.999999999999998224, 0.000000000000000000, -143.3750000040967905 ) ) ;
#39221 = CARTESIAN_POINT ( 'NONE',  ( -5.405949406250003975, -9.363379034771801557, -158.0312500020484094 ) ) ;
#39222 = CARTESIAN_POINT ( 'NONE',  ( -4.999999999999996447, 8.660254037844387298, -0.3750000040967649273 ) ) ;
#39223 = CARTESIAN_POINT ( 'NONE',  ( -9.999999999999804601, 5.773502691896371886, -178.3750000000000284 ) ) ;
#39224 = CARTESIAN_POINT ( 'NONE',  ( -2.293366432827344421E-15, -12.48450537969573659, -123.2187500020483952 ) ) ;
#39225 = CARTESIAN_POINT ( 'NONE',  ( -10.81189881249999907, -6.242252689847864744, -101.1562500020483952 ) ) ;
#39226 = CARTESIAN_POINT ( 'NONE',  ( -10.81189881249999729, 1.324075727343319199E-15, -105.5937500020483810 ) ) ;
#39227 = CARTESIAN_POINT ( 'NONE',  ( -10.81189881249999907, -6.242252689847864744, -78.46875000204838102 ) ) ;
#39228 = CARTESIAN_POINT ( 'NONE',  ( 7.644554776091147741E-16, 12.48450537969573659, -86.65625000204838102 ) ) ;
#39229 = CARTESIAN_POINT ( 'NONE',  ( 9.999999999999998224, 0.000000000000000000, -170.3750000040968189 ) ) ;
#39230 = CARTESIAN_POINT ( 'NONE',  ( 9.999999999999998224, 0.000000000000000000, -81.87500000409676204 ) ) ;
#39231 = CARTESIAN_POINT ( 'NONE',  ( 7.644554776091147741E-16, 12.48450537969573659, -163.1562500020483810 ) ) ;
#39232 = CARTESIAN_POINT ( 'NONE',  ( -5.405949406250003975, -9.363379034771801557, -177.5312500020483810 ) ) ;
#39233 = EDGE_CURVE ( 'NONE', #32014, #11758, #41254, .T. ) ;
#39234 = CARTESIAN_POINT ( 'NONE',  ( 9.999999999999996447, -5.773502691896262640, -160.0000000040968189 ) ) ;
#39235 = CARTESIAN_POINT ( 'NONE',  ( 7.644554776091147741E-16, 12.48450537969573659, -6.968750002048357040 ) ) ;
#39236 = CARTESIAN_POINT ( 'NONE',  ( 9.999999999999479527, 5.773502691896553074, -127.8749999999999858 ) ) ;
#39237 = CARTESIAN_POINT ( 'NONE',  ( -5.405949406250003975, -9.363379034771801557, -117.3437500020483810 ) ) ;
#39238 = CARTESIAN_POINT ( 'NONE',  ( 9.999999999999996447, -5.773502691896262640, -81.62499999999998579 ) ) ;
#39239 = CARTESIAN_POINT ( 'NONE',  ( -2.293366432827344421E-15, -12.48450537969573659, -12.40625000204836859 ) ) ;
#39240 = CARTESIAN_POINT ( 'NONE',  ( 5.000000000000000000, 8.660254037844385522, -98.12500000409677625 ) ) ;
#39241 = CARTESIAN_POINT ( 'NONE',  ( 0.000000000000000000, 0.000000000000000000, -200.0000000000000000 ) ) ;
#39242 = CARTESIAN_POINT ( 'NONE',  ( -5.405949406249996869, 9.363379034771805109, -104.5312500020483810 ) ) ;
#39243 = CARTESIAN_POINT ( 'NONE',  ( 10.81189881249999729, 0.000000000000000000, -93.03125000204838102 ) ) ;
#39244 = ORIENTED_EDGE ( 'NONE', *, *, #8166, .T. ) ;
#39245 = CARTESIAN_POINT ( 'NONE',  ( -9.999999999999998224, 5.773502691896259087, -82.75000000409676204 ) ) ;
#39246 = DIRECTION ( 'NONE',  ( -0.000000000000000000, -0.000000000000000000, -1.000000000000000000 ) ) ;
#39247 = CARTESIAN_POINT ( 'NONE',  ( 5.405949406249992428, -9.363379034771808662, -42.09375000204837391 ) ) ;
#39248 = ORIENTED_EDGE ( 'NONE', *, *, #25954, .T. ) ;
#39249 = CARTESIAN_POINT ( 'NONE',  ( -9.999999999999998224, 1.224646799147353059E-15, -17.74999999999996092 ) ) ;
#39250 = VECTOR ( 'NONE', #1367, 1000.000000000000000 ) ;
#39251 = CARTESIAN_POINT ( 'NONE',  ( 9.999999999999998224, 0.000000000000000000, -143.0000000000000000 ) ) ;
#39252 = CARTESIAN_POINT ( 'NONE',  ( -4.999999999999996447, 8.660254037844387298, -13.87500000409674961 ) ) ;
#39253 = EDGE_CURVE ( 'NONE', #17857, #33970, #4338, .T. ) ;
#39254 =( BOUNDED_CURVE ( )  B_SPLINE_CURVE ( 2, ( #33401, #42656, #26487, #10492, #3190, #35992, #30158 ),
 .UNSPECIFIED., .F., .F. ) 
 B_SPLINE_CURVE_WITH_KNOTS ( ( 3, 2, 2, 3 ),
 ( 0.6268656716417911889, 0.6281094527363185742, 0.6293532338308458485, 0.6305970149253732338 ),
 .UNSPECIFIED. ) 
 CURVE ( )  GEOMETRIC_REPRESENTATION_ITEM ( )  RATIONAL_B_SPLINE_CURVE ( ( 0.9999999999999880096, 0.8660254037844506980, 1.000000000000000000, 0.8660254037844387076, 1.000000000000000000, 0.8660254037844267172, 1.000000000000011990 ) ) 
 REPRESENTATION_ITEM ( '' )  );
#39255 = AXIS2_PLACEMENT_3D ( 'NONE', #35488, #28372, #2045 ) ;
#39256 = CARTESIAN_POINT ( 'NONE',  ( -5.000000000000003553, -8.660254037844383745, -197.5000000000000000 ) ) ;
#39258 = EDGE_LOOP ( 'NONE', ( #11759, #33145 ) ) ;
#39257 = CARTESIAN_POINT ( 'NONE',  ( -10.81189881249999907, -6.242252689847864744, -120.6562500020483810 ) ) ;
#39259 = CARTESIAN_POINT ( 'NONE',  ( 5.000000000000000000, 8.660254037844385522, -65.12500000409676204 ) ) ;
#39260 = ORIENTED_EDGE ( 'NONE', *, *, #8656, .T. ) ;
#39261 = CARTESIAN_POINT ( 'NONE',  ( 10.81189881249999729, 0.000000000000000000, -52.53125000204835970 ) ) ;
#39262 = PERSON_AND_ORGANIZATION_ROLE ( 'creator' ) ;
#39263 = CARTESIAN_POINT ( 'NONE',  ( 10.81189881249999551, -6.242252689847874514, -106.4687500020483810 ) ) ;
#39264 = ORIENTED_EDGE ( 'NONE', *, *, #2858, .F. ) ;
#39265 = CARTESIAN_POINT ( 'NONE',  ( -2.121150477449813534E-15, -11.54700538379251284, -83.37499999999997158 ) ) ;
#39266 = CARTESIAN_POINT ( 'NONE',  ( 0.000000000000000000, 0.000000000000000000, -103.0000000000000000 ) ) ;
#39267 = CARTESIAN_POINT ( 'NONE',  ( 7.644554776091147741E-16, 12.48450537969573659, -182.6562500020484094 ) ) ;
#39268 = CARTESIAN_POINT ( 'NONE',  ( 5.405949406249999534, 9.363379034771803333, 0.4062499979516354109 ) ) ;
#39269 = DIRECTION ( 'NONE',  ( 0.000000000000000000, -1.000000000000000000, 0.000000000000000000 ) ) ;
#39270 = CIRCLE ( 'NONE', #17226, 9.999999999999998224 ) ;
#39271 = CARTESIAN_POINT ( 'NONE',  ( -10.81189881249999729, 6.242252689847871849, -134.2187500020483810 ) ) ;
#39272 = CARTESIAN_POINT ( 'NONE',  ( -10.81189881249999907, -6.242252689847864744, -102.4687500020483810 ) ) ;
#39273 = FACE_OUTER_BOUND ( 'NONE', #22877, .T. ) ;
#39274 = CARTESIAN_POINT ( 'NONE',  ( -10.81189881249999729, 1.324075727343319199E-15, -105.7812500020483810 ) ) ;
#39275 = CARTESIAN_POINT ( 'NONE',  ( 5.000000000000000000, 8.660254037844385522, -197.1250000040967905 ) ) ;
#39276 = CARTESIAN_POINT ( 'NONE',  ( -5.405949406250003975, -9.363379034771801557, -112.8437500020483810 ) ) ;
#39277 = CARTESIAN_POINT ( 'NONE',  ( 10.81189881249999729, 6.242252689847867408, -185.9062500020484094 ) ) ;
#39278 = EDGE_CURVE ( 'NONE', #29829, #23935, #29429, .T. ) ;
#39279 = CYLINDRICAL_SURFACE ( 'NONE', #30988, 9.999999999999998224 ) ;
#39280 = CARTESIAN_POINT ( 'NONE',  ( 9.999999999999996447, -5.773502691896262640, -143.1250000000000000 ) ) ;
#39281 = CARTESIAN_POINT ( 'NONE',  ( 4.999999999999992006, -8.660254037844389075, -8.249999999999952038 ) ) ;
#39282 = CARTESIAN_POINT ( 'NONE',  ( 7.644554776091147741E-16, 12.48450537969573659, -63.96875000204838102 ) ) ;
#39283 = CARTESIAN_POINT ( 'NONE',  ( -10.81189881249999729, 1.324075727343319199E-15, -50.09375000204835260 ) ) ;
#39284 = CARTESIAN_POINT ( 'NONE',  ( -4.999999999999996447, 8.660254037844387298, -181.8750000040967905 ) ) ;
#39285 = CARTESIAN_POINT ( 'NONE',  ( -10.81189881249999729, 6.242252689847871849, -17.40625000204838457 ) ) ;
#39286 = CARTESIAN_POINT ( 'NONE',  ( -10.81189881249999907, -6.242252689847864744, -25.96875000204837391 ) ) ;
#39287 = CARTESIAN_POINT ( 'NONE',  ( 5.405949406249992428, -9.363379034771808662, -136.5937500020483810 ) ) ;
#39288 = CARTESIAN_POINT ( 'NONE',  ( 5.000000000000000000, 8.660254037844385522, -102.2500000000000000 ) ) ;
#39289 = DIRECTION ( 'NONE',  ( -0.000000000000000000, -0.000000000000000000, 1.000000000000000000 ) ) ;
#39290 = CARTESIAN_POINT ( 'NONE',  ( -10.00000000000000000, -5.773502691896251982, -64.12499999999998579 ) ) ;
#39291 = CARTESIAN_POINT ( 'NONE',  ( -10.81189881249999729, 1.324075727343319199E-15, -135.7812500020483810 ) ) ;
#39292 = CARTESIAN_POINT ( 'NONE',  ( -10.81189881249999729, 6.242252689847871849, -113.4062500020483952 ) ) ;
#39293 = ORIENTED_EDGE ( 'NONE', *, *, #31002, .F. ) ;
#39294 = CARTESIAN_POINT ( 'NONE',  ( 9.999999999999998224, 0.000000000000000000, -143.0000000000000000 ) ) ;
#39295 = CARTESIAN_POINT ( 'NONE',  ( -5.000000000000003553, -8.660254037844383745, -109.3750000040967763 ) ) ;
#39296 = CARTESIAN_POINT ( 'NONE',  ( 5.405949406249999534, 9.363379034771803333, -67.09375000204836681 ) ) ;
#39297 = VERTEX_POINT ( 'NONE', #2016 ) ;
#39298 = CARTESIAN_POINT ( 'NONE',  ( -5.000000000000003553, -8.660254037844383745, -39.99999999999997868 ) ) ;
#39299 = CARTESIAN_POINT ( 'NONE',  ( -9.999999999999998224, 1.224646799147353059E-15, -16.62500000409675138 ) ) ;
#39300 = CARTESIAN_POINT ( 'NONE',  ( -5.405949406250003975, -9.363379034771801557, -44.03125000204838102 ) ) ;
#39301 = CARTESIAN_POINT ( 'NONE',  ( 9.999999999999998224, 0.000000000000000000, -156.8750000040967905 ) ) ;
#39302 = CARTESIAN_POINT ( 'NONE',  ( -10.00000000000000000, -5.773502691896251982, -36.00000000409675494 ) ) ;
#39303 = CARTESIAN_POINT ( 'NONE',  ( -10.81189881249999729, 1.324075727343319199E-15, -36.78125000204837391 ) ) ;
#39304 = CARTESIAN_POINT ( 'NONE',  ( 0.000000000000000000, 0.000000000000000000, -99.99999999999998579 ) ) ;
#39305 = CARTESIAN_POINT ( 'NONE',  ( 10.81189881249999729, 0.000000000000000000, -135.0312500020484094 ) ) ;
#39306 = CARTESIAN_POINT ( 'NONE',  ( -10.81189881249999729, 1.324075727343319199E-15, -147.7812500020483810 ) ) ;
#39307 = EDGE_CURVE ( 'NONE', #2493, #32481, #6876, .T. ) ;
#39308 = CYLINDRICAL_SURFACE ( 'NONE', #16900, 20.00000000000000000 ) ;
#39309 = ORIENTED_EDGE ( 'NONE', *, *, #12220, .T. ) ;
#39310 = ORIENTED_EDGE ( 'NONE', *, *, #36863, .T. ) ;
#39311 = ORIENTED_EDGE ( 'NONE', *, *, #19650, .T. ) ;
#39312 = CARTESIAN_POINT ( 'NONE',  ( -2.121150477449813534E-15, -11.54700538379251284, -129.8750000000000000 ) ) ;
#39313 = CARTESIAN_POINT ( 'NONE',  ( 5.405949406249999534, 9.363379034771803333, -175.0937500020484094 ) ) ;
#39314 = CARTESIAN_POINT ( 'NONE',  ( -10.81189881249999729, 1.324075727343319199E-15, -24.59375000204835970 ) ) ;
#39315 = CARTESIAN_POINT ( 'NONE',  ( -10.00000000000076916, 5.773502691895813221, -111.2500000040967620 ) ) ;
#39316 = CARTESIAN_POINT ( 'NONE',  ( 10.81189881249999729, 6.242252689847867408, -155.7187500020483810 ) ) ;
#39317 = CARTESIAN_POINT ( 'NONE',  ( 5.405949406249999534, 9.363379034771803333, -145.0937500020483810 ) ) ;
#39318 = CARTESIAN_POINT ( 'NONE',  ( -5.405949406249996869, 9.363379034771805109, -126.8437500020483952 ) ) ;
#39319 = CARTESIAN_POINT ( 'NONE',  ( -2.293366432827344421E-15, -12.48450537969573659, -132.4062500020483810 ) ) ;
#39320 = CARTESIAN_POINT ( 'NONE',  ( 10.81189881249999551, -6.242252689847874514, -19.46875000204837391 ) ) ;
#39321 = CARTESIAN_POINT ( 'NONE',  ( -2.293366432827344421E-15, -12.48450537969573659, -139.7187500020483810 ) ) ;
#39322 = DIRECTION ( 'NONE',  ( -0.000000000000000000, -0.000000000000000000, -1.000000000000000000 ) ) ;
#39323 = CARTESIAN_POINT ( 'NONE',  ( 0.000000000000000000, 0.000000000000000000, -200.0000000000000000 ) ) ;
#39324 = CARTESIAN_POINT ( 'NONE',  ( -4.999999999999996447, 8.660254037844387298, -163.5000000000000000 ) ) ;
#39325 = CARTESIAN_POINT ( 'NONE',  ( -9.999999999999998224, 1.224646799147353059E-15, -200.0000000000000000 ) ) ;
#39326 = CC_DESIGN_APPROVAL ( #5680, ( #2849 ) ) ;
#39327 = CARTESIAN_POINT ( 'NONE',  ( -10.81189881249999907, -6.242252689847864744, -75.46875000204836681 ) ) ;
#39328 = CARTESIAN_POINT ( 'NONE',  ( 7.644554776091147741E-16, 12.48450537969573659, -38.65625000204835260 ) ) ;
#39329 = CARTESIAN_POINT ( 'NONE',  ( 5.405949406249992428, -9.363379034771808662, -54.09375000204835970 ) ) ;
#39330 = LINE ( 'NONE', #19266, #632 ) ;
#39331 = CARTESIAN_POINT ( 'NONE',  ( 10.81189881249999907, 6.242252689847868297, -163.2187500020483810 ) ) ;
#39332 = AXIS2_PLACEMENT_3D ( 'NONE', #6820, #19761, #13484 ) ;
#39333 = CARTESIAN_POINT ( 'NONE',  ( 10.00000000000000000, 5.773502691896255534, -135.3750000000000000 ) ) ;
#39334 = CARTESIAN_POINT ( 'NONE',  ( 10.81189881249999729, 0.000000000000000000, -135.0312500020484094 ) ) ;
#39335 = CARTESIAN_POINT ( 'NONE',  ( 9.999999999999998224, 0.000000000000000000, -200.0000000000000000 ) ) ;
#39336 = CARTESIAN_POINT ( 'NONE',  ( 10.00000000000000000, 5.773502691896255534, -116.2500000040967905 ) ) ;
#39337 = CARTESIAN_POINT ( 'NONE',  ( 9.999999999999998224, 0.000000000000000000, -91.99999999999998579 ) ) ;
#39338 = ORIENTED_EDGE ( 'NONE', *, *, #34657, .F. ) ;
#39339 = CARTESIAN_POINT ( 'NONE',  ( -5.405949406250003975, -9.363379034771801557, -116.0312500020483952 ) ) ;
#39340 = CARTESIAN_POINT ( 'NONE',  ( -5.000000000000003553, -8.660254037844383745, -134.8750000040967905 ) ) ;
#39341 = CARTESIAN_POINT ( 'NONE',  ( -9.999999999998969713, -5.773502691896847949, -22.50000000409674783 ) ) ;
#39342 = CARTESIAN_POINT ( 'NONE',  ( -10.81189881249999729, 6.242252689847871849, -173.4062500020483810 ) ) ;
#39343 = CARTESIAN_POINT ( 'NONE',  ( -9.999999999999998224, 1.224646799147353059E-15, -45.12500000409677625 ) ) ;
#39344 = CARTESIAN_POINT ( 'NONE',  ( -5.405949406250003975, -9.363379034771801557, -62.03125000204837391 ) ) ;
#39345 = CARTESIAN_POINT ( 'NONE',  ( 0.000000000000000000, 0.000000000000000000, -200.0000000000000000 ) ) ;
#39346 = CARTESIAN_POINT ( 'NONE',  ( 7.644554776091147741E-16, 12.48450537969573659, -161.6562500020484379 ) ) ;
#39347 = ADVANCED_FACE ( 'NONE', ( #41902 ), #25534, .T. ) ;
#39348 = CARTESIAN_POINT ( 'NONE',  ( 7.644554776091147741E-16, 12.48450537969573659, -141.9687500020483810 ) ) ;
#39350 = EDGE_CURVE ( 'NONE', #36973, #7623, #14516, .T. ) ;
#39349 = CARTESIAN_POINT ( 'NONE',  ( 9.999999999999998224, 0.000000000000000000, -171.8750000040968189 ) ) ;
#39351 = ORIENTED_EDGE ( 'NONE', *, *, #14112, .T. ) ;
#39352 = EDGE_CURVE ( 'NONE', #37499, #10842, #6881, .T. ) ;
#39353 = CARTESIAN_POINT ( 'NONE',  ( 7.070501591499376803E-16, 11.54700538379251284, -189.5000000040968189 ) ) ;
#39354 = VECTOR ( 'NONE', #16619, 1000.000000000000000 ) ;
#39355 = LOCAL_TIME ( 11, 57, 6.000000000000000000, #21108 ) ;
#39357 = ORIENTED_EDGE ( 'NONE', *, *, #5309, .T. ) ;
#39356 = CARTESIAN_POINT ( 'NONE',  ( -10.81189881249999729, 6.242252689847871849, -71.40625000204838102 ) ) ;
#39358 = COORDINATED_UNIVERSAL_TIME_OFFSET ( 6, 0, .AHEAD. ) ;
#39360 = ORIENTED_EDGE ( 'NONE', *, *, #23820, .F. ) ;
#39359 = CARTESIAN_POINT ( 'NONE',  ( 10.81189881249999729, 0.000000000000000000, -122.8437500020483952 ) ) ;
#39361 = ORIENTED_EDGE ( 'NONE', *, *, #7748, .T. ) ;
#39362 =( BOUNDED_CURVE ( )  B_SPLINE_CURVE ( 2, ( #24466, #21419, #36967, #24251, #27476, #37613, #30517 ),
 .UNSPECIFIED., .F., .F. ) 
 B_SPLINE_CURVE_WITH_KNOTS ( ( 3, 2, 2, 3 ),
 ( 0.2761194029850747578, 0.2773631840796020875, 0.2786069651741294728, 0.2798507462686568026 ),
 .UNSPECIFIED. ) 
 CURVE ( )  GEOMETRIC_REPRESENTATION_ITEM ( )  RATIONAL_B_SPLINE_CURVE ( ( 0.9999999999999880096, 0.8660254037844506980, 1.000000000000000000, 0.8660254037844387076, 1.000000000000000000, 0.8660254037844267172, 1.000000000000011990 ) ) 
 REPRESENTATION_ITEM ( '' )  );
#39363 = CARTESIAN_POINT ( 'NONE',  ( 5.405949406249992428, -9.363379034771808662, -24.09375000204835970 ) ) ;
#39364 = CARTESIAN_POINT ( 'NONE',  ( 10.81189881249999729, 0.000000000000000000, -197.8437500020484094 ) ) ;
#39365 = CARTESIAN_POINT ( 'NONE',  ( -2.293366432827344421E-15, -12.48450537969573659, -46.71875000204835970 ) ) ;
#39366 = CARTESIAN_POINT ( 'NONE',  ( 4.999999999999992006, -8.660254037844389075, -134.2499999999999716 ) ) ;
#39367 = CARTESIAN_POINT ( 'NONE',  ( 9.999999999999996447, -5.773502691896262640, -26.12499999999998224 ) ) ;
#39368 = ADVANCED_FACE ( 'NONE', ( #40299 ), #10319, .T. ) ;
#39369 = CARTESIAN_POINT ( 'NONE',  ( -10.81189881249999729, 6.242252689847871849, -183.7187500020484379 ) ) ;
#39370 = CARTESIAN_POINT ( 'NONE',  ( -2.293366432827344421E-15, -12.48450537969573659, -165.2187500020484094 ) ) ;
#39371 = CARTESIAN_POINT ( 'NONE',  ( 10.81189881249999551, -6.242252689847874514, -151.4687500020483810 ) ) ;
#39372 = CARTESIAN_POINT ( 'NONE',  ( -5.405949406250003975, -9.363379034771801557, -162.3437500020484094 ) ) ;
#39373 = DIRECTION ( 'NONE',  ( 0.000000000000000000, 0.000000000000000000, -1.000000000000000000 ) ) ;
#39374 = DIRECTION ( 'NONE',  ( -0.000000000000000000, -0.000000000000000000, -1.000000000000000000 ) ) ;
#39375 = CARTESIAN_POINT ( 'NONE',  ( 10.00000000000000000, 5.773502691896255534, -184.8750000000000000 ) ) ;
#39376 = CARTESIAN_POINT ( 'NONE',  ( 10.81189881249999551, -6.242252689847874514, -94.46875000204838102 ) ) ;
#39377 = LINE ( 'NONE', #38759, #11393 ) ;
#39378 = CARTESIAN_POINT ( 'NONE',  ( 10.81189881249999907, 6.242252689847868297, -71.90625000204836681 ) ) ;
#39379 = CARTESIAN_POINT ( 'NONE',  ( 7.070501591499376803E-16, 11.54700538379251284, -89.00000000409679046 ) ) ;
#39380 = CARTESIAN_POINT ( 'NONE',  ( -10.81189881249999729, 6.242252689847871849, -182.2187500020484379 ) ) ;
#39381 = EDGE_CURVE ( 'NONE', #20180, #24638, #33227, .T. ) ;
#39382 = ADVANCED_FACE ( 'NONE', ( #30411 ), #10109, .T. ) ;
#39383 = CARTESIAN_POINT ( 'NONE',  ( 10.81189881249999729, 0.000000000000000000, -165.0312500020484094 ) ) ;
#39384 = CARTESIAN_POINT ( 'NONE',  ( -10.81189881249999729, 1.324075727343319199E-15, -59.28125000204836681 ) ) ;
#39385 = CARTESIAN_POINT ( 'NONE',  ( 4.999999999999992006, -8.660254037844389075, -136.1250000040967620 ) ) ;
#39386 = CARTESIAN_POINT ( 'NONE',  ( 7.070501591499377789E-16, 11.54700538379251284, -117.1249999999999858 ) ) ;
#39387 = EDGE_LOOP ( 'NONE', ( #30093, #19355, #22763, #6921 ) ) ;
#39388 = CARTESIAN_POINT ( 'NONE',  ( -10.81189881249999729, -6.242252689847864744, -141.6562500020484094 ) ) ;
#39389 = CARTESIAN_POINT ( 'NONE',  ( -5.405949406250003975, -9.363379034771801557, -156.5312500020484094 ) ) ;
#39390 = CC_DESIGN_SECURITY_CLASSIFICATION ( #40065, ( #42691 ) ) ;
#39391 = CARTESIAN_POINT ( 'NONE',  ( -2.293366432827344421E-15, -12.48450537969573659, -198.4062500020484094 ) ) ;
#39392 = CARTESIAN_POINT ( 'NONE',  ( 9.999999999999998224, 0.000000000000000000, -200.0000000000000000 ) ) ;
#39393 = CARTESIAN_POINT ( 'NONE',  ( 5.405949406249999534, 9.363379034771803333, -86.59375000204836681 ) ) ;
#39394 = VERTEX_POINT ( 'NONE', #36655 ) ;
#39395 = CARTESIAN_POINT ( 'NONE',  ( -4.999999999999996447, 8.660254037844387298, -61.49999999999997158 ) ) ;
#39396 = CARTESIAN_POINT ( 'NONE',  ( 10.81189881249999729, 0.000000000000000000, -191.8437500020484094 ) ) ;
#39397 = CARTESIAN_POINT ( 'NONE',  ( 10.00000000000000000, 5.773502691896255534, -62.25000000409677625 ) ) ;
#39398 = CARTESIAN_POINT ( 'NONE',  ( -10.00000000000102496, 5.773502691895664007, -65.87499999999995737 ) ) ;
#39399 = DIRECTION ( 'NONE',  ( 1.000000000000000000, 0.000000000000000000, 0.000000000000000000 ) ) ;
#39400 = CARTESIAN_POINT ( 'NONE',  ( -10.81189881249999907, -6.242252689847864744, -84.65625000204836681 ) ) ;
#39401 = CARTESIAN_POINT ( 'NONE',  ( 5.405949406249999534, 9.363379034771803333, -70.28125000204838102 ) ) ;
#39402 = CARTESIAN_POINT ( 'NONE',  ( 9.999999999999998224, 0.000000000000000000, -62.37500000409676204 ) ) ;
#39403 = CARTESIAN_POINT ( 'NONE',  ( -5.405949406249996869, 9.363379034771805109, -17.34375000204835260 ) ) ;
#39404 = CARTESIAN_POINT ( 'NONE',  ( -4.999999999999996447, 8.660254037844387298, -37.87500000409676915 ) ) ;
#39405 = CARTESIAN_POINT ( 'NONE',  ( 10.81189881249999907, 6.242252689847868297, -184.4062500020484094 ) ) ;
#39406 = AXIS2_PLACEMENT_3D ( 'NONE', #6267, #10121, #29561 ) ;
#39407 = CARTESIAN_POINT ( 'NONE',  ( 10.81189881249999551, -6.242252689847874514, -12.15625000204836859 ) ) ;
#39408 = CARTESIAN_POINT ( 'NONE',  ( 9.999999999999998224, 0.000000000000000000, -40.99999999999997868 ) ) ;
#39410 = EDGE_CURVE ( 'NONE', #4655, #18018, #8754, .T. ) ;
#39409 = CARTESIAN_POINT ( 'NONE',  ( -10.00000000000012434, 5.773502691896184480, -164.8749999999999716 ) ) ;
#39411 = FACE_OUTER_BOUND ( 'NONE', #39387, .T. ) ;
#39412 = CARTESIAN_POINT ( 'NONE',  ( -6.652853726956784897, 8.522716305231336165, -100.0000000000000142 ) ) ;
#39413 = ADVANCED_FACE ( 'NONE', ( #16782 ), #17000, .F. ) ;
#39414 = CARTESIAN_POINT ( 'NONE',  ( 9.999999999999996447, -5.773502691896262640, -168.6250000000000000 ) ) ;
#39415 = DIRECTION ( 'NONE',  ( -0.000000000000000000, -0.000000000000000000, 1.000000000000000000 ) ) ;
#39416 = EDGE_CURVE ( 'NONE', #28218, #20460, #18954, .T. ) ;
#39418 = ORIENTED_EDGE ( 'NONE', *, *, #32437, .F. ) ;
#39417 = CARTESIAN_POINT ( 'NONE',  ( -10.81189881249999907, -6.242252689847864744, -96.65625000204839523 ) ) ;
#39419 = CARTESIAN_POINT ( 'NONE',  ( -11.54700538379250396, -20.00000000000000355, 49.99999999999998579 ) ) ;
#39421 = ORIENTED_EDGE ( 'NONE', *, *, #4231, .T. ) ;
#39420 = CARTESIAN_POINT ( 'NONE',  ( 5.405949406249992428, -9.363379034771808662, -102.0937500020483810 ) ) ;
#39422 = ORIENTED_EDGE ( 'NONE', *, *, #10150, .T. ) ;
#39423 = AXIS2_PLACEMENT_3D ( 'NONE', #25227, #22608, #28677 ) ;
#39424 = CARTESIAN_POINT ( 'NONE',  ( 5.405949406249999534, 9.363379034771803333, -31.09375000204836326 ) ) ;
#39425 = CARTESIAN_POINT ( 'NONE',  ( -5.405949406250003975, -9.363379034771801557, -20.03125000204836326 ) ) ;
#39426 = DATE_AND_TIME ( #171, #23898 ) ;
#39427 = CARTESIAN_POINT ( 'NONE',  ( -5.405949406249996869, 9.363379034771805109, -71.34375000204836681 ) ) ;
#39428 = CARTESIAN_POINT ( 'NONE',  ( -9.999999999998969713, -5.773502691896847949, -84.00000000409676204 ) ) ;
#39429 = CARTESIAN_POINT ( 'NONE',  ( -5.405949406250003975, -9.363379034771801557, -192.3437500020484094 ) ) ;
#39430 = EDGE_CURVE ( 'NONE', #5733, #41070, #23713, .T. ) ;
#39431 = CARTESIAN_POINT ( 'NONE',  ( 9.999999999999998224, 1.224646799147353059E-15, -99.99999999999998579 ) ) ;
#39432 = CARTESIAN_POINT ( 'NONE',  ( 7.071067811865472841, 7.071067811865472841, -200.0000000000000000 ) ) ;
#39433 = CARTESIAN_POINT ( 'NONE',  ( 10.81189881249999551, -6.242252689847874514, -156.1562500020484094 ) ) ;
#39434 = CARTESIAN_POINT ( 'NONE',  ( 10.00000000000000000, 5.773502691896255534, -2.250000004096754491 ) ) ;
#39435 = CARTESIAN_POINT ( 'NONE',  ( 7.070501591499376803E-16, 11.54700538379251284, -50.00000000409675494 ) ) ;
#39436 = CARTESIAN_POINT ( 'NONE',  ( -5.405949406249996869, 9.363379034771805109, -122.3437500020483952 ) ) ;
#39437 = CARTESIAN_POINT ( 'NONE',  ( -10.81189881249999729, 1.324075727343319199E-15, -99.78125000204839523 ) ) ;
#39438 = CARTESIAN_POINT ( 'NONE',  ( -5.405949406249996869, 9.363379034771805109, -111.8437500020483810 ) ) ;
#39439 = CARTESIAN_POINT ( 'NONE',  ( -10.81189881249999729, 1.324075727343319199E-15, -78.59375000204838102 ) ) ;
#39440 = CARTESIAN_POINT ( 'NONE',  ( 5.405949406249999534, 9.363379034771803333, -88.28125000204838102 ) ) ;
#39441 = CARTESIAN_POINT ( 'NONE',  ( -10.00000000000000000, -5.773502691896251982, -159.0000000040967905 ) ) ;
#39442 = DIRECTION ( 'NONE',  ( -0.000000000000000000, -0.000000000000000000, 1.000000000000000000 ) ) ;
#39443 = CARTESIAN_POINT ( 'NONE',  ( 10.81189881249999551, -6.242252689847874514, -168.1562500020484094 ) ) ;
#39444 = CARTESIAN_POINT ( 'NONE',  ( 5.405949406249999534, 9.363379034771803333, -181.2812500020483810 ) ) ;
#39445 = CARTESIAN_POINT ( 'NONE',  ( 10.00000000000000000, 5.773502691896255534, -158.2500000040967905 ) ) ;
#39446 = CARTESIAN_POINT ( 'NONE',  ( 4.999999999999992006, -8.660254037844389075, -156.7500000000000000 ) ) ;
#39447 = CARTESIAN_POINT ( 'NONE',  ( 10.81189881249999551, -6.242252689847874514, -4.468750002048355263 ) ) ;
#39448 = CYLINDRICAL_SURFACE ( 'NONE', #15072, 9.999999999999998224 ) ;
#39449 = CARTESIAN_POINT ( 'NONE',  ( 7.644554776091147741E-16, 12.48450537969573659, -111.9687500020483952 ) ) ;
#39450 = CARTESIAN_POINT ( 'NONE',  ( -10.00000000000000000, -5.773502691896251982, -85.12499999999997158 ) ) ;
#39451 = CARTESIAN_POINT ( 'NONE',  ( -10.81189881249999729, 6.242252689847871849, -11.40625000204836859 ) ) ;
#39452 = CARTESIAN_POINT ( 'NONE',  ( -9.999999999999998224, 5.773502691896259087, -96.25000000409677625 ) ) ;
#39453 = FACE_OUTER_BOUND ( 'NONE', #23987, .T. ) ;
#39454 = CARTESIAN_POINT ( 'NONE',  ( 7.644554776091147741E-16, 12.48450537969573659, -107.6562500020483810 ) ) ;
#39455 = CARTESIAN_POINT ( 'NONE',  ( 5.405949406249992428, -9.363379034771808662, -94.78125000204838102 ) ) ;
#39456 = ORIENTED_EDGE ( 'NONE', *, *, #42575, .F. ) ;
#39457 = AXIS2_PLACEMENT_3D ( 'NONE', #2740, #29274, #12848 ) ;
#39458 = CARTESIAN_POINT ( 'NONE',  ( 10.00000000000000000, 5.773502691896255534, -87.75000000409677625 ) ) ;
#39459 = PLANE ( 'NONE',  #37377 ) ;
#39460 = CARTESIAN_POINT ( 'NONE',  ( -10.81189881249999907, -6.242252689847864744, -40.96875000204835260 ) ) ;
#39461 = ORIENTED_EDGE ( 'NONE', *, *, #836, .F. ) ;
#39462 = CARTESIAN_POINT ( 'NONE',  ( -4.999999999999996447, 8.660254037844387298, -8.999999999999952038 ) ) ;
#39463 = CARTESIAN_POINT ( 'NONE',  ( 5.000000000000000000, 8.660254037844385522, -144.2500000000000000 ) ) ;
#39464 =( BOUNDED_CURVE ( )  B_SPLINE_CURVE ( 2, ( #27490, #957, #4396, #30736, #17535, #23408, #7207 ),
 .UNSPECIFIED., .F., .F. ) 
 B_SPLINE_CURVE_WITH_KNOTS ( ( 3, 2, 2, 3 ),
 ( 0.9365671641791047941, 0.9378109452736321794, 0.9390547263681594536, 0.9402985074626868389 ),
 .UNSPECIFIED. ) 
 CURVE ( )  GEOMETRIC_REPRESENTATION_ITEM ( )  RATIONAL_B_SPLINE_CURVE ( ( 0.9999999999999641398, 0.8660254037844745678, 1.000000000000000000, 0.8660254037844387076, 1.000000000000000000, 0.8660254037844148378, 1.000000000000023981 ) ) 
 REPRESENTATION_ITEM ( '' )  );
#39465 = CARTESIAN_POINT ( 'NONE',  ( -10.00000000000000000, -5.773502691896251982, -9.000000004096758488 ) ) ;
#39466 = CARTESIAN_POINT ( 'NONE',  ( -5.000000000000003553, -8.660254037844383745, -194.5000000000000000 ) ) ;
#39468 = ORIENTED_EDGE ( 'NONE', *, *, #39278, .F. ) ;
#39467 = CARTESIAN_POINT ( 'NONE',  ( -2.293366432827344421E-15, -12.48450537969573659, -121.9062500020483952 ) ) ;
#39469 = DIRECTION ( 'NONE',  ( -0.000000000000000000, -0.000000000000000000, -1.000000000000000000 ) ) ;
#39470 = ORIENTED_EDGE ( 'NONE', *, *, #9783, .T. ) ;
#39471 = CARTESIAN_POINT ( 'NONE',  ( 5.405949406249999534, 9.363379034771803333, -44.78125000204838102 ) ) ;
#39472 = APPLICATION_PROTOCOL_DEFINITION ( 'international standard', 'config_control_design', 1994, #3865 ) ;
#39473 = EDGE_CURVE ( 'NONE', #8961, #20303, #17540, .T. ) ;
#39474 = CARTESIAN_POINT ( 'NONE',  ( -10.81189881249999907, -6.242252689847864744, -100.9687500020483810 ) ) ;
#39475 = CARTESIAN_POINT ( 'NONE',  ( 10.81189881249999729, 6.242252689847867408, -127.4062500020483810 ) ) ;
#39476 = ORIENTED_EDGE ( 'NONE', *, *, #41442, .T. ) ;
#39477 = CARTESIAN_POINT ( 'NONE',  ( -8.675003188131697129, -4.974413003141672895, -0.0003472602639886801512 ) ) ;
#39478 = CARTESIAN_POINT ( 'NONE',  ( -5.321294541346989426, 5.321294541346989426, -219.9999999999999716 ) ) ;
#39479 = CARTESIAN_POINT ( 'NONE',  ( -5.405949406250003975, -9.363379034771801557, -180.5312500020483810 ) ) ;
#39480 = CARTESIAN_POINT ( 'NONE',  ( 10.81189881249999907, 6.242252689847868297, 0.2812499979516534521 ) ) ;
#39481 = CYLINDRICAL_SURFACE ( 'NONE', #7319, 35.00000000000000711 ) ;
#39482 = CARTESIAN_POINT ( 'NONE',  ( 5.405949406249999534, 9.363379034771803333, -130.0937500020483810 ) ) ;
#39483 = CARTESIAN_POINT ( 'NONE',  ( 10.81189881249999729, 0.000000000000000000, -101.8437500020483810 ) ) ;
#39484 = CARTESIAN_POINT ( 'NONE',  ( 5.000000000000000000, 8.660254037844385522, -116.1250000040967905 ) ) ;
#39485 = CARTESIAN_POINT ( 'NONE',  ( 5.405949406249992428, -9.363379034771808662, -105.2812500020483810 ) ) ;
#39486 = CARTESIAN_POINT ( 'NONE',  ( -10.00000000000000000, -5.773502691896251982, -184.5000000040968189 ) ) ;
#39487 = CARTESIAN_POINT ( 'NONE',  ( 10.81189881249999729, 6.242252689847867408, -115.2187500020483810 ) ) ;
#39488 = CARTESIAN_POINT ( 'NONE',  ( 5.405949406249992428, -9.363379034771808662, -187.7812500020484094 ) ) ;
#39489 = CARTESIAN_POINT ( 'NONE',  ( 9.999999999999998224, 0.000000000000000000, -94.99999999999998579 ) ) ;
#39490 = CARTESIAN_POINT ( 'NONE',  ( 0.000000000000000000, 0.000000000000000000, -200.0000000000000000 ) ) ;
#39491 = CARTESIAN_POINT ( 'NONE',  ( -10.00000000000000000, -5.773502691896251982, -139.1250000000000000 ) ) ;
#39492 = CARTESIAN_POINT ( 'NONE',  ( 10.00000000000000000, 5.773502691896255534, -1.874999999999960254 ) ) ;
#39493 = CARTESIAN_POINT ( 'NONE',  ( 10.81189881249999551, -6.242252689847874514, -59.96875000204837391 ) ) ;
#39494 = CARTESIAN_POINT ( 'NONE',  ( -2.293366432827344421E-15, -12.48450537969573659, -48.21875000204836681 ) ) ;
#39495 = CARTESIAN_POINT ( 'NONE',  ( 9.999999999999998224, 0.000000000000000000, -180.8750000040967905 ) ) ;
#39496 = CARTESIAN_POINT ( 'NONE',  ( -10.81189881249999729, 1.324075727343319199E-15, -15.78125000204835793 ) ) ;
#39497 = CARTESIAN_POINT ( 'NONE',  ( 10.81189881249999729, 0.000000000000000000, -28.34375000204836326 ) ) ;
#39498 = DIRECTION ( 'NONE',  ( 0.5000000000000002220, -0.8660254037844384856, 0.000000000000000000 ) ) ;
#39499 = CARTESIAN_POINT ( 'NONE',  ( 5.405949406249999534, 9.363379034771803333, -139.0937500020483810 ) ) ;
#39500 = CARTESIAN_POINT ( 'NONE',  ( 9.999999999999998224, 0.000000000000000000, -106.9999999999999858 ) ) ;
#39501 = CARTESIAN_POINT ( 'NONE',  ( -5.405949406249996869, 9.363379034771805109, -34.03125000204837391 ) ) ;
#39502 = LINE ( 'NONE', #30017, #14127 ) ;
#39503 = CARTESIAN_POINT ( 'NONE',  ( 4.999999999999992006, -8.660254037844389075, -71.24999999999998579 ) ) ;
#39504 = CARTESIAN_POINT ( 'NONE',  ( 10.81189881249999551, -6.242252689847874514, -130.6562500020484094 ) ) ;
#39505 = CARTESIAN_POINT ( 'NONE',  ( -10.81189881249999729, -6.242252689847864744, -116.1562500020483952 ) ) ;
#39506 = ORIENTED_EDGE ( 'NONE', *, *, #2632, .F. ) ;
#39507 =( BOUNDED_CURVE ( )  B_SPLINE_CURVE ( 2, ( #37687, #37905, #8129, #40470, #8349, #21500, #24111 ),
 .UNSPECIFIED., .F., .F. ) 
 B_SPLINE_CURVE_WITH_KNOTS ( ( 3, 2, 2, 3 ),
 ( 0.03358208955223884046, 0.03482587064676620492, 0.03606965174129356938, 0.03731343283582092690 ),
 .UNSPECIFIED. ) 
 CURVE ( )  GEOMETRIC_REPRESENTATION_ITEM ( )  RATIONAL_B_SPLINE_CURVE ( ( 0.9999999999999963363, 0.8660254037844424824, 1.000000000000000000, 0.8660254037844387076, 1.000000000000000000, 0.8660254037844349329, 1.000000000000003775 ) ) 
 REPRESENTATION_ITEM ( '' )  );
#39508 = CARTESIAN_POINT ( 'NONE',  ( -9.999999999999479527, -5.773502691896549521, -7.124999999999955591 ) ) ;
#39509 = CARTESIAN_POINT ( 'NONE',  ( 7.070501591499377789E-16, 11.54700538379251284, -110.0000000040968047 ) ) ;
#39510 = CARTESIAN_POINT ( 'NONE',  ( 7.070501591499376803E-16, 11.54700538379251284, -162.1250000000000284 ) ) ;
#39511 = CARTESIAN_POINT ( 'NONE',  ( -10.81189881249999907, -6.242252689847864744, -69.46875000204838102 ) ) ;
#39512 = ORIENTED_EDGE ( 'NONE', *, *, #25059, .F. ) ;
#39513 = CARTESIAN_POINT ( 'NONE',  ( -10.00000000000000000, -5.773502691896251982, -29.62499999999995026 ) ) ;
#39514 = CARTESIAN_POINT ( 'NONE',  ( 9.999999999999998224, 0.000000000000000000, -20.37500000409675494 ) ) ;
#39515 = CARTESIAN_POINT ( 'NONE',  ( 10.81189881249999551, -6.242252689847874514, -43.65625000204838102 ) ) ;
#39516 = CARTESIAN_POINT ( 'NONE',  ( -5.000000000000003553, -8.660254037844383745, -2.499999999999974243 ) ) ;
#39517 = CARTESIAN_POINT ( 'NONE',  ( 7.070501591499377789E-16, 11.54700538379251284, -38.00000000409675494 ) ) ;
#39518 =( BOUNDED_CURVE ( )  B_SPLINE_CURVE ( 2, ( #19676, #23574, #30264, #16638, #40162, #6950, #3081 ),
 .UNSPECIFIED., .F., .F. ) 
 B_SPLINE_CURVE_WITH_KNOTS ( ( 3, 2, 2, 3 ),
 ( 0.6567164179104479915, 0.6579601990049753768, 0.6592039800995028731, 0.6604477611940301474 ),
 .UNSPECIFIED. ) 
 CURVE ( )  GEOMETRIC_REPRESENTATION_ITEM ( )  RATIONAL_B_SPLINE_CURVE ( ( 0.9999999999999761302, 0.8660254037844625774, 1.000000000000000000, 0.8660254037844387076, 1.000000000000000000, 0.8660254037844028474, 1.000000000000035971 ) ) 
 REPRESENTATION_ITEM ( '' )  );
#39519 = DIRECTION ( 'NONE',  ( -0.000000000000000000, -0.000000000000000000, 1.000000000000000000 ) ) ;
#39520 = CARTESIAN_POINT ( 'NONE',  ( 10.81189881249999907, 6.242252689847868297, -140.9062500020484094 ) ) ;
#39521 = CARTESIAN_POINT ( 'NONE',  ( -10.81189881249999729, 6.242252689847871849, -138.9062500020484094 ) ) ;
#39522 = ORIENTED_EDGE ( 'NONE', *, *, #34438, .F. ) ;
#39523 = EDGE_CURVE ( 'NONE', #19597, #32882, #20671, .T. ) ;
#39524 = VERTEX_POINT ( 'NONE', #27374 ) ;
#39525 = EDGE_LOOP ( 'NONE', ( #30305, #646, #29231, #37727 ) ) ;
#39526 = DIRECTION ( 'NONE',  ( -0.000000000000000000, -0.000000000000000000, 1.000000000000000000 ) ) ;
#39527 = CARTESIAN_POINT ( 'NONE',  ( -10.81189881249999729, 6.242252689847871849, -177.7187500020483810 ) ) ;
#39528 = CARTESIAN_POINT ( 'NONE',  ( 10.81189881249999551, -6.242252689847874514, -25.46875000204837391 ) ) ;
#39529 = CARTESIAN_POINT ( 'NONE',  ( 0.000000000000000000, 0.000000000000000000, -200.0000000000000000 ) ) ;
#39530 = CARTESIAN_POINT ( 'NONE',  ( -10.81189881249999729, -6.242252689847864744, -153.4687500020484094 ) ) ;
#39531 = CARTESIAN_POINT ( 'NONE',  ( 5.405949406249992428, -9.363379034771808662, -144.0937500020483810 ) ) ;
#39532 = ADVANCED_FACE ( 'NONE', ( #38364 ), #34288, .T. ) ;
#39533 = CARTESIAN_POINT ( 'NONE',  ( -5.000000000000003553, -8.660254037844383745, -9.999999999999953815 ) ) ;
#39534 = CARTESIAN_POINT ( 'NONE',  ( -10.81189881249999729, 6.242252689847871849, -126.7187500020483952 ) ) ;
#39535 = CARTESIAN_POINT ( 'NONE',  ( -2.293366432827344421E-15, -12.48450537969573659, -133.9062500020483810 ) ) ;
#39536 = CARTESIAN_POINT ( 'NONE',  ( 10.81189881249999907, 6.242252689847868297, -17.71875000204836681 ) ) ;
#39537 = CARTESIAN_POINT ( 'NONE',  ( -10.81189881249999729, -6.242252689847864744, -139.9687500020483810 ) ) ;
#39538 = CARTESIAN_POINT ( 'NONE',  ( -5.000000000000003553, -8.660254037844383745, -125.8750000040967905 ) ) ;
#39539 = CARTESIAN_POINT ( 'NONE',  ( 80.00000000000002842, 19.99999999999999289, -170.0000000000000000 ) ) ;
#39540 = CARTESIAN_POINT ( 'NONE',  ( 10.00000000000000000, 5.773502691896255534, -160.8750000000000000 ) ) ;
#39541 = CARTESIAN_POINT ( 'NONE',  ( -5.405949406250003975, -9.363379034771801557, -76.84375000204838102 ) ) ;
#39542 = CARTESIAN_POINT ( 'NONE',  ( -10.81189881249999729, 6.242252689847871849, -45.90625000204836681 ) ) ;
#39543 = CARTESIAN_POINT ( 'NONE',  ( -10.81189881249999907, -6.242252689847864744, -57.46875000204836681 ) ) ;
#39544 = CARTESIAN_POINT ( 'NONE',  ( 4.999999999999992006, -8.660254037844389075, -174.7500000000000284 ) ) ;
#39545 = CARTESIAN_POINT ( 'NONE',  ( -5.405949406249996869, 9.363379034771805109, -165.8437500020484094 ) ) ;
#39546 = CARTESIAN_POINT ( 'NONE',  ( 9.999999999999996447, -5.773502691896262640, -131.1250000000000000 ) ) ;
#39547 = CARTESIAN_POINT ( 'NONE',  ( -10.81189881249999729, 6.242252689847871849, -141.9062500020484094 ) ) ;
#39548 = CYLINDRICAL_SURFACE ( 'NONE', #27943, 9.999999999999998224 ) ;
#39549 = CARTESIAN_POINT ( 'NONE',  ( 5.000000000000000000, 8.660254037844385522, -116.1250000040967905 ) ) ;
#39550 = CARTESIAN_POINT ( 'NONE',  ( -2.121150477449813534E-15, -11.54700538379251284, -95.37500000000000000 ) ) ;
#39551 = EDGE_LOOP ( 'NONE', ( #22436, #29191, #5307, #26979 ) ) ;
#39552 = CARTESIAN_POINT ( 'NONE',  ( -10.81189881249999729, -6.242252689847864744, -113.1562500020483952 ) ) ;
#39553 = CARTESIAN_POINT ( 'NONE',  ( -4.999999999999996447, 8.660254037844387298, -129.3750000040967905 ) ) ;
#39554 = LINE ( 'NONE', #16873, #33275 ) ;
#39555 = CARTESIAN_POINT ( 'NONE',  ( -5.405949406249996869, 9.363379034771805109, -161.5312500020484094 ) ) ;
#39556 = CARTESIAN_POINT ( 'NONE',  ( -4.999999999999996447, 8.660254037844387298, -40.87500000409677625 ) ) ;
#39557 = DIRECTION ( 'NONE',  ( 1.000000000000000000, 0.000000000000000000, 0.000000000000000000 ) ) ;
#39558 = CARTESIAN_POINT ( 'NONE',  ( 5.405949406249999534, 9.363379034771803333, -56.78125000204836681 ) ) ;
#39559 = DIRECTION ( 'NONE',  ( 0.8660254037844439257, 0.000000000000000000, 0.4999999999999907296 ) ) ;
#39560 = CARTESIAN_POINT ( 'NONE',  ( -5.405949406250003975, -9.363379034771801557, -162.5312500020484094 ) ) ;
#39561 = CARTESIAN_POINT ( 'NONE',  ( 10.81189881249999551, -6.242252689847874514, -133.4687500020483810 ) ) ;
#39562 = DIRECTION ( 'NONE',  ( -0.000000000000000000, -0.000000000000000000, 1.000000000000000000 ) ) ;
#39563 = CARTESIAN_POINT ( 'NONE',  ( 10.00000000000012790, 5.773502691896179151, -171.7500000040967620 ) ) ;
#39564 = ORIENTED_EDGE ( 'NONE', *, *, #2242, .T. ) ;
#39565 = CARTESIAN_POINT ( 'NONE',  ( 9.999999999999479527, 5.773502691896553074, -114.7500000040967620 ) ) ;
#39567 = ORIENTED_EDGE ( 'NONE', *, *, #24757, .T. ) ;
#39566 = CARTESIAN_POINT ( 'NONE',  ( 5.405949406249992428, -9.363379034771808662, -67.78125000204838102 ) ) ;
#39568 = COORDINATED_UNIVERSAL_TIME_OFFSET ( 6, 0, .AHEAD. ) ;
#39570 = VERTEX_POINT ( 'NONE', #31049 ) ;
#39569 = CARTESIAN_POINT ( 'NONE',  ( 10.81189881249999907, 6.242252689847868297, -122.7187500020483810 ) ) ;
#39571 = ORIENTED_EDGE ( 'NONE', *, *, #39107, .F. ) ;
#39572 = CARTESIAN_POINT ( 'NONE',  ( -10.81189881249999729, -6.242252689847864744, -19.96875000204837747 ) ) ;
#39573 = CARTESIAN_POINT ( 'NONE',  ( 7.644554776091147741E-16, 12.48450537969573659, -197.4687500020484094 ) ) ;
#39574 = CARTESIAN_POINT ( 'NONE',  ( 10.81189881249999551, -6.242252689847874514, -47.96875000204836681 ) ) ;
#39575 = CARTESIAN_POINT ( 'NONE',  ( -2.121150477449813534E-15, -11.54700538379251284, -71.75000000409676204 ) ) ;
#39576 = CARTESIAN_POINT ( 'NONE',  ( -9.999999999999998224, 1.224646799147353059E-15, -25.24999999999996803 ) ) ;
#39577 = CARTESIAN_POINT ( 'NONE',  ( 7.644554776091147741E-16, 12.48450537969573659, -179.4687500020484094 ) ) ;
#39578 = CARTESIAN_POINT ( 'NONE',  ( -5.405949406250003975, -9.363379034771801557, -168.3437500020484094 ) ) ;
#39579 = CARTESIAN_POINT ( 'NONE',  ( 10.81189881249999907, 6.242252689847868297, -151.2187500020483810 ) ) ;
#39580 = CARTESIAN_POINT ( 'NONE',  ( 10.81189881249999551, -6.242252689847874514, -163.4687500020483810 ) ) ;
#39581 = CARTESIAN_POINT ( 'NONE',  ( -9.999999999999998224, 1.224646799147353059E-15, -123.1250000040967905 ) ) ;
#39582 = CARTESIAN_POINT ( 'NONE',  ( -9.999999999999998224, 1.224646799147353059E-15, -193.2500000000000000 ) ) ;
#39583 = CARTESIAN_POINT ( 'NONE',  ( 4.999999999999992006, -8.660254037844389075, -189.7500000000000000 ) ) ;
#39584 = CARTESIAN_POINT ( 'NONE',  ( -5.405949406250003975, -9.363379034771801557, -97.84375000204838102 ) ) ;
#39585 = CARTESIAN_POINT ( 'NONE',  ( 9.999999999999479527, 5.773502691896553074, -34.87499999999994316 ) ) ;
#39586 = CARTESIAN_POINT ( 'NONE',  ( -2.293366432827344421E-15, -12.48450537969573659, -63.40625000204838102 ) ) ;
#39587 = EDGE_CURVE ( 'NONE', #8170, #12734, #21985, .T. ) ;
#39588 = CARTESIAN_POINT ( 'NONE',  ( 5.405949406249992428, -9.363379034771808662, -187.5937500020483810 ) ) ;
#39589 = CARTESIAN_POINT ( 'NONE',  ( -10.81189881249999907, -6.242252689847864744, -122.1562500020484094 ) ) ;
#39590 = CARTESIAN_POINT ( 'NONE',  ( -5.405949406249996869, 9.363379034771805109, -164.5312500020484094 ) ) ;
#39591 = EDGE_CURVE ( 'NONE', #6518, #25484, #3840, .T. ) ;
#39592 = CARTESIAN_POINT ( 'NONE',  ( 7.644554776091147741E-16, 12.48450537969573659, -49.15625000204837391 ) ) ;
#39593 = CARTESIAN_POINT ( 'NONE',  ( 5.000000000000000000, 8.660254037844385522, -135.6250000040967620 ) ) ;
#39594 = CARTESIAN_POINT ( 'NONE',  ( -5.000000000000003553, -8.660254037844383745, -116.4999999999999858 ) ) ;
#39595 = ORIENTED_EDGE ( 'NONE', *, *, #10920, .T. ) ;
#39596 = CARTESIAN_POINT ( 'NONE',  ( 10.81189881249999551, -6.242252689847874514, -133.6562500020483810 ) ) ;
#39597 = CARTESIAN_POINT ( 'NONE',  ( 10.81189881249999729, 0.000000000000000000, -145.5312500020483810 ) ) ;
#39598 = CARTESIAN_POINT ( 'NONE',  ( -2.293366432827344421E-15, -12.48450537969573659, -195.4062500020484094 ) ) ;
#39599 = DIRECTION ( 'NONE',  ( -0.000000000000000000, -0.000000000000000000, -1.000000000000000000 ) ) ;
#39600 = CARTESIAN_POINT ( 'NONE',  ( -2.293366432827344421E-15, -12.48450537969573659, -78.21875000204838102 ) ) ;
#39601 = ORIENTED_EDGE ( 'NONE', *, *, #17172, .F. ) ;
#39602 = CARTESIAN_POINT ( 'NONE',  ( 4.999999999999992006, -8.660254037844389075, -54.74999999999996447 ) ) ;
#39603 = CARTESIAN_POINT ( 'NONE',  ( 5.405949406249992428, -9.363379034771808662, -186.0937500020483810 ) ) ;
#39604 = CARTESIAN_POINT ( 'NONE',  ( -9.999999999999998224, 5.773502691896259087, -63.25000000409679757 ) ) ;
#39605 = FACE_OUTER_BOUND ( 'NONE', #5920, .T. ) ;
#39606 = CARTESIAN_POINT ( 'NONE',  ( 7.070501591499376803E-16, 11.54700538379251284, -140.0000000040967905 ) ) ;
#39607 = CARTESIAN_POINT ( 'NONE',  ( 5.405949406249999534, 9.363379034771803333, -83.78125000204838102 ) ) ;
#39608 = CARTESIAN_POINT ( 'NONE',  ( -2.293366432827344421E-15, -12.48450537969573659, -57.40625000204838102 ) ) ;
#39609 = CARTESIAN_POINT ( 'NONE',  ( 7.070501591499377789E-16, 11.54700538379251284, -59.00000000409677625 ) ) ;
#39610 = CARTESIAN_POINT ( 'NONE',  ( -10.81189881249999729, 1.324075727343319199E-15, -15.59375000204835082 ) ) ;
#39611 = CARTESIAN_POINT ( 'NONE',  ( 4.999999999999992006, -8.660254037844389075, -151.1250000040967905 ) ) ;
#39612 = CARTESIAN_POINT ( 'NONE',  ( 10.81189881249999729, 0.000000000000000000, -183.0312500020484094 ) ) ;
#39613 = CARTESIAN_POINT ( 'NONE',  ( -5.405949406249996869, 9.363379034771805109, -11.53125000204835438 ) ) ;
#39614 = CARTESIAN_POINT ( 'NONE',  ( -5.000000000000003553, -8.660254037844383745, -148.3750000040967905 ) ) ;
#39615 = LINE ( 'NONE', #36597, #24972 ) ;
#39616 = CARTESIAN_POINT ( 'NONE',  ( 0.000000000000000000, 0.000000000000000000, -200.0000000000000000 ) ) ;
#39617 =( BOUNDED_CURVE ( )  B_SPLINE_CURVE ( 2, ( #26202, #30299, #16885, #6985, #10418, #3960, #19500 ),
 .UNSPECIFIED., .F., .F. ) 
 B_SPLINE_CURVE_WITH_KNOTS ( ( 3, 2, 2, 3 ),
 ( 0.4141791044776120256, 0.4154228855721394109, 0.4166666666666667962, 0.4179104477611941260 ),
 .UNSPECIFIED. ) 
 CURVE ( )  GEOMETRIC_REPRESENTATION_ITEM ( )  RATIONAL_B_SPLINE_CURVE ( ( 0.9999999999999880096, 0.8660254037844506980, 1.000000000000000000, 0.8660254037844387076, 1.000000000000000000, 0.8660254037844267172, 1.000000000000011990 ) ) 
 REPRESENTATION_ITEM ( '' )  );
#39618 = CARTESIAN_POINT ( 'NONE',  ( 9.999999999999996447, -5.773502691896262640, -170.1250000000000000 ) ) ;
#39619 = DIRECTION ( 'NONE',  ( -0.000000000000000000, -0.000000000000000000, -1.000000000000000000 ) ) ;
#39621 = VERTEX_POINT ( 'NONE', #31694 ) ;
#39620 = CARTESIAN_POINT ( 'NONE',  ( 5.405949406249999534, 9.363379034771803333, -95.78125000204838102 ) ) ;
#39623 = ORIENTED_EDGE ( 'NONE', *, *, #28102, .F. ) ;
#39622 = CARTESIAN_POINT ( 'NONE',  ( -10.00000000000025580, 5.773502691896109873, -161.8749999999999716 ) ) ;
#39624 = EDGE_LOOP ( 'NONE', ( #42275, #24900, #12551, #9583 ) ) ;
#39625 = CARTESIAN_POINT ( 'NONE',  ( -2.293366432827344421E-15, -12.48450537969573659, -34.71875000204835260 ) ) ;
#39626 = CARTESIAN_POINT ( 'NONE',  ( -10.81189881249999729, 1.324075727343319199E-15, -21.78125000204836326 ) ) ;
#39627 = PERSON_AND_ORGANIZATION ( #8875, #10786 ) ;
#39628 = CARTESIAN_POINT ( 'NONE',  ( 7.644554776091147741E-16, 12.48450537969573659, -71.46875000204838102 ) ) ;
#39629 = CARTESIAN_POINT ( 'NONE',  ( -9.999999999999998224, 1.224646799147353059E-15, -165.1250000040967905 ) ) ;
#39630 = CARTESIAN_POINT ( 'NONE',  ( -10.81189881249999729, 1.324075727343319199E-15, -197.0937500020484094 ) ) ;
#39631 = CARTESIAN_POINT ( 'NONE',  ( -5.405949406250003975, -9.363379034771801557, -153.3437500020483810 ) ) ;
#39632 = DIRECTION ( 'NONE',  ( -0.000000000000000000, -0.000000000000000000, 1.000000000000000000 ) ) ;
#39633 = CARTESIAN_POINT ( 'NONE',  ( 9.999999999999998224, 0.000000000000000000, -112.9999999999999858 ) ) ;
#39634 = CARTESIAN_POINT ( 'NONE',  ( 5.405949406249999534, 9.363379034771803333, -151.2812500020484094 ) ) ;
#39635 = CARTESIAN_POINT ( 'NONE',  ( 9.999999999999998224, 0.000000000000000000, 0.6249999959032359609 ) ) ;
#39636 = CARTESIAN_POINT ( 'NONE',  ( -9.999999999999998224, 1.224646799147353059E-15, -143.7500000000000000 ) ) ;
#39637 = CARTESIAN_POINT ( 'NONE',  ( -2.293366432827344421E-15, -12.48450537969573659, -120.2187500020483952 ) ) ;
#39638 = ADVANCED_FACE ( 'NONE', ( #27805 ), #5518, .T. ) ;
#39639 = CARTESIAN_POINT ( 'NONE',  ( -10.81189881249999907, -6.242252689847864744, -87.65625000204836681 ) ) ;
#39640 = ADVANCED_FACE ( 'NONE', ( #14616 ), #40936, .T. ) ;
#39641 = CARTESIAN_POINT ( 'NONE',  ( -5.405949406249996869, 9.363379034771805109, -110.3437500020483810 ) ) ;
#39642 = CARTESIAN_POINT ( 'NONE',  ( -10.81189881249999729, 1.324075727343319199E-15, -74.09375000204838102 ) ) ;
#39643 = CARTESIAN_POINT ( 'NONE',  ( -10.81189881249999729, 6.242252689847871849, -83.40625000204836681 ) ) ;
#39644 = CARTESIAN_POINT ( 'NONE',  ( -9.999999999999998224, 5.773502691896259087, -163.7500000040967905 ) ) ;
#39645 = EDGE_CURVE ( 'NONE', #39928, #40993, #8260, .T. ) ;
#39646 = FACE_OUTER_BOUND ( 'NONE', #55, .T. ) ;
#39647 = CARTESIAN_POINT ( 'NONE',  ( -10.81189881249999729, -6.242252689847864744, -167.1562500020484094 ) ) ;
#39648 = CARTESIAN_POINT ( 'NONE',  ( 10.81189881249999729, 0.000000000000000000, -180.0312500020483810 ) ) ;
#39649 = CARTESIAN_POINT ( 'NONE',  ( -5.000000000000003553, -8.660254037844383745, -157.3750000040967905 ) ) ;
#39650 = CYLINDRICAL_SURFACE ( 'NONE', #25650, 9.999999999999998224 ) ;
#39651 = CARTESIAN_POINT ( 'NONE',  ( 7.644554776091147741E-16, 12.48450537969573659, -3.968750002048354819 ) ) ;
#39652 = CARTESIAN_POINT ( 'NONE',  ( 0.000000000000000000, 0.000000000000000000, -200.0000000000000000 ) ) ;
#39653 = CARTESIAN_POINT ( 'NONE',  ( -2.293366432827344421E-15, -12.48450537969573659, -117.2187500020483952 ) ) ;
#39654 = CARTESIAN_POINT ( 'NONE',  ( 10.00000000000000000, 5.773502691896255534, -84.37499999999998579 ) ) ;
#39655 = CARTESIAN_POINT ( 'NONE',  ( -10.81189881249999729, 1.324075727343319199E-15, -11.28125000204835438 ) ) ;
#39656 = CARTESIAN_POINT ( 'NONE',  ( 9.999999999999998224, 0.000000000000000000, -87.87500000409677625 ) ) ;
#39657 = VECTOR ( 'NONE', #10630, 1000.000000000000114 ) ;
#39658 = DIRECTION ( 'NONE',  ( -0.000000000000000000, -0.000000000000000000, 1.000000000000000000 ) ) ;
#39659 = CC_DESIGN_PERSON_AND_ORGANIZATION_ASSIGNMENT ( #4499, #27813, ( #28392 ) ) ;
#39660 = CARTESIAN_POINT ( 'NONE',  ( -10.81189881249999729, 6.242252689847871849, -108.9062500020483810 ) ) ;
#39661 = CARTESIAN_POINT ( 'NONE',  ( 5.405949406249992428, -9.363379034771808662, -79.78125000204838102 ) ) ;
#39662 = EDGE_LOOP ( 'NONE', ( #28063, #9698, #20355, #19745, #29129, #8641, #31109, #17515, #21480, #15231, #13551, #37510, #21811, #31456, #16715, #18775, #24469, #39571, #28329, #28463, #9792, #10424, #849, #31218, #11058, #23719, #36646, #855, #38425, #2861, #2244, #8389, #19651, #7661, #41694, #15471, #26443, #30521, #14537, #32745, #12390, #38408, #28160, #15099, #4284, #29444, #556, #8688, #33750, #1864, #5514, #38631, #31358, #19039, #41856, #15616, #31313, #42593, #16565, #1040, #38417, #23085, #21644, #12654, #35556, #13379, #40255, #39211, #35081, #20335, #27434, #5082, #1860, #18132, #17961, #31327, #12441, #1619, #26325, #24471, #32783, #6208, #10372, #35039, #37438, #3997, #19862, #17201, #33331, #37179, #9799, #1375, #12322, #7313, #16094, #11703, #22692, #28760, #14502, #8600, #13338, #1373, #19231, #10958, #28239, #5063, #4604, #38897, #6939, #32511, #33755 ) ) ;
#39663 = CARTESIAN_POINT ( 'NONE',  ( -4.999999999999996447, 8.660254037844387298, -87.37500000409677625 ) ) ;
#39664 = CARTESIAN_POINT ( 'NONE',  ( 9.999999999999998224, 0.000000000000000000, -117.5000000000000000 ) ) ;
#39665 = CARTESIAN_POINT ( 'NONE',  ( 10.81189881249999551, -6.242252689847874514, -44.96875000204835970 ) ) ;
#39666 = ORIENTED_EDGE ( 'NONE', *, *, #35493, .F. ) ;
#39667 = CARTESIAN_POINT ( 'NONE',  ( 5.000000000000000000, 8.660254037844385522, -6.249999999999977796 ) ) ;
#39668 = CARTESIAN_POINT ( 'NONE',  ( 9.999999999999998224, 0.000000000000000000, -146.0000000000000000 ) ) ;
#39669 = CARTESIAN_POINT ( 'NONE',  ( 4.999999999999992006, -8.660254037844389075, -32.24999999999997158 ) ) ;
#39670 = CARTESIAN_POINT ( 'NONE',  ( 9.999999999999998224, 0.000000000000000000, -8.375000004096744277 ) ) ;
#39671 = ADVANCED_FACE ( 'NONE', ( #1480 ), #37942, .T. ) ;
#39672 = CARTESIAN_POINT ( 'NONE',  ( 4.999999999999992006, -8.660254037844389075, -186.7500000000000000 ) ) ;
#39673 = CARTESIAN_POINT ( 'NONE',  ( 9.999999999999998224, 0.000000000000000000, -200.0000000000000000 ) ) ;
#39675 = ORIENTED_EDGE ( 'NONE', *, *, #21969, .F. ) ;
#39674 = CARTESIAN_POINT ( 'NONE',  ( -10.81189881249999729, 6.242252689847871849, -119.4062500020483952 ) ) ;
#39676 = CARTESIAN_POINT ( 'NONE',  ( 24.99999999999999645, 3.061616997868382648E-15, -103.0000000000000000 ) ) ;
#39677 = VECTOR ( 'NONE', #14777, 1000.000000000000000 ) ;
#39678 = ORIENTED_EDGE ( 'NONE', *, *, #28973, .T. ) ;
#39679 = VECTOR ( 'NONE', #38362, 1000.000000000000114 ) ;
#39680 = CARTESIAN_POINT ( 'NONE',  ( 10.81189881249999907, 6.242252689847868297, -49.40625000204837391 ) ) ;
#39681 = PERSON_AND_ORGANIZATION ( #11915, #17965 ) ;
#39682 = CARTESIAN_POINT ( 'NONE',  ( 10.81189881249999729, 0.000000000000000000, -98.84375000204838102 ) ) ;
#39683 = CARTESIAN_POINT ( 'NONE',  ( -10.81189881249999729, 6.242252689847871849, -126.9062500020483810 ) ) ;
#39684 = VERTEX_POINT ( 'NONE', #8596 ) ;
#39685 = AXIS2_PLACEMENT_3D ( 'NONE', #29884, #33344, #24046 ) ;
#39686 = CARTESIAN_POINT ( 'NONE',  ( -2.121150477449813534E-15, -11.54700538379251284, -132.8750000000000000 ) ) ;
#39687 = FACE_OUTER_BOUND ( 'NONE', #3179, .T. ) ;
#39688 = CARTESIAN_POINT ( 'NONE',  ( -10.81189881249999729, 6.242252689847871849, -179.4062500020484094 ) ) ;
#39689 = PLANE ( 'NONE',  #37629 ) ;
#39690 = CARTESIAN_POINT ( 'NONE',  ( -10.81189881249999729, 6.242252689847871849, -128.2187500020483810 ) ) ;
#39691 = CARTESIAN_POINT ( 'NONE',  ( 7.644554776091147741E-16, 12.48450537969573659, -99.96875000204839523 ) ) ;
#39692 = CARTESIAN_POINT ( 'NONE',  ( -9.999999999999872102, -5.773502691896326589, -158.6250000000000284 ) ) ;
#39693 = CARTESIAN_POINT ( 'NONE',  ( -10.81189881249999729, 1.324075727343319199E-15, -110.2812500020483810 ) ) ;
#39694 = CARTESIAN_POINT ( 'NONE',  ( -5.000000000000003553, -8.660254037844383745, -187.3750000040967905 ) ) ;
#39695 = CARTESIAN_POINT ( 'NONE',  ( 5.405949406249992428, -9.363379034771808662, -111.0937500020483810 ) ) ;
#39696 = CARTESIAN_POINT ( 'NONE',  ( -5.405949406250003975, -9.363379034771801557, -189.5312500020484094 ) ) ;
#39697 = CARTESIAN_POINT ( 'NONE',  ( -5.000000000000003553, -8.660254037844383745, -95.49999999999998579 ) ) ;
#39698 = CARTESIAN_POINT ( 'NONE',  ( -9.999999999999998224, 1.224646799147353059E-15, -115.2499999999999858 ) ) ;
#39699 = CARTESIAN_POINT ( 'NONE',  ( -4.999999999999996447, 8.660254037844387298, -127.5000000000000000 ) ) ;
#39700 = CARTESIAN_POINT ( 'NONE',  ( -4.999999999999996447, 8.660254037844387298, -4.499999999999976019 ) ) ;
#39701 = CARTESIAN_POINT ( 'NONE',  ( -5.405949406250003975, -9.363379034771801557, -61.84375000204836681 ) ) ;
#39702 = CARTESIAN_POINT ( 'NONE',  ( -5.405949406249996869, 9.363379034771805109, -51.84375000204835260 ) ) ;
#39703 = CARTESIAN_POINT ( 'NONE',  ( -5.000000000000003553, -8.660254037844383745, -178.3750000040967905 ) ) ;
#39704 = CARTESIAN_POINT ( 'NONE',  ( 10.81189881249999551, -6.242252689847874514, -18.15625000204837036 ) ) ;
#39705 = CARTESIAN_POINT ( 'NONE',  ( 5.405949406249999534, 9.363379034771803333, -29.59375000204836326 ) ) ;
#39706 = CARTESIAN_POINT ( 'NONE',  ( 5.405949406249999534, 9.363379034771803333, -142.0937500020483810 ) ) ;
#39707 = CARTESIAN_POINT ( 'NONE',  ( -10.00000000000000000, -5.773502691896251982, -101.6249999999999858 ) ) ;
#39708 = CARTESIAN_POINT ( 'NONE',  ( -10.81189881249999729, 1.324075727343319199E-15, -38.28125000204838102 ) ) ;
#39709 =( BOUNDED_CURVE ( )  B_SPLINE_CURVE ( 2, ( #17063, #26800, #30046, #23995, #27012, #20955, #30261 ),
 .UNSPECIFIED., .F., .F. ) 
 B_SPLINE_CURVE_WITH_KNOTS ( ( 3, 2, 2, 3 ),
 ( 0.1417910447761193959, 0.1430348258706467535, 0.1442786069651741387, 0.1455223880597014963 ),
 .UNSPECIFIED. ) 
 CURVE ( )  GEOMETRIC_REPRESENTATION_ITEM ( )  RATIONAL_B_SPLINE_CURVE ( ( 1.000000000000000000, 0.8660254037844387076, 1.000000000000000000, 0.8660254037844387076, 1.000000000000000000, 0.8660254037844387076, 1.000000000000000000 ) ) 
 REPRESENTATION_ITEM ( '' )  );
#39710 = CARTESIAN_POINT ( 'NONE',  ( 10.00000000000051159, -5.773502691895965988, -114.6249999999999574 ) ) ;
#39711 = AXIS2_PLACEMENT_3D ( 'NONE', #41650, #25281, #35624 ) ;
#39712 = CARTESIAN_POINT ( 'NONE',  ( -4.999999999999996447, 8.660254037844387298, -59.99999999999997158 ) ) ;
#39713 = CARTESIAN_POINT ( 'NONE',  ( 10.81189881249999907, 6.242252689847868297, -131.9062500020484094 ) ) ;
#39714 = CARTESIAN_POINT ( 'NONE',  ( -10.81189881249999729, 6.242252689847871849, -111.9062500020483810 ) ) ;
#39715 = ORIENTED_EDGE ( 'NONE', *, *, #4039, .T. ) ;
#39716 = DIRECTION ( 'NONE',  ( -0.000000000000000000, -0.000000000000000000, 1.000000000000000000 ) ) ;
#39717 = CARTESIAN_POINT ( 'NONE',  ( -9.999999999999998224, 1.224646799147353059E-15, -109.6250000040967763 ) ) ;
#39718 = LINE ( 'NONE', #23335, #31207 ) ;
#39719 = CARTESIAN_POINT ( 'NONE',  ( 10.81189881249999551, -6.242252689847874514, -62.96875000204838102 ) ) ;
#39720 = ORIENTED_EDGE ( 'NONE', *, *, #29149, .T. ) ;
#39721 = CARTESIAN_POINT ( 'NONE',  ( -10.00000000000000000, -5.773502691896251982, -35.62499999999996447 ) ) ;
#39722 = EDGE_CURVE ( 'NONE', #30518, #33970, #21101, .T. ) ;
#39723 = CARTESIAN_POINT ( 'NONE',  ( 5.000000000000000000, 8.660254037844385522, -21.62500000409675494 ) ) ;
#39724 = CARTESIAN_POINT ( 'NONE',  ( 10.81189881249999551, -6.242252689847874514, -45.15625000204836681 ) ) ;
#39725 = CARTESIAN_POINT ( 'NONE',  ( 4.999999999999992006, -8.660254037844389075, -2.249999999999974243 ) ) ;
#39726 = CARTESIAN_POINT ( 'NONE',  ( 5.000000000000000000, 8.660254037844385522, -33.62500000409676915 ) ) ;
#39727 = CARTESIAN_POINT ( 'NONE',  ( -10.00000000000025580, 5.773502691896109873, -117.2500000040968047 ) ) ;
#39728 = CARTESIAN_POINT ( 'NONE',  ( 7.644554776091147741E-16, 12.48450537969573659, -143.6562500020484094 ) ) ;
#39729 = CARTESIAN_POINT ( 'NONE',  ( -10.00000000000025580, 5.773502691896109873, -121.7500000040967905 ) ) ;
#39730 = VERTEX_POINT ( 'NONE', #17852 ) ;
#39731 = VERTEX_POINT ( 'NONE', #34505 ) ;
#39732 = ORIENTED_EDGE ( 'NONE', *, *, #23539, .F. ) ;
#39733 = CARTESIAN_POINT ( 'NONE',  ( 7.070501591499376803E-16, 11.54700538379251284, -159.1250000000000284 ) ) ;
#39734 = FACE_OUTER_BOUND ( 'NONE', #37082, .T. ) ;
#39735 = CARTESIAN_POINT ( 'NONE',  ( -10.81189881249999729, 6.242252689847871849, -170.2187500020483810 ) ) ;
#39736 = CARTESIAN_POINT ( 'NONE',  ( 9.999999999999996447, -5.773502691896262640, -192.6250000000000284 ) ) ;
#39737 = CARTESIAN_POINT ( 'NONE',  ( -5.405949406250003975, -9.363379034771801557, -21.34375000204835615 ) ) ;
#39738 = DIRECTION ( 'NONE',  ( -0.000000000000000000, -0.000000000000000000, 1.000000000000000000 ) ) ;
#39739 = CARTESIAN_POINT ( 'NONE',  ( -5.405949406249996869, 9.363379034771805109, -159.8437500020484094 ) ) ;
#39740 = CARTESIAN_POINT ( 'NONE',  ( -10.81189881249999729, 1.324075727343319199E-15, -144.5937500020483810 ) ) ;
#39741 = CARTESIAN_POINT ( 'NONE',  ( -9.999999999999996447, 5.773502691896259975, -172.7500000040967905 ) ) ;
#39742 = CARTESIAN_POINT ( 'NONE',  ( -5.405949406249996869, 9.363379034771805109, -122.3437500020483952 ) ) ;
#39743 = CARTESIAN_POINT ( 'NONE',  ( 10.81189881249999729, 0.000000000000000000, -135.0312500020484094 ) ) ;
#39744 = CARTESIAN_POINT ( 'NONE',  ( 5.405949406249992428, -9.363379034771808662, -9.093750002048345493 ) ) ;
#39745 = CARTESIAN_POINT ( 'NONE',  ( -5.405949406250003975, -9.363379034771801557, -136.8437500020484094 ) ) ;
#39746 = CARTESIAN_POINT ( 'NONE',  ( -9.999999999999998224, 1.224646799147353059E-15, -130.2499999999999716 ) ) ;
#39747 =( BOUNDED_CURVE ( )  B_SPLINE_CURVE ( 2, ( #8240, #34571, #28527, #5002, #8457, #31339, #21608 ),
 .UNSPECIFIED., .F., .F. ) 
 B_SPLINE_CURVE_WITH_KNOTS ( ( 3, 2, 2, 3 ),
 ( 0.1902985074626866169, 0.1915422885572139744, 0.1927860696517413319, 0.1940298507462686894 ),
 .UNSPECIFIED. ) 
 CURVE ( )  GEOMETRIC_REPRESENTATION_ITEM ( )  RATIONAL_B_SPLINE_CURVE ( ( 0.9999999999999940048, 0.8660254037844447028, 1.000000000000000000, 0.8660254037844387076, 1.000000000000000000, 0.8660254037844357100, 1.000000000000003109 ) ) 
 REPRESENTATION_ITEM ( '' )  );
#39748 = CARTESIAN_POINT ( 'NONE',  ( 7.070501591499376803E-16, 11.54700538379251284, -44.00000000409676204 ) ) ;
#39749 = CARTESIAN_POINT ( 'NONE',  ( -9.999999999999998224, 1.224646799147353059E-15, -158.7500000000000000 ) ) ;
#39750 = CARTESIAN_POINT ( 'NONE',  ( 10.81189881249999551, -6.242252689847874514, -0.1562500020483581498 ) ) ;
#39751 = CARTESIAN_POINT ( 'NONE',  ( -10.81189881249999729, 1.324075727343319199E-15, -77.09375000204838102 ) ) ;
#39752 = CARTESIAN_POINT ( 'NONE',  ( 5.405949406249992428, -9.363379034771808662, -39.28125000204838102 ) ) ;
#39753 = CARTESIAN_POINT ( 'NONE',  ( 7.644554776091147741E-16, 12.48450537969573659, -56.46875000204837391 ) ) ;
#39754 = CARTESIAN_POINT ( 'NONE',  ( -9.999999999999227285, -5.773502691896698735, -114.0000000040967478 ) ) ;
#39755 = CARTESIAN_POINT ( 'NONE',  ( 5.405949406249999534, 9.363379034771803333, -166.0937500020484094 ) ) ;
#39756 = CARTESIAN_POINT ( 'NONE',  ( -9.999999999999998224, 1.224646799147353059E-15, -130.2499999999999716 ) ) ;
#39757 = CARTESIAN_POINT ( 'NONE',  ( 5.405949406249999534, 9.363379034771803333, -136.2812500020483810 ) ) ;
#39758 = DIRECTION ( 'NONE',  ( -0.000000000000000000, -0.000000000000000000, -1.000000000000000000 ) ) ;
#39759 = CARTESIAN_POINT ( 'NONE',  ( 5.000000000000000000, 8.660254037844385522, -114.6250000040967763 ) ) ;
#39760 = CARTESIAN_POINT ( 'NONE',  ( -4.999999999999996447, 8.660254037844387298, -89.99999999999998579 ) ) ;
#39761 = ORIENTED_EDGE ( 'NONE', *, *, #4849, .T. ) ;
#39762 =( BOUNDED_CURVE ( )  B_SPLINE_CURVE ( 2, ( #5632, #15737, #18572, #42489, #41857, #42074, #12504 ),
 .UNSPECIFIED., .F., .F. ) 
 B_SPLINE_CURVE_WITH_KNOTS ( ( 3, 2, 2, 3 ),
 ( 0.1194029850746269744, 0.1206467661691543042, 0.1218905472636816062, 0.1231343283582089221 ),
 .UNSPECIFIED. ) 
 CURVE ( )  GEOMETRIC_REPRESENTATION_ITEM ( )  RATIONAL_B_SPLINE_CURVE ( ( 0.9999999999999880096, 0.8660254037844506980, 1.000000000000000000, 0.8660254037844387076, 1.000000000000000000, 0.8660254037844417052, 0.9999999999999970024 ) ) 
 REPRESENTATION_ITEM ( '' )  );
#39763 = CARTESIAN_POINT ( 'NONE',  ( 7.644554776091147741E-16, 12.48450537969573659, -109.1562500020483810 ) ) ;
#39764 = CARTESIAN_POINT ( 'NONE',  ( -4.999999999999996447, 8.660254037844387298, -130.8750000040967905 ) ) ;
#39765 = CARTESIAN_POINT ( 'NONE',  ( -9.999999999999998224, 1.224646799147353059E-15, -200.0000000000000000 ) ) ;
#39766 = CARTESIAN_POINT ( 'NONE',  ( 7.644554776091147741E-16, 12.48450537969573659, -161.6562500020484379 ) ) ;
#39767 = CARTESIAN_POINT ( 'NONE',  ( -4.999999999999996447, 8.660254037844387298, -39.37500000409676915 ) ) ;
#39768 = CARTESIAN_POINT ( 'NONE',  ( -4.999999999999996447, 8.660254037844387298, -154.8750000040967905 ) ) ;
#39769 = CARTESIAN_POINT ( 'NONE',  ( 10.81189881249999729, 0.000000000000000000, -51.03125000204835970 ) ) ;
#39770 = CARTESIAN_POINT ( 'NONE',  ( -2.121150477449813534E-15, -11.54700538379251284, -63.87499999999998579 ) ) ;
#39771 = CARTESIAN_POINT ( 'NONE',  ( -10.81189881249999729, 6.242252689847871849, -162.9062500020484094 ) ) ;
#39772 = CARTESIAN_POINT ( 'NONE',  ( 10.81189881249999729, 0.000000000000000000, -136.3437500020484094 ) ) ;
#39773 = CARTESIAN_POINT ( 'NONE',  ( 9.999999999999998224, 0.000000000000000000, -60.87500000409676204 ) ) ;
#39774 = CARTESIAN_POINT ( 'NONE',  ( 9.999999999999998224, 0.000000000000000000, -143.0000000000000000 ) ) ;
#39775 = ORIENTED_EDGE ( 'NONE', *, *, #30548, .F. ) ;
#39776 = CARTESIAN_POINT ( 'NONE',  ( 9.999999999999998224, 0.000000000000000000, -171.5000000000000000 ) ) ;
#39777 = EDGE_CURVE ( 'NONE', #40396, #12739, #2127, .T. ) ;
#39779 = VERTEX_POINT ( 'NONE', #18075 ) ;
#39778 = CARTESIAN_POINT ( 'NONE',  ( 10.81189881249999551, -6.242252689847874514, -67.65625000204838102 ) ) ;
#39781 = ORIENTED_EDGE ( 'NONE', *, *, #11956, .F. ) ;
#39780 = CARTESIAN_POINT ( 'NONE',  ( -5.405949406249996869, 9.363379034771805109, -122.3437500020483952 ) ) ;
#39782 = ORIENTED_EDGE ( 'NONE', *, *, #42588, .T. ) ;
#39783 = CARTESIAN_POINT ( 'NONE',  ( 7.644554776091147741E-16, 12.48450537969573659, -24.96875000204837036 ) ) ;
#39784 = UNCERTAINTY_MEASURE_WITH_UNIT (LENGTH_MEASURE( 1.000000000000000082E-05 ), #40886, 'distance_accuracy_value', 'NONE');
#39785 = CARTESIAN_POINT ( 'NONE',  ( -10.81189881249999729, 1.324075727343319199E-15, -195.5937500020484094 ) ) ;
#39786 = CARTESIAN_POINT ( 'NONE',  ( 10.81189881249999551, -6.242252689847874514, -49.46875000204835970 ) ) ;
#39787 = CARTESIAN_POINT ( 'NONE',  ( -9.999999999999998224, 1.224646799147353059E-15, -200.0000000000000000 ) ) ;
#39788 = DIRECTION ( 'NONE',  ( -1.000000000000000000, 0.000000000000000000, 0.000000000000000000 ) ) ;
#39789 = CARTESIAN_POINT ( 'NONE',  ( -5.405949406250003975, -9.363379034771801557, -177.3437500020483810 ) ) ;
#39790 = CARTESIAN_POINT ( 'NONE',  ( -5.405949406250003975, -9.363379034771801557, -171.3437500020484094 ) ) ;
#39791 = CARTESIAN_POINT ( 'NONE',  ( -10.81189881249999729, 6.242252689847871849, -146.2187500020483810 ) ) ;
#39792 = CARTESIAN_POINT ( 'NONE',  ( 10.81189881249999551, -6.242252689847874514, -164.9687500020483810 ) ) ;
#39793 = CARTESIAN_POINT ( 'NONE',  ( -79.99999999999992895, 19.99999999999998934, -170.0000000000000000 ) ) ;
#39794 = DIRECTION ( 'NONE',  ( -1.000000000000000000, 0.000000000000000000, 0.000000000000000000 ) ) ;
#39795 = CARTESIAN_POINT ( 'NONE',  ( -5.000000000000003553, -8.660254037844383745, -184.0000000000000000 ) ) ;
#39796 = CARTESIAN_POINT ( 'NONE',  ( -2.293366432827344421E-15, -12.48450537969573659, -99.21875000204839523 ) ) ;
#39797 = EDGE_CURVE ( 'NONE', #8336, #2222, #15663, .T. ) ;
#39798 = CARTESIAN_POINT ( 'NONE',  ( -9.999999999999998224, 1.224646799147353059E-15, -151.2500000000000000 ) ) ;
#39799 = CARTESIAN_POINT ( 'NONE',  ( 10.81189881249999551, -6.242252689847874514, -67.65625000204838102 ) ) ;
#39800 = CARTESIAN_POINT ( 'NONE',  ( -9.999999999999998224, 1.224646799147353059E-15, -5.749999999999976907 ) ) ;
#39801 = CARTESIAN_POINT ( 'NONE',  ( 5.405949406249999534, 9.363379034771803333, -187.0937500020483810 ) ) ;
#39802 = CARTESIAN_POINT ( 'NONE',  ( 10.81189881249999551, -6.242252689847874514, -124.6562500020483952 ) ) ;
#39803 = CARTESIAN_POINT ( 'NONE',  ( 10.81189881249999729, 0.000000000000000000, -160.5312500020484094 ) ) ;
#39804 = CARTESIAN_POINT ( 'NONE',  ( -10.81189881249999729, 6.242252689847871849, -56.40625000204838813 ) ) ;
#39805 = CARTESIAN_POINT ( 'NONE',  ( 5.000000000000000000, 8.660254037844385522, -138.6250000040967905 ) ) ;
#39806 = CARTESIAN_POINT ( 'NONE',  ( 5.000000000000000000, 8.660254037844385522, -118.7500000000000000 ) ) ;
#39807 = ORIENTED_EDGE ( 'NONE', *, *, #29664, .F. ) ;
#39808 = CARTESIAN_POINT ( 'NONE',  ( -2.293366432827344421E-15, -12.48450537969573659, -133.9062500020483810 ) ) ;
#39809 = CARTESIAN_POINT ( 'NONE',  ( 5.405949406249999534, 9.363379034771803333, -145.2812500020483810 ) ) ;
#39810 = CARTESIAN_POINT ( 'NONE',  ( -2.293366432827344421E-15, -12.48450537969573659, -192.4062500020484094 ) ) ;
#39811 = CARTESIAN_POINT ( 'NONE',  ( -9.999999999998969713, -5.773502691896847949, -43.50000000409674783 ) ) ;
#39812 = CARTESIAN_POINT ( 'NONE',  ( -5.405949406250003975, -9.363379034771801557, -85.84375000204836681 ) ) ;
#39813 = ORIENTED_EDGE ( 'NONE', *, *, #23289, .F. ) ;
#39814 = CARTESIAN_POINT ( 'NONE',  ( -9.999999999999998224, 5.773502691896259087, -56.87499999999998579 ) ) ;
#39815 = CARTESIAN_POINT ( 'NONE',  ( -5.405949406250003975, -9.363379034771801557, -180.3437500020483810 ) ) ;
#39816 = CARTESIAN_POINT ( 'NONE',  ( 5.000000000000000000, 8.660254037844385522, -63.62500000409676204 ) ) ;
#39817 = VECTOR ( 'NONE', #41810, 1000.000000000000000 ) ;
#39818 = CARTESIAN_POINT ( 'NONE',  ( -4.999999999999996447, 8.660254037844387298, -21.37500000409675494 ) ) ;
#39819 = CARTESIAN_POINT ( 'NONE',  ( 9.999999999999612754, 5.773502691896477579, -179.2500000040967905 ) ) ;
#39820 = CARTESIAN_POINT ( 'NONE',  ( 5.405949406249992428, -9.363379034771808662, -76.78125000204838102 ) ) ;
#39821 = CARTESIAN_POINT ( 'NONE',  ( -10.81189881249999729, -6.242252689847864744, -56.15625000204837391 ) ) ;
#39822 = CARTESIAN_POINT ( 'NONE',  ( -9.999999999999998224, 5.773502691896259087, -51.25000000409677625 ) ) ;
#39823 = CARTESIAN_POINT ( 'NONE',  ( 5.405949406249992428, -9.363379034771808662, -7.593750002048343717 ) ) ;
#39824 = CARTESIAN_POINT ( 'NONE',  ( 9.999999999999998224, 0.000000000000000000, -137.3750000040967905 ) ) ;
#39825 = CARTESIAN_POINT ( 'NONE',  ( -5.405949406250003975, -9.363379034771801557, -183.5312500020484094 ) ) ;
#39826 = CARTESIAN_POINT ( 'NONE',  ( 5.405949406249992428, -9.363379034771808662, -9.281250002048352599 ) ) ;
#39827 = CARTESIAN_POINT ( 'NONE',  ( 7.070501591499376803E-16, 11.54700538379251284, -79.62500000000000000 ) ) ;
#39828 = CYLINDRICAL_SURFACE ( 'NONE', #34458, 9.999999999999998224 ) ;
#39829 =( BOUNDED_CURVE ( )  B_SPLINE_CURVE ( 2, ( #7131, #24404, #23749, #1518, #37112, #3900, #26771 ),
 .UNSPECIFIED., .F., .F. ) 
 B_SPLINE_CURVE_WITH_KNOTS ( ( 3, 2, 2, 3 ),
 ( 0.7425373134328361324, 0.7437810945273634067, 0.7450248756218907920, 0.7462686567164180662 ),
 .UNSPECIFIED. ) 
 CURVE ( )  GEOMETRIC_REPRESENTATION_ITEM ( )  RATIONAL_B_SPLINE_CURVE ( ( 0.9999999999999641398, 0.8660254037844745678, 1.000000000000000000, 0.8660254037844387076, 1.000000000000000000, 0.8660254037844267172, 1.000000000000011990 ) ) 
 REPRESENTATION_ITEM ( '' )  );
#39830 = LINE ( 'NONE', #6411, #20094 ) ;
#39831 = DIRECTION ( 'NONE',  ( -1.000000000000000000, 0.000000000000000000, 0.000000000000000000 ) ) ;
#39832 = CARTESIAN_POINT ( 'NONE',  ( 10.00000000000000000, 5.773502691896255534, -166.8750000000000000 ) ) ;
#39833 = CYLINDRICAL_SURFACE ( 'NONE', #15144, 9.999999999999998224 ) ;
#39835 = ORIENTED_EDGE ( 'NONE', *, *, #32845, .T. ) ;
#39834 = CARTESIAN_POINT ( 'NONE',  ( -5.405949406249996869, 9.363379034771805109, -91.03125000204838102 ) ) ;
#39836 = DIRECTION ( 'NONE',  ( -0.000000000000000000, -0.000000000000000000, 1.000000000000000000 ) ) ;
#39837 = EDGE_CURVE ( 'NONE', #32599, #3542, #31477, .T. ) ;
#39839 = ORIENTED_EDGE ( 'NONE', *, *, #18037, .F. ) ;
#39838 = CARTESIAN_POINT ( 'NONE',  ( 7.070501591499376803E-16, 11.54700538379251284, -162.1250000000000284 ) ) ;
#39840 = ORIENTED_EDGE ( 'NONE', *, *, #4578, .T. ) ;
#39841 = CARTESIAN_POINT ( 'NONE',  ( -10.81189881249999729, 6.242252689847871849, -33.71875000204835260 ) ) ;
#39842 = CARTESIAN_POINT ( 'NONE',  ( 10.81189881249999551, -6.242252689847874514, -18.15625000204837036 ) ) ;
#39843 = CARTESIAN_POINT ( 'NONE',  ( -5.405949406250003975, -9.363379034771801557, -73.84375000204838102 ) ) ;
#39844 = DIRECTION ( 'NONE',  ( 1.000000000000000000, 0.000000000000000000, 0.000000000000000000 ) ) ;
#39845 = CARTESIAN_POINT ( 'NONE',  ( 5.405949406249992428, -9.363379034771808662, -195.0937500020484094 ) ) ;
#39846 = CARTESIAN_POINT ( 'NONE',  ( -5.405949406250003975, -9.363379034771801557, -151.8437500020483810 ) ) ;
#39847 = CARTESIAN_POINT ( 'NONE',  ( -2.121150477449813534E-15, -11.54700538379251284, -79.25000000409677625 ) ) ;
#39848 = FACE_OUTER_BOUND ( 'NONE', #18772, .T. ) ;
#39849 = CARTESIAN_POINT ( 'NONE',  ( 7.644554776091147741E-16, 12.48450537969573659, -151.1562500020484094 ) ) ;
#39850 = CARTESIAN_POINT ( 'NONE',  ( 10.00000000000000000, 5.773502691896255534, -6.750000004096744277 ) ) ;
#39851 = CARTESIAN_POINT ( 'NONE',  ( -2.121150477449813534E-15, -11.54700538379251284, -103.2500000040967763 ) ) ;
#39852 = CARTESIAN_POINT ( 'NONE',  ( -10.81189881249999729, 6.242252689847871849, -122.2187500020483810 ) ) ;
#39853 = LINE ( 'NONE', #10707, #12805 ) ;
#39854 = CARTESIAN_POINT ( 'NONE',  ( -10.81189881249999729, 6.242252689847871849, -90.90625000204838102 ) ) ;
#39855 = CARTESIAN_POINT ( 'NONE',  ( 10.81189881249999551, -6.242252689847874514, -106.4687500020483810 ) ) ;
#39856 = CARTESIAN_POINT ( 'NONE',  ( 5.405949406249999534, 9.363379034771803333, -68.59375000204836681 ) ) ;
#39857 = CARTESIAN_POINT ( 'NONE',  ( -2.293366432827344421E-15, -12.48450537969573659, -73.90625000204836681 ) ) ;
#39858 = CARTESIAN_POINT ( 'NONE',  ( 4.999999999999992006, -8.660254037844389075, -161.6250000040967905 ) ) ;
#39859 = DIRECTION ( 'NONE',  ( -0.000000000000000000, -0.000000000000000000, -1.000000000000000000 ) ) ;
#39860 = CARTESIAN_POINT ( 'NONE',  ( -5.405949406249996869, 9.363379034771805109, -161.5312500020484094 ) ) ;
#39861 = CARTESIAN_POINT ( 'NONE',  ( -2.293366432827344421E-15, -12.48450537969573659, -172.9062500020484379 ) ) ;
#39862 = CYLINDRICAL_SURFACE ( 'NONE', #28432, 9.999999999999998224 ) ;
#39863 = CARTESIAN_POINT ( 'NONE',  ( 10.81189881249999907, 6.242252689847868297, 0.2812499979516491777 ) ) ;
#39864 = CARTESIAN_POINT ( 'NONE',  ( -10.00000000000051337, 5.773502691895962435, -108.2500000040967763 ) ) ;
#39865 = CARTESIAN_POINT ( 'NONE',  ( -10.81189881249999907, -6.242252689847864744, -105.4687500020483668 ) ) ;
#39866 = CARTESIAN_POINT ( 'NONE',  ( 9.999999999999998224, 0.000000000000000000, -81.49999999999998579 ) ) ;
#39867 = CARTESIAN_POINT ( 'NONE',  ( -5.405949406250003975, -9.363379034771801557, -6.531250002048377468 ) ) ;
#39868 = CARTESIAN_POINT ( 'NONE',  ( 9.999999999999998224, 0.000000000000000000, -86.37500000409677625 ) ) ;
#39869 = CARTESIAN_POINT ( 'NONE',  ( 9.999999999999998224, 0.000000000000000000, -107.3750000040967763 ) ) ;
#39870 = CARTESIAN_POINT ( 'NONE',  ( 5.405949406249999534, 9.363379034771803333, -109.2812500020483810 ) ) ;
#39871 = CARTESIAN_POINT ( 'NONE',  ( 10.81189881249999729, 6.242252689847867408, -86.90625000204836681 ) ) ;
#39872 = EDGE_LOOP ( 'NONE', ( #37550, #19040, #41433, #26945 ) ) ;
#39873 =( BOUNDED_CURVE ( )  B_SPLINE_CURVE ( 2, ( #7622, #41039, #11482, #40828, #24684, #20557, #14062 ),
 .UNSPECIFIED., .F., .F. ) 
 B_SPLINE_CURVE_WITH_KNOTS ( ( 3, 2, 2, 3 ),
 ( 0.4701492537313434195, 0.4713930348258707492, 0.4726368159203981900, 0.4738805970149255198 ),
 .UNSPECIFIED. ) 
 CURVE ( )  GEOMETRIC_REPRESENTATION_ITEM ( )  RATIONAL_B_SPLINE_CURVE ( ( 0.9999999999999880096, 0.8660254037844506980, 1.000000000000000000, 0.8660254037844387076, 1.000000000000000000, 0.8660254037844207220, 1.000000000000017986 ) ) 
 REPRESENTATION_ITEM ( '' )  );
#39874 = CARTESIAN_POINT ( 'NONE',  ( -9.999999999999998224, 1.224646799147353059E-15, -84.12500000409677625 ) ) ;
#39875 = CARTESIAN_POINT ( 'NONE',  ( 9.999999999999998224, 0.000000000000000000, -134.3750000040967905 ) ) ;
#39876 = CARTESIAN_POINT ( 'NONE',  ( 10.81189881249999551, -6.242252689847874514, -35.96875000204835260 ) ) ;
#39877 = ORIENTED_EDGE ( 'NONE', *, *, #7199, .F. ) ;
#39878 = CARTESIAN_POINT ( 'NONE',  ( 9.999999999999998224, 0.000000000000000000, -9.499999999999953815 ) ) ;
#39879 = CARTESIAN_POINT ( 'NONE',  ( -4.999999999999996447, 8.660254037844387298, -142.5000000000000000 ) ) ;
#39880 = CARTESIAN_POINT ( 'NONE',  ( -9.999999999998969713, -5.773502691896847949, -15.00000000409674072 ) ) ;
#39881 = AXIS2_PLACEMENT_3D ( 'NONE', #8889, #8039, #1569 ) ;
#39882 = CARTESIAN_POINT ( 'NONE',  ( 9.999999999999996447, -5.773502691896262640, -14.50000000409676382 ) ) ;
#39883 = CARTESIAN_POINT ( 'NONE',  ( -5.000000000000003553, -8.660254037844383745, -191.5000000000000000 ) ) ;
#39884 = ADVANCED_FACE ( 'NONE', ( #2965 ), #26264, .T. ) ;
#39885 = CARTESIAN_POINT ( 'NONE',  ( -9.999999999999998224, 1.224646799147353059E-15, -95.74999999999998579 ) ) ;
#39887 = ORIENTED_EDGE ( 'NONE', *, *, #35386, .F. ) ;
#39886 = CARTESIAN_POINT ( 'NONE',  ( -5.405949406249996869, 9.363379034771805109, -115.0312500020483952 ) ) ;
#39888 = CARTESIAN_POINT ( 'NONE',  ( -2.275517850991317657E-15, -20.00000000000000000, -232.0000000000000000 ) ) ;
#39889 = EDGE_CURVE ( 'NONE', #19247, #13498, #28931, .T. ) ;
#39890 = EDGE_CURVE ( 'NONE', #12005, #21356, #19554, .T. ) ;
#39891 = ORIENTED_EDGE ( 'NONE', *, *, #33336, .T. ) ;
#39892 = EDGE_CURVE ( 'NONE', #36657, #23120, #36345, .T. ) ;
#39893 = CARTESIAN_POINT ( 'NONE',  ( -10.81189881249999729, 6.242252689847871849, -44.40625000204836681 ) ) ;
#39894 = PERSON_AND_ORGANIZATION ( #11915, #17965 ) ;
#39895 = CARTESIAN_POINT ( 'NONE',  ( -10.81189881249999729, 6.242252689847871849, -95.21875000204838102 ) ) ;
#39896 = CARTESIAN_POINT ( 'NONE',  ( 5.405949406249999534, 9.363379034771803333, -125.7812500020483668 ) ) ;
#39897 = VERTEX_POINT ( 'NONE', #26054 ) ;
#39898 = CARTESIAN_POINT ( 'NONE',  ( 9.999999999998969713, 5.773502691896851502, -51.75000000409674783 ) ) ;
#39899 = CARTESIAN_POINT ( 'NONE',  ( 7.070501591499376803E-16, 11.54700538379251284, -128.0000000040967905 ) ) ;
#39900 = CARTESIAN_POINT ( 'NONE',  ( -10.81189881249999729, 1.324075727343319199E-15, -173.2812500020484094 ) ) ;
#39901 = DIRECTION ( 'NONE',  ( -0.000000000000000000, -0.000000000000000000, 1.000000000000000000 ) ) ;
#39902 = ADVANCED_FACE ( 'NONE', ( #6414 ), #32118, .T. ) ;
#39903 = CARTESIAN_POINT ( 'NONE',  ( -5.405949406250003975, -9.363379034771801557, -132.3437500020484094 ) ) ;
#39904 = CARTESIAN_POINT ( 'NONE',  ( -10.81189881249999729, 1.324075727343319199E-15, -95.09375000204838102 ) ) ;
#39905 = LINE ( 'NONE', #7537, #3573 ) ;
#39906 = CARTESIAN_POINT ( 'NONE',  ( 10.81189881249999551, -6.242252689847874514, -103.6562500020483668 ) ) ;
#39907 = CARTESIAN_POINT ( 'NONE',  ( -10.00000000000000000, -5.773502691896251982, -183.0000000040967905 ) ) ;
#39908 = CARTESIAN_POINT ( 'NONE',  ( -5.405949406249996869, 9.363379034771805109, -113.3437500020483810 ) ) ;
#39909 = CARTESIAN_POINT ( 'NONE',  ( -5.405949406250003975, -9.363379034771801557, -179.0312500020483810 ) ) ;
#39910 = DIRECTION ( 'NONE',  ( 0.000000000000000000, 0.000000000000000000, -1.000000000000000000 ) ) ;
#39911 = CARTESIAN_POINT ( 'NONE',  ( -5.405949406249996869, 9.363379034771805109, -179.5312500020483810 ) ) ;
#39912 = CARTESIAN_POINT ( 'NONE',  ( -5.405949406249996869, 9.363379034771805109, -199.0312500020484094 ) ) ;
#39913 = EDGE_CURVE ( 'NONE', #7881, #36957, #12439, .T. ) ;
#39914 = CARTESIAN_POINT ( 'NONE',  ( -5.405949406249996869, 9.363379034771805109, -62.34375000204836681 ) ) ;
#39915 = CARTESIAN_POINT ( 'NONE',  ( -2.293366432827344421E-15, -12.48450537969573659, -40.71875000204835260 ) ) ;
#39916 = CARTESIAN_POINT ( 'NONE',  ( 9.999999999999998224, 0.000000000000000000, -182.3750000040967905 ) ) ;
#39917 = CARTESIAN_POINT ( 'NONE',  ( 5.405949406249992428, -9.363379034771808662, -21.28125000204836326 ) ) ;
#39918 = CARTESIAN_POINT ( 'NONE',  ( -2.293366432827344421E-15, -12.48450537969573659, -27.21875000204837747 ) ) ;
#39919 = CARTESIAN_POINT ( 'NONE',  ( -9.214310226692173294E-15, 125.0000000000000000, 32.24999999999999289 ) ) ;
#39920 = CARTESIAN_POINT ( 'NONE',  ( 7.644554776091147741E-16, 12.48450537969573659, -129.9687500020483810 ) ) ;
#39921 = CARTESIAN_POINT ( 'NONE',  ( 10.00000000000000000, 5.773502691896255534, -103.8750000000000000 ) ) ;
#39922 = CARTESIAN_POINT ( 'NONE',  ( 10.81189881249999729, 0.000000000000000000, -37.53125000204838102 ) ) ;
#39923 = EDGE_CURVE ( 'NONE', #39570, #40457, #31707, .T. ) ;
#39924 = LINE ( 'NONE', #674, #3136 ) ;
#39925 = CARTESIAN_POINT ( 'NONE',  ( -10.00000000000000000, -5.773502691896251982, -56.62499999999997868 ) ) ;
#39926 = CARTESIAN_POINT ( 'NONE',  ( 5.405949406249999534, 9.363379034771803333, -128.7812500020483810 ) ) ;
#39927 = CARTESIAN_POINT ( 'NONE',  ( 5.405949406249992428, -9.363379034771808662, -108.2812500020483810 ) ) ;
#39928 = VERTEX_POINT ( 'NONE', #19350 ) ;
#39929 = DIRECTION ( 'NONE',  ( 0.000000000000000000, 0.000000000000000000, -1.000000000000000000 ) ) ;
#39930 = CARTESIAN_POINT ( 'NONE',  ( -9.999999999999998224, 1.224646799147353059E-15, -108.1250000040967763 ) ) ;
#39931 = CARTESIAN_POINT ( 'NONE',  ( -9.999999999999998224, 1.224646799147353059E-15, -161.7500000000000000 ) ) ;
#39932 = CARTESIAN_POINT ( 'NONE',  ( -10.81189881249999729, 1.324075727343319199E-15, -63.59375000204836681 ) ) ;
#39933 = ORIENTED_EDGE ( 'NONE', *, *, #17095, .F. ) ;
#39934 = CARTESIAN_POINT ( 'NONE',  ( 9.999999999999996447, -5.773502691896262640, -30.62499999999995381 ) ) ;
#39935 = CARTESIAN_POINT ( 'NONE',  ( 10.81189881249999551, -6.242252689847874514, -36.15625000204835970 ) ) ;
#39936 = CARTESIAN_POINT ( 'NONE',  ( -4.999999999999996447, 8.660254037844387298, -36.37500000409676915 ) ) ;
#39937 = CARTESIAN_POINT ( 'NONE',  ( 5.405949406249999534, 9.363379034771803333, -142.2812500020483810 ) ) ;
#39938 = DIRECTION ( 'NONE',  ( -1.000000000000000000, 0.000000000000000000, 0.000000000000000000 ) ) ;
#39939 = ORIENTED_EDGE ( 'NONE', *, *, #37085, .T. ) ;
#39940 = EDGE_CURVE ( 'NONE', #8113, #7578, #29083, .T. ) ;
#39941 = AXIS2_PLACEMENT_3D ( 'NONE', #1862, #40887, #1643 ) ;
#39942 = EDGE_CURVE ( 'NONE', #31108, #41855, #20086, .T. ) ;
#39943 = ORIENTED_EDGE ( 'NONE', *, *, #5390, .F. ) ;
#39944 = CARTESIAN_POINT ( 'NONE',  ( -10.00000000000076916, 5.773502691895813221, -126.2500000040967763 ) ) ;
#39945 = FACE_OUTER_BOUND ( 'NONE', #32227, .T. ) ;
#39946 = CARTESIAN_POINT ( 'NONE',  ( -5.405949406250003975, -9.363379034771801557, -168.3437500020484094 ) ) ;
#39947 = CARTESIAN_POINT ( 'NONE',  ( 0.000000000000000000, 0.000000000000000000, -99.99999999999998579 ) ) ;
#39948 = CARTESIAN_POINT ( 'NONE',  ( 5.405949406249999534, 9.363379034771803333, -22.09375000204835615 ) ) ;
#39949 = CARTESIAN_POINT ( 'NONE',  ( -9.999999999999998224, 0.000000000000000000, -99.99999999999998579 ) ) ;
#39950 = CARTESIAN_POINT ( 'NONE',  ( 9.999999999999479527, 5.773502691896553074, -150.3750000000000000 ) ) ;
#39951 = CARTESIAN_POINT ( 'NONE',  ( -10.81189881249999729, 1.324075727343319199E-15, -155.0937500020483810 ) ) ;
#39952 = CARTESIAN_POINT ( 'NONE',  ( 10.81189881249999907, 6.242252689847868297, -140.7187500020483810 ) ) ;
#39953 =( BOUNDED_CURVE ( )  B_SPLINE_CURVE ( 2, ( #33059, #12958, #36291, #36076, #20087, #39727, #22704 ),
 .UNSPECIFIED., .F., .F. ) 
 B_SPLINE_CURVE_WITH_KNOTS ( ( 3, 2, 2, 3 ),
 ( 0.4029850746268657802, 0.4042288557213931655, 0.4054726368159204397, 0.4067164179104478250 ),
 .UNSPECIFIED. ) 
 CURVE ( )  GEOMETRIC_REPRESENTATION_ITEM ( )  RATIONAL_B_SPLINE_CURVE ( ( 0.9999999999999880096, 0.8660254037844506980, 1.000000000000000000, 0.8660254037844387076, 1.000000000000000000, 0.8660254037844327124, 1.000000000000005995 ) ) 
 REPRESENTATION_ITEM ( '' )  );
#39954 = CARTESIAN_POINT ( 'NONE',  ( -5.000000000000003553, -8.660254037844383745, -8.875000004096744277 ) ) ;
#39955 = CARTESIAN_POINT ( 'NONE',  ( -5.405949406250003975, -9.363379034771801557, -129.3437500020484094 ) ) ;
#39956 = CARTESIAN_POINT ( 'NONE',  ( 9.999999999999996447, -5.773502691896262640, -196.0000000040968189 ) ) ;
#39957 = CARTESIAN_POINT ( 'NONE',  ( 10.81189881249999551, -6.242252689847874514, -133.6562500020483810 ) ) ;
#39958 = CARTESIAN_POINT ( 'NONE',  ( -5.405949406249996869, 9.363379034771805109, -8.343750002048345493 ) ) ;
#39960 = ADVANCED_FACE ( 'NONE', ( #5780 ), #22814, .T. ) ;
#39959 = CARTESIAN_POINT ( 'NONE',  ( 10.81189881249999729, 6.242252689847867408, -139.2187500020483810 ) ) ;
#39961 = CARTESIAN_POINT ( 'NONE',  ( -9.999999999999998224, 0.000000000000000000, -99.99999999999998579 ) ) ;
#39962 = CARTESIAN_POINT ( 'NONE',  ( 9.999999999998969713, 5.773502691896851502, -5.250000004096743389 ) ) ;
#39963 = CARTESIAN_POINT ( 'NONE',  ( 7.070501591499377789E-16, 11.54700538379251284, -157.6250000000000000 ) ) ;
#39964 = LINE ( 'NONE', #39325, #14978 ) ;
#39965 = CARTESIAN_POINT ( 'NONE',  ( 5.405949406249999534, 9.363379034771803333, -86.59375000204836681 ) ) ;
#39966 = CARTESIAN_POINT ( 'NONE',  ( -2.293366432827344421E-15, -12.48450537969573659, -64.71875000204838102 ) ) ;
#39967 = CARTESIAN_POINT ( 'NONE',  ( 5.405949406249992428, -9.363379034771808662, -40.78125000204838102 ) ) ;
#39968 = CARTESIAN_POINT ( 'NONE',  ( -5.405949406250003975, -9.363379034771801557, -51.34375000204835260 ) ) ;
#39969 = CARTESIAN_POINT ( 'NONE',  ( 4.999999999999992006, -8.660254037844389075, -139.1250000040967905 ) ) ;
#39970 = CARTESIAN_POINT ( 'NONE',  ( -5.405949406250003975, -9.363379034771801557, -160.8437500020484094 ) ) ;
#39971 = CARTESIAN_POINT ( 'NONE',  ( -4.999999999999996447, 8.660254037844387298, -130.5000000000000000 ) ) ;
#39972 = CARTESIAN_POINT ( 'NONE',  ( 5.405949406249999534, 9.363379034771803333, -137.7812500020483810 ) ) ;
#39973 = DIRECTION ( 'NONE',  ( -1.000000000000000000, 0.000000000000000000, 0.000000000000000000 ) ) ;
#39974 = CARTESIAN_POINT ( 'NONE',  ( 10.00000000000000000, 5.773502691896255534, -84.37499999999998579 ) ) ;
#39975 = CARTESIAN_POINT ( 'NONE',  ( -5.405949406249996869, 9.363379034771805109, -20.53125000204836326 ) ) ;
#39976 = VERTEX_POINT ( 'NONE', #5993 ) ;
#39977 = CARTESIAN_POINT ( 'NONE',  ( -10.81189881249999729, 1.324075727343319199E-15, -111.7812500020483810 ) ) ;
#39978 = CARTESIAN_POINT ( 'NONE',  ( 9.999999999999996447, -5.773502691896262640, -136.0000000040967905 ) ) ;
#39979 = CARTESIAN_POINT ( 'NONE',  ( -5.000000000000003553, -8.660254037844383745, -178.0000000000000000 ) ) ;
#39980 = AXIS2_PLACEMENT_3D ( 'NONE', #19139, #19343, #38359 ) ;
#39981 = CARTESIAN_POINT ( 'NONE',  ( -5.000000000000003553, -8.660254037844383745, -43.37500000409677625 ) ) ;
#39982 = CARTESIAN_POINT ( 'NONE',  ( 0.000000000000000000, 0.000000000000000000, -99.99999999999998579 ) ) ;
#39983 = CARTESIAN_POINT ( 'NONE',  ( -10.81189881249999729, 1.324075727343319199E-15, -48.78125000204838813 ) ) ;
#39984 = CARTESIAN_POINT ( 'NONE',  ( 7.644554776091147741E-16, 12.48450537969573659, -158.6562500020484094 ) ) ;
#39985 = CARTESIAN_POINT ( 'NONE',  ( -10.81189881249999907, -6.242252689847864744, -138.4687500020484094 ) ) ;
#39986 = LINE ( 'NONE', #10417, #31165 ) ;
#39987 = CARTESIAN_POINT ( 'NONE',  ( 7.070501591499376803E-16, 11.54700538379251284, -151.6250000000000000 ) ) ;
#39988 = ORIENTED_EDGE ( 'NONE', *, *, #7202, .T. ) ;
#39989 = CARTESIAN_POINT ( 'NONE',  ( 4.999999999999992006, -8.660254037844389075, -78.74999999999998579 ) ) ;
#39991 = ORIENTED_EDGE ( 'NONE', *, *, #28811, .F. ) ;
#39990 = CARTESIAN_POINT ( 'NONE',  ( -2.293366432827344421E-15, -12.48450537969573659, -64.90625000204838102 ) ) ;
#39992 = APPROVAL_ROLE ( '' ) ;
#39994 = ORIENTED_EDGE ( 'NONE', *, *, #20835, .T. ) ;
#39993 = CARTESIAN_POINT ( 'NONE',  ( 10.81189881249999907, 6.242252689847868297, -121.2187500020483952 ) ) ;
#39995 = CARTESIAN_POINT ( 'NONE',  ( 5.405949406249992428, -9.363379034771808662, -21.09375000204835615 ) ) ;
#39996 =( BOUNDED_CURVE ( )  B_SPLINE_CURVE ( 2, ( #32846, #38462, #2644, #18823, #29181, #32216, #39301 ),
 .UNSPECIFIED., .F., .F. ) 
 B_SPLINE_CURVE_WITH_KNOTS ( ( 3, 2, 2, 3 ),
 ( 0.2052238805970149627, 0.2064676616915423202, 0.2077114427860697055, 0.2089552238805970630 ),
 .UNSPECIFIED. ) 
 CURVE ( )  GEOMETRIC_REPRESENTATION_ITEM ( )  RATIONAL_B_SPLINE_CURVE ( ( 0.9999999999999970024, 0.8660254037844417052, 1.000000000000000000, 0.8660254037844387076, 1.000000000000000000, 0.8660254037844327124, 1.000000000000005995 ) ) 
 REPRESENTATION_ITEM ( '' )  );
#39997 = CARTESIAN_POINT ( 'NONE',  ( 5.405949406249992428, -9.363379034771808662, -195.0937500020484094 ) ) ;
#39998 = AXIS2_PLACEMENT_3D ( 'NONE', #24743, #11112, #37889 ) ;
#40000 = EDGE_CURVE ( 'NONE', #9954, #26056, #24519, .T. ) ;
#39999 = CARTESIAN_POINT ( 'NONE',  ( -10.81189881249999729, 1.324075727343319199E-15, -50.09375000204835260 ) ) ;
#40001 = CARTESIAN_POINT ( 'NONE',  ( 0.000000000000000000, 0.000000000000000000, -200.0000000000000000 ) ) ;
#40002 = CYLINDRICAL_SURFACE ( 'NONE', #39685, 9.999999999999998224 ) ;
#40003 = CIRCLE ( 'NONE', #11756, 5.500000000000003553 ) ;
#40004 = CARTESIAN_POINT ( 'NONE',  ( -5.405949406249996869, 9.363379034771805109, -180.8437500020483810 ) ) ;
#40005 = CARTESIAN_POINT ( 'NONE',  ( -10.81189881249999729, 1.324075727343319199E-15, -158.0937500020483810 ) ) ;
#40006 = CARTESIAN_POINT ( 'NONE',  ( -10.81189881249999907, -6.242252689847864744, -151.9687500020484094 ) ) ;
#40007 = CARTESIAN_POINT ( 'NONE',  ( -10.81189881249999729, 6.242252689847871849, -159.7187500020483810 ) ) ;
#40008 = FACE_OUTER_BOUND ( 'NONE', #22183, .T. ) ;
#40009 =( BOUNDED_CURVE ( )  B_SPLINE_CURVE ( 2, ( #13487, #12856, #20194, #13064, #26676, #13275, #26259 ),
 .UNSPECIFIED., .F., .F. ) 
 B_SPLINE_CURVE_WITH_KNOTS ( ( 3, 2, 2, 3 ),
 ( 0.1305970149253731227, 0.1318407960199005080, 0.1330845771144278378, 0.1343283582089551953 ),
 .UNSPECIFIED. ) 
 CURVE ( )  GEOMETRIC_REPRESENTATION_ITEM ( )  RATIONAL_B_SPLINE_CURVE ( ( 1.000000000000000000, 0.8660254037844387076, 1.000000000000000000, 0.8660254037844387076, 1.000000000000000000, 0.8660254037844417052, 0.9999999999999970024 ) ) 
 REPRESENTATION_ITEM ( '' )  );
#40010 = CARTESIAN_POINT ( 'NONE',  ( -9.999999999999998224, 1.224646799147353059E-15, -187.6250000040967905 ) ) ;
#40011 = CARTESIAN_POINT ( 'NONE',  ( 7.070501591499377789E-16, 11.54700538379251284, -183.1250000000000000 ) ) ;
#40012 = CARTESIAN_POINT ( 'NONE',  ( 10.81189881249999729, 0.000000000000000000, -97.34375000204838102 ) ) ;
#40013 = CARTESIAN_POINT ( 'NONE',  ( 0.000000000000000000, 0.000000000000000000, -200.0000000000000000 ) ) ;
#40014 = CARTESIAN_POINT ( 'NONE',  ( -2.293366432827344421E-15, -12.48450537969573659, -67.90625000204840944 ) ) ;
#40015 = CARTESIAN_POINT ( 'NONE',  ( -2.121150477449813534E-15, -11.54700538379251284, -97.25000000409677625 ) ) ;
#40016 = CARTESIAN_POINT ( 'NONE',  ( 10.81189881249999729, 0.000000000000000000, -184.3437500020483810 ) ) ;
#40017 = CARTESIAN_POINT ( 'NONE',  ( 5.405949406249992428, -9.363379034771808662, -118.7812500020483952 ) ) ;
#40018 = CARTESIAN_POINT ( 'NONE',  ( -10.81189881249999729, 6.242252689847871849, -162.9062500020483810 ) ) ;
#40019 = CARTESIAN_POINT ( 'NONE',  ( -5.405949406249996869, 9.363379034771805109, -56.53125000204836681 ) ) ;
#40020 = CARTESIAN_POINT ( 'NONE',  ( -2.121150477449813534E-15, -11.54700538379251284, -140.7500000040967905 ) ) ;
#40021 = CARTESIAN_POINT ( 'NONE',  ( -9.999999999999998224, 1.224646799147353059E-15, -110.7499999999999858 ) ) ;
#40022 = EDGE_CURVE ( 'NONE', #18615, #40773, #37028, .T. ) ;
#40023 = VERTEX_POINT ( 'NONE', #36395 ) ;
#40024 = CARTESIAN_POINT ( 'NONE',  ( -10.81189881249999729, 6.242252689847871849, -137.4062500020484094 ) ) ;
#40025 = CARTESIAN_POINT ( 'NONE',  ( -10.81189881249999729, 1.324075727343319199E-15, -149.2812500020483810 ) ) ;
#40026 = CARTESIAN_POINT ( 'NONE',  ( 10.81189881249999551, -6.242252689847874514, -192.1562500020484094 ) ) ;
#40027 = CARTESIAN_POINT ( 'NONE',  ( 10.81189881249999551, -6.242252689847874514, -83.96875000204838102 ) ) ;
#40028 = VERTEX_POINT ( 'NONE', #7466 ) ;
#40029 = CARTESIAN_POINT ( 'NONE',  ( 9.999999999999996447, -5.773502691896262640, -50.12499999999998579 ) ) ;
#40030 = CARTESIAN_POINT ( 'NONE',  ( 10.81189881249999551, -6.242252689847874514, -178.4687500020484094 ) ) ;
#40031 = CARTESIAN_POINT ( 'NONE',  ( 9.999999999999998224, 0.000000000000000000, -66.87500000409676204 ) ) ;
#40032 = CARTESIAN_POINT ( 'NONE',  ( -9.999999999999998224, 1.224646799147353059E-15, -101.7500000000000000 ) ) ;
#40033 = CARTESIAN_POINT ( 'NONE',  ( 4.999999999999992006, -8.660254037844389075, -175.1250000040968189 ) ) ;
#40034 = CARTESIAN_POINT ( 'NONE',  ( 10.81189881249999907, 6.242252689847868297, -73.40625000204836681 ) ) ;
#40035 = CARTESIAN_POINT ( 'NONE',  ( 5.405949406249999534, 9.363379034771803333, -56.78125000204836681 ) ) ;
#40036 = CARTESIAN_POINT ( 'NONE',  ( 9.999999999999996447, -5.773502691896262640, -55.00000000409677625 ) ) ;
#40037 = CARTESIAN_POINT ( 'NONE',  ( -5.405949406249996869, 9.363379034771805109, -11.34375000204834727 ) ) ;
#40038 = CARTESIAN_POINT ( 'NONE',  ( 0.000000000000000000, 0.000000000000000000, -200.0000000000000000 ) ) ;
#40039 = CARTESIAN_POINT ( 'NONE',  ( -10.81189881249999729, 1.324075727343319199E-15, -186.7812500020484094 ) ) ;
#40040 = CARTESIAN_POINT ( 'NONE',  ( -5.405949406249996869, 9.363379034771805109, -7.031250002048378356 ) ) ;
#40041 = CARTESIAN_POINT ( 'NONE',  ( -10.81189881249999729, 1.324075727343319199E-15, -0.5937500020483654772 ) ) ;
#40042 = DIRECTION ( 'NONE',  ( -0.08715574274765837404, 0.000000000000000000, -0.9961946980917455452 ) ) ;
#40043 = CARTESIAN_POINT ( 'NONE',  ( -9.999999999999998224, 1.224646799147353059E-15, -177.1250000040968189 ) ) ;
#40044 = CARTESIAN_POINT ( 'NONE',  ( -2.121150477449813534E-15, -11.54700538379251284, -122.3749999999999858 ) ) ;
#40046 = ORIENTED_EDGE ( 'NONE', *, *, #10620, .T. ) ;
#40045 = CARTESIAN_POINT ( 'NONE',  ( -2.293366432827344421E-15, -12.48450537969573659, -90.40625000204838102 ) ) ;
#40047 = CARTESIAN_POINT ( 'NONE',  ( 10.00000000000012257, -5.773502691896187144, -160.0000000040968189 ) ) ;
#40049 = ORIENTED_EDGE ( 'NONE', *, *, #15782, .T. ) ;
#40048 = CARTESIAN_POINT ( 'NONE',  ( -10.81189881249999729, 6.242252689847871849, -102.7187500020483810 ) ) ;
#40050 = EDGE_LOOP ( 'NONE', ( #39678, #36819, #33151, #28820, #41679, #25638, #42484, #27681 ) ) ;
#40051 = EDGE_CURVE ( 'NONE', #14981, #311, #27265, .T. ) ;
#40052 = CARTESIAN_POINT ( 'NONE',  ( 10.81189881249999551, -6.242252689847874514, -29.96875000204834549 ) ) ;
#40053 = CARTESIAN_POINT ( 'NONE',  ( -10.81189881249999729, 6.242252689847871849, -23.40625000204837747 ) ) ;
#40054 = CONTEXT_DEPENDENT_SHAPE_REPRESENTATION ( #22899, #12758 ) ;
#40055 = CARTESIAN_POINT ( 'NONE',  ( 5.405949406249999534, 9.363379034771803333, -74.59375000204838102 ) ) ;
#40056 = CARTESIAN_POINT ( 'NONE',  ( -2.121150477449813534E-15, -11.54700538379251284, -115.2500000040967905 ) ) ;
#40057 = CARTESIAN_POINT ( 'NONE',  ( 5.000000000000000000, 8.660254037844385522, -45.24999999999998579 ) ) ;
#40058 = CARTESIAN_POINT ( 'NONE',  ( 10.81189881249999551, -6.242252689847874514, -191.9687500020484379 ) ) ;
#40059 = CARTESIAN_POINT ( 'NONE',  ( -10.81189881249999729, 6.242252689847871849, -147.7187500020484094 ) ) ;
#40060 = CARTESIAN_POINT ( 'NONE',  ( -2.121150477449813534E-15, -11.54700538379251284, -121.2500000040967905 ) ) ;
#40061 = CARTESIAN_POINT ( 'NONE',  ( -9.999999999999998224, 1.224646799147353059E-15, -172.2500000000000000 ) ) ;
#40062 = CARTESIAN_POINT ( 'NONE',  ( 10.81189881249999907, 6.242252689847868297, -151.4062500020484094 ) ) ;
#40063 = CARTESIAN_POINT ( 'NONE',  ( 9.999999999999996447, -5.773502691896262640, -2.500000004096755823 ) ) ;
#40064 = LINE ( 'NONE', #10496, #14280 ) ;
#40065 = SECURITY_CLASSIFICATION ( '', '', #22395 ) ;
#40066 = CARTESIAN_POINT ( 'NONE',  ( 7.644554776091147741E-16, 12.48450537969573659, -120.9687500020483952 ) ) ;
#40067 = CYLINDRICAL_SURFACE ( 'NONE', #20390, 9.999999999999998224 ) ;
#40068 = CARTESIAN_POINT ( 'NONE',  ( -10.81189881249999729, 6.242252689847871849, -89.40625000204838102 ) ) ;
#40069 = CARTESIAN_POINT ( 'NONE',  ( -10.81189881249999729, 6.242252689847871849, -99.71875000204838102 ) ) ;
#40070 = EDGE_CURVE ( 'NONE', #18513, #24472, #789, .T. ) ;
#40071 = CARTESIAN_POINT ( 'NONE',  ( 10.81189881249999551, -6.242252689847874514, -70.46875000204839523 ) ) ;
#40072 = CARTESIAN_POINT ( 'NONE',  ( 5.405949406249999534, 9.363379034771803333, -74.78125000204838102 ) ) ;
#40073 = CARTESIAN_POINT ( 'NONE',  ( 7.070501591499377789E-16, 11.54700538379251284, -161.0000000040967905 ) ) ;
#40074 = CARTESIAN_POINT ( 'NONE',  ( -5.405949406250003975, -9.363379034771801557, -159.5312500020484094 ) ) ;
#40075 = CARTESIAN_POINT ( 'NONE',  ( -5.405949406250003975, -9.363379034771801557, -170.0312500020484094 ) ) ;
#40076 = CARTESIAN_POINT ( 'NONE',  ( -9.999999999999998224, 1.224646799147353059E-15, -184.2500000000000000 ) ) ;
#40077 = CARTESIAN_POINT ( 'NONE',  ( 10.00000000000051159, -5.773502691895965988, -145.0000000040967620 ) ) ;
#40078 = CARTESIAN_POINT ( 'NONE',  ( 9.999999999999998224, 0.000000000000000000, -195.5000000000000000 ) ) ;
#40079 = CARTESIAN_POINT ( 'NONE',  ( 7.644554776091147741E-16, 12.48450537969573659, -108.9687500020483952 ) ) ;
#40080 = CARTESIAN_POINT ( 'NONE',  ( 9.999999999999996447, -5.773502691896262640, -83.12499999999998579 ) ) ;
#40081 = CARTESIAN_POINT ( 'NONE',  ( -10.81189881249999729, 6.242252689847871849, -3.906250002048361480 ) ) ;
#40082 = CARTESIAN_POINT ( 'NONE',  ( -4.999999999999996447, 8.660254037844387298, -87.37500000409677625 ) ) ;
#40083 =( BOUNDED_CURVE ( )  B_SPLINE_CURVE ( 2, ( #26137, #9723, #33, #19858, #26562, #26349, #10146 ),
 .UNSPECIFIED., .F., .F. ) 
 B_SPLINE_CURVE_WITH_KNOTS ( ( 3, 2, 2, 3 ),
 ( 0.8544776119402988090, 0.8557213930348261943, 0.8569651741293534686, 0.8582089552238808539 ),
 .UNSPECIFIED. ) 
 CURVE ( )  GEOMETRIC_REPRESENTATION_ITEM ( )  RATIONAL_B_SPLINE_CURVE ( ( 0.9999999999999641398, 0.8660254037844745678, 1.000000000000000000, 0.8660254037844387076, 1.000000000000000000, 0.8660254037844148378, 1.000000000000023981 ) ) 
 REPRESENTATION_ITEM ( '' )  );
#40084 = CYLINDRICAL_SURFACE ( 'NONE', #38934, 9.999999999999998224 ) ;
#40085 = CARTESIAN_POINT ( 'NONE',  ( -10.81189881249999729, 6.242252689847871849, -102.9062500020483810 ) ) ;
#40086 = CARTESIAN_POINT ( 'NONE',  ( 7.644554776091147741E-16, 12.48450537969573659, -80.65625000204838102 ) ) ;
#40087 = CARTESIAN_POINT ( 'NONE',  ( -9.999999999999998224, 1.224646799147353059E-15, -73.62500000409677625 ) ) ;
#40088 = CARTESIAN_POINT ( 'NONE',  ( -9.999999999999998224, 1.224646799147353059E-15, -145.6250000040967905 ) ) ;
#40089 = CARTESIAN_POINT ( 'NONE',  ( -10.81189881249999729, 1.324075727343319199E-15, -32.09375000204836681 ) ) ;
#40090 = ORIENTED_EDGE ( 'NONE', *, *, #3754, .F. ) ;
#40091 = CARTESIAN_POINT ( 'NONE',  ( 9.999999999999998224, 0.000000000000000000, -12.49999999999995559 ) ) ;
#40092 = CARTESIAN_POINT ( 'NONE',  ( -10.81189881249999729, 1.324075727343319199E-15, -29.28125000204837036 ) ) ;
#40093 = CARTESIAN_POINT ( 'NONE',  ( -9.999999999999998224, 5.773502691896259087, -148.3750000000000000 ) ) ;
#40094 = CARTESIAN_POINT ( 'NONE',  ( -11.54700538379251817, 20.00000000000000355, 0.000000000000000000 ) ) ;
#40095 = CARTESIAN_POINT ( 'NONE',  ( -4.999999999999996447, 8.660254037844387298, -1.875000004096766260 ) ) ;
#40096 = AXIS2_PLACEMENT_3D ( 'NONE', #3451, #19418, #6272 ) ;
#40097 = CARTESIAN_POINT ( 'NONE',  ( -2.121150477449813534E-15, -11.54700538379251284, -194.3750000000000284 ) ) ;
#40098 = CARTESIAN_POINT ( 'NONE',  ( -10.00000000000025580, 5.773502691896109873, -122.8750000000000000 ) ) ;
#40100 = ORIENTED_EDGE ( 'NONE', *, *, #31744, .F. ) ;
#40099 = CARTESIAN_POINT ( 'NONE',  ( 10.81189881249999729, 0.000000000000000000, -118.5312500020483952 ) ) ;
#40101 = CARTESIAN_POINT ( 'NONE',  ( 5.000000000000000000, 8.660254037844385522, -13.74999999999995737 ) ) ;
#40102 = ORIENTED_EDGE ( 'NONE', *, *, #38051, .F. ) ;
#40103 = ORIENTED_EDGE ( 'NONE', *, *, #5361, .F. ) ;
#40104 = CARTESIAN_POINT ( 'NONE',  ( 10.81189881249999729, 0.000000000000000000, -49.53125000204838813 ) ) ;
#40105 = PERSON_AND_ORGANIZATION ( #11915, #17965 ) ;
#40106 = CARTESIAN_POINT ( 'NONE',  ( -5.405949406249996869, 9.363379034771805109, -92.34375000204838102 ) ) ;
#40107 = CARTESIAN_POINT ( 'NONE',  ( 5.405949406249999534, 9.363379034771803333, -119.7812500020483952 ) ) ;
#40108 = VERTEX_POINT ( 'NONE', #16518 ) ;
#40109 = CARTESIAN_POINT ( 'NONE',  ( 5.405949406249992428, -9.363379034771808662, -196.5937500020484094 ) ) ;
#40110 = CARTESIAN_POINT ( 'NONE',  ( -10.81189881249999907, -6.242252689847864744, -170.1562500020483810 ) ) ;
#40111 = PLANE ( 'NONE',  #41051 ) ;
#40112 = CARTESIAN_POINT ( 'NONE',  ( -5.405949406249996869, 9.363379034771805109, -120.8437500020483952 ) ) ;
#40113 = CARTESIAN_POINT ( 'NONE',  ( -10.81189881249999907, -6.242252689847864744, -94.96875000204838102 ) ) ;
#40114 = CARTESIAN_POINT ( 'NONE',  ( 5.405949406249999534, 9.363379034771803333, -199.0937500020484094 ) ) ;
#40115 = CARTESIAN_POINT ( 'NONE',  ( -10.81189881249999907, -6.242252689847864744, -101.1562500020483952 ) ) ;
#40116 = CARTESIAN_POINT ( 'NONE',  ( -5.000000000000003553, -8.660254037844383745, -182.8750000040967905 ) ) ;
#40117 = CARTESIAN_POINT ( 'NONE',  ( 5.405949406249999534, 9.363379034771803333, -104.5937500020483810 ) ) ;
#40118 = VECTOR ( 'NONE', #7287, 1000.000000000000000 ) ;
#40119 = CARTESIAN_POINT ( 'NONE',  ( -2.293366432827344421E-15, -12.48450537969573659, -180.4062500020484379 ) ) ;
#40120 =( BOUNDED_CURVE ( )  B_SPLINE_CURVE ( 2, ( #6076, #26134, #28, #19223, #3047, #39076, #19016 ),
 .UNSPECIFIED., .F., .F. ) 
 B_SPLINE_CURVE_WITH_KNOTS ( ( 3, 2, 2, 3 ),
 ( 0.4104477611940299253, 0.4116915422885572551, 0.4129353233830846959, 0.4141791044776120256 ),
 .UNSPECIFIED. ) 
 CURVE ( )  GEOMETRIC_REPRESENTATION_ITEM ( )  RATIONAL_B_SPLINE_CURVE ( ( 0.9999999999999940048, 0.8660254037844447028, 1.000000000000000000, 0.8660254037844387076, 1.000000000000000000, 0.8660254037844267172, 1.000000000000011990 ) ) 
 REPRESENTATION_ITEM ( '' )  );
#40121 = CARTESIAN_POINT ( 'NONE',  ( -2.121150477449813534E-15, -11.54700538379251284, -104.7500000040967763 ) ) ;
#40122 = CARTESIAN_POINT ( 'NONE',  ( -9.999999999999998224, 1.224646799147353059E-15, -132.1250000040967620 ) ) ;
#40123 = CARTESIAN_POINT ( 'NONE',  ( 5.405949406249999534, 9.363379034771803333, -193.2812500020484094 ) ) ;
#40124 = CARTESIAN_POINT ( 'NONE',  ( -5.405949406250003975, -9.363379034771801557, -58.84375000204835970 ) ) ;
#40125 = CARTESIAN_POINT ( 'NONE',  ( 10.81189881249999551, -6.242252689847874514, -40.46875000204835260 ) ) ;
#40126 = CARTESIAN_POINT ( 'NONE',  ( 9.999999999999998224, 0.000000000000000000, -168.8750000040967905 ) ) ;
#40127 = CARTESIAN_POINT ( 'NONE',  ( 7.644554776091147741E-16, 12.48450537969573659, -16.15625000204837747 ) ) ;
#40128 = CARTESIAN_POINT ( 'NONE',  ( 5.405949406249992428, -9.363379034771808662, -25.59375000204835970 ) ) ;
#40129 = CARTESIAN_POINT ( 'NONE',  ( -5.000000000000005329, -20.00000000000000000, -235.0000000000000000 ) ) ;
#40130 = CARTESIAN_POINT ( 'NONE',  ( 5.405949406249992428, -9.363379034771808662, -132.0937500020483810 ) ) ;
#40131 = EDGE_CURVE ( 'NONE', #12962, #41098, #38877, .T. ) ;
#40132 = CARTESIAN_POINT ( 'NONE',  ( 5.000000000000000000, 8.660254037844385522, -105.2499999999999858 ) ) ;
#40133 = CARTESIAN_POINT ( 'NONE',  ( -2.293366432827344421E-15, -12.48450537969573659, -25.90625000204838102 ) ) ;
#40134 = DIRECTION ( 'NONE',  ( 0.000000000000000000, 0.000000000000000000, -1.000000000000000000 ) ) ;
#40135 = EDGE_CURVE ( 'NONE', #40345, #6396, #4228, .T. ) ;
#40136 = CARTESIAN_POINT ( 'NONE',  ( -9.999999999999998224, 5.773502691896259087, -56.87499999999998579 ) ) ;
#40137 = CARTESIAN_POINT ( 'NONE',  ( 10.81189881249999907, 6.242252689847868297, -127.4062500020483810 ) ) ;
#40138 = CARTESIAN_POINT ( 'NONE',  ( 10.81189881249999729, 6.242252689847867408, -109.4062500020483952 ) ) ;
#40139 = ORIENTED_EDGE ( 'NONE', *, *, #34683, .F. ) ;
#40140 = CARTESIAN_POINT ( 'NONE',  ( -2.121150477449813534E-15, -11.54700538379251284, -6.874999999999968914 ) ) ;
#40141 = CARTESIAN_POINT ( 'NONE',  ( 7.070501591499377789E-16, 11.54700538379251284, -101.0000000040967905 ) ) ;
#40142 = CARTESIAN_POINT ( 'NONE',  ( -9.999999999999479527, -5.773502691896549521, -146.6249999999999716 ) ) ;
#40143 = CARTESIAN_POINT ( 'NONE',  ( 10.81189881249999907, 6.242252689847868297, -56.71875000204838813 ) ) ;
#40144 = ORIENTED_EDGE ( 'NONE', *, *, #2158, .T. ) ;
#40145 = CARTESIAN_POINT ( 'NONE',  ( -9.999999999999998224, 1.224646799147353059E-15, -37.24999999999997868 ) ) ;
#40146 = VECTOR ( 'NONE', #40980, 1000.000000000000000 ) ;
#40147 = CARTESIAN_POINT ( 'NONE',  ( -5.405949406249996869, 9.363379034771805109, -35.53125000204837391 ) ) ;
#40148 = CARTESIAN_POINT ( 'NONE',  ( -9.999999999999998224, 1.224646799147353059E-15, -36.12500000409676915 ) ) ;
#40149 = CARTESIAN_POINT ( 'NONE',  ( 7.070501591499376803E-16, 11.54700538379251284, -161.0000000040968189 ) ) ;
#40150 = CARTESIAN_POINT ( 'NONE',  ( -10.81189881249999729, 1.324075727343319199E-15, -140.2812500020483810 ) ) ;
#40151 = CARTESIAN_POINT ( 'NONE',  ( 9.999999999999479527, 5.773502691896553074, -174.7500000040967905 ) ) ;
#40152 = ORIENTED_EDGE ( 'NONE', *, *, #12373, .T. ) ;
#40153 = VERTEX_POINT ( 'NONE', #40250 ) ;
#40154 = CARTESIAN_POINT ( 'NONE',  ( -9.999999999999998224, 1.224646799147353059E-15, -113.7499999999999858 ) ) ;
#40155 = CARTESIAN_POINT ( 'NONE',  ( -8.571370657139813766E-15, 145.0000000000000000, 37.49999999999997868 ) ) ;
#40156 = CARTESIAN_POINT ( 'NONE',  ( 5.405949406249992428, -9.363379034771808662, -168.0937500020484094 ) ) ;
#40157 = CARTESIAN_POINT ( 'NONE',  ( -10.81189881249999729, 1.324075727343319199E-15, -198.7812500020484094 ) ) ;
#40158 = CARTESIAN_POINT ( 'NONE',  ( -10.81189881249999907, -6.242252689847864744, -15.46875000204835793 ) ) ;
#40159 = CARTESIAN_POINT ( 'NONE',  ( 9.999999999999998224, 0.000000000000000000, -62.37500000409676204 ) ) ;
#40160 = CARTESIAN_POINT ( 'NONE',  ( 10.81189881249999729, 0.000000000000000000, -157.3437500020483810 ) ) ;
#40161 = CARTESIAN_POINT ( 'NONE',  ( 5.405949406249992428, -9.363379034771808662, -136.5937500020483810 ) ) ;
#40162 = CARTESIAN_POINT ( 'NONE',  ( -4.999999999999996447, 8.660254037844387298, -67.49999999999997158 ) ) ;
#40163 = CARTESIAN_POINT ( 'NONE',  ( -2.293366432827344421E-15, -12.48450537969573659, -117.2187500020483952 ) ) ;
#40164 = CARTESIAN_POINT ( 'NONE',  ( 7.070501591499377789E-16, 11.54700538379251284, -197.0000000040968189 ) ) ;
#40165 = CARTESIAN_POINT ( 'NONE',  ( -5.405949406250003975, -9.363379034771801557, -125.0312500020483952 ) ) ;
#40166 = CARTESIAN_POINT ( 'NONE',  ( -10.81189881249999907, -6.242252689847864744, -12.46875000204837391 ) ) ;
#40167 = CARTESIAN_POINT ( 'NONE',  ( 10.81189881249999729, 0.000000000000000000, -142.3437500020483810 ) ) ;
#40168 = CARTESIAN_POINT ( 'NONE',  ( 7.644554776091147741E-16, 12.48450537969573659, -199.1562500020484379 ) ) ;
#40169 = CARTESIAN_POINT ( 'NONE',  ( -9.999999999999998224, 1.224646799147353059E-15, -97.24999999999998579 ) ) ;
#40170 = CARTESIAN_POINT ( 'NONE',  ( 5.000000000000000000, 8.660254037844385522, -159.2500000000000000 ) ) ;
#40171 = CARTESIAN_POINT ( 'NONE',  ( -10.00000000000000000, -5.773502691896251982, -19.12499999999997513 ) ) ;
#40172 = CARTESIAN_POINT ( 'NONE',  ( 5.405949406249992428, -9.363379034771808662, -85.59375000204836681 ) ) ;
#40173 = CARTESIAN_POINT ( 'NONE',  ( 7.644554776091147741E-16, 12.48450537969573659, -66.96875000204838102 ) ) ;
#40174 = CARTESIAN_POINT ( 'NONE',  ( -2.293366432827344421E-15, -12.48450537969573659, -45.40625000204837391 ) ) ;
#40175 = CARTESIAN_POINT ( 'NONE',  ( -5.405949406249996869, 9.363379034771805109, -45.84375000204838102 ) ) ;
#40176 = FACE_OUTER_BOUND ( 'NONE', #6517, .T. ) ;
#40177 = CARTESIAN_POINT ( 'NONE',  ( 10.81189881249999907, 6.242252689847868297, -151.2187500020483810 ) ) ;
#40178 = ADVANCED_FACE ( 'NONE', ( #30570 ), #27320, .T. ) ;
#40179 = CARTESIAN_POINT ( 'NONE',  ( 7.070501591499377789E-16, 11.54700538379251284, -129.1250000000000000 ) ) ;
#40180 = CARTESIAN_POINT ( 'NONE',  ( -5.405949406250003975, -9.363379034771801557, -129.5312500020484094 ) ) ;
#40181 = CARTESIAN_POINT ( 'NONE',  ( 1.917121039151881590, 10.12589884400897056, -180.0000000000000853 ) ) ;
#40182 = CARTESIAN_POINT ( 'NONE',  ( -4.999999999999996447, 8.660254037844387298, -82.49999999999998579 ) ) ;
#40183 = CARTESIAN_POINT ( 'NONE',  ( -5.405949406250003975, -9.363379034771801557, -17.03125000204835970 ) ) ;
#40184 = ADVANCED_FACE ( 'NONE', ( #10686 ), #39833, .F. ) ;
#40185 = ORIENTED_EDGE ( 'NONE', *, *, #2738, .F. ) ;
#40186 = CARTESIAN_POINT ( 'NONE',  ( -10.81189881249999729, 1.324075727343319199E-15, -108.7812500020483810 ) ) ;
#40187 = CARTESIAN_POINT ( 'NONE',  ( -9.999999999999998224, 1.224646799147353059E-15, -132.1250000040967620 ) ) ;
#40188 = CARTESIAN_POINT ( 'NONE',  ( 9.999999999999998224, 0.000000000000000000, -164.0000000000000000 ) ) ;
#40189 = EDGE_CURVE ( 'NONE', #29348, #23986, #27534, .T. ) ;
#40190 = CARTESIAN_POINT ( 'NONE',  ( 9.999999999999996447, -5.773502691896262640, -41.50000000409674783 ) ) ;
#40191 = CARTESIAN_POINT ( 'NONE',  ( 9.999999999999998224, 0.000000000000000000, -68.37500000409677625 ) ) ;
#40192 = APPROVAL ( #14887, 'UNSPECIFIED' ) ;
#40193 = CARTESIAN_POINT ( 'NONE',  ( -10.81189881249999729, 1.324075727343319199E-15, -51.78125000204835970 ) ) ;
#40194 = CARTESIAN_POINT ( 'NONE',  ( -9.999999999999998224, 1.224646799147353059E-15, -76.24999999999998579 ) ) ;
#40195 = CARTESIAN_POINT ( 'NONE',  ( 10.81189881249999907, 6.242252689847868297, -149.9062500020484094 ) ) ;
#40196 = CARTESIAN_POINT ( 'NONE',  ( 10.81189881249999907, 6.242252689847868297, -139.2187500020484094 ) ) ;
#40197 = CARTESIAN_POINT ( 'NONE',  ( 9.999999999999998224, 0.000000000000000000, -195.5000000000000000 ) ) ;
#40198 = ADVANCED_FACE ( 'NONE', ( #7047 ), #3809, .T. ) ;
#40199 = VERTEX_POINT ( 'NONE', #581 ) ;
#40200 = DIRECTION ( 'NONE',  ( -0.000000000000000000, -0.000000000000000000, 1.000000000000000000 ) ) ;
#40202 = ORIENTED_EDGE ( 'NONE', *, *, #33406, .T. ) ;
#40201 = CARTESIAN_POINT ( 'NONE',  ( -10.81189881249999907, -6.242252689847864744, -60.65625000204840234 ) ) ;
#40203 = APPROVAL_DATE_TIME ( #1971, #19877 ) ;
#40205 = ORIENTED_EDGE ( 'NONE', *, *, #18829, .T. ) ;
#40204 = CARTESIAN_POINT ( 'NONE',  ( 10.81189881249999907, 6.242252689847868297, -115.2187500020483810 ) ) ;
#40206 =( BOUNDED_CURVE ( )  B_SPLINE_CURVE ( 2, ( #27741, #10678, #41086, #17793, #11529, #30990, #23871 ),
 .UNSPECIFIED., .F., .F. ) 
 B_SPLINE_CURVE_WITH_KNOTS ( ( 3, 2, 2, 3 ),
 ( 0.8395522388059704078, 0.8407960199004976820, 0.8420398009950251783, 0.8432835820895525636 ),
 .UNSPECIFIED. ) 
 CURVE ( )  GEOMETRIC_REPRESENTATION_ITEM ( )  RATIONAL_B_SPLINE_CURVE ( ( 0.9999999999999761302, 0.8660254037844625774, 1.000000000000000000, 0.8660254037844387076, 1.000000000000000000, 0.8660254037844028474, 1.000000000000035971 ) ) 
 REPRESENTATION_ITEM ( '' )  );
#40207 = CARTESIAN_POINT ( 'NONE',  ( 5.405949406249999534, 9.363379034771803333, -20.59375000204835615 ) ) ;
#40208 = CARTESIAN_POINT ( 'NONE',  ( -2.293366432827344421E-15, -12.48450537969573659, -193.7187500020484094 ) ) ;
#40209 = CARTESIAN_POINT ( 'NONE',  ( 5.405949406249999534, 9.363379034771803333, -47.59375000204838102 ) ) ;
#40210 = CARTESIAN_POINT ( 'NONE',  ( 10.81189881249999729, 0.000000000000000000, -181.3437500020483810 ) ) ;
#40211 = CARTESIAN_POINT ( 'NONE',  ( 5.405949406249992428, -9.363379034771808662, -162.0937500020484094 ) ) ;
#40212 = CARTESIAN_POINT ( 'NONE',  ( 5.405949406249999534, 9.363379034771803333, -142.0937500020483810 ) ) ;
#40213 = CARTESIAN_POINT ( 'NONE',  ( 10.81189881249999551, -6.242252689847874514, -158.9687500020484094 ) ) ;
#40214 = CARTESIAN_POINT ( 'NONE',  ( -5.500000000000005329, -20.00000000000000000, -232.0000000000000000 ) ) ;
#40215 = CARTESIAN_POINT ( 'NONE',  ( 0.000000000000000000, 0.000000000000000000, -200.0000000000000000 ) ) ;
#40216 = CARTESIAN_POINT ( 'NONE',  ( -9.999999999999998224, 1.224646799147353059E-15, -182.7500000000000000 ) ) ;
#40217 = CARTESIAN_POINT ( 'NONE',  ( -2.293366432827344421E-15, -12.48450537969573659, -88.71875000204838102 ) ) ;
#40218 = CARTESIAN_POINT ( 'NONE',  ( -10.00000000000076916, 5.773502691895813221, -137.8750000000000000 ) ) ;
#40219 = CARTESIAN_POINT ( 'NONE',  ( -10.81189881249999729, 6.242252689847871849, -69.90625000204839523 ) ) ;
#40220 = DIRECTION ( 'NONE',  ( -1.000000000000000000, 0.000000000000000000, 0.000000000000000000 ) ) ;
#40221 = CARTESIAN_POINT ( 'NONE',  ( 10.81189881249999907, 6.242252689847868297, -175.2187500020484094 ) ) ;
#40222 = CARTESIAN_POINT ( 'NONE',  ( -10.81189881249999907, -6.242252689847864744, -123.6562500020484094 ) ) ;
#40223 = CARTESIAN_POINT ( 'NONE',  ( -10.81189881249999729, 1.324075727343319199E-15, -165.7812500020484094 ) ) ;
#40224 = CARTESIAN_POINT ( 'NONE',  ( 5.405949406249999534, 9.363379034771803333, -53.78125000204836681 ) ) ;
#40225 = CARTESIAN_POINT ( 'NONE',  ( 5.000000000000000000, 8.660254037844385522, -131.1250000040967620 ) ) ;
#40226 = CARTESIAN_POINT ( 'NONE',  ( -10.00000000000000000, -5.773502691896251982, -106.1249999999999858 ) ) ;
#40227 = ORIENTED_EDGE ( 'NONE', *, *, #9361, .T. ) ;
#40228 = CARTESIAN_POINT ( 'NONE',  ( 5.405949406249999534, 9.363379034771803333, -133.2812500020483810 ) ) ;
#40229 = CARTESIAN_POINT ( 'NONE',  ( 5.405949406249999534, 9.363379034771803333, -148.2812500020483810 ) ) ;
#40230 = CARTESIAN_POINT ( 'NONE',  ( 5.405949406249992428, -9.363379034771808662, -186.2812500020484094 ) ) ;
#40231 = CARTESIAN_POINT ( 'NONE',  ( 10.81189881249999907, 6.242252689847868297, -83.71875000204836681 ) ) ;
#40232 = ORIENTED_EDGE ( 'NONE', *, *, #38083, .F. ) ;
#40233 = CARTESIAN_POINT ( 'NONE',  ( -9.999999999999998224, 1.224646799147353059E-15, -50.74999999999996447 ) ) ;
#40234 = CARTESIAN_POINT ( 'NONE',  ( -5.405949406250003975, -9.363379034771801557, -177.3437500020483810 ) ) ;
#40235 = CARTESIAN_POINT ( 'NONE',  ( -2.121150477449813534E-15, -11.54700538379251284, -62.75000000409679046 ) ) ;
#40236 = CARTESIAN_POINT ( 'NONE',  ( -9.999999999999998224, 1.224646799147353059E-15, -178.6250000040968189 ) ) ;
#40237 = CARTESIAN_POINT ( 'NONE',  ( -2.293366432827344421E-15, -12.48450537969573659, -76.90625000204839523 ) ) ;
#40238 = CARTESIAN_POINT ( 'NONE',  ( -5.405949406250003975, -9.363379034771801557, -59.03125000204836681 ) ) ;
#40239 = CARTESIAN_POINT ( 'NONE',  ( -10.00000000000000000, -5.773502691896251982, -55.50000000409676915 ) ) ;
#40240 = CARTESIAN_POINT ( 'NONE',  ( -2.293366432827344421E-15, -12.48450537969573659, -9.218750002048359704 ) ) ;
#40241 = CARTESIAN_POINT ( 'NONE',  ( -9.999999999999998224, 1.224646799147353059E-15, -88.24999999999998579 ) ) ;
#40242 = CARTESIAN_POINT ( 'NONE',  ( 10.81189881249999551, -6.242252689847874514, -180.1562500020484379 ) ) ;
#40243 = EDGE_CURVE ( 'NONE', #4916, #3061, #13698, .T. ) ;
#40244 = CARTESIAN_POINT ( 'NONE',  ( 7.644554776091147741E-16, 12.48450537969573659, -2.656250002048360592 ) ) ;
#40245 = DIRECTION ( 'NONE',  ( 1.000000000000000000, 0.000000000000000000, 0.000000000000000000 ) ) ;
#40246 = CARTESIAN_POINT ( 'NONE',  ( 9.999999999999998224, 0.000000000000000000, -165.5000000000000000 ) ) ;
#40247 = CARTESIAN_POINT ( 'NONE',  ( -4.999999999999996447, 8.660254037844387298, -154.5000000000000000 ) ) ;
#40248 = CARTESIAN_POINT ( 'NONE',  ( 9.999999999999998224, 0.000000000000000000, -200.0000000000000000 ) ) ;
#40249 =( BOUNDED_CURVE ( )  B_SPLINE_CURVE ( 2, ( #41080, #37658, #8098, #21249, #17998, #14757, #19078 ),
 .UNSPECIFIED., .F., .F. ) 
 B_SPLINE_CURVE_WITH_KNOTS ( ( 3, 2, 2, 3 ),
 ( 0.3134328358208955390, 0.3146766169154229242, 0.3159203980099503650, 0.3171641791044778058 ),
 .UNSPECIFIED. ) 
 CURVE ( )  GEOMETRIC_REPRESENTATION_ITEM ( )  RATIONAL_B_SPLINE_CURVE ( ( 1.000000000000000000, 0.8660254037844387076, 1.000000000000000000, 0.8660254037844387076, 1.000000000000000000, 0.8660254037844207220, 1.000000000000017986 ) ) 
 REPRESENTATION_ITEM ( '' )  );
#40250 = CARTESIAN_POINT ( 'NONE',  ( 9.999999999999998224, 0.000000000000000000, -165.5000000000000000 ) ) ;
#40252 = ORIENTED_EDGE ( 'NONE', *, *, #35728, .F. ) ;
#40251 = CARTESIAN_POINT ( 'NONE',  ( -10.81189881249999907, -6.242252689847864744, -84.65625000204836681 ) ) ;
#40254 = ORIENTED_EDGE ( 'NONE', *, *, #26163, .F. ) ;
#40253 = CARTESIAN_POINT ( 'NONE',  ( 7.070501591499376803E-16, 11.54700538379251284, -81.12500000000000000 ) ) ;
#40255 = ORIENTED_EDGE ( 'NONE', *, *, #18282, .F. ) ;
#40256 = CARTESIAN_POINT ( 'NONE',  ( -10.81189881249999729, 1.324075727343319199E-15, -26.09375000204835970 ) ) ;
#40257 = CARTESIAN_POINT ( 'NONE',  ( 10.81189881249999551, -6.242252689847874514, -16.65625000204837747 ) ) ;
#40258 =( BOUNDED_CURVE ( )  B_SPLINE_CURVE ( 2, ( #26826, #14053, #4160, #36747, #17305, #26404, #6758 ),
 .UNSPECIFIED., .F., .F. ) 
 B_SPLINE_CURVE_WITH_KNOTS ( ( 3, 2, 2, 3 ),
 ( 0.4365671641791046276, 0.4378109452736320129, 0.4390547263681593981, 0.4402985074626867279 ),
 .UNSPECIFIED. ) 
 CURVE ( )  GEOMETRIC_REPRESENTATION_ITEM ( )  RATIONAL_B_SPLINE_CURVE ( ( 0.9999999999999820144, 0.8660254037844566932, 1.000000000000000000, 0.8660254037844387076, 1.000000000000000000, 0.8660254037844207220, 1.000000000000017986 ) ) 
 REPRESENTATION_ITEM ( '' )  );
#40259 = CARTESIAN_POINT ( 'NONE',  ( -10.81189881249999729, 1.324075727343319199E-15, -74.09375000204838102 ) ) ;
#40260 = CARTESIAN_POINT ( 'NONE',  ( 9.999999999999998224, 0.000000000000000000, -164.3750000040967905 ) ) ;
#40261 = CARTESIAN_POINT ( 'NONE',  ( 5.000000000000000000, 8.660254037844385522, -42.24999999999997868 ) ) ;
#40262 = CARTESIAN_POINT ( 'NONE',  ( 5.405949406249999534, 9.363379034771803333, -187.0937500020483810 ) ) ;
#40263 = CARTESIAN_POINT ( 'NONE',  ( 10.81189881249999907, 6.242252689847868297, -164.7187500020483810 ) ) ;
#40264 = CARTESIAN_POINT ( 'NONE',  ( 5.000000000000000000, 8.660254037844385522, -175.7500000000000284 ) ) ;
#40265 = LINE ( 'NONE', #4029, #8138 ) ;
#40266 = CARTESIAN_POINT ( 'NONE',  ( 4.999999999999992006, -8.660254037844389075, -167.6250000040967905 ) ) ;
#40267 = CARTESIAN_POINT ( 'NONE',  ( -4.999999999999996447, 8.660254037844387298, -144.0000000000000000 ) ) ;
#40268 = DIRECTION ( 'NONE',  ( -0.000000000000000000, -0.000000000000000000, 1.000000000000000000 ) ) ;
#40269 = CARTESIAN_POINT ( 'NONE',  ( 5.405949406249992428, -9.363379034771808662, -117.0937500020483810 ) ) ;
#40270 = LINE ( 'NONE', #23904, #36937 ) ;
#40271 = CARTESIAN_POINT ( 'NONE',  ( 7.644554776091147741E-16, 12.48450537969573659, -92.65625000204839523 ) ) ;
#40272 = CARTESIAN_POINT ( 'NONE',  ( -5.405949406250003975, -9.363379034771801557, -96.34375000204838102 ) ) ;
#40273 = CARTESIAN_POINT ( 'NONE',  ( -10.81189881249999729, 1.324075727343319199E-15, -71.09375000204836681 ) ) ;
#40274 = CARTESIAN_POINT ( 'NONE',  ( 10.81189881249999729, 0.000000000000000000, -79.53125000204838102 ) ) ;
#40275 = CARTESIAN_POINT ( 'NONE',  ( -2.121150477449813534E-15, -11.54700538379251284, -164.7500000040967620 ) ) ;
#40276 = CARTESIAN_POINT ( 'NONE',  ( -2.293366432827344421E-15, -12.48450537969573659, -156.4062500020484379 ) ) ;
#40277 = CARTESIAN_POINT ( 'NONE',  ( -5.405949406250003975, -9.363379034771801557, -173.0312500020484094 ) ) ;
#40278 = CARTESIAN_POINT ( 'NONE',  ( -5.405949406250003975, -9.363379034771801557, -0.3437500020483652552 ) ) ;
#40279 = CARTESIAN_POINT ( 'NONE',  ( 9.999999999999998224, 1.224646799147353059E-15, -99.99999999999998579 ) ) ;
#40280 = CARTESIAN_POINT ( 'NONE',  ( -5.405949406249996869, 9.363379034771805109, -108.8437500020483810 ) ) ;
#40281 = CYLINDRICAL_SURFACE ( 'NONE', #40353, 9.999999999999998224 ) ;
#40282 = CARTESIAN_POINT ( 'NONE',  ( 10.00000000000000000, 5.773502691896255534, -73.87499999999995737 ) ) ;
#40283 = CARTESIAN_POINT ( 'NONE',  ( -10.81189881249999907, -6.242252689847864744, -6.656250002048364145 ) ) ;
#40284 = CARTESIAN_POINT ( 'NONE',  ( -10.00000000000000000, -5.773502691896251982, -91.50000000409677625 ) ) ;
#40285 = CARTESIAN_POINT ( 'NONE',  ( 9.999999999999994671, -5.773502691896262640, -171.6250000000000000 ) ) ;
#40286 = CARTESIAN_POINT ( 'NONE',  ( -2.293366432827344421E-15, -12.48450537969573659, -99.40625000204839523 ) ) ;
#40287 = CARTESIAN_POINT ( 'NONE',  ( -5.405949406249996869, 9.363379034771805109, -83.53125000204838102 ) ) ;
#40288 = CARTESIAN_POINT ( 'NONE',  ( -4.999999999999996447, 8.660254037844387298, -76.87500000409677625 ) ) ;
#40289 = CARTESIAN_POINT ( 'NONE',  ( 7.070501591499376803E-16, 11.54700538379251284, -21.12499999999997513 ) ) ;
#40290 = CARTESIAN_POINT ( 'NONE',  ( 5.405949406249992428, -9.363379034771808662, -36.09375000204836681 ) ) ;
#40291 = ORIENTED_EDGE ( 'NONE', *, *, #42405, .T. ) ;
#40292 = CARTESIAN_POINT ( 'NONE',  ( -2.121150477449813534E-15, -11.54700538379251284, -12.87499999999996447 ) ) ;
#40293 = CARTESIAN_POINT ( 'NONE',  ( 10.81189881249999907, 6.242252689847868297, -31.40625000204835615 ) ) ;
#40294 = CARTESIAN_POINT ( 'NONE',  ( -10.81189881249999729, -6.242252689847864744, -9.468750002048361480 ) ) ;
#40295 = CARTESIAN_POINT ( 'NONE',  ( -10.00000000000000000, -5.773502691896251982, -6.000000004096756712 ) ) ;
#40296 = CARTESIAN_POINT ( 'NONE',  ( 5.405949406249992428, -9.363379034771808662, -139.7812500020483810 ) ) ;
#40297 = AXIS2_PLACEMENT_3D ( 'NONE', #31625, #7885, #1627 ) ;
#40298 = CARTESIAN_POINT ( 'NONE',  ( -5.000000000000003553, -8.660254037844383745, -187.0000000000000000 ) ) ;
#40299 = FACE_OUTER_BOUND ( 'NONE', #2055, .T. ) ;
#40301 = VERTEX_POINT ( 'NONE', #36814 ) ;
#40300 = CARTESIAN_POINT ( 'NONE',  ( 5.405949406249992428, -9.363379034771808662, -112.7812500020483952 ) ) ;
#40302 = LINE ( 'NONE', #13337, #22805 ) ;
#40303 = ORIENTED_EDGE ( 'NONE', *, *, #9375, .F. ) ;
#40304 = ORIENTED_EDGE ( 'NONE', *, *, #17490, .F. ) ;
#40305 = ADVANCED_FACE ( 'NONE', ( #7254 ), #19982, .T. ) ;
#40306 = CARTESIAN_POINT ( 'NONE',  ( -5.405949406250003975, -9.363379034771801557, -45.53125000204838102 ) ) ;
#40307 = CALENDAR_DATE ( 2026, 28, 9 ) ;
#40308 = CARTESIAN_POINT ( 'NONE',  ( 10.81189881249999729, 0.000000000000000000, -97.34375000204838102 ) ) ;
#40309 = CARTESIAN_POINT ( 'NONE',  ( 4.999999999999992006, -8.660254037844389075, -167.2500000000000000 ) ) ;
#40310 = CARTESIAN_POINT ( 'NONE',  ( -9.999999999999998224, 1.224646799147353059E-15, -19.24999999999996092 ) ) ;
#40311 = AXIS2_PLACEMENT_3D ( 'NONE', #33463, #37320, #10977 ) ;
#40312 = CARTESIAN_POINT ( 'NONE',  ( 5.405949406249992428, -9.363379034771808662, -193.5937500020484094 ) ) ;
#40313 = CARTESIAN_POINT ( 'NONE',  ( -5.405949406250003975, -9.363379034771801557, -173.0312500020484094 ) ) ;
#40314 = CARTESIAN_POINT ( 'NONE',  ( 9.999999999999998224, 0.000000000000000000, -138.5000000000000000 ) ) ;
#40315 = CARTESIAN_POINT ( 'NONE',  ( 10.81189881249999729, 6.242252689847867408, -125.7187500020483810 ) ) ;
#40316 =( BOUNDED_CURVE ( )  B_SPLINE_CURVE ( 2, ( #8829, #21775, #1935, #8619, #35163, #5163, #41820 ),
 .UNSPECIFIED., .F., .F. ) 
 B_SPLINE_CURVE_WITH_KNOTS ( ( 3, 2, 2, 3 ),
 ( 0.4776119402985076756, 0.4788557213930350054, 0.4800995024875623352, 0.4813432835820896649 ),
 .UNSPECIFIED. ) 
 CURVE ( )  GEOMETRIC_REPRESENTATION_ITEM ( )  RATIONAL_B_SPLINE_CURVE ( ( 0.9999999999999761302, 0.8660254037844625774, 1.000000000000000000, 0.8660254037844387076, 1.000000000000000000, 0.8660254037844267172, 1.000000000000011990 ) ) 
 REPRESENTATION_ITEM ( '' )  );
#40317 = CARTESIAN_POINT ( 'NONE',  ( -10.81189881249999729, 6.242252689847871849, -95.21875000204838102 ) ) ;
#40318 = FACE_OUTER_BOUND ( 'NONE', #8278, .T. ) ;
#40319 = CARTESIAN_POINT ( 'NONE',  ( 5.405949406249992428, -9.363379034771808662, -100.7812500020483952 ) ) ;
#40320 = CARTESIAN_POINT ( 'NONE',  ( -9.999999999999998224, 1.224646799147353059E-15, -187.6250000040967905 ) ) ;
#40321 = CARTESIAN_POINT ( 'NONE',  ( 5.405949406249992428, -9.363379034771808662, -108.0937500020483810 ) ) ;
#40322 = CARTESIAN_POINT ( 'NONE',  ( 10.81189881249999729, 6.242252689847867408, -178.4062500020484094 ) ) ;
#40323 = AXIS2_PLACEMENT_3D ( 'NONE', #23158, #36321, #17723 ) ;
#40324 = CARTESIAN_POINT ( 'NONE',  ( 9.999999999999612754, 5.773502691896477579, -180.3750000000000000 ) ) ;
#40325 = CARTESIAN_POINT ( 'NONE',  ( 9.999999999999998224, 0.000000000000000000, -132.8750000040967905 ) ) ;
#40326 = CARTESIAN_POINT ( 'NONE',  ( -10.81189881249999729, 1.324075727343319199E-15, -195.7812500020484094 ) ) ;
#40327 = CARTESIAN_POINT ( 'NONE',  ( -2.293366432827344421E-15, -12.48450537969573659, -55.71875000204837391 ) ) ;
#40328 = CARTESIAN_POINT ( 'NONE',  ( 5.405949406249999534, 9.363379034771803333, -38.59375000204837391 ) ) ;
#40329 = CARTESIAN_POINT ( 'NONE',  ( 9.999999999999996447, -5.773502691896262640, -172.0000000040967905 ) ) ;
#40330 = CARTESIAN_POINT ( 'NONE',  ( 10.81189881249999729, 0.000000000000000000, -7.531250002048350822 ) ) ;
#40331 = CARTESIAN_POINT ( 'NONE',  ( 10.81189881249999907, 6.242252689847868297, -23.71875000204837036 ) ) ;
#40332 = CYLINDRICAL_SURFACE ( 'NONE', #2686, 9.999999999999998224 ) ;
#40333 = CARTESIAN_POINT ( 'NONE',  ( -5.405949406250003975, -9.363379034771801557, -132.3437500020484094 ) ) ;
#40334 = CARTESIAN_POINT ( 'NONE',  ( -9.999999999999998224, 1.224646799147353059E-15, -95.74999999999998579 ) ) ;
#40335 = CARTESIAN_POINT ( 'NONE',  ( -10.81189881249999729, 6.242252689847871849, -32.40625000204835970 ) ) ;
#40336 = CARTESIAN_POINT ( 'NONE',  ( 5.000000000000000000, 8.660254037844385522, -102.2500000000000000 ) ) ;
#40337 = CARTESIAN_POINT ( 'NONE',  ( 4.999999999999992006, -8.660254037844389075, -56.24999999999996447 ) ) ;
#40338 = CARTESIAN_POINT ( 'NONE',  ( 10.81189881249999907, 6.242252689847868297, -124.4062500020483810 ) ) ;
#40339 = CARTESIAN_POINT ( 'NONE',  ( 10.81189881249999551, -6.242252689847874514, -105.1562500020483810 ) ) ;
#40340 = ORIENTED_EDGE ( 'NONE', *, *, #31655, .T. ) ;
#40341 = CARTESIAN_POINT ( 'NONE',  ( -9.999999999999998224, 1.224646799147353059E-15, -200.0000000000000000 ) ) ;
#40342 = CARTESIAN_POINT ( 'NONE',  ( -5.000000000000003553, -8.660254037844383745, -103.3750000040967763 ) ) ;
#40343 = CARTESIAN_POINT ( 'NONE',  ( -9.999999999999872102, -5.773502691896326589, -166.5000000040967905 ) ) ;
#40344 = CARTESIAN_POINT ( 'NONE',  ( 7.644554776091147741E-16, 12.48450537969573659, -60.96875000204838102 ) ) ;
#40345 = VERTEX_POINT ( 'NONE', #17579 ) ;
#40346 = CARTESIAN_POINT ( 'NONE',  ( -4.999999999999996447, 8.660254037844387298, -34.49999999999997158 ) ) ;
#40347 = CARTESIAN_POINT ( 'NONE',  ( -10.81189881249999729, -6.242252689847864744, -33.65625000204836681 ) ) ;
#40348 = CARTESIAN_POINT ( 'NONE',  ( 9.999999999999998224, 0.000000000000000000, -1.999999999999973799 ) ) ;
#40349 = CARTESIAN_POINT ( 'NONE',  ( 9.999999999999998224, 0.000000000000000000, -24.87500000409675849 ) ) ;
#40350 = VECTOR ( 'NONE', #30466, 1000.000000000000000 ) ;
#40351 = CARTESIAN_POINT ( 'NONE',  ( -2.121150477449813534E-15, -11.54700538379251284, -138.8750000000000000 ) ) ;
#40352 = CARTESIAN_POINT ( 'NONE',  ( -2.293366432827344421E-15, -12.48450537969573659, -138.4062500020483810 ) ) ;
#40353 = AXIS2_PLACEMENT_3D ( 'NONE', #37059, #21082, #13945 ) ;
#40354 = CARTESIAN_POINT ( 'NONE',  ( 7.070501591499376803E-16, 11.54700538379251284, -162.5000000040967905 ) ) ;
#40355 = ORIENTED_EDGE ( 'NONE', *, *, #27800, .T. ) ;
#40356 = EDGE_CURVE ( 'NONE', #42118, #2342, #17049, .T. ) ;
#40357 = ORIENTED_EDGE ( 'NONE', *, *, #486, .F. ) ;
#40358 = CARTESIAN_POINT ( 'NONE',  ( 0.000000000000000000, 0.000000000000000000, -200.0000000000000000 ) ) ;
#40359 =( BOUNDED_CURVE ( )  B_SPLINE_CURVE ( 2, ( #18912, #25820, #29266, #35332, #3152, #5759, #19535 ),
 .UNSPECIFIED., .F., .F. ) 
 B_SPLINE_CURVE_WITH_KNOTS ( ( 3, 2, 2, 3 ),
 ( 0.4701492537313434195, 0.4713930348258707492, 0.4726368159203981900, 0.4738805970149255198 ),
 .UNSPECIFIED. ) 
 CURVE ( )  GEOMETRIC_REPRESENTATION_ITEM ( )  RATIONAL_B_SPLINE_CURVE ( ( 0.9999999999999880096, 0.8660254037844506980, 1.000000000000000000, 0.8660254037844387076, 1.000000000000000000, 0.8660254037844207220, 1.000000000000017986 ) ) 
 REPRESENTATION_ITEM ( '' )  );
#40360 = CARTESIAN_POINT ( 'NONE',  ( 10.81189881249999907, 6.242252689847868297, -167.7187500020483810 ) ) ;
#40361 = CARTESIAN_POINT ( 'NONE',  ( 10.81189881249999551, -6.242252689847874514, -195.1562500020484379 ) ) ;
#40362 = CARTESIAN_POINT ( 'NONE',  ( 10.81189881249999907, 6.242252689847868297, -13.21875000204836148 ) ) ;
#40363 = CARTESIAN_POINT ( 'NONE',  ( 0.000000000000000000, 0.000000000000000000, -200.0000000000000000 ) ) ;
#40364 = CARTESIAN_POINT ( 'NONE',  ( -10.81189881249999729, 6.242252689847871849, -147.7187500020484094 ) ) ;
#40365 = CARTESIAN_POINT ( 'NONE',  ( 7.644554776091147741E-16, 12.48450537969573659, -140.4687500020483810 ) ) ;
#40366 = CARTESIAN_POINT ( 'NONE',  ( -5.405949406250003975, -9.363379034771801557, -102.5312500020483952 ) ) ;
#40367 = CARTESIAN_POINT ( 'NONE',  ( 7.644554776091147741E-16, 12.48450537969573659, -117.9687500020483668 ) ) ;
#40368 = CARTESIAN_POINT ( 'NONE',  ( -9.999999999999998224, 1.224646799147353059E-15, -193.6250000040967905 ) ) ;
#40369 = CARTESIAN_POINT ( 'NONE',  ( 5.405949406249992428, -9.363379034771808662, -124.7812500020483952 ) ) ;
#40370 = CARTESIAN_POINT ( 'NONE',  ( 10.81189881249999907, 6.242252689847868297, -10.21875000204836326 ) ) ;
#40371 = CARTESIAN_POINT ( 'NONE',  ( -10.81189881249999729, 1.324075727343319199E-15, -126.5937500020483668 ) ) ;
#40372 = DIRECTION ( 'NONE',  ( -0.000000000000000000, -0.000000000000000000, 1.000000000000000000 ) ) ;
#40373 = CARTESIAN_POINT ( 'NONE',  ( -2.121150477449813534E-15, -11.54700538379251284, -155.3750000000000000 ) ) ;
#40374 = CARTESIAN_POINT ( 'NONE',  ( -2.121150477449813534E-15, -11.54700538379251284, -21.87499999999997868 ) ) ;
#40375 = CARTESIAN_POINT ( 'NONE',  ( -5.405949406249996869, 9.363379034771805109, -86.34375000204836681 ) ) ;
#40376 = CARTESIAN_POINT ( 'NONE',  ( 7.644554776091147741E-16, 12.48450537969573659, -62.46875000204839523 ) ) ;
#40377 = CARTESIAN_POINT ( 'NONE',  ( 0.000000000000000000, 0.000000000000000000, -99.99999999999998579 ) ) ;
#40378 = CARTESIAN_POINT ( 'NONE',  ( 10.81189881249999551, -6.242252689847874514, -33.15625000204835970 ) ) ;
#40379 = CARTESIAN_POINT ( 'NONE',  ( 10.81189881249999729, 0.000000000000000000, -43.34375000204837391 ) ) ;
#40380 = DIRECTION ( 'NONE',  ( -0.000000000000000000, -0.000000000000000000, 1.000000000000000000 ) ) ;
#40381 = CARTESIAN_POINT ( 'NONE',  ( 5.405949406249992428, -9.363379034771808662, -153.0937500020483810 ) ) ;
#40382 = CARTESIAN_POINT ( 'NONE',  ( 4.999999999999992006, -8.660254037844389075, -128.2499999999999716 ) ) ;
#40383 = CARTESIAN_POINT ( 'NONE',  ( 7.644554776091147741E-16, 12.48450537969573659, -130.1562500020483810 ) ) ;
#40384 = CARTESIAN_POINT ( 'NONE',  ( -4.999999999999996447, 8.660254037844387298, -80.99999999999998579 ) ) ;
#40385 = CARTESIAN_POINT ( 'NONE',  ( 5.405949406249999534, 9.363379034771803333, -19.28125000204835970 ) ) ;
#40386 = ORIENTED_EDGE ( 'NONE', *, *, #40453, .T. ) ;
#40387 = CARTESIAN_POINT ( 'NONE',  ( -10.81189881249999729, 6.242252689847871849, -107.4062500020483668 ) ) ;
#40388 = CARTESIAN_POINT ( 'NONE',  ( 5.000000000000000000, 8.660254037844385522, -125.1250000040967620 ) ) ;
#40389 = CARTESIAN_POINT ( 'NONE',  ( -9.999999999999998224, 1.224646799147353059E-15, -30.12500000409676204 ) ) ;
#40390 = FACE_OUTER_BOUND ( 'NONE', #17351, .T. ) ;
#40391 = CARTESIAN_POINT ( 'NONE',  ( -10.81189881249999729, 6.242252689847871849, -54.90625000204837391 ) ) ;
#40392 = CARTESIAN_POINT ( 'NONE',  ( 4.999999999999992006, -8.660254037844389075, -146.2500000000000000 ) ) ;
#40393 = CARTESIAN_POINT ( 'NONE',  ( -10.81189881249999729, 1.324075727343319199E-15, -150.7812500020483810 ) ) ;
#40394 = CARTESIAN_POINT ( 'NONE',  ( -10.81189881249999729, 6.242252689847871849, -138.7187500020483810 ) ) ;
#40395 = CARTESIAN_POINT ( 'NONE',  ( -10.00000000000102496, 5.773502691895664007, -3.250000004096733619 ) ) ;
#40396 = VERTEX_POINT ( 'NONE', #34872 ) ;
#40397 = CARTESIAN_POINT ( 'NONE',  ( 7.070501591499376803E-16, 11.54700538379251284, -164.0000000040967905 ) ) ;
#40398 = EDGE_LOOP ( 'NONE', ( #1309, #36156 ) ) ;
#40399 = ORIENTED_EDGE ( 'NONE', *, *, #27555, .T. ) ;
#40400 = APPROVAL_DATE_TIME ( #14068, #5916 ) ;
#40401 = EDGE_CURVE ( 'NONE', #18552, #40567, #33337, .T. ) ;
#40403 = VERTEX_POINT ( 'NONE', #1640 ) ;
#40402 = CARTESIAN_POINT ( 'NONE',  ( 5.405949406249999534, 9.363379034771803333, -109.0937500020483810 ) ) ;
#40404 = ADVANCED_FACE ( 'NONE', ( #14557 ), #41315, .T. ) ;
#40405 = EDGE_CURVE ( 'NONE', #4880, #10744, #9629, .T. ) ;
#40406 = CARTESIAN_POINT ( 'NONE',  ( -10.00000000000051337, 5.773502691895962435, -103.3749999999999858 ) ) ;
#40407 = CARTESIAN_POINT ( 'NONE',  ( 10.81189881249999907, 6.242252689847868297, -193.2187500020484094 ) ) ;
#40408 = CARTESIAN_POINT ( 'NONE',  ( 5.405949406249999534, 9.363379034771803333, -35.59375000204836681 ) ) ;
#40409 = CARTESIAN_POINT ( 'NONE',  ( -2.129899540880850761, -10.13128953862508652, 1.243155832063081174E-14 ) ) ;
#40410 = DIRECTION ( 'NONE',  ( -0.000000000000000000, -0.000000000000000000, -1.000000000000000000 ) ) ;
#40411 = CARTESIAN_POINT ( 'NONE',  ( -5.405949406249996869, 9.363379034771805109, -170.3437500020484094 ) ) ;
#40412 = CARTESIAN_POINT ( 'NONE',  ( 10.81189881249999907, 6.242252689847868297, -158.7187500020483810 ) ) ;
#40413 = CC_DESIGN_DATE_AND_TIME_ASSIGNMENT ( #35987, #19563, ( #37345 ) ) ;
#40414 = CARTESIAN_POINT ( 'NONE',  ( -2.121150477449813534E-15, -11.54700538379251284, -122.7500000040967905 ) ) ;
#40415 = CARTESIAN_POINT ( 'NONE',  ( -10.81189881249999729, 6.242252689847871849, -140.2187500020483810 ) ) ;
#40416 = CARTESIAN_POINT ( 'NONE',  ( -5.405949406249996869, 9.363379034771805109, -158.3437500020483810 ) ) ;
#40417 = CARTESIAN_POINT ( 'NONE',  ( 9.999999999999998224, 0.000000000000000000, -155.0000000000000000 ) ) ;
#40418 = CARTESIAN_POINT ( 'NONE',  ( 9.999999999999998224, 0.000000000000000000, -66.87500000409676204 ) ) ;
#40419 = CARTESIAN_POINT ( 'NONE',  ( 5.000000000000000000, 8.660254037844385522, -175.7500000000000284 ) ) ;
#40420 = CARTESIAN_POINT ( 'NONE',  ( 5.405949406249999534, 9.363379034771803333, -88.09375000204836681 ) ) ;
#40421 = FACE_OUTER_BOUND ( 'NONE', #37031, .T. ) ;
#40422 = CARTESIAN_POINT ( 'NONE',  ( -10.81189881249999729, 1.324075727343319199E-15, -63.78125000204837391 ) ) ;
#40423 = DIRECTION ( 'NONE',  ( 1.000000000000000000, 0.000000000000000000, 0.000000000000000000 ) ) ;
#40424 = CARTESIAN_POINT ( 'NONE',  ( 5.405949406249999534, 9.363379034771803333, -181.0937500020483810 ) ) ;
#40425 = EDGE_CURVE ( 'NONE', #14436, #31963, #24142, .T. ) ;
#40426 = CARTESIAN_POINT ( 'NONE',  ( -10.81189881249999729, 6.242252689847871849, -120.9062500020483952 ) ) ;
#40427 = CARTESIAN_POINT ( 'NONE',  ( 10.81189881249999729, 0.000000000000000000, -154.5312500020484094 ) ) ;
#40428 = CARTESIAN_POINT ( 'NONE',  ( -10.81189881249999907, -6.242252689847864744, -51.65625000204837391 ) ) ;
#40429 = CARTESIAN_POINT ( 'NONE',  ( -2.121150477449813534E-15, -11.54700538379251284, -130.2500000040967905 ) ) ;
#40430 = CARTESIAN_POINT ( 'NONE',  ( 5.000000000000000000, 8.660254037844385522, -111.2499999999999858 ) ) ;
#40431 = ORIENTED_EDGE ( 'NONE', *, *, #40356, .T. ) ;
#40432 = CARTESIAN_POINT ( 'NONE',  ( -5.405949406249996869, 9.363379034771805109, -133.0312500020484094 ) ) ;
#40433 = CARTESIAN_POINT ( 'NONE',  ( -9.999999999999998224, 1.224646799147353059E-15, -148.6250000040967905 ) ) ;
#40434 = CARTESIAN_POINT ( 'NONE',  ( -10.81189881249999907, -6.242252689847864744, -152.1562500020484094 ) ) ;
#40435 = ADVANCED_FACE ( 'NONE', ( #5085 ), #37455, .T. ) ;
#40436 = CARTESIAN_POINT ( 'NONE',  ( -10.81189881249999729, 6.242252689847871849, -186.9062500020484094 ) ) ;
#40437 = ORIENTED_EDGE ( 'NONE', *, *, #1114, .T. ) ;
#40438 = CARTESIAN_POINT ( 'NONE',  ( 10.00000000000000000, 5.773502691896255534, -46.87499999999996447 ) ) ;
#40439 = CARTESIAN_POINT ( 'NONE',  ( -10.81189881249999729, 1.324075727343319199E-15, -180.5937500020484094 ) ) ;
#40440 = CARTESIAN_POINT ( 'NONE',  ( -5.000000000000003553, -8.660254037844383745, -55.37500000409675494 ) ) ;
#40441 = EDGE_CURVE ( 'NONE', #22759, #35200, #11108, .T. ) ;
#40442 = CARTESIAN_POINT ( 'NONE',  ( -2.121150477449813534E-15, -11.54700538379251284, -110.3749999999999858 ) ) ;
#40443 = DIRECTION ( 'NONE',  ( -0.000000000000000000, -0.000000000000000000, -1.000000000000000000 ) ) ;
#40444 = CARTESIAN_POINT ( 'NONE',  ( 10.81189881249999729, 0.000000000000000000, -78.03125000204838102 ) ) ;
#40445 = CARTESIAN_POINT ( 'NONE',  ( -10.81189881249999729, 6.242252689847871849, -60.90625000204837391 ) ) ;
#40446 = CARTESIAN_POINT ( 'NONE',  ( 4.999999999999992006, -8.660254037844389075, -52.12500000409675494 ) ) ;
#40447 = CARTESIAN_POINT ( 'NONE',  ( -5.405949406250003975, -9.363379034771801557, -12.34375000204834905 ) ) ;
#40448 = DIRECTION ( 'NONE',  ( -0.000000000000000000, -0.000000000000000000, -1.000000000000000000 ) ) ;
#40449 = CARTESIAN_POINT ( 'NONE',  ( 10.81189881249999729, 0.000000000000000000, -178.5312500020483810 ) ) ;
#40450 = CARTESIAN_POINT ( 'NONE',  ( 10.81189881249999729, 0.000000000000000000, -3.031250002048374803 ) ) ;
#40451 = CARTESIAN_POINT ( 'NONE',  ( -9.999999999999998224, 1.224646799147353059E-15, -88.24999999999998579 ) ) ;
#40452 = CARTESIAN_POINT ( 'NONE',  ( 9.999999999999998224, 0.000000000000000000, -106.9999999999999858 ) ) ;
#40453 = EDGE_CURVE ( 'NONE', #27421, #13539, #37671, .T. ) ;
#40454 = CARTESIAN_POINT ( 'NONE',  ( 9.999999999999998224, 0.000000000000000000, -177.5000000000000000 ) ) ;
#40455 = DIRECTION ( 'NONE',  ( -1.000000000000000000, 0.000000000000000000, 0.000000000000000000 ) ) ;
#40457 = VERTEX_POINT ( 'NONE', #4868 ) ;
#40456 = CARTESIAN_POINT ( 'NONE',  ( -2.293366432827344421E-15, -12.48450537969573659, -84.40625000204838102 ) ) ;
#40459 = ORIENTED_EDGE ( 'NONE', *, *, #14833, .T. ) ;
#40458 = CARTESIAN_POINT ( 'NONE',  ( 9.999999999999998224, 0.000000000000000000, -92.37500000409677625 ) ) ;
#40460 = ORIENTED_EDGE ( 'NONE', *, *, #2776, .F. ) ;
#40461 = CARTESIAN_POINT ( 'NONE',  ( 10.81189881249999729, 6.242252689847867408, -34.21875000204835260 ) ) ;
#40462 = CARTESIAN_POINT ( 'NONE',  ( -5.405949406249996869, 9.363379034771805109, -26.34375000204835970 ) ) ;
#40463 = CARTESIAN_POINT ( 'NONE',  ( -5.405949406249996869, 9.363379034771805109, -10.03125000204835260 ) ) ;
#40464 = CARTESIAN_POINT ( 'NONE',  ( 10.81189881249999551, -6.242252689847874514, -65.96875000204836681 ) ) ;
#40465 = DIRECTION ( 'NONE',  ( -0.000000000000000000, -0.000000000000000000, 1.000000000000000000 ) ) ;
#40466 = CARTESIAN_POINT ( 'NONE',  ( -2.121150477449813534E-15, -11.54700538379251284, -44.37499999999997158 ) ) ;
#40467 = CARTESIAN_POINT ( 'NONE',  ( -10.81189881249999729, 6.242252689847871849, -185.2187500020483810 ) ) ;
#40468 = CARTESIAN_POINT ( 'NONE',  ( 5.405949406249999534, 9.363379034771803333, -167.5937500020484094 ) ) ;
#40469 = CARTESIAN_POINT ( 'NONE',  ( 10.81189881249999551, -6.242252689847874514, -2.968750002048361925 ) ) ;
#40470 = CARTESIAN_POINT ( 'NONE',  ( -2.121150477449813534E-15, -11.54700538379251284, -192.8750000000000284 ) ) ;
#40471 = CARTESIAN_POINT ( 'NONE',  ( -10.00000000000051337, 5.773502691895962435, -70.75000000409677625 ) ) ;
#40472 = CARTESIAN_POINT ( 'NONE',  ( -9.999999999999998224, 1.224646799147353059E-15, -125.7499999999999716 ) ) ;
#40473 = FACE_OUTER_BOUND ( 'NONE', #13112, .T. ) ;
#40474 = CARTESIAN_POINT ( 'NONE',  ( 10.81189881249999907, 6.242252689847868297, -116.7187500020483810 ) ) ;
#40475 = CARTESIAN_POINT ( 'NONE',  ( 5.000000000000000000, 8.660254037844385522, -15.24999999999995737 ) ) ;
#40476 = CARTESIAN_POINT ( 'NONE',  ( 10.81189881249999729, 0.000000000000000000, -93.03125000204838102 ) ) ;
#40477 = CARTESIAN_POINT ( 'NONE',  ( 5.405949406249992428, -9.363379034771808662, -99.09375000204838102 ) ) ;
#40478 = VECTOR ( 'NONE', #35469, 1000.000000000000000 ) ;
#40479 = CARTESIAN_POINT ( 'NONE',  ( 10.81189881249999551, -6.242252689847874514, -67.46875000204838102 ) ) ;
#40480 = CARTESIAN_POINT ( 'NONE',  ( -10.81189881249999729, 6.242252689847871849, -77.40625000204838102 ) ) ;
#40481 = CARTESIAN_POINT ( 'NONE',  ( -4.999999999999996447, 8.660254037844387298, -150.3750000040967905 ) ) ;
#40482 = CARTESIAN_POINT ( 'NONE',  ( -5.000000000000003553, -8.660254037844383745, -134.5000000000000000 ) ) ;
#40483 =( BOUNDED_CURVE ( )  B_SPLINE_CURVE ( 2, ( #41375, #34073, #18078, #24800, #11592, #37294, #17426 ),
 .UNSPECIFIED., .F., .F. ) 
 B_SPLINE_CURVE_WITH_KNOTS ( ( 3, 2, 2, 3 ),
 ( 0.02238805970149256030, 0.02363184079601992477, 0.02487562189054729270, 0.02611940298507465369 ),
 .UNSPECIFIED. ) 
 CURVE ( )  GEOMETRIC_REPRESENTATION_ITEM ( )  RATIONAL_B_SPLINE_CURVE ( ( 0.9999999999999973355, 0.8660254037844413721, 1.000000000000000000, 0.8660254037844387076, 1.000000000000000000, 0.8660254037844357100, 1.000000000000003109 ) ) 
 REPRESENTATION_ITEM ( '' )  );
#40484 = CARTESIAN_POINT ( 'NONE',  ( -2.293366432827344421E-15, -12.48450537969573659, -160.9062500020483810 ) ) ;
#40485 = CARTESIAN_POINT ( 'NONE',  ( -5.405949406250003975, -9.363379034771801557, -171.5312500020484094 ) ) ;
#40486 = DIRECTION ( 'NONE',  ( 0.000000000000000000, 0.000000000000000000, 1.000000000000000000 ) ) ;
#40487 = CARTESIAN_POINT ( 'NONE',  ( 9.999999999999998224, 0.000000000000000000, -101.3750000040967905 ) ) ;
#40488 = CARTESIAN_POINT ( 'NONE',  ( 5.405949406249999534, 9.363379034771803333, -106.0937500020483810 ) ) ;
#40489 = CARTESIAN_POINT ( 'NONE',  ( 7.070501591499376803E-16, 11.54700538379251284, -10.62499999999995381 ) ) ;
#40490 = CARTESIAN_POINT ( 'NONE',  ( 4.999999999999992006, -8.660254037844389075, -75.74999999999998579 ) ) ;
#40491 = CARTESIAN_POINT ( 'NONE',  ( -2.293366432827344421E-15, -12.48450537969573659, -3.406250002048361036 ) ) ;
#40492 = CARTESIAN_POINT ( 'NONE',  ( -5.000000000000003553, -8.660254037844383745, -91.37500000409677625 ) ) ;
#40493 = CARTESIAN_POINT ( 'NONE',  ( 9.999999999999872102, 5.773502691896329253, -168.7500000040967905 ) ) ;
#40494 = CARTESIAN_POINT ( 'NONE',  ( 10.81189881249999551, -6.242252689847874514, -97.65625000204839523 ) ) ;
#40495 = CARTESIAN_POINT ( 'NONE',  ( 5.405949406249992428, -9.363379034771808662, -85.78125000204838102 ) ) ;
#40496 =( BOUNDED_CURVE ( )  B_SPLINE_CURVE ( 2, ( #32294, #18902, #29466, #32502, #25808, #32083, #19310 ),
 .UNSPECIFIED., .F., .F. ) 
 B_SPLINE_CURVE_WITH_KNOTS ( ( 3, 2, 2, 3 ),
 ( 0.01492537313432837180, 0.01616915422885573453, 0.01741293532338310246, 0.01865671641791046345 ),
 .UNSPECIFIED. ) 
 CURVE ( )  GEOMETRIC_REPRESENTATION_ITEM ( )  RATIONAL_B_SPLINE_CURVE ( ( 0.9999999999999984457, 0.8660254037844402619, 1.000000000000000000, 0.8660254037844387076, 1.000000000000000000, 0.8660254037844368202, 1.000000000000001776 ) ) 
 REPRESENTATION_ITEM ( '' )  );
#40497 = CARTESIAN_POINT ( 'NONE',  ( 4.999999999999992006, -8.660254037844389075, -79.12500000409677625 ) ) ;
#40498 = CARTESIAN_POINT ( 'NONE',  ( 9.999999999999998224, 0.000000000000000000, -19.99999999999996092 ) ) ;
#40499 = CARTESIAN_POINT ( 'NONE',  ( -10.81189881249999729, 1.324075727343319199E-15, -38.09375000204837391 ) ) ;
#40500 = ORIENTED_EDGE ( 'NONE', *, *, #6966, .F. ) ;
#40501 = CARTESIAN_POINT ( 'NONE',  ( 9.999999999999996447, -5.773502691896262640, -2.124999999999945821 ) ) ;
#40502 = CARTESIAN_POINT ( 'NONE',  ( 5.405949406249992428, -9.363379034771808662, -31.78125000204837391 ) ) ;
#40503 = CARTESIAN_POINT ( 'NONE',  ( -10.81189881249999729, 1.324075727343319199E-15, -17.09375000204835260 ) ) ;
#40504 = CARTESIAN_POINT ( 'NONE',  ( -4.999999999999996447, 8.660254037844387298, -160.5000000000000000 ) ) ;
#40505 = CARTESIAN_POINT ( 'NONE',  ( 4.999999999999992006, -8.660254037844389075, -7.125000004096743389 ) ) ;
#40506 = CARTESIAN_POINT ( 'NONE',  ( -10.81189881249999729, 6.242252689847871849, -132.9062500020483810 ) ) ;
#40507 =( BOUNDED_CURVE ( )  B_SPLINE_CURVE ( 2, ( #23265, #13098, #13524, #16550, #26710, #29748, #2995 ),
 .UNSPECIFIED., .F., .F. ) 
 B_SPLINE_CURVE_WITH_KNOTS ( ( 3, 2, 2, 3 ),
 ( 0.04850746268656720706, 0.04975124378109457846, 0.05099502487562193598, 0.05223880597014930738 ),
 .UNSPECIFIED. ) 
 CURVE ( )  GEOMETRIC_REPRESENTATION_ITEM ( )  RATIONAL_B_SPLINE_CURVE ( ( 0.9999999999999955591, 0.8660254037844431485, 1.000000000000000000, 0.8660254037844387076, 1.000000000000000000, 0.8660254037844327124, 1.000000000000005995 ) ) 
 REPRESENTATION_ITEM ( '' )  );
#40508 = CARTESIAN_POINT ( 'NONE',  ( -9.999999999999998224, 1.224646799147353059E-15, -185.7500000000000000 ) ) ;
#40509 = DIRECTION ( 'NONE',  ( -0.000000000000000000, -0.000000000000000000, 1.000000000000000000 ) ) ;
#40511 = VERTEX_POINT ( 'NONE', #18015 ) ;
#40510 = CARTESIAN_POINT ( 'NONE',  ( 10.81189881249999551, -6.242252689847874514, -112.6562500020483810 ) ) ;
#40512 = VECTOR ( 'NONE', #14788, 1000.000000000000000 ) ;
#40513 = DIRECTION ( 'NONE',  ( -0.000000000000000000, -0.000000000000000000, 1.000000000000000000 ) ) ;
#40514 = ORIENTED_EDGE ( 'NONE', *, *, #12373, .F. ) ;
#40515 = ORIENTED_EDGE ( 'NONE', *, *, #3288, .F. ) ;
#40516 = CARTESIAN_POINT ( 'NONE',  ( 7.644554776091147741E-16, 12.48450537969573659, -34.15625000204836681 ) ) ;
#40517 = APPROVAL_STATUS ( 'not_yet_approved' ) ;
#40518 = CARTESIAN_POINT ( 'NONE',  ( -10.81189881249999907, -6.242252689847864744, -97.96875000204838102 ) ) ;
#40519 = DIRECTION ( 'NONE',  ( -0.000000000000000000, -0.000000000000000000, 1.000000000000000000 ) ) ;
#40520 = CARTESIAN_POINT ( 'NONE',  ( 9.999999999999998224, 0.000000000000000000, -147.8750000040967905 ) ) ;
#40521 = CARTESIAN_POINT ( 'NONE',  ( 7.644554776091147741E-16, 12.48450537969573659, -197.4687500020484094 ) ) ;
#40522 = CARTESIAN_POINT ( 'NONE',  ( 10.81189881249999729, 0.000000000000000000, -169.5312500020484094 ) ) ;
#40523 = CARTESIAN_POINT ( 'NONE',  ( 9.999999999999998224, 0.000000000000000000, -138.5000000000000000 ) ) ;
#40524 = ADVANCED_FACE ( 'NONE', ( #31214 ), #28182, .T. ) ;
#40525 = CARTESIAN_POINT ( 'NONE',  ( 10.81189881249999729, 0.000000000000000000, -122.8437500020483952 ) ) ;
#40526 = CARTESIAN_POINT ( 'NONE',  ( 5.405949406249999534, 9.363379034771803333, -94.09375000204838102 ) ) ;
#40527 = CARTESIAN_POINT ( 'NONE',  ( -5.405949406250003975, -9.363379034771801557, -5.031250002048376579 ) ) ;
#40528 = CARTESIAN_POINT ( 'NONE',  ( -10.00000000000051337, 5.773502691895962435, -106.3749999999999716 ) ) ;
#40529 = CARTESIAN_POINT ( 'NONE',  ( 7.644554776091147741E-16, 12.48450537969573659, -100.1562500020483952 ) ) ;
#40530 = CARTESIAN_POINT ( 'NONE',  ( 10.00000000000000000, 5.773502691896255534, -179.2500000040967905 ) ) ;
#40531 = CARTESIAN_POINT ( 'NONE',  ( -10.81189881249999729, -6.242252689847864744, -109.9687500020483810 ) ) ;
#40532 = CARTESIAN_POINT ( 'NONE',  ( -5.405949406250003975, -9.363379034771801557, -180.5312500020483810 ) ) ;
#40533 = CARTESIAN_POINT ( 'NONE',  ( 9.999999999999998224, 0.000000000000000000, -106.9999999999999858 ) ) ;
#40534 = CARTESIAN_POINT ( 'NONE',  ( -9.999999999999998224, 1.224646799147353059E-15, -86.74999999999998579 ) ) ;
#40535 = CARTESIAN_POINT ( 'NONE',  ( -10.81189881249999729, 6.242252689847871849, -197.4062500020484379 ) ) ;
#40536 = CARTESIAN_POINT ( 'NONE',  ( -10.81189881249999729, -6.242252689847864744, -52.96875000204837391 ) ) ;
#40537 = CARTESIAN_POINT ( 'NONE',  ( -10.81189881249999907, -6.242252689847864744, -42.46875000204835260 ) ) ;
#40538 = CARTESIAN_POINT ( 'NONE',  ( -9.999999999999998224, 1.224646799147353059E-15, -175.6250000040968189 ) ) ;
#40539 = CARTESIAN_POINT ( 'NONE',  ( 7.644554776091147741E-16, 12.48450537969573659, -7.156250002048365921 ) ) ;
#40540 = CARTESIAN_POINT ( 'NONE',  ( -10.81189881249999729, 1.324075727343319199E-15, -20.09375000204835615 ) ) ;
#40541 = CARTESIAN_POINT ( 'NONE',  ( -9.999999999999998224, 1.224646799147353059E-15, -93.12500000409677625 ) ) ;
#40542 = CARTESIAN_POINT ( 'NONE',  ( 5.405949406249992428, -9.363379034771808662, -133.5937500020483810 ) ) ;
#40543 = CARTESIAN_POINT ( 'NONE',  ( 10.00000000000000000, 5.773502691896255534, -97.87499999999998579 ) ) ;
#40544 = CARTESIAN_POINT ( 'NONE',  ( -2.293366432827344421E-15, -12.48450537969573659, -27.40625000204838102 ) ) ;
#40545 = CARTESIAN_POINT ( 'NONE',  ( -9.999999999999998224, 1.224646799147353059E-15, -112.6250000040967763 ) ) ;
#40546 = CARTESIAN_POINT ( 'NONE',  ( 4.999999999999992006, -8.660254037844389075, -26.62500000409676204 ) ) ;
#40547 = CARTESIAN_POINT ( 'NONE',  ( 4.999999999999992006, -8.660254037844389075, -60.74999999999997158 ) ) ;
#40548 = CARTESIAN_POINT ( 'NONE',  ( -2.293366432827344421E-15, -12.48450537969573659, -127.9062500020483952 ) ) ;
#40549 = CARTESIAN_POINT ( 'NONE',  ( -5.405949406250003975, -9.363379034771801557, -104.0312500020483810 ) ) ;
#40550 = EDGE_CURVE ( 'NONE', #35982, #26720, #12636, .T. ) ;
#40551 = ORIENTED_EDGE ( 'NONE', *, *, #36754, .T. ) ;
#40552 = CARTESIAN_POINT ( 'NONE',  ( 4.999999999999992006, -8.660254037844389075, -117.7500000000000000 ) ) ;
#40553 = CARTESIAN_POINT ( 'NONE',  ( -4.999999999999996447, 8.660254037844387298, -102.3750000040967905 ) ) ;
#40554 = CARTESIAN_POINT ( 'NONE',  ( -10.00000000000051337, 5.773502691895962435, -141.2500000040967905 ) ) ;
#40555 = CARTESIAN_POINT ( 'NONE',  ( 10.81189881249999551, -6.242252689847874514, -165.1562500020483526 ) ) ;
#40556 = CARTESIAN_POINT ( 'NONE',  ( -5.405949406249996869, 9.363379034771805109, -59.34375000204835970 ) ) ;
#40557 = ORIENTED_EDGE ( 'NONE', *, *, #33639, .T. ) ;
#40558 = CARTESIAN_POINT ( 'NONE',  ( 5.000000000000000000, 8.660254037844385522, -25.74999999999996803 ) ) ;
#40559 = CARTESIAN_POINT ( 'NONE',  ( 5.405949406249992428, -9.363379034771808662, -34.78125000204837391 ) ) ;
#40560 = CARTESIAN_POINT ( 'NONE',  ( -9.999999999999998224, 1.224646799147353059E-15, -164.7500000000000000 ) ) ;
#40561 = CARTESIAN_POINT ( 'NONE',  ( 0.000000000000000000, 0.000000000000000000, -99.99999999999998579 ) ) ;
#40562 = CARTESIAN_POINT ( 'NONE',  ( 7.070501591499377789E-16, 11.54700538379251284, -32.00000000409674783 ) ) ;
#40563 = CARTESIAN_POINT ( 'NONE',  ( -2.293366432827344421E-15, -12.48450537969573659, -135.4062500020483810 ) ) ;
#40564 = CARTESIAN_POINT ( 'NONE',  ( 8.421130500909246308, 6.441071276087089181, -7.741086494507740905E-15 ) ) ;
#40565 = CYLINDRICAL_SURFACE ( 'NONE', #3849, 9.999999999999998224 ) ;
#40566 = VERTEX_POINT ( 'NONE', #24312 ) ;
#40568 = ORIENTED_EDGE ( 'NONE', *, *, #42224, .F. ) ;
#40567 = VERTEX_POINT ( 'NONE', #32060 ) ;
#40569 = AXIS2_PLACEMENT_3D ( 'NONE', #21016, #1394, #37641 ) ;
#40570 =( BOUNDED_CURVE ( )  B_SPLINE_CURVE ( 2, ( #9396, #2091, #31876, #12612, #25805, #25386, #15221 ),
 .UNSPECIFIED., .F., .F. ) 
 B_SPLINE_CURVE_WITH_KNOTS ( ( 3, 2, 2, 3 ),
 ( 0.8694029850746272103, 0.8706467661691545956, 0.8718905472636818699, 0.8731343283582092551 ),
 .UNSPECIFIED. ) 
 CURVE ( )  GEOMETRIC_REPRESENTATION_ITEM ( )  RATIONAL_B_SPLINE_CURVE ( ( 0.9999999999999641398, 0.8660254037844745678, 1.000000000000000000, 0.8660254037844387076, 1.000000000000000000, 0.8660254037844028474, 1.000000000000035971 ) ) 
 REPRESENTATION_ITEM ( '' )  );
#40571 = CYLINDRICAL_SURFACE ( 'NONE', #25229, 9.999999999999998224 ) ;
#40572 = CARTESIAN_POINT ( 'NONE',  ( -9.999999999999227285, -5.773502691896698735, -134.6249999999999716 ) ) ;
#40574 = EDGE_CURVE ( 'NONE', #25583, #37654, #16519, .T. ) ;
#40573 = CARTESIAN_POINT ( 'NONE',  ( 5.405949406249999534, 9.363379034771803333, -167.5937500020484094 ) ) ;
#40575 = CARTESIAN_POINT ( 'NONE',  ( 10.81189881249999907, 6.242252689847868297, -193.4062500020484094 ) ) ;
#40576 = CARTESIAN_POINT ( 'NONE',  ( -10.81189881249999729, 1.324075727343319199E-15, -18.59375000204835260 ) ) ;
#40577 = AXIS2_PLACEMENT_3D ( 'NONE', #39652, #11568, #11786 ) ;
#40578 = FACE_OUTER_BOUND ( 'NONE', #31642, .T. ) ;
#40579 = CARTESIAN_POINT ( 'NONE',  ( 10.81189881249999551, -6.242252689847874514, -146.9687500020484094 ) ) ;
#40580 = CARTESIAN_POINT ( 'NONE',  ( -10.81189881249999729, 1.324075727343319199E-15, -137.0937500020483810 ) ) ;
#40581 = CARTESIAN_POINT ( 'NONE',  ( 5.405949406249992428, -9.363379034771808662, -105.2812500020483810 ) ) ;
#40582 = CARTESIAN_POINT ( 'NONE',  ( -10.81189881249999907, -6.242252689847864744, -120.4687500020483810 ) ) ;
#40583 = CARTESIAN_POINT ( 'NONE',  ( 9.999999999999998224, 0.000000000000000000, -198.8750000040967905 ) ) ;
#40584 = CARTESIAN_POINT ( 'NONE',  ( -5.405949406250003975, -9.363379034771801557, -128.0312500020484094 ) ) ;
#40585 = CARTESIAN_POINT ( 'NONE',  ( 10.81189881249999551, -6.242252689847874514, -11.96875000204837214 ) ) ;
#40586 = CARTESIAN_POINT ( 'NONE',  ( -10.81189881249999729, -6.242252689847864744, -132.4687500020483810 ) ) ;
#40587 = DIRECTION ( 'NONE',  ( 1.000000000000000000, 0.000000000000000000, 0.000000000000000000 ) ) ;
#40588 = CARTESIAN_POINT ( 'NONE',  ( -10.00000000000019362, -5.773502691896140959, -178.5000000040968189 ) ) ;
#40589 = CARTESIAN_POINT ( 'NONE',  ( -4.999999999999996447, 8.660254037844387298, -156.0000000000000000 ) ) ;
#40590 = CARTESIAN_POINT ( 'NONE',  ( -2.121150477449813534E-15, -11.54700538379251284, -17.37499999999997513 ) ) ;
#40591 = CARTESIAN_POINT ( 'NONE',  ( 10.81189881249999729, 0.000000000000000000, -77.84375000204838102 ) ) ;
#40592 = CARTESIAN_POINT ( 'NONE',  ( 10.81189881249999729, 0.000000000000000000, -61.34375000204836681 ) ) ;
#40593 = CARTESIAN_POINT ( 'NONE',  ( 9.999999999999998224, 0.000000000000000000, -200.0000000000000000 ) ) ;
#40594 = CARTESIAN_POINT ( 'NONE',  ( -2.293366432827344421E-15, -12.48450537969573659, -33.40625000204835970 ) ) ;
#40595 = CARTESIAN_POINT ( 'NONE',  ( 7.644554776091147741E-16, 12.48450537969573659, -47.46875000204836681 ) ) ;
#40596 = CARTESIAN_POINT ( 'NONE',  ( -10.81189881249999907, -6.242252689847864744, -151.9687500020484094 ) ) ;
#40597 = CARTESIAN_POINT ( 'NONE',  ( 9.999999999999996447, -5.773502691896262640, -120.6250000000000000 ) ) ;
#40598 = CARTESIAN_POINT ( 'NONE',  ( 5.405949406249992428, -9.363379034771808662, -129.2812500020483810 ) ) ;
#40599 = CARTESIAN_POINT ( 'NONE',  ( -5.000000000000003553, -8.660254037844383745, -187.3750000040967905 ) ) ;
#40600 = CARTESIAN_POINT ( 'NONE',  ( -10.00000000000000000, -5.773502691896251982, -82.12499999999998579 ) ) ;
#40601 = CARTESIAN_POINT ( 'NONE',  ( -10.81189881249999729, 6.242252689847871849, -15.90625000204837391 ) ) ;
#40602 = ORIENTED_EDGE ( 'NONE', *, *, #15445, .F. ) ;
#40603 = CARTESIAN_POINT ( 'NONE',  ( -10.81189881249999729, 1.324075727343319199E-15, -102.7812500020483952 ) ) ;
#40604 = CARTESIAN_POINT ( 'NONE',  ( 7.070501591499377789E-16, 11.54700538379251284, -120.5000000040967905 ) ) ;
#40605 = CARTESIAN_POINT ( 'NONE',  ( -9.999999999999998224, 1.224646799147353059E-15, -37.62500000409676915 ) ) ;
#40606 = ADVANCED_FACE ( 'NONE', ( #38515 ), #35510, .T. ) ;
#40607 = CARTESIAN_POINT ( 'NONE',  ( -2.121150477449813534E-15, -11.54700538379251284, -2.750000004096757156 ) ) ;
#40608 = CARTESIAN_POINT ( 'NONE',  ( -2.293366432827344421E-15, -12.48450537969573659, -52.90625000204837391 ) ) ;
#40609 = CARTESIAN_POINT ( 'NONE',  ( -5.405949406249996869, 9.363379034771805109, -152.5312500020484094 ) ) ;
#40610 = AXIS2_PLACEMENT_3D ( 'NONE', #17209, #36866, #10954 ) ;
#40611 = CARTESIAN_POINT ( 'NONE',  ( -2.293366432827344421E-15, -12.48450537969573659, -126.2187500020483952 ) ) ;
#40612 = CARTESIAN_POINT ( 'NONE',  ( 5.000000000000000000, 8.660254037844385522, -109.7499999999999858 ) ) ;
#40613 = ORIENTED_EDGE ( 'NONE', *, *, #11920, .T. ) ;
#40614 = CARTESIAN_POINT ( 'NONE',  ( 9.999999999998456346, 5.773502691897149042, -22.87499999999994316 ) ) ;
#40615 = VERTEX_POINT ( 'NONE', #21904 ) ;
#40616 =( BOUNDED_CURVE ( )  B_SPLINE_CURVE ( 2, ( #33548, #747, #17113, #33760, #27489, #27065, #4181 ),
 .UNSPECIFIED., .F., .F. ) 
 B_SPLINE_CURVE_WITH_KNOTS ( ( 3, 2, 2, 3 ),
 ( 0.6791044776119405935, 0.6803482587064679787, 0.6815920398009952530, 0.6828358208955226383 ),
 .UNSPECIFIED. ) 
 CURVE ( )  GEOMETRIC_REPRESENTATION_ITEM ( )  RATIONAL_B_SPLINE_CURVE ( ( 0.9999999999999641398, 0.8660254037844745678, 1.000000000000000000, 0.8660254037844387076, 1.000000000000000000, 0.8660254037844148378, 1.000000000000023981 ) ) 
 REPRESENTATION_ITEM ( '' )  );
#40617 = AXIS2_PLACEMENT_3D ( 'NONE', #17551, #30752, #4626 ) ;
#40618 = ORIENTED_EDGE ( 'NONE', *, *, #1972, .F. ) ;
#40620 = ORIENTED_EDGE ( 'NONE', *, *, #5677, .T. ) ;
#40619 = CARTESIAN_POINT ( 'NONE',  ( -5.405949406249996869, 9.363379034771805109, -108.8437500020483810 ) ) ;
#40621 = CARTESIAN_POINT ( 'NONE',  ( -9.999999999999998224, 1.224646799147353059E-15, -188.7500000000000000 ) ) ;
#40622 = CARTESIAN_POINT ( 'NONE',  ( -10.81189881249999907, -6.242252689847864744, -186.4687500020484094 ) ) ;
#40623 = CARTESIAN_POINT ( 'NONE',  ( 10.81189881249999729, 0.000000000000000000, -41.84375000204837391 ) ) ;
#40624 = CARTESIAN_POINT ( 'NONE',  ( -5.000000000000003553, -8.660254037844383745, -155.8750000040967905 ) ) ;
#40625 = CARTESIAN_POINT ( 'NONE',  ( -5.405949406250003975, -9.363379034771801557, -169.8437500020484094 ) ) ;
#40626 = CARTESIAN_POINT ( 'NONE',  ( 10.81189881249999551, -6.242252689847874514, -163.4687500020483810 ) ) ;
#40627 = DIRECTION ( 'NONE',  ( -0.000000000000000000, -0.000000000000000000, 1.000000000000000000 ) ) ;
#40628 = CARTESIAN_POINT ( 'NONE',  ( -2.293366432827344421E-15, -12.48450537969573659, -144.2187500020483810 ) ) ;
#40629 = CARTESIAN_POINT ( 'NONE',  ( 7.644554776091147741E-16, 12.48450537969573659, -153.9687500020484094 ) ) ;
#40630 = CARTESIAN_POINT ( 'NONE',  ( -9.999999999999479527, -5.773502691896549521, -94.12499999999997158 ) ) ;
#40631 = CYLINDRICAL_SURFACE ( 'NONE', #5469, 9.999999999999998224 ) ;
#40632 = CARTESIAN_POINT ( 'NONE',  ( 4.999999999999992006, -8.660254037844389075, -180.7500000000000284 ) ) ;
#40633 = AXIS2_PLACEMENT_3D ( 'NONE', #22180, #35565, #9012 ) ;
#40634 = CARTESIAN_POINT ( 'NONE',  ( -10.81189881249999907, -6.242252689847864744, -90.46875000204836681 ) ) ;
#40635 = DIRECTION ( 'NONE',  ( -1.000000000000000000, 0.000000000000000000, 0.000000000000000000 ) ) ;
#40636 = CARTESIAN_POINT ( 'NONE',  ( 5.405949406249992428, -9.363379034771808662, -58.78125000204836681 ) ) ;
#40637 = CARTESIAN_POINT ( 'NONE',  ( 7.070501591499376803E-16, 11.54700538379251284, -146.0000000040967905 ) ) ;
#40638 = CARTESIAN_POINT ( 'NONE',  ( 5.405949406249992428, -9.363379034771808662, -180.0937500020484094 ) ) ;
#40639 = CARTESIAN_POINT ( 'NONE',  ( -5.405949406250003975, -9.363379034771801557, -111.5312500020483810 ) ) ;
#40640 = CARTESIAN_POINT ( 'NONE',  ( -10.81189881249999729, -6.242252689847864744, -150.6562500020484094 ) ) ;
#40641 = CYLINDRICAL_SURFACE ( 'NONE', #16492, 9.999999999999998224 ) ;
#40642 = CARTESIAN_POINT ( 'NONE',  ( -10.81189881249999907, -6.242252689847864744, -47.15625000204837391 ) ) ;
#40643 = CARTESIAN_POINT ( 'NONE',  ( -9.999999999999998224, 1.224646799147353059E-15, -129.1250000040967620 ) ) ;
#40644 = CARTESIAN_POINT ( 'NONE',  ( -2.121150477449813534E-15, -11.54700538379251284, -108.8749999999999858 ) ) ;
#40645 = EDGE_LOOP ( 'NONE', ( #4531, #34908, #26004, #18885 ) ) ;
#40646 = CARTESIAN_POINT ( 'NONE',  ( 7.644554776091147741E-16, 12.48450537969573659, -122.6562500020483952 ) ) ;
#40647 = CARTESIAN_POINT ( 'NONE',  ( 5.000000000000000000, 8.660254037844385522, -147.6250000040967905 ) ) ;
#40648 = CARTESIAN_POINT ( 'NONE',  ( -10.81189881249999907, -6.242252689847864744, -186.6562500020484094 ) ) ;
#40649 = EDGE_LOOP ( 'NONE', ( #7399, #27483, #39567, #34394 ) ) ;
#40650 = CARTESIAN_POINT ( 'NONE',  ( 9.999999999999996447, -5.773502691896262640, -45.62499999999995737 ) ) ;
#40651 = CARTESIAN_POINT ( 'NONE',  ( -5.405949406249996869, 9.363379034771805109, -180.8437500020483810 ) ) ;
#40652 = CARTESIAN_POINT ( 'NONE',  ( 5.000000000000000000, 8.660254037844385522, -59.12500000409676204 ) ) ;
#40653 = EDGE_CURVE ( 'NONE', #311, #16498, #37736, .T. ) ;
#40654 = CARTESIAN_POINT ( 'NONE',  ( 4.999999999999992006, -8.660254037844389075, -18.74999999999996092 ) ) ;
#40655 = DIRECTION ( 'NONE',  ( -1.000000000000000000, -4.506943796211477094E-16, -0.000000000000000000 ) ) ;
#40656 = EDGE_CURVE ( 'NONE', #18647, #36180, #39270, .T. ) ;
#40657 = CARTESIAN_POINT ( 'NONE',  ( -5.405949406250003975, -9.363379034771801557, -75.53125000204838102 ) ) ;
#40658 = CARTESIAN_POINT ( 'NONE',  ( 10.81189881249999551, -6.242252689847874514, -48.15625000204836681 ) ) ;
#40659 = CARTESIAN_POINT ( 'NONE',  ( -9.999999999999998224, 5.773502691896259087, -55.75000000409677625 ) ) ;
#40660 = CARTESIAN_POINT ( 'NONE',  ( -10.81189881249999729, 1.324075727343319199E-15, -11.09375000204834727 ) ) ;
#40661 = DIRECTION ( 'NONE',  ( -1.000000000000000000, 0.000000000000000000, 0.000000000000000000 ) ) ;
#40662 = CARTESIAN_POINT ( 'NONE',  ( 5.405949406249999534, 9.363379034771803333, -176.7812500020484094 ) ) ;
#40663 = CARTESIAN_POINT ( 'NONE',  ( -10.81189881249999907, -6.242252689847864744, -2.156250002048359704 ) ) ;
#40664 = LINE ( 'NONE', #4435, #15943 ) ;
#40665 = CARTESIAN_POINT ( 'NONE',  ( 5.000000000000000000, 8.660254037844385522, -148.7500000000000000 ) ) ;
#40666 = CARTESIAN_POINT ( 'NONE',  ( 5.000000000000000000, 8.660254037844385522, -117.2500000000000000 ) ) ;
#40667 = LINE ( 'NONE', #40248, #26597 ) ;
#40668 = CARTESIAN_POINT ( 'NONE',  ( 9.999999999999998224, 0.000000000000000000, -19.99999999999996092 ) ) ;
#40669 = AXIS2_PLACEMENT_3D ( 'NONE', #1052, #4928, #14826 ) ;
#40671 = ORIENTED_EDGE ( 'NONE', *, *, #41532, .F. ) ;
#40670 = CARTESIAN_POINT ( 'NONE',  ( 10.81189881249999551, -6.242252689847874514, -85.65625000204838102 ) ) ;
#40672 =( NAMED_UNIT ( * ) SI_UNIT ( $, .STERADIAN. ) SOLID_ANGLE_UNIT ( ) );
#40673 = EDGE_CURVE ( 'NONE', #29666, #27948, #12384, .T. ) ;
#40675 = EDGE_LOOP ( 'NONE', ( #24257, #944, #15928, #24039 ) ) ;
#40674 = DIRECTION ( 'NONE',  ( -0.000000000000000000, -0.000000000000000000, -1.000000000000000000 ) ) ;
#40676 = ORIENTED_EDGE ( 'NONE', *, *, #5559, .F. ) ;
#40677 = CARTESIAN_POINT ( 'NONE',  ( 5.405949406249992428, -9.363379034771808662, -39.09375000204837391 ) ) ;
#40678 = CARTESIAN_POINT ( 'NONE',  ( 5.405949406249992428, -9.363379034771808662, -24.09375000204835970 ) ) ;
#40679 = CARTESIAN_POINT ( 'NONE',  ( -2.293366432827344421E-15, -12.48450537969573659, -13.90625000204836503 ) ) ;
#40680 = CARTESIAN_POINT ( 'NONE',  ( 7.644554776091147741E-16, 12.48450537969573659, -60.96875000204838102 ) ) ;
#40681 = CARTESIAN_POINT ( 'NONE',  ( -2.121150477449813534E-15, -11.54700538379251284, -122.3749999999999858 ) ) ;
#40682 = CARTESIAN_POINT ( 'NONE',  ( 9.999999999999996447, -5.773502691896262640, -41.12499999999997158 ) ) ;
#40683 = EDGE_CURVE ( 'NONE', #34991, #19338, #9876, .T. ) ;
#40684 = CARTESIAN_POINT ( 'NONE',  ( 10.81189881249999729, 0.000000000000000000, -181.3437500020483810 ) ) ;
#40685 = CARTESIAN_POINT ( 'NONE',  ( -2.293366432827344421E-15, -12.48450537969573659, -162.2187500020483810 ) ) ;
#40686 = CARTESIAN_POINT ( 'NONE',  ( 10.81189881249999729, 0.000000000000000000, -178.3437500020483810 ) ) ;
#40687 = CARTESIAN_POINT ( 'NONE',  ( 10.00000000000000000, 5.773502691896255534, -132.3750000000000000 ) ) ;
#40688 = LINE ( 'NONE', #24331, #19851 ) ;
#40689 = CARTESIAN_POINT ( 'NONE',  ( 9.999999999999998224, 0.000000000000000000, -126.5000000000000000 ) ) ;
#40690 = LINE ( 'NONE', #13931, #8135 ) ;
#40691 = CARTESIAN_POINT ( 'NONE',  ( 10.81189881249999907, 6.242252689847868297, -109.2187500020483810 ) ) ;
#40692 = CARTESIAN_POINT ( 'NONE',  ( 5.321294541346989426, 0.000000000000000000, -220.0000000000000000 ) ) ;
#40693 = CARTESIAN_POINT ( 'NONE',  ( -10.81189881249999729, 1.324075727343319199E-15, -78.78125000204838102 ) ) ;
#40694 = CARTESIAN_POINT ( 'NONE',  ( -10.81189881249999729, 1.324075727343319199E-15, -99.59375000204838102 ) ) ;
#40695 = CARTESIAN_POINT ( 'NONE',  ( 5.405949406249999534, 9.363379034771803333, -73.09375000204838102 ) ) ;
#40696 = CARTESIAN_POINT ( 'NONE',  ( -5.405949406249996869, 9.363379034771805109, -76.03125000204838102 ) ) ;
#40697 = CARTESIAN_POINT ( 'NONE',  ( 4.999999999999992006, -8.660254037844389075, -157.1250000040967905 ) ) ;
#40698 = CARTESIAN_POINT ( 'NONE',  ( 9.999999999999996447, -5.773502691896262640, -128.1249999999999716 ) ) ;
#40699 = CARTESIAN_POINT ( 'NONE',  ( 5.405949406249992428, -9.363379034771808662, -157.7812500020484094 ) ) ;
#40700 = CARTESIAN_POINT ( 'NONE',  ( 5.405949406249992428, -9.363379034771808662, -171.2812500020484094 ) ) ;
#40701 = APPROVAL_PERSON_ORGANIZATION ( #741, #5916, #33753 ) ;
#40702 = FACE_BOUND ( 'NONE', #14866, .T. ) ;
#40703 = CARTESIAN_POINT ( 'NONE',  ( -5.000000000000003553, -8.660254037844383745, -197.5000000000000000 ) ) ;
#40704 = CARTESIAN_POINT ( 'NONE',  ( 10.81189881249999907, 6.242252689847868297, -104.7187500020483810 ) ) ;
#40705 = DIRECTION ( 'NONE',  ( -0.000000000000000000, -0.000000000000000000, -1.000000000000000000 ) ) ;
#40706 = CARTESIAN_POINT ( 'NONE',  ( 5.000000000000000000, 8.660254037844385522, -72.24999999999998579 ) ) ;
#40707 = CARTESIAN_POINT ( 'NONE',  ( -10.81189881249999907, -6.242252689847864744, -8.156250002048365033 ) ) ;
#40708 = CARTESIAN_POINT ( 'NONE',  ( -2.121150477449813534E-15, -11.54700538379251284, -85.25000000409676204 ) ) ;
#40709 = EDGE_CURVE ( 'NONE', #12005, #13682, #7576, .T. ) ;
#40710 = CARTESIAN_POINT ( 'NONE',  ( 9.999999999999479527, 5.773502691896553074, -115.8749999999999858 ) ) ;
#40711 = CARTESIAN_POINT ( 'NONE',  ( 10.81189881249999907, 6.242252689847868297, -101.9062500020484094 ) ) ;
#40712 = CARTESIAN_POINT ( 'NONE',  ( -5.405949406249996869, 9.363379034771805109, -74.53125000204838102 ) ) ;
#40713 = EDGE_CURVE ( 'NONE', #26528, #36280, #25162, .T. ) ;
#40714 = CARTESIAN_POINT ( 'NONE',  ( -5.000000000000003553, -8.660254037844383745, -79.37500000409677625 ) ) ;
#40715 = CARTESIAN_POINT ( 'NONE',  ( -10.00000000000025580, 5.773502691896109873, -118.3750000000000142 ) ) ;
#40716 = CARTESIAN_POINT ( 'NONE',  ( 10.81189881249999551, -6.242252689847874514, -37.46875000204835970 ) ) ;
#40717 = ORIENTED_EDGE ( 'NONE', *, *, #3448, .T. ) ;
#40718 = CARTESIAN_POINT ( 'NONE',  ( -5.405949406249996869, 9.363379034771805109, -199.0312500020484094 ) ) ;
#40719 = ADVANCED_FACE ( 'NONE', ( #7516 ), #33642, .T. ) ;
#40720 = CARTESIAN_POINT ( 'NONE',  ( 10.81189881249999551, -6.242252689847874514, -25.65625000204838102 ) ) ;
#40721 = CARTESIAN_POINT ( 'NONE',  ( -10.81189881249999729, 1.324075727343319199E-15, -15.59375000204835082 ) ) ;
#40722 = FACE_BOUND ( 'NONE', #2068, .T. ) ;
#40723 = CARTESIAN_POINT ( 'NONE',  ( 9.999999999999996447, -5.773502691896262640, -1.000000004096751605 ) ) ;
#40724 = CC_DESIGN_PERSON_AND_ORGANIZATION_ASSIGNMENT ( #16890, #10425, ( #2849 ) ) ;
#40725 = CARTESIAN_POINT ( 'NONE',  ( 10.81189881249999551, -6.242252689847874514, -129.1562500020483810 ) ) ;
#40726 = CARTESIAN_POINT ( 'NONE',  ( -5.000000000000003553, -8.660254037844383745, -182.5000000000000000 ) ) ;
#40728 = ORIENTED_EDGE ( 'NONE', *, *, #18568, .T. ) ;
#40727 = CARTESIAN_POINT ( 'NONE',  ( -10.81189881249999729, 1.324075727343319199E-15, -111.7812500020483810 ) ) ;
#40729 = CARTESIAN_POINT ( 'NONE',  ( -2.121150477449813534E-15, -11.54700538379251284, -154.2500000040968189 ) ) ;
#40730 = ORIENTED_EDGE ( 'NONE', *, *, #20943, .T. ) ;
#40731 = EDGE_LOOP ( 'NONE', ( #4813, #22652, #27379, #39207 ) ) ;
#40732 = EDGE_CURVE ( 'NONE', #39394, #12699, #16779, .T. ) ;
#40733 = AXIS2_PLACEMENT_3D ( 'NONE', #21588, #24199, #14665 ) ;
#40734 = CARTESIAN_POINT ( 'NONE',  ( 10.81189881249999907, 6.242252689847868297, -38.90625000204835970 ) ) ;
#40735 = DATE_AND_TIME ( #25018, #5618 ) ;
#40736 = LOCAL_TIME ( 11, 57, 6.000000000000000000, #15048 ) ;
#40737 = CARTESIAN_POINT ( 'NONE',  ( 7.644554776091147741E-16, 12.48450537969573659, -89.46875000204838102 ) ) ;
#40738 = DIRECTION ( 'NONE',  ( -0.000000000000000000, -0.000000000000000000, -1.000000000000000000 ) ) ;
#40739 = CARTESIAN_POINT ( 'NONE',  ( 7.070501591499376803E-16, 11.54700538379251284, -174.1250000000000000 ) ) ;
#40740 =( BOUNDED_CURVE ( )  B_SPLINE_CURVE ( 2, ( #28663, #9212, #12434, #25630, #8005, #40992, #18348 ),
 .UNSPECIFIED., .F., .F. ) 
 B_SPLINE_CURVE_WITH_KNOTS ( ( 3, 2, 2, 3 ),
 ( 0.2910447761194031036, 0.2922885572139304333, 0.2935323383084578186, 0.2947761194029852039 ),
 .UNSPECIFIED. ) 
 CURVE ( )  GEOMETRIC_REPRESENTATION_ITEM ( )  RATIONAL_B_SPLINE_CURVE ( ( 0.9999999999999880096, 0.8660254037844506980, 1.000000000000000000, 0.8660254037844387076, 1.000000000000000000, 0.8660254037844267172, 1.000000000000011990 ) ) 
 REPRESENTATION_ITEM ( '' )  );
#40741 = FACE_OUTER_BOUND ( 'NONE', #20026, .T. ) ;
#40742 = CARTESIAN_POINT ( 'NONE',  ( -2.293366432827344421E-15, -12.48450537969573659, -162.4062500020483810 ) ) ;
#40743 = CARTESIAN_POINT ( 'NONE',  ( -60.00000000000000711, 7.347880794884119933E-15, -236.9999999999999716 ) ) ;
#40744 = CARTESIAN_POINT ( 'NONE',  ( -10.81189881249999729, 1.324075727343319199E-15, -125.0937500020483668 ) ) ;
#40745 = CARTESIAN_POINT ( 'NONE',  ( -5.405949406249996869, 9.363379034771805109, -90.84375000204838102 ) ) ;
#40746 = CARTESIAN_POINT ( 'NONE',  ( 0.000000000000000000, 0.000000000000000000, -200.0000000000000000 ) ) ;
#40747 = CARTESIAN_POINT ( 'NONE',  ( -10.81189881249999729, 6.242252689847871849, -198.7187500020484379 ) ) ;
#40748 = CARTESIAN_POINT ( 'NONE',  ( -10.81189881249999729, 1.324075727343319199E-15, -98.28125000204839523 ) ) ;
#40749 = CARTESIAN_POINT ( 'NONE',  ( 9.999999999999996447, -5.773502691896262640, -175.0000000040968189 ) ) ;
#40750 = CARTESIAN_POINT ( 'NONE',  ( -10.81189881249999729, 1.324075727343319199E-15, -104.0937500020483810 ) ) ;
#40751 = CARTESIAN_POINT ( 'NONE',  ( 5.405949406249999534, 9.363379034771803333, -175.2812500020484094 ) ) ;
#40752 = LINE ( 'NONE', #661, #10281 ) ;
#40753 = CARTESIAN_POINT ( 'NONE',  ( 9.975233911794434860, 6.725301395491736223, -179.8869040731969449 ) ) ;
#40754 = CARTESIAN_POINT ( 'NONE',  ( -5.405949406249996869, 9.363379034771805109, -194.5312500020484094 ) ) ;
#40755 = CARTESIAN_POINT ( 'NONE',  ( 10.81189881249999551, -6.242252689847874514, -50.96875000204836681 ) ) ;
#40756 = CARTESIAN_POINT ( 'NONE',  ( 7.070501591499377789E-16, 11.54700538379251284, -174.5000000040967905 ) ) ;
#40757 = CARTESIAN_POINT ( 'NONE',  ( 5.405949406249992428, -9.363379034771808662, -7.781250002048350822 ) ) ;
#40758 = CARTESIAN_POINT ( 'NONE',  ( 10.81189881249999907, 6.242252689847868297, -22.21875000204836681 ) ) ;
#40759 = CARTESIAN_POINT ( 'NONE',  ( -9.999999999999872102, -5.773502691896326589, -193.5000000040967620 ) ) ;
#40760 = CARTESIAN_POINT ( 'NONE',  ( 10.81189881249999907, 6.242252689847868297, -130.2187500020483810 ) ) ;
#40761 = CARTESIAN_POINT ( 'NONE',  ( 4.999999999999992006, -8.660254037844389075, -98.24999999999998579 ) ) ;
#40762 = CARTESIAN_POINT ( 'NONE',  ( 5.405949406249999534, 9.363379034771803333, -26.78125000204836681 ) ) ;
#40763 = CARTESIAN_POINT ( 'NONE',  ( -2.121150477449813534E-15, -11.54700538379251284, -107.7500000040967763 ) ) ;
#40764 = CARTESIAN_POINT ( 'NONE',  ( 9.999999999999479527, 5.773502691896553074, -102.3749999999999858 ) ) ;
#40765 = CARTESIAN_POINT ( 'NONE',  ( 9.999999999999996447, -5.773502691896262640, -53.12499999999997868 ) ) ;
#40766 = CARTESIAN_POINT ( 'NONE',  ( 5.405949406249999534, 9.363379034771803333, -127.2812500020483810 ) ) ;
#40767 = CARTESIAN_POINT ( 'NONE',  ( -10.81189881249999729, -6.242252689847864744, -105.6562500020483952 ) ) ;
#40768 = ORIENTED_EDGE ( 'NONE', *, *, #28566, .T. ) ;
#40769 = CARTESIAN_POINT ( 'NONE',  ( -10.00000000000000000, -5.773502691896251982, -99.00000000409679046 ) ) ;
#40770 = CARTESIAN_POINT ( 'NONE',  ( 4.999999999999992006, -8.660254037844389075, -151.1250000040967905 ) ) ;
#40771 = CARTESIAN_POINT ( 'NONE',  ( 10.81189881249999729, 0.000000000000000000, -162.0312500020484094 ) ) ;
#40772 = CARTESIAN_POINT ( 'NONE',  ( 5.405949406249992428, -9.363379034771808662, -55.59375000204835970 ) ) ;
#40773 = VERTEX_POINT ( 'NONE', #40094 ) ;
#40774 = CARTESIAN_POINT ( 'NONE',  ( -4.999999999999996447, 8.660254037844387298, -25.49999999999996803 ) ) ;
#40775 = CARTESIAN_POINT ( 'NONE',  ( 5.000000000000000000, 8.660254037844385522, -11.12500000409674605 ) ) ;
#40776 = CARTESIAN_POINT ( 'NONE',  ( -10.81189881249999729, 6.242252689847871849, -33.90625000204836681 ) ) ;
#40777 = CARTESIAN_POINT ( 'NONE',  ( 5.000000000000000000, 8.660254037844385522, -159.2500000000000000 ) ) ;
#40778 = FACE_OUTER_BOUND ( 'NONE', #10788, .T. ) ;
#40779 = CARTESIAN_POINT ( 'NONE',  ( -2.121150477449813534E-15, -11.54700538379251284, -31.25000000409675494 ) ) ;
#40780 = VECTOR ( 'NONE', #21369, 1000.000000000000000 ) ;
#40781 = EDGE_CURVE ( 'NONE', #7470, #40028, #21476, .T. ) ;
#40782 = CARTESIAN_POINT ( 'NONE',  ( 5.405949406249992428, -9.363379034771808662, -130.7812500020483810 ) ) ;
#40783 = CARTESIAN_POINT ( 'NONE',  ( -4.638487482233418113, 8.887449022414848798, 2.775557561562891982E-14 ) ) ;
#40784 = ORIENTED_EDGE ( 'NONE', *, *, #19372, .F. ) ;
#40786 = VERTEX_POINT ( 'NONE', #17419 ) ;
#40785 = EDGE_LOOP ( 'NONE', ( #23184, #17006, #9682, #19087 ) ) ;
#40787 = DIRECTION ( 'NONE',  ( 0.000000000000000000, 0.000000000000000000, -1.000000000000000000 ) ) ;
#40788 = VECTOR ( 'NONE', #8251, 1000.000000000000000 ) ;
#40789 = CARTESIAN_POINT ( 'NONE',  ( 9.999999999999994671, -5.773502691896262640, -134.1250000000000000 ) ) ;
#40790 = CARTESIAN_POINT ( 'NONE',  ( 10.81189881249999551, -6.242252689847874514, -166.4687500020484094 ) ) ;
#40791 = CARTESIAN_POINT ( 'NONE',  ( 5.405949406249999534, 9.363379034771803333, -193.2812500020484094 ) ) ;
#40792 = CARTESIAN_POINT ( 'NONE',  ( -10.81189881249999729, 1.324075727343319199E-15, -12.59375000204834905 ) ) ;
#40793 = CARTESIAN_POINT ( 'NONE',  ( 9.999999999999998224, 0.000000000000000000, -22.99999999999996447 ) ) ;
#40794 = CARTESIAN_POINT ( 'NONE',  ( -10.81189881249999729, 6.242252689847871849, -149.2187500020484379 ) ) ;
#40795 = CARTESIAN_POINT ( 'NONE',  ( -5.405949406249996869, 9.363379034771805109, -137.3437500020484094 ) ) ;
#40796 = CARTESIAN_POINT ( 'NONE',  ( -2.293366432827344421E-15, -12.48450537969573659, -109.9062500020483952 ) ) ;
#40797 = CARTESIAN_POINT ( 'NONE',  ( 5.405949406249999534, 9.363379034771803333, -119.5937500020483810 ) ) ;
#40798 = CARTESIAN_POINT ( 'NONE',  ( -5.000000000000003553, -8.660254037844383745, -197.8750000040967905 ) ) ;
#40799 = CARTESIAN_POINT ( 'NONE',  ( -10.81189881249999907, -6.242252689847864744, -128.1562500020483810 ) ) ;
#40800 = CARTESIAN_POINT ( 'NONE',  ( -10.81189881249999729, 1.324075727343319199E-15, -5.093750002048369474 ) ) ;
#40801 = CARTESIAN_POINT ( 'NONE',  ( -5.405949406250003975, -9.363379034771801557, -132.3437500020484094 ) ) ;
#40802 = CARTESIAN_POINT ( 'NONE',  ( 9.999999999999998224, 0.000000000000000000, -81.87500000409676204 ) ) ;
#40803 = DIRECTION ( 'NONE',  ( -1.000000000000000000, 0.000000000000000000, 0.000000000000000000 ) ) ;
#40804 = CARTESIAN_POINT ( 'NONE',  ( -10.00000000000000000, -5.773502691896251982, -145.1250000000000284 ) ) ;
#40805 = CARTESIAN_POINT ( 'NONE',  ( -9.999999999999998224, 5.773502691896259087, -22.37499999999997868 ) ) ;
#40806 = VECTOR ( 'NONE', #7402, 1000.000000000000000 ) ;
#40807 = CARTESIAN_POINT ( 'NONE',  ( -10.81189881249999729, -6.242252689847864744, -75.46875000204836681 ) ) ;
#40808 = CARTESIAN_POINT ( 'NONE',  ( 10.81189881249999551, -6.242252689847874514, -67.46875000204838102 ) ) ;
#40809 = CARTESIAN_POINT ( 'NONE',  ( -9.999999999999742428, -5.773502691896402084, -159.0000000040967905 ) ) ;
#40810 = CARTESIAN_POINT ( 'NONE',  ( 10.81189881249999551, -6.242252689847874514, -36.15625000204835970 ) ) ;
#40811 = CARTESIAN_POINT ( 'NONE',  ( -2.293366432827344421E-15, -12.48450537969573659, -48.21875000204836681 ) ) ;
#40812 = CARTESIAN_POINT ( 'NONE',  ( -2.121150477449813534E-15, -11.54700538379251284, -163.2500000040968189 ) ) ;
#40813 = CARTESIAN_POINT ( 'NONE',  ( -10.81189881249999729, 1.324075727343319199E-15, -155.0937500020483810 ) ) ;
#40814 = CARTESIAN_POINT ( 'NONE',  ( -5.000000000000003553, -8.660254037844383745, -118.0000000000000000 ) ) ;
#40815 = CARTESIAN_POINT ( 'NONE',  ( 5.405949406249999534, 9.363379034771803333, -128.7812500020483810 ) ) ;
#40816 = CARTESIAN_POINT ( 'NONE',  ( -9.999999999999998224, 1.224646799147353059E-15, -67.62500000409676204 ) ) ;
#40817 = CARTESIAN_POINT ( 'NONE',  ( -2.121150477449813534E-15, -11.54700538379251284, -83.37499999999997158 ) ) ;
#40818 = CARTESIAN_POINT ( 'NONE',  ( -5.405949406250003975, -9.363379034771801557, -21.53125000204836326 ) ) ;
#40819 = VERTEX_POINT ( 'NONE', #36861 ) ;
#40820 = CARTESIAN_POINT ( 'NONE',  ( 10.81189881249999729, 6.242252689847867408, -106.4062500020483952 ) ) ;
#40821 = CARTESIAN_POINT ( 'NONE',  ( 4.999999999999992006, -8.660254037844389075, -124.1250000040967905 ) ) ;
#40822 = CARTESIAN_POINT ( 'NONE',  ( -9.999999999999998224, 1.224646799147353059E-15, -57.12500000409676204 ) ) ;
#40823 = CARTESIAN_POINT ( 'NONE',  ( -10.00000000000000000, -5.773502691896251982, -37.50000000409676204 ) ) ;
#40824 = CARTESIAN_POINT ( 'NONE',  ( -5.405949406250003975, -9.363379034771801557, -47.03125000204838813 ) ) ;
#40825 = CARTESIAN_POINT ( 'NONE',  ( 9.999999999999479527, 5.773502691896553074, -147.3750000000000000 ) ) ;
#40826 = CARTESIAN_POINT ( 'NONE',  ( 10.81189881249999907, 6.242252689847868297, -155.9062500020484094 ) ) ;
#40827 = CARTESIAN_POINT ( 'NONE',  ( -10.81189881249999907, -6.242252689847864744, -130.9687500020483810 ) ) ;
#40828 = CARTESIAN_POINT ( 'NONE',  ( 7.070501591499376803E-16, 11.54700538379251284, -104.0000000040967763 ) ) ;
#40829 = EDGE_LOOP ( 'NONE', ( #12837, #22974, #21934, #35086 ) ) ;
#40830 =( BOUNDED_CURVE ( )  B_SPLINE_CURVE ( 2, ( #3282, #16409, #30037, #13387, #26579, #39729, #13598 ),
 .UNSPECIFIED., .F., .F. ) 
 B_SPLINE_CURVE_WITH_KNOTS ( ( 3, 2, 2, 3 ),
 ( 0.3805970149253732338, 0.3818407960199006190, 0.3830845771144278933, 0.3843283582089552786 ),
 .UNSPECIFIED. ) 
 CURVE ( )  GEOMETRIC_REPRESENTATION_ITEM ( )  RATIONAL_B_SPLINE_CURVE ( ( 0.9999999999999880096, 0.8660254037844506980, 1.000000000000000000, 0.8660254037844387076, 1.000000000000000000, 0.8660254037844327124, 1.000000000000005995 ) ) 
 REPRESENTATION_ITEM ( '' )  );
#40831 = DIRECTION ( 'NONE',  ( 1.000000000000000000, 0.000000000000000000, 0.000000000000000000 ) ) ;
#40832 = EDGE_LOOP ( 'NONE', ( #22570, #17944, #32273, #41748 ) ) ;
#40833 = CIRCLE ( 'NONE', #35360, 25.00000000000000000 ) ;
#40834 = ORIENTED_EDGE ( 'NONE', *, *, #4286, .T. ) ;
#40836 = ORIENTED_EDGE ( 'NONE', *, *, #1914, .T. ) ;
#40835 = CARTESIAN_POINT ( 'NONE',  ( -5.405949406250003975, -9.363379034771801557, -114.3437500020483810 ) ) ;
#40837 = ADVANCED_FACE ( 'NONE', ( #6878 ), #1044, .T. ) ;
#40838 = DIRECTION ( 'NONE',  ( -0.000000000000000000, -0.000000000000000000, 1.000000000000000000 ) ) ;
#40839 = CARTESIAN_POINT ( 'NONE',  ( 7.644554776091147741E-16, 12.48450537969573659, -191.4687500020484094 ) ) ;
#40840 = CARTESIAN_POINT ( 'NONE',  ( -5.405949406250003975, -9.363379034771801557, -37.84375000204837391 ) ) ;
#40841 = CARTESIAN_POINT ( 'NONE',  ( 6.060903205933096061, -8.803638040079722060, -4.316514933816155161E-15 ) ) ;
#40842 = CARTESIAN_POINT ( 'NONE',  ( 10.00000000000051159, -5.773502691895965988, -74.12499999999995737 ) ) ;
#40843 = CARTESIAN_POINT ( 'NONE',  ( 5.405949406249992428, -9.363379034771808662, -169.5937500020484094 ) ) ;
#40844 = CARTESIAN_POINT ( 'NONE',  ( 10.81189881249999729, 0.000000000000000000, -160.3437500020484094 ) ) ;
#40845 = CARTESIAN_POINT ( 'NONE',  ( -9.999999999999998224, 1.224646799147353059E-15, -149.7500000000000000 ) ) ;
#40846 = CARTESIAN_POINT ( 'NONE',  ( 10.81189881249999551, -6.242252689847874514, -142.4687500020483810 ) ) ;
#40847 = CARTESIAN_POINT ( 'NONE',  ( 5.405949406249992428, -9.363379034771808662, -150.2812500020483810 ) ) ;
#40848 = CARTESIAN_POINT ( 'NONE',  ( -10.81189881249999729, 1.324075727343319199E-15, -153.5937500020483810 ) ) ;
#40849 = CARTESIAN_POINT ( 'NONE',  ( 9.999999999999998224, 0.000000000000000000, -42.49999999999998579 ) ) ;
#40850 = CARTESIAN_POINT ( 'NONE',  ( -9.999999999999998224, 1.224646799147353059E-15, -102.1250000040967905 ) ) ;
#40851 = CARTESIAN_POINT ( 'NONE',  ( -9.999999999999998224, 5.773502691896259087, -181.3750000000000000 ) ) ;
#40852 = CARTESIAN_POINT ( 'NONE',  ( 7.644554776091147741E-16, 12.48450537969573659, -89.46875000204838102 ) ) ;
#40853 = CARTESIAN_POINT ( 'NONE',  ( -9.999999999999998224, 0.000000000000000000, -99.99999999999998579 ) ) ;
#40854 = CARTESIAN_POINT ( 'NONE',  ( 10.81189881249999551, -6.242252689847874514, -55.65625000204836681 ) ) ;
#40855 = CARTESIAN_POINT ( 'NONE',  ( 10.81189881249999907, 6.242252689847868297, -179.7187500020484094 ) ) ;
#40856 = CARTESIAN_POINT ( 'NONE',  ( 5.405949406249999534, 9.363379034771803333, -118.2812500020483952 ) ) ;
#40857 = CARTESIAN_POINT ( 'NONE',  ( 10.81189881249999551, -6.242252689847874514, -157.6562500020484094 ) ) ;
#40858 = CARTESIAN_POINT ( 'NONE',  ( -9.999999999999998224, 1.224646799147353059E-15, -200.0000000000000000 ) ) ;
#40859 = CARTESIAN_POINT ( 'NONE',  ( 10.81189881249999551, -6.242252689847874514, -46.65625000204836681 ) ) ;
#40860 = CARTESIAN_POINT ( 'NONE',  ( 5.000000000000000000, 8.660254037844385522, -129.6250000040967620 ) ) ;
#40861 = CARTESIAN_POINT ( 'NONE',  ( 4.999999999999992006, -8.660254037844389075, -105.7499999999999858 ) ) ;
#40862 = VERTEX_POINT ( 'NONE', #23282 ) ;
#40863 = CARTESIAN_POINT ( 'NONE',  ( 5.405949406249992428, -9.363379034771808662, -126.2812500020483668 ) ) ;
#40864 = CARTESIAN_POINT ( 'NONE',  ( -4.999999999999996447, 8.660254037844387298, -144.3750000040967905 ) ) ;
#40865 = CARTESIAN_POINT ( 'NONE',  ( 9.999999999999998224, 0.000000000000000000, -68.37500000409677625 ) ) ;
#40866 = CARTESIAN_POINT ( 'NONE',  ( 5.405949406249999534, 9.363379034771803333, -181.2812500020483810 ) ) ;
#40867 = VERTEX_POINT ( 'NONE', #13747 ) ;
#40868 = CARTESIAN_POINT ( 'NONE',  ( 9.999999999999998224, 0.000000000000000000, -49.99999999999998579 ) ) ;
#40869 = CARTESIAN_POINT ( 'NONE',  ( -5.405949406250003975, -9.363379034771801557, -172.8437500020484094 ) ) ;
#40870 = CARTESIAN_POINT ( 'NONE',  ( 10.00000000000000000, 5.773502691896255534, -54.75000000409678336 ) ) ;
#40871 = FACE_OUTER_BOUND ( 'NONE', #6618, .T. ) ;
#40872 = DIRECTION ( 'NONE',  ( -0.000000000000000000, -0.000000000000000000, 1.000000000000000000 ) ) ;
#40873 = CARTESIAN_POINT ( 'NONE',  ( -10.81189881249999729, 1.324075727343319199E-15, -66.78125000204838102 ) ) ;
#40874 = CARTESIAN_POINT ( 'NONE',  ( 10.81189881249999729, 0.000000000000000000, -55.53125000204836681 ) ) ;
#40875 =( BOUNDED_CURVE ( )  B_SPLINE_CURVE ( 2, ( #23357, #274, #3078, #32443, #36088, #39315, #6946 ),
 .UNSPECIFIED., .F., .F. ) 
 B_SPLINE_CURVE_WITH_KNOTS ( ( 3, 2, 2, 3 ),
 ( 0.4328358208955225273, 0.4340796019900499125, 0.4353233830845772978, 0.4365671641791046276 ),
 .UNSPECIFIED. ) 
 CURVE ( )  GEOMETRIC_REPRESENTATION_ITEM ( )  RATIONAL_B_SPLINE_CURVE ( ( 0.9999999999999820144, 0.8660254037844566932, 1.000000000000000000, 0.8660254037844387076, 1.000000000000000000, 0.8660254037844207220, 1.000000000000017986 ) ) 
 REPRESENTATION_ITEM ( '' )  );
#40876 = CARTESIAN_POINT ( 'NONE',  ( 9.999999999999998224, 0.000000000000000000, -47.37500000409677625 ) ) ;
#40877 = CARTESIAN_POINT ( 'NONE',  ( -10.81189881249999729, 6.242252689847871849, -2.218750002048353043 ) ) ;
#40878 = CARTESIAN_POINT ( 'NONE',  ( -5.405949406250003975, -9.363379034771801557, -177.5312500020483810 ) ) ;
#40879 = CARTESIAN_POINT ( 'NONE',  ( 9.999999999999998224, 0.000000000000000000, -153.5000000000000000 ) ) ;
#40880 = CARTESIAN_POINT ( 'NONE',  ( -4.999999999999996447, 8.660254037844387298, -138.3750000040967905 ) ) ;
#40881 = ORIENTED_EDGE ( 'NONE', *, *, #40946, .T. ) ;
#40882 = CARTESIAN_POINT ( 'NONE',  ( -10.00000000000051337, 5.773502691895962435, -116.8749999999999858 ) ) ;
#40883 = DIRECTION ( 'NONE',  ( 0.000000000000000000, 0.000000000000000000, -1.000000000000000000 ) ) ;
#40885 = ORIENTED_EDGE ( 'NONE', *, *, #19089, .T. ) ;
#40884 = CARTESIAN_POINT ( 'NONE',  ( 5.405949406249999534, 9.363379034771803333, -86.78125000204838102 ) ) ;
#40886 =( LENGTH_UNIT ( ) NAMED_UNIT ( * ) SI_UNIT ( .MILLI., .METRE. ) );
#40888 = ORIENTED_EDGE ( 'NONE', *, *, #16988, .F. ) ;
#40887 = DIRECTION ( 'NONE',  ( -0.000000000000000000, -0.000000000000000000, -1.000000000000000000 ) ) ;
#40889 = ORIENTED_EDGE ( 'NONE', *, *, #1662, .T. ) ;
#40890 = CARTESIAN_POINT ( 'NONE',  ( -2.293366432827344421E-15, -12.48450537969573659, -39.21875000204835970 ) ) ;
#40891 = CARTESIAN_POINT ( 'NONE',  ( -5.405949406250003975, -9.363379034771801557, -27.34375000204835970 ) ) ;
#40892 = CARTESIAN_POINT ( 'NONE',  ( 10.81189881249999907, 6.242252689847868297, -11.90625000204835615 ) ) ;
#40894 = ORIENTED_EDGE ( 'NONE', *, *, #39777, .F. ) ;
#40893 = CARTESIAN_POINT ( 'NONE',  ( -10.81189881249999729, 6.242252689847871849, -65.21875000204838102 ) ) ;
#40895 = CARTESIAN_POINT ( 'NONE',  ( 0.000000000000000000, 0.000000000000000000, -200.0000000000000000 ) ) ;
#40896 = ADVANCED_FACE ( 'NONE', ( #30616 ), #29765, .T. ) ;
#40897 = CARTESIAN_POINT ( 'NONE',  ( -9.999999999999998224, 5.773502691896259087, -32.87499999999995737 ) ) ;
#40898 = CARTESIAN_POINT ( 'NONE',  ( 7.644554776091147741E-16, 12.48450537969573659, -188.4687500020484094 ) ) ;
#40899 = EDGE_CURVE ( 'NONE', #38354, #10167, #2455, .T. ) ;
#40900 = CARTESIAN_POINT ( 'NONE',  ( 10.81189881249999907, 6.242252689847868297, -169.2187500020483810 ) ) ;
#40901 = CARTESIAN_POINT ( 'NONE',  ( -10.81189881249999729, -6.242252689847864744, -178.9687500020484094 ) ) ;
#40902 = CARTESIAN_POINT ( 'NONE',  ( 7.070501591499376803E-16, 11.54700538379251284, -199.6250000000000284 ) ) ;
#40903 = DIRECTION ( 'NONE',  ( -1.000000000000000000, 0.000000000000000000, -0.000000000000000000 ) ) ;
#40904 = CARTESIAN_POINT ( 'NONE',  ( 9.999999999999479527, 5.773502691896553074, -104.2500000040967478 ) ) ;
#40905 = PLANE ( 'NONE',  #13607 ) ;
#40906 = CARTESIAN_POINT ( 'NONE',  ( 10.81189881249999551, -6.242252689847874514, -112.4687500020483810 ) ) ;
#40907 = DIRECTION ( 'NONE',  ( -0.000000000000000000, -1.000000000000000000, -0.000000000000000000 ) ) ;
#40908 = CARTESIAN_POINT ( 'NONE',  ( 10.81189881249999907, 6.242252689847868297, -79.40625000204839523 ) ) ;
#40909 = CARTESIAN_POINT ( 'NONE',  ( -10.81189881249999729, 6.242252689847871849, -101.2187500020483810 ) ) ;
#40910 = CARTESIAN_POINT ( 'NONE',  ( 7.644554776091147741E-16, 12.48450537969573659, -59.46875000204837391 ) ) ;
#40911 = CARTESIAN_POINT ( 'NONE',  ( -10.81189881249999729, 6.242252689847871849, -65.40625000204838102 ) ) ;
#40912 = CARTESIAN_POINT ( 'NONE',  ( -9.999999999999998224, 1.224646799147353059E-15, -157.6250000040967905 ) ) ;
#40913 = CARTESIAN_POINT ( 'NONE',  ( -9.999999999999998224, 5.773502691896259087, -131.8749999999999716 ) ) ;
#40914 = CARTESIAN_POINT ( 'NONE',  ( 10.81189881249999729, 6.242252689847867408, -152.9062500020483810 ) ) ;
#40915 = CARTESIAN_POINT ( 'NONE',  ( -10.81189881249999729, 1.324075727343319199E-15, -167.2812500020484094 ) ) ;
#40916 = CARTESIAN_POINT ( 'NONE',  ( -4.999999999999996447, 8.660254037844387298, -97.87500000409677625 ) ) ;
#40917 = CARTESIAN_POINT ( 'NONE',  ( 9.999999999999998224, 0.000000000000000000, -150.8750000040967905 ) ) ;
#40918 = CARTESIAN_POINT ( 'NONE',  ( 5.405949406249992428, -9.363379034771808662, -102.0937500020483810 ) ) ;
#40919 = CARTESIAN_POINT ( 'NONE',  ( -5.000000000000003553, -8.660254037844383745, -72.99999999999998579 ) ) ;
#40920 = CARTESIAN_POINT ( 'NONE',  ( -5.405949406249996869, 9.363379034771805109, -192.8437500020484094 ) ) ;
#40921 = CARTESIAN_POINT ( 'NONE',  ( 5.000000000000000000, 8.660254037844385522, -80.12500000409677625 ) ) ;
#40922 = CARTESIAN_POINT ( 'NONE',  ( -10.00000000000154188, 5.773502691895366468, -25.75000000409673362 ) ) ;
#40923 = CARTESIAN_POINT ( 'NONE',  ( 10.81189881249999729, 0.000000000000000000, -94.53125000204838102 ) ) ;
#40924 = CARTESIAN_POINT ( 'NONE',  ( 5.405949406249999534, 9.363379034771803333, -79.28125000204838102 ) ) ;
#40925 = CARTESIAN_POINT ( 'NONE',  ( -5.000000000000003553, -8.660254037844383745, -74.87500000409677625 ) ) ;
#40926 = CARTESIAN_POINT ( 'NONE',  ( 10.81189881249999907, 6.242252689847868297, -22.21875000204836681 ) ) ;
#40927 = ORIENTED_EDGE ( 'NONE', *, *, #24415, .F. ) ;
#40928 = CARTESIAN_POINT ( 'NONE',  ( 9.999999999999996447, -5.773502691896262640, -0.6249999999999709122 ) ) ;
#40929 = SHAPE_REPRESENTATION ( 'T-handle', ( #39998 ), #28294 ) ;
#40930 = CARTESIAN_POINT ( 'NONE',  ( 10.81189881249999729, 0.000000000000000000, -31.53125000204837391 ) ) ;
#40931 = CARTESIAN_POINT ( 'NONE',  ( 10.81189881249999729, 0.000000000000000000, -10.34375000204834549 ) ) ;
#40932 = CARTESIAN_POINT ( 'NONE',  ( -9.999999999999998224, 1.224646799147353059E-15, -64.62500000409676204 ) ) ;
#40933 = CARTESIAN_POINT ( 'NONE',  ( -5.000000000000003553, -8.660254037844383745, -4.375000004096768258 ) ) ;
#40934 = CARTESIAN_POINT ( 'NONE',  ( -10.81189881249999729, 6.242252689847871849, -126.9062500020483810 ) ) ;
#40935 = CARTESIAN_POINT ( 'NONE',  ( 4.999999999999992006, -8.660254037844389075, -185.2500000000000000 ) ) ;
#40936 = CYLINDRICAL_SURFACE ( 'NONE', #730, 9.999999999999998224 ) ;
#40938 = EDGE_LOOP ( 'NONE', ( #7471, #24836, #5184, #32109 ) ) ;
#40937 = CARTESIAN_POINT ( 'NONE',  ( -5.405949406249996869, 9.363379034771805109, -109.0312500020483810 ) ) ;
#40939 = CYLINDRICAL_SURFACE ( 'NONE', #19340, 5.000000000000002665 ) ;
#40940 = ORIENTED_EDGE ( 'NONE', *, *, #18399, .F. ) ;
#40941 = ORIENTED_EDGE ( 'NONE', *, *, #21192, .F. ) ;
#40942 = CARTESIAN_POINT ( 'NONE',  ( -10.81189881249999907, -6.242252689847864744, -39.65625000204835970 ) ) ;
#40943 = APPROVAL_STATUS ( 'not_yet_approved' ) ;
#40944 = CARTESIAN_POINT ( 'NONE',  ( 10.81189881249999729, 0.000000000000000000, -86.84375000204836681 ) ) ;
#40945 = CARTESIAN_POINT ( 'NONE',  ( -8.265208957352974318E-15, 145.0000000000000000, 37.49999999999997868 ) ) ;
#40946 = EDGE_CURVE ( 'NONE', #3072, #25696, #26727, .T. ) ;
#40947 = EDGE_CURVE ( 'NONE', #36017, #16045, #22870, .T. ) ;
#40948 = CARTESIAN_POINT ( 'NONE',  ( 6.372319074206731493, 8.485273278836908517, -99.99999999999994316 ) ) ;
#40949 = EDGE_CURVE ( 'NONE', #41097, #12174, #817, .T. ) ;
#40950 = ADVANCED_FACE ( 'NONE', ( #33002 ), #36651, .T. ) ;
#40951 = CARTESIAN_POINT ( 'NONE',  ( 5.405949406249992428, -9.363379034771808662, -160.7812500020484094 ) ) ;
#40952 = CARTESIAN_POINT ( 'NONE',  ( -4.999999999999996447, 8.660254037844387298, -138.0000000000000000 ) ) ;
#40953 = CARTESIAN_POINT ( 'NONE',  ( 5.405949406249999534, 9.363379034771803333, -122.5937500020483952 ) ) ;
#40954 = APPROVAL ( #5358, 'UNSPECIFIED' ) ;
#40955 = CARTESIAN_POINT ( 'NONE',  ( 10.81189881249999551, -6.242252689847874514, -88.46875000204836681 ) ) ;
#40956 = CARTESIAN_POINT ( 'NONE',  ( 7.644554776091147741E-16, 12.48450537969573659, -4.156250002048351710 ) ) ;
#40957 = CARTESIAN_POINT ( 'NONE',  ( -5.405949406250003975, -9.363379034771801557, -196.8437500020484094 ) ) ;
#40958 = CARTESIAN_POINT ( 'NONE',  ( 5.405949406249999534, 9.363379034771803333, -95.78125000204838102 ) ) ;
#40959 = CARTESIAN_POINT ( 'NONE',  ( 9.999999999999996447, -5.773502691896262640, -179.5000000040968189 ) ) ;
#40960 = CARTESIAN_POINT ( 'NONE',  ( -10.81189881249999729, -6.242252689847864744, -167.1562500020484094 ) ) ;
#40961 = CARTESIAN_POINT ( 'NONE',  ( -9.999999999998456346, -5.773502691897145489, -28.50000000409671230 ) ) ;
#40962 = CARTESIAN_POINT ( 'NONE',  ( 5.405949406249999534, 9.363379034771803333, -170.7812500020484094 ) ) ;
#40963 = CARTESIAN_POINT ( 'NONE',  ( -2.293366432827344421E-15, -12.48450537969573659, -189.4062500020484094 ) ) ;
#40964 = CARTESIAN_POINT ( 'NONE',  ( -5.405949406250003975, -9.363379034771801557, -55.84375000204835970 ) ) ;
#40965 = CARTESIAN_POINT ( 'NONE',  ( -10.00000000000000000, -5.773502691896251982, -172.5000000040967905 ) ) ;
#40966 = CARTESIAN_POINT ( 'NONE',  ( -5.405949406250003975, -9.363379034771801557, -14.03125000204835615 ) ) ;
#40967 = CARTESIAN_POINT ( 'NONE',  ( 10.81189881249999551, -6.242252689847874514, -25.46875000204837391 ) ) ;
#40968 = CARTESIAN_POINT ( 'NONE',  ( -9.999999999999998224, 1.224646799147353059E-15, -125.7499999999999716 ) ) ;
#40969 = CARTESIAN_POINT ( 'NONE',  ( -10.81189881249999729, 1.324075727343319199E-15, -119.0937500020483810 ) ) ;
#40970 = CARTESIAN_POINT ( 'NONE',  ( 5.000000000000000000, 8.660254037844385522, -100.7499999999999858 ) ) ;
#40971 = CARTESIAN_POINT ( 'NONE',  ( -10.81189881249999907, -6.242252689847864744, -30.65625000204835970 ) ) ;
#40972 = CARTESIAN_POINT ( 'NONE',  ( 9.999999999999998224, 0.000000000000000000, -105.8750000040967763 ) ) ;
#40973 = CARTESIAN_POINT ( 'NONE',  ( 4.999999999999992006, -8.660254037844389075, -190.1250000040967905 ) ) ;
#40974 = CARTESIAN_POINT ( 'NONE',  ( 4.999999999999992006, -8.660254037844389075, -53.24999999999996447 ) ) ;
#40975 = CARTESIAN_POINT ( 'NONE',  ( -10.81189881249999729, 1.324075727343319199E-15, -128.2812500020483810 ) ) ;
#40976 = CARTESIAN_POINT ( 'NONE',  ( -10.81189881249999729, 1.324075727343319199E-15, -96.78125000204839523 ) ) ;
#40977 = ORIENTED_EDGE ( 'NONE', *, *, #303, .T. ) ;
#40978 = AXIS2_PLACEMENT_3D ( 'NONE', #39033, #22637, #10095 ) ;
#40979 = CARTESIAN_POINT ( 'NONE',  ( 10.00000000000000000, 5.773502691896255534, -96.75000000409679046 ) ) ;
#40980 = DIRECTION ( 'NONE',  ( -0.000000000000000000, -0.000000000000000000, -1.000000000000000000 ) ) ;
#40981 = CARTESIAN_POINT ( 'NONE',  ( -10.81189881249999907, -6.242252689847864744, -164.1562500020484094 ) ) ;
#40982 = CARTESIAN_POINT ( 'NONE',  ( -10.81189881249999729, 6.242252689847871849, -59.21875000204837391 ) ) ;
#40984 = EDGE_CURVE ( 'NONE', #30365, #38772, #24261, .T. ) ;
#40983 = ORIENTED_EDGE ( 'NONE', *, *, #31744, .T. ) ;
#40985 = CARTESIAN_POINT ( 'NONE',  ( 4.999999999999992006, -8.660254037844389075, -24.74999999999996803 ) ) ;
#40986 = CARTESIAN_POINT ( 'NONE',  ( 5.405949406249999534, 9.363379034771803333, -31.28125000204837036 ) ) ;
#40987 = CARTESIAN_POINT ( 'NONE',  ( -10.00000000000000000, -5.773502691896251982, -158.6250000000000284 ) ) ;
#40988 = FACE_OUTER_BOUND ( 'NONE', #20289, .T. ) ;
#40989 = CARTESIAN_POINT ( 'NONE',  ( 9.999999999999998224, 0.000000000000000000, -30.87500000409676559 ) ) ;
#40990 = CARTESIAN_POINT ( 'NONE',  ( -9.999999999998969713, -5.773502691896847949, -23.62499999999995737 ) ) ;
#40991 = CARTESIAN_POINT ( 'NONE',  ( -2.293366432827344421E-15, -12.48450537969573659, -133.9062500020483810 ) ) ;
#40992 = CARTESIAN_POINT ( 'NONE',  ( -10.00000000000051337, 5.773502691895962435, -139.7500000040967905 ) ) ;
#40993 = VERTEX_POINT ( 'NONE', #18068 ) ;
#40994 =( BOUNDED_CURVE ( )  B_SPLINE_CURVE ( 2, ( #18884, #19292, #31641, #32486, #12388, #38310, #11970 ),
 .UNSPECIFIED., .F., .F. ) 
 B_SPLINE_CURVE_WITH_KNOTS ( ( 3, 2, 2, 3 ),
 ( 0.04850746268656720706, 0.04975124378109457846, 0.05099502487562193598, 0.05223880597014930738 ),
 .UNSPECIFIED. ) 
 CURVE ( )  GEOMETRIC_REPRESENTATION_ITEM ( )  RATIONAL_B_SPLINE_CURVE ( ( 0.9999999999999955591, 0.8660254037844431485, 1.000000000000000000, 0.8660254037844387076, 1.000000000000000000, 0.8660254037844327124, 1.000000000000005995 ) ) 
 REPRESENTATION_ITEM ( '' )  );
#40995 = CARTESIAN_POINT ( 'NONE',  ( 5.405949406249992428, -9.363379034771808662, -61.78125000204837391 ) ) ;
#40997 = ORIENTED_EDGE ( 'NONE', *, *, #38893, .T. ) ;
#40996 = ORIENTED_EDGE ( 'NONE', *, *, #16948, .T. ) ;
#40998 = CARTESIAN_POINT ( 'NONE',  ( 9.999999999999998224, 0.000000000000000000, -177.5000000000000000 ) ) ;
#40999 = DIRECTION ( 'NONE',  ( -0.000000000000000000, -0.000000000000000000, 1.000000000000000000 ) ) ;
#41000 = CARTESIAN_POINT ( 'NONE',  ( -10.81189881249999729, 1.324075727343319199E-15, -159.5937500020484094 ) ) ;
#41001 = CARTESIAN_POINT ( 'NONE',  ( 10.81189881249999551, -6.242252689847874514, -190.6562500020484094 ) ) ;
#41002 = CARTESIAN_POINT ( 'NONE',  ( -5.405949406249996869, 9.363379034771805109, -18.84375000204835260 ) ) ;
#41003 = CARTESIAN_POINT ( 'NONE',  ( 9.999999999999742428, 5.773502691896404748, -129.3750000000000000 ) ) ;
#41004 = CARTESIAN_POINT ( 'NONE',  ( -2.293366432827344421E-15, -12.48450537969573659, -150.2187500020484094 ) ) ;
#41005 = CARTESIAN_POINT ( 'NONE',  ( 10.81189881249999729, 0.000000000000000000, -128.8437500020484094 ) ) ;
#41006 = CARTESIAN_POINT ( 'NONE',  ( -10.81189881249999729, 6.242252689847871849, -104.4062500020483810 ) ) ;
#41007 = CARTESIAN_POINT ( 'NONE',  ( 10.81189881249999729, 0.000000000000000000, -112.3437500020483810 ) ) ;
#41008 = CARTESIAN_POINT ( 'NONE',  ( -10.81189881249999907, -6.242252689847864744, -123.6562500020484094 ) ) ;
#41009 = CARTESIAN_POINT ( 'NONE',  ( -5.405949406250003975, -9.363379034771801557, -0.3437500020483652552 ) ) ;
#41010 = CARTESIAN_POINT ( 'NONE',  ( -5.405949406249996869, 9.363379034771805109, -132.8437500020484094 ) ) ;
#41011 = CARTESIAN_POINT ( 'NONE',  ( -9.999999999999998224, 1.224646799147353059E-15, -164.7500000000000000 ) ) ;
#41012 = CYLINDRICAL_SURFACE ( 'NONE', #4076, 9.999999999999998224 ) ;
#41013 = CARTESIAN_POINT ( 'NONE',  ( 4.999999999999992006, -8.660254037844389075, -147.7500000000000000 ) ) ;
#41014 = CARTESIAN_POINT ( 'NONE',  ( 10.00000000000000000, 5.773502691896255534, -24.37499999999997868 ) ) ;
#41015 = EDGE_CURVE ( 'NONE', #5685, #16734, #11162, .T. ) ;
#41016 = CARTESIAN_POINT ( 'NONE',  ( 7.644554776091147741E-16, 12.48450537969573659, -78.96875000204838102 ) ) ;
#41017 = CARTESIAN_POINT ( 'NONE',  ( -10.81189881249999729, 6.242252689847871849, -60.71875000204838102 ) ) ;
#41018 = CARTESIAN_POINT ( 'NONE',  ( -9.999999999999998224, 1.224646799147353059E-15, -145.2500000000000000 ) ) ;
#41019 = CARTESIAN_POINT ( 'NONE',  ( 10.81189881249999729, 0.000000000000000000, -36.03125000204837391 ) ) ;
#41020 = CARTESIAN_POINT ( 'NONE',  ( 10.81189881249999907, 6.242252689847868297, -47.71875000204835970 ) ) ;
#41021 = CYLINDRICAL_SURFACE ( 'NONE', #3354, 9.999999999999998224 ) ;
#41022 = CARTESIAN_POINT ( 'NONE',  ( 5.405949406249999534, 9.363379034771803333, -155.5937500020483810 ) ) ;
#41023 = CARTESIAN_POINT ( 'NONE',  ( -9.999999999999998224, 5.773502691896259087, -121.3750000000000000 ) ) ;
#41024 = CARTESIAN_POINT ( 'NONE',  ( -2.121150477449813534E-15, -11.54700538379251284, -187.2500000040967905 ) ) ;
#41025 = VECTOR ( 'NONE', #5908, 1000.000000000000000 ) ;
#41026 = CARTESIAN_POINT ( 'NONE',  ( -9.999999999999998224, 5.773502691896259087, -73.37499999999997158 ) ) ;
#41027 = CARTESIAN_POINT ( 'NONE',  ( 10.81189881249999551, -6.242252689847874514, -9.156250002048375691 ) ) ;
#41028 = ORIENTED_EDGE ( 'NONE', *, *, #30335, .F. ) ;
#41029 = CARTESIAN_POINT ( 'NONE',  ( -2.293366432827344421E-15, -12.48450537969573659, -103.9062500020483810 ) ) ;
#41030 = CARTESIAN_POINT ( 'NONE',  ( 4.999999999999992006, -8.660254037844389075, -122.6250000040967905 ) ) ;
#41031 = CARTESIAN_POINT ( 'NONE',  ( -2.121150477449813534E-15, -11.54700538379251284, -179.7500000040967905 ) ) ;
#41032 = CARTESIAN_POINT ( 'NONE',  ( -5.405949406249996869, 9.363379034771805109, -81.84375000204838102 ) ) ;
#41033 = CARTESIAN_POINT ( 'NONE',  ( -5.000000000000003553, -8.660254037844383745, -35.87500000409676915 ) ) ;
#41034 = CARTESIAN_POINT ( 'NONE',  ( -10.00000000000076916, 5.773502691895813221, -130.3750000000000000 ) ) ;
#41035 = CARTESIAN_POINT ( 'NONE',  ( -10.81189881249999907, -6.242252689847864744, -44.15625000204837391 ) ) ;
#41036 = CARTESIAN_POINT ( 'NONE',  ( -9.999999999999998224, 1.224646799147353059E-15, -137.7499999999999716 ) ) ;
#41037 = CARTESIAN_POINT ( 'NONE',  ( -10.81189881249999729, 6.242252689847871849, -153.9062500020483810 ) ) ;
#41038 = CARTESIAN_POINT ( 'NONE',  ( -5.405949406250003975, -9.363379034771801557, -129.3437500020484094 ) ) ;
#41039 = CARTESIAN_POINT ( 'NONE',  ( 9.999999999999479527, 5.773502691896553074, -104.2500000040967478 ) ) ;
#41040 = VERTEX_POINT ( 'NONE', #24361 ) ;
#41041 = DIRECTION ( 'NONE',  ( -0.000000000000000000, -0.000000000000000000, 1.000000000000000000 ) ) ;
#41042 = ORIENTED_EDGE ( 'NONE', *, *, #4875, .F. ) ;
#41043 = ORIENTED_EDGE ( 'NONE', *, *, #40356, .F. ) ;
#41044 = VERTEX_POINT ( 'NONE', #18281 ) ;
#41045 = CARTESIAN_POINT ( 'NONE',  ( -9.999999999999998224, 1.224646799147353059E-15, -104.7499999999999858 ) ) ;
#41046 = CARTESIAN_POINT ( 'NONE',  ( 10.81189881249999729, 0.000000000000000000, -191.8437500020484094 ) ) ;
#41047 = CARTESIAN_POINT ( 'NONE',  ( -10.81189881249999907, -6.242252689847864744, -39.46875000204835970 ) ) ;
#41048 = CARTESIAN_POINT ( 'NONE',  ( -7.071067811865472841, -7.071067811865472841, -200.0000000000000000 ) ) ;
#41049 = CARTESIAN_POINT ( 'NONE',  ( -9.999999999999998224, 1.224646799147353059E-15, -177.1250000040968189 ) ) ;
#41050 = CARTESIAN_POINT ( 'NONE',  ( -10.81189881249999729, -6.242252689847864744, -169.9687500020483526 ) ) ;
#41051 = AXIS2_PLACEMENT_3D ( 'NONE', #19834, #26956, #227 ) ;
#41052 = CARTESIAN_POINT ( 'NONE',  ( -5.405949406250003975, -9.363379034771801557, -150.3437500020483810 ) ) ;
#41053 = CARTESIAN_POINT ( 'NONE',  ( -5.000000000000003553, -8.660254037844383745, -122.8750000040967905 ) ) ;
#41054 = CARTESIAN_POINT ( 'NONE',  ( 5.405949406249992428, -9.363379034771808662, -142.5937500020483810 ) ) ;
#41055 = CARTESIAN_POINT ( 'NONE',  ( -10.81189881249999907, -6.242252689847864744, -149.1562500020483810 ) ) ;
#41056 = CARTESIAN_POINT ( 'NONE',  ( 5.405949406249992428, -9.363379034771808662, -156.0937500020483810 ) ) ;
#41057 = CARTESIAN_POINT ( 'NONE',  ( -9.999999999998969713, -5.773502691896847949, -43.12499999999995737 ) ) ;
#41058 = DIRECTION ( 'NONE',  ( -1.000000000000000000, 0.000000000000000000, 0.000000000000000000 ) ) ;
#41059 = CARTESIAN_POINT ( 'NONE',  ( -4.999999999999996447, 8.660254037844387298, -172.5000000000000284 ) ) ;
#41060 = CARTESIAN_POINT ( 'NONE',  ( 10.81189881249999551, -6.242252689847874514, -89.96875000204838102 ) ) ;
#41061 = CARTESIAN_POINT ( 'NONE',  ( 5.405949406249992428, -9.363379034771808662, -61.78125000204837391 ) ) ;
#41062 = CARTESIAN_POINT ( 'NONE',  ( -5.000000000000003553, -8.660254037844383745, -99.99999999999998579 ) ) ;
#41063 = CARTESIAN_POINT ( 'NONE',  ( 5.405949406249992428, -9.363379034771808662, -178.5937500020484094 ) ) ;
#41064 = CARTESIAN_POINT ( 'NONE',  ( 10.81189881249999551, -6.242252689847874514, -111.1562500020483952 ) ) ;
#41065 = CARTESIAN_POINT ( 'NONE',  ( -10.81189881249999729, 1.324075727343319199E-15, -152.2812500020484094 ) ) ;
#41066 = CARTESIAN_POINT ( 'NONE',  ( -9.999999999998456346, -5.773502691897145489, -11.62499999999992184 ) ) ;
#41067 = CARTESIAN_POINT ( 'NONE',  ( -2.293366432827344421E-15, -12.48450537969573659, -40.90625000204836681 ) ) ;
#41068 = CARTESIAN_POINT ( 'NONE',  ( -5.000000000000003553, -8.660254037844383745, -128.8750000040967905 ) ) ;
#41069 = CARTESIAN_POINT ( 'NONE',  ( 5.000000000000000000, 8.660254037844385522, -102.2500000000000000 ) ) ;
#41070 = VERTEX_POINT ( 'NONE', #21310 ) ;
#41071 = CARTESIAN_POINT ( 'NONE',  ( 7.644554776091147741E-16, 12.48450537969573659, -127.1562500020483810 ) ) ;
#41072 = CARTESIAN_POINT ( 'NONE',  ( -4.999999999999996447, 8.660254037844387298, -151.8750000040967905 ) ) ;
#41073 = CARTESIAN_POINT ( 'NONE',  ( -9.999999999999998224, 1.224646799147353059E-15, -192.1250000040967905 ) ) ;
#41074 = CARTESIAN_POINT ( 'NONE',  ( -10.81189881249999907, -6.242252689847864744, -180.6562500020484094 ) ) ;
#41075 = ORIENTED_EDGE ( 'NONE', *, *, #28211, .F. ) ;
#41076 = CARTESIAN_POINT ( 'NONE',  ( -2.293366432827344421E-15, -12.48450537969573659, -175.7187500020483810 ) ) ;
#41077 = CARTESIAN_POINT ( 'NONE',  ( -10.00000000000000000, -5.773502691896251982, -60.00000000409676915 ) ) ;
#41078 = CARTESIAN_POINT ( 'NONE',  ( -9.999999999998456346, -5.773502691897145489, -19.12499999999994316 ) ) ;
#41079 =( BOUNDED_CURVE ( )  B_SPLINE_CURVE ( 2, ( #32555, #26283, #23041, #39435, #23472, #181, #36413 ),
 .UNSPECIFIED., .F., .F. ) 
 B_SPLINE_CURVE_WITH_KNOTS ( ( 3, 2, 2, 3 ),
 ( 0.7388059701492539766, 0.7400497512437813619, 0.7412935323383087471, 0.7425373134328361324 ),
 .UNSPECIFIED. ) 
 CURVE ( )  GEOMETRIC_REPRESENTATION_ITEM ( )  RATIONAL_B_SPLINE_CURVE ( ( 0.9999999999999761302, 0.8660254037844625774, 1.000000000000000000, 0.8660254037844387076, 1.000000000000000000, 0.8660254037844028474, 1.000000000000035971 ) ) 
 REPRESENTATION_ITEM ( '' )  );
#41080 = CARTESIAN_POINT ( 'NONE',  ( 9.999999999999998224, 0.000000000000000000, -135.8750000040967905 ) ) ;
#41081 = CARTESIAN_POINT ( 'NONE',  ( 10.81189881249999729, 0.000000000000000000, -70.53125000204838102 ) ) ;
#41082 = CARTESIAN_POINT ( 'NONE',  ( 5.405949406249999534, 9.363379034771803333, -49.28125000204838813 ) ) ;
#41083 = EDGE_CURVE ( 'NONE', #26629, #8170, #9374, .T. ) ;
#41084 = CARTESIAN_POINT ( 'NONE',  ( -10.00000000000000000, -5.773502691896251982, -45.00000000409676204 ) ) ;
#41085 = CARTESIAN_POINT ( 'NONE',  ( -5.405949406250003975, -9.363379034771801557, -4.843750002048369474 ) ) ;
#41086 = CARTESIAN_POINT ( 'NONE',  ( -5.000000000000003553, -8.660254037844383745, -29.87500000409676204 ) ) ;
#41087 = CARTESIAN_POINT ( 'NONE',  ( -5.405949406249996869, 9.363379034771805109, -181.0312500020483810 ) ) ;
#41088 = DIRECTION ( 'NONE',  ( -0.000000000000000000, -0.000000000000000000, 1.000000000000000000 ) ) ;
#41089 = DIRECTION ( 'NONE',  ( 1.000000000000000000, 0.000000000000000000, 0.000000000000000000 ) ) ;
#41090 = VERTEX_POINT ( 'NONE', #1690 ) ;
#41091 = CARTESIAN_POINT ( 'NONE',  ( -5.000000000000003553, -8.660254037844383745, -0.9999999999999731326 ) ) ;
#41092 = DIRECTION ( 'NONE',  ( 1.000000000000000000, 0.000000000000000000, 0.000000000000000000 ) ) ;
#41093 = DIRECTION ( 'NONE',  ( -0.000000000000000000, -0.000000000000000000, 1.000000000000000000 ) ) ;
#41095 = EDGE_LOOP ( 'NONE', ( #40252, #21105, #23458, #20547 ) ) ;
#41094 = CARTESIAN_POINT ( 'NONE',  ( 10.81189881249999907, 6.242252689847868297, -89.90625000204839523 ) ) ;
#41097 = VERTEX_POINT ( 'NONE', #34923 ) ;
#41096 = DIRECTION ( 'NONE',  ( 1.000000000000000000, -0.000000000000000000, -0.000000000000000000 ) ) ;
#41098 = VERTEX_POINT ( 'NONE', #25006 ) ;
#41099 = CARTESIAN_POINT ( 'NONE',  ( 10.81189881249999551, -6.242252689847874514, -37.46875000204836681 ) ) ;
#41100 = LINE ( 'NONE', #22550, #1100 ) ;
#41101 = CARTESIAN_POINT ( 'NONE',  ( 5.405949406249999534, 9.363379034771803333, -11.78125000204835438 ) ) ;
#41103 = ORIENTED_EDGE ( 'NONE', *, *, #35465, .F. ) ;
#41102 = CARTESIAN_POINT ( 'NONE',  ( -2.293366432827344421E-15, -12.48450537969573659, -60.21875000204837391 ) ) ;
#41104 = CARTESIAN_POINT ( 'NONE',  ( -99.99999999999994316, -40.00000000000000711, -170.0000000000000000 ) ) ;
#41105 = EDGE_CURVE ( 'NONE', #38843, #17527, #14264, .T. ) ;
#41106 = CARTESIAN_POINT ( 'NONE',  ( 10.00000000000000000, 5.773502691896255534, -39.37499999999996447 ) ) ;
#41107 = CARTESIAN_POINT ( 'NONE',  ( 10.81189881249999907, 6.242252689847868297, -182.7187500020484094 ) ) ;
#41108 = CARTESIAN_POINT ( 'NONE',  ( 5.405949406249992428, -9.363379034771808662, -169.5937500020484094 ) ) ;
#41110 = EDGE_CURVE ( 'NONE', #22821, #31054, #4978, .T. ) ;
#41109 = CARTESIAN_POINT ( 'NONE',  ( 7.644554776091147741E-16, 12.48450537969573659, -179.4687500020484094 ) ) ;
#41111 = CARTESIAN_POINT ( 'NONE',  ( -10.00000000000102496, 5.773502691895664007, -131.8749999999999432 ) ) ;
#41112 = CARTESIAN_POINT ( 'NONE',  ( 9.999999999999998224, 0.000000000000000000, -140.0000000000000000 ) ) ;
#41113 = CARTESIAN_POINT ( 'NONE',  ( -5.000000000000003553, -8.660254037844383745, -20.87500000409675494 ) ) ;
#41114 = CARTESIAN_POINT ( 'NONE',  ( 4.999999999999992006, -8.660254037844389075, -197.2500000000000000 ) ) ;
#41115 = CARTESIAN_POINT ( 'NONE',  ( 10.81189881249999551, -6.242252689847874514, -115.4687500020483810 ) ) ;
#41116 = LINE ( 'NONE', #11555, #20423 ) ;
#41117 = CLOSED_SHELL ( 'NONE', ( #32505, #40305, #22512, #18565, #22009, #31262, #38345, #28755, #5414, #4161, #5412, #13757, #23614, #26991 ) ) ;
#41118 = CARTESIAN_POINT ( 'NONE',  ( -5.405949406250003975, -9.363379034771801557, -78.53125000204838102 ) ) ;
#41119 = CARTESIAN_POINT ( 'NONE',  ( -5.405949406250003975, -9.363379034771801557, -91.84375000204838102 ) ) ;
#41120 = CARTESIAN_POINT ( 'NONE',  ( -5.405949406250003975, -9.363379034771801557, -61.84375000204836681 ) ) ;
#41121 = CARTESIAN_POINT ( 'NONE',  ( -5.405949406249996869, 9.363379034771805109, -67.03125000204838102 ) ) ;
#41122 = CARTESIAN_POINT ( 'NONE',  ( 9.999999999999998224, 0.000000000000000000, -150.8750000040967905 ) ) ;
#41123 = CARTESIAN_POINT ( 'NONE',  ( 7.070501591499377789E-16, 11.54700538379251284, -127.6249999999999858 ) ) ;
#41124 =( BOUNDED_CURVE ( )  B_SPLINE_CURVE ( 2, ( #34233, #578, #4226, #23877, #4649, #27104, #787 ),
 .UNSPECIFIED., .F., .F. ) 
 B_SPLINE_CURVE_WITH_KNOTS ( ( 3, 2, 2, 3 ),
 ( 0.4738805970149255198, 0.4751243781094529051, 0.4763681592039803459, 0.4776119402985076756 ),
 .UNSPECIFIED. ) 
 CURVE ( )  GEOMETRIC_REPRESENTATION_ITEM ( )  RATIONAL_B_SPLINE_CURVE ( ( 0.9999999999999820144, 0.8660254037844566932, 1.000000000000000000, 0.8660254037844387076, 1.000000000000000000, 0.8660254037844148378, 1.000000000000023981 ) ) 
 REPRESENTATION_ITEM ( '' )  );
#41125 = CARTESIAN_POINT ( 'NONE',  ( 7.644554776091147741E-16, 12.48450537969573659, -148.1562500020484094 ) ) ;
#41126 = CARTESIAN_POINT ( 'NONE',  ( -2.293366432827344421E-15, -12.48450537969573659, -165.4062500020483810 ) ) ;
#41127 = DIRECTION ( 'NONE',  ( -0.000000000000000000, -0.000000000000000000, -1.000000000000000000 ) ) ;
#41128 = CARTESIAN_POINT ( 'NONE',  ( 0.000000000000000000, 0.000000000000000000, -200.0000000000000000 ) ) ;
#41129 = CARTESIAN_POINT ( 'NONE',  ( -10.81189881249999907, -6.242252689847864744, -96.46875000204838102 ) ) ;
#41130 = CARTESIAN_POINT ( 'NONE',  ( 9.999999999999998224, 0.000000000000000000, -42.87500000409677625 ) ) ;
#41131 = CARTESIAN_POINT ( 'NONE',  ( 4.999999999999992006, -8.660254037844389075, -71.24999999999998579 ) ) ;
#41132 = CARTESIAN_POINT ( 'NONE',  ( 5.405949406249999534, 9.363379034771803333, -196.0937500020484094 ) ) ;
#41133 = CARTESIAN_POINT ( 'NONE',  ( 10.00000000000000000, 5.773502691896255534, -78.75000000409679046 ) ) ;
#41134 = CARTESIAN_POINT ( 'NONE',  ( 10.81189881249999551, -6.242252689847874514, -94.65625000204838102 ) ) ;
#41135 = CARTESIAN_POINT ( 'NONE',  ( 10.81189881249999729, 0.000000000000000000, -73.53125000204838102 ) ) ;
#41136 =( BOUNDED_CURVE ( )  B_SPLINE_CURVE ( 2, ( #7138, #36698, #22913, #20502, #29597, #10154, #32839 ),
 .UNSPECIFIED., .F., .F. ) 
 B_SPLINE_CURVE_WITH_KNOTS ( ( 3, 2, 2, 3 ),
 ( 0.4850746268656717652, 0.4863184079601990950, 0.4875621890547264248, 0.4888059701492538101 ),
 .UNSPECIFIED. ) 
 CURVE ( )  GEOMETRIC_REPRESENTATION_ITEM ( )  RATIONAL_B_SPLINE_CURVE ( ( 0.9999999999999880096, 0.8660254037844506980, 1.000000000000000000, 0.8660254037844387076, 1.000000000000000000, 0.8660254037844327124, 1.000000000000005995 ) ) 
 REPRESENTATION_ITEM ( '' )  );
#41137 = CARTESIAN_POINT ( 'NONE',  ( 5.000000000000000000, 8.660254037844385522, -69.62500000409677625 ) ) ;
#41138 = CARTESIAN_POINT ( 'NONE',  ( -9.999999999999998224, 1.224646799147353059E-15, -59.74999999999997158 ) ) ;
#41139 = CARTESIAN_POINT ( 'NONE',  ( 7.644554776091147741E-16, 12.48450537969573659, -27.96875000204837747 ) ) ;
#41140 = EDGE_LOOP ( 'NONE', ( #25398, #6184, #9002, #25164 ) ) ;
#41141 = CARTESIAN_POINT ( 'NONE',  ( -5.000000000000003553, -8.660254037844383745, -0.9999999999999731326 ) ) ;
#41142 = CARTESIAN_POINT ( 'NONE',  ( 10.81189881249999907, 6.242252689847868297, -17.90625000204837391 ) ) ;
#41143 = ADVANCED_FACE ( 'NONE', ( #27584, #40722 ), #24572, .T. ) ;
#41144 = CARTESIAN_POINT ( 'NONE',  ( 10.81189881249999551, -6.242252689847874514, -13.46875000204836326 ) ) ;
#41145 = DIRECTION ( 'NONE',  ( -1.000000000000000000, 0.000000000000000000, -0.000000000000000000 ) ) ;
#41146 = CARTESIAN_POINT ( 'NONE',  ( 10.81189881249999907, 6.242252689847868297, -143.7187500020483810 ) ) ;
#41147 = CARTESIAN_POINT ( 'NONE',  ( -9.999999999999998224, 1.224646799147353059E-15, -66.12500000409676204 ) ) ;
#41148 = CARTESIAN_POINT ( 'NONE',  ( -10.00000000000025580, 5.773502691896109873, -151.7500000040967336 ) ) ;
#41149 = CARTESIAN_POINT ( 'NONE',  ( -10.81189881249999907, -6.242252689847864744, -132.6562500020484094 ) ) ;
#41150 = CARTESIAN_POINT ( 'NONE',  ( 5.000000000000000000, 8.660254037844385522, -181.7500000000000000 ) ) ;
#41151 = CARTESIAN_POINT ( 'NONE',  ( 4.999999999999992006, -8.660254037844389075, -35.62500000409676915 ) ) ;
#41153 = ORIENTED_EDGE ( 'NONE', *, *, #3222, .F. ) ;
#41152 = CARTESIAN_POINT ( 'NONE',  ( 10.81189881249999907, 6.242252689847868297, -110.9062500020483952 ) ) ;
#41154 = CARTESIAN_POINT ( 'NONE',  ( 4.999999999999992006, -8.660254037844389075, -154.1250000040967905 ) ) ;
#41155 = ORIENTED_EDGE ( 'NONE', *, *, #3091, .F. ) ;
#41156 = ORIENTED_EDGE ( 'NONE', *, *, #40070, .F. ) ;
#41157 = CARTESIAN_POINT ( 'NONE',  ( -10.81189881249999729, 6.242252689847871849, -38.40625000204835260 ) ) ;
#41158 = COORDINATED_UNIVERSAL_TIME_OFFSET ( 6, 0, .AHEAD. ) ;
#41159 = CARTESIAN_POINT ( 'NONE',  ( -5.405949406249996869, 9.363379034771805109, -90.84375000204838102 ) ) ;
#41160 = CARTESIAN_POINT ( 'NONE',  ( 0.000000000000000000, 0.000000000000000000, -99.99999999999998579 ) ) ;
#41161 = AXIS2_PLACEMENT_3D ( 'NONE', #25856, #2981, #28891 ) ;
#41162 = CARTESIAN_POINT ( 'NONE',  ( 9.999999999999998224, 0.000000000000000000, -114.4999999999999858 ) ) ;
#41163 = CARTESIAN_POINT ( 'NONE',  ( 5.000000000000000000, 8.660254037844385522, -123.2500000000000000 ) ) ;
#41164 = CARTESIAN_POINT ( 'NONE',  ( 5.405949406249999534, 9.363379034771803333, -166.2812500020484094 ) ) ;
#41165 = CARTESIAN_POINT ( 'NONE',  ( -9.999999999999998224, 1.224646799147353059E-15, -54.12500000409675494 ) ) ;
#41166 = CARTESIAN_POINT ( 'NONE',  ( 5.405949406249992428, -9.363379034771808662, -112.5937500020483810 ) ) ;
#41167 = CARTESIAN_POINT ( 'NONE',  ( -10.81189881249999907, -6.242252689847864744, -82.96875000204836681 ) ) ;
#41168 = CARTESIAN_POINT ( 'NONE',  ( -2.293366432827344421E-15, -12.48450537969573659, -4.906250002048355263 ) ) ;
#41169 = CARTESIAN_POINT ( 'NONE',  ( 7.644554776091147741E-16, 12.48450537969573659, -191.4687500020484094 ) ) ;
#41170 = CARTESIAN_POINT ( 'NONE',  ( -2.293366432827344421E-15, -12.48450537969573659, -90.40625000204838102 ) ) ;
#41171 = CARTESIAN_POINT ( 'NONE',  ( -9.999999999999998224, 1.224646799147353059E-15, -180.1250000040968189 ) ) ;
#41172 = CARTESIAN_POINT ( 'NONE',  ( -10.81189881249999729, -6.242252689847864744, -173.1562500020484379 ) ) ;
#41173 = CARTESIAN_POINT ( 'NONE',  ( -4.999999999999996447, 8.660254037844387298, -103.5000000000000000 ) ) ;
#41174 = CARTESIAN_POINT ( 'NONE',  ( 10.81189881249999729, 0.000000000000000000, -177.0312500020483810 ) ) ;
#41175 = CARTESIAN_POINT ( 'NONE',  ( -10.81189881249999729, 1.324075727343319199E-15, -191.2812500020484094 ) ) ;
#41176 = CARTESIAN_POINT ( 'NONE',  ( -10.81189881249999729, -6.242252689847864744, -54.46875000204838102 ) ) ;
#41177 = CARTESIAN_POINT ( 'NONE',  ( 9.999999999999998224, 0.000000000000000000, -161.3750000040967905 ) ) ;
#41178 = CARTESIAN_POINT ( 'NONE',  ( -10.81189881249999729, 1.324075727343319199E-15, -8.281250002048350822 ) ) ;
#41179 = CARTESIAN_POINT ( 'NONE',  ( -10.81189881249999729, 1.324075727343319199E-15, -12.59375000204834905 ) ) ;
#41180 = CARTESIAN_POINT ( 'NONE',  ( -4.999999999999996447, 8.660254037844387298, -53.99999999999996447 ) ) ;
#41181 = CARTESIAN_POINT ( 'NONE',  ( 10.81189881249999729, 0.000000000000000000, -125.8437500020483952 ) ) ;
#41182 = CARTESIAN_POINT ( 'NONE',  ( -9.999999999999998224, 1.224646799147353059E-15, -94.24999999999998579 ) ) ;
#41183 = CARTESIAN_POINT ( 'NONE',  ( -2.293366432827344421E-15, -12.48450537969573659, -21.40625000204837747 ) ) ;
#41184 = CARTESIAN_POINT ( 'NONE',  ( -2.121150477449813534E-15, -11.54700538379251284, -109.2500000040967763 ) ) ;
#41185 = CARTESIAN_POINT ( 'NONE',  ( 0.000000000000000000, 0.000000000000000000, -200.0000000000000000 ) ) ;
#41186 = CARTESIAN_POINT ( 'NONE',  ( 5.000000000000000000, 8.660254037844385522, -49.74999999999998579 ) ) ;
#41187 = CARTESIAN_POINT ( 'NONE',  ( 10.81189881249999551, -6.242252689847874514, -120.1562500020483810 ) ) ;
#41188 = CARTESIAN_POINT ( 'NONE',  ( -10.81189881249999729, -6.242252689847864744, -96.65625000204839523 ) ) ;
#41189 = EDGE_LOOP ( 'NONE', ( #40836, #19774, #7742, #32741 ) ) ;
#41190 = CARTESIAN_POINT ( 'NONE',  ( -2.121150477449813534E-15, -11.54700538379251284, -95.75000000409677625 ) ) ;
#41191 = CARTESIAN_POINT ( 'NONE',  ( -9.999999999999998224, 1.224646799147353059E-15, -141.1250000040967905 ) ) ;
#41192 = CARTESIAN_POINT ( 'NONE',  ( 7.644554776091147741E-16, 12.48450537969573659, -160.1562500020484094 ) ) ;
#41193 = CARTESIAN_POINT ( 'NONE',  ( 10.81189881249999551, -6.242252689847874514, -52.46875000204837391 ) ) ;
#41194 = EDGE_LOOP ( 'NONE', ( #3812, #17214, #9492, #34130 ) ) ;
#41195 = CARTESIAN_POINT ( 'NONE',  ( 9.999999999999998224, 0.000000000000000000, -28.99999999999997158 ) ) ;
#41196 = EDGE_CURVE ( 'NONE', #12994, #40615, #25645, .T. ) ;
#41197 = EDGE_CURVE ( 'NONE', #26528, #16951, #18449, .T. ) ;
#41198 = CARTESIAN_POINT ( 'NONE',  ( 5.405949406249999534, 9.363379034771803333, -25.28125000204836681 ) ) ;
#41199 = CARTESIAN_POINT ( 'NONE',  ( -2.121150477449813534E-15, -11.54700538379251284, -162.8750000000000000 ) ) ;
#41200 = AXIS2_PLACEMENT_3D ( 'NONE', #13025, #29242, #3764 ) ;
#41201 = CARTESIAN_POINT ( 'NONE',  ( 10.00000000000051159, -5.773502691895965988, -90.62499999999997158 ) ) ;
#41202 = CARTESIAN_POINT ( 'NONE',  ( 5.000000000000000000, 8.660254037844385522, -27.62500000409676204 ) ) ;
#41203 = EDGE_CURVE ( 'NONE', #27433, #7656, #12228, .T. ) ;
#41204 = CARTESIAN_POINT ( 'NONE',  ( -1.040834085586084257E-14, -20.00000000000000355, 22.49999999999999289 ) ) ;
#41205 = CARTESIAN_POINT ( 'NONE',  ( -10.81189881249999729, 6.242252689847871849, -134.4062500020484094 ) ) ;
#41206 = CARTESIAN_POINT ( 'NONE',  ( 9.999999999999998224, 0.000000000000000000, -75.87500000409677625 ) ) ;
#41207 =( BOUNDED_CURVE ( )  B_SPLINE_CURVE ( 2, ( #25093, #38239, #463, #38873, #6290, #42515, #29168 ),
 .UNSPECIFIED., .F., .F. ) 
 B_SPLINE_CURVE_WITH_KNOTS ( ( 3, 2, 2, 3 ),
 ( 0.2574626865671643117, 0.2587064676616916414, 0.2599502487562190267, 0.2611940298507463565 ),
 .UNSPECIFIED. ) 
 CURVE ( )  GEOMETRIC_REPRESENTATION_ITEM ( )  RATIONAL_B_SPLINE_CURVE ( ( 0.9999999999999880096, 0.8660254037844506980, 1.000000000000000000, 0.8660254037844387076, 1.000000000000000000, 0.8660254037844267172, 1.000000000000011990 ) ) 
 REPRESENTATION_ITEM ( '' )  );
#41208 = CARTESIAN_POINT ( 'NONE',  ( 10.00000000000102318, -5.773502691895667560, -68.50000000409674783 ) ) ;
#41209 = ORIENTED_EDGE ( 'NONE', *, *, #1968, .T. ) ;
#41210 = CARTESIAN_POINT ( 'NONE',  ( 10.81189881249999907, 6.242252689847868297, -64.40625000204839523 ) ) ;
#41211 = COORDINATED_UNIVERSAL_TIME_OFFSET ( 6, 0, .AHEAD. ) ;
#41213 = ORIENTED_EDGE ( 'NONE', *, *, #16935, .F. ) ;
#41212 = ORIENTED_EDGE ( 'NONE', *, *, #16204, .F. ) ;
#41214 = EDGE_CURVE ( 'NONE', #20412, #21356, #15836, .T. ) ;
#41215 = CARTESIAN_POINT ( 'NONE',  ( -4.999999999999996447, 8.660254037844387298, -181.8750000040967905 ) ) ;
#41216 = CARTESIAN_POINT ( 'NONE',  ( 0.000000000000000000, 0.000000000000000000, -99.99999999999998579 ) ) ;
#41217 = CARTESIAN_POINT ( 'NONE',  ( 5.405949406249999534, 9.363379034771803333, -157.0937500020483810 ) ) ;
#41218 = CARTESIAN_POINT ( 'NONE',  ( -10.81189881249999729, 1.324075727343319199E-15, -186.7812500020484094 ) ) ;
#41219 = CARTESIAN_POINT ( 'NONE',  ( 10.81189881249999551, -6.242252689847874514, -7.468750002048351710 ) ) ;
#41220 = FACE_OUTER_BOUND ( 'NONE', #25271, .T. ) ;
#41221 = ADVANCED_FACE ( 'NONE', ( #28453 ), #9636, .T. ) ;
#41222 = CARTESIAN_POINT ( 'NONE',  ( -10.81189881249999729, 6.242252689847871849, -146.2187500020484094 ) ) ;
#41223 = AXIS2_PLACEMENT_3D ( 'NONE', #33935, #4359, #40587 ) ;
#41224 = CARTESIAN_POINT ( 'NONE',  ( 7.644554776091147741E-16, 12.48450537969573659, -103.1562500020483952 ) ) ;
#41225 = CARTESIAN_POINT ( 'NONE',  ( 5.405949406249992428, -9.363379034771808662, -111.0937500020483810 ) ) ;
#41226 = CARTESIAN_POINT ( 'NONE',  ( 9.999999999999998224, 0.000000000000000000, -55.99999999999996447 ) ) ;
#41227 = CARTESIAN_POINT ( 'NONE',  ( -10.81189881249999729, 6.242252689847871849, -113.4062500020483810 ) ) ;
#41228 = CARTESIAN_POINT ( 'NONE',  ( -10.81189881249999729, 6.242252689847871849, -5.218750002048340164 ) ) ;
#41229 = CARTESIAN_POINT ( 'NONE',  ( -5.405949406250003975, -9.363379034771801557, -129.3437500020484094 ) ) ;
#41230 = CARTESIAN_POINT ( 'NONE',  ( -5.405949406249996869, 9.363379034771805109, -193.0312500020484094 ) ) ;
#41231 = CARTESIAN_POINT ( 'NONE',  ( -9.999999999999998224, 1.224646799147353059E-15, -178.6250000040968189 ) ) ;
#41232 = CARTESIAN_POINT ( 'NONE',  ( 9.999999999999998224, 0.000000000000000000, -150.5000000000000000 ) ) ;
#41233 = CARTESIAN_POINT ( 'NONE',  ( -5.000000000000003553, -8.660254037844383745, -9.999999999999953815 ) ) ;
#41234 = CARTESIAN_POINT ( 'NONE',  ( 7.644554776091147741E-16, 12.48450537969573659, -74.46875000204838102 ) ) ;
#41235 = CARTESIAN_POINT ( 'NONE',  ( 7.644554776091147741E-16, 12.48450537969573659, -60.96875000204838102 ) ) ;
#41236 = CARTESIAN_POINT ( 'NONE',  ( 9.999999999999996447, -5.773502691896262640, -187.0000000040968189 ) ) ;
#41237 = CARTESIAN_POINT ( 'NONE',  ( 5.405949406249992428, -9.363379034771808662, -31.78125000204837391 ) ) ;
#41238 = CARTESIAN_POINT ( 'NONE',  ( 10.81189881249999729, 0.000000000000000000, -34.34375000204836681 ) ) ;
#41239 = CARTESIAN_POINT ( 'NONE',  ( -9.999999999999998224, 1.224646799147353059E-15, -142.6250000040967905 ) ) ;
#41240 = CARTESIAN_POINT ( 'NONE',  ( -10.81189881249999907, -6.242252689847864744, -147.4687500020484094 ) ) ;
#41241 = CARTESIAN_POINT ( 'NONE',  ( -9.999999999999998224, 5.773502691896259087, -119.8750000000000000 ) ) ;
#41242 = CARTESIAN_POINT ( 'NONE',  ( -9.999999999999998224, 0.000000000000000000, -99.99999999999998579 ) ) ;
#41243 = CARTESIAN_POINT ( 'NONE',  ( 7.070501591499377789E-16, 11.54700538379251284, -72.12499999999997158 ) ) ;
#41244 = CARTESIAN_POINT ( 'NONE',  ( 7.644554776091147741E-16, 12.48450537969573659, -142.1562500020483810 ) ) ;
#41245 = CARTESIAN_POINT ( 'NONE',  ( -5.405949406250003975, -9.363379034771801557, -14.03125000204835615 ) ) ;
#41246 = ORIENTED_EDGE ( 'NONE', *, *, #3499, .F. ) ;
#41247 = CARTESIAN_POINT ( 'NONE',  ( 10.81189881249999729, 6.242252689847867408, -101.9062500020483952 ) ) ;
#41248 = CARTESIAN_POINT ( 'NONE',  ( -5.000000000000003553, -8.660254037844383745, -122.8750000040967905 ) ) ;
#41249 = LINE ( 'NONE', #37821, #180 ) ;
#41250 = CARTESIAN_POINT ( 'NONE',  ( -10.81189881249999907, -6.242252689847864744, -76.96875000204836681 ) ) ;
#41251 = CARTESIAN_POINT ( 'NONE',  ( -5.000000000000003553, -8.660254037844383745, -32.87500000409676915 ) ) ;
#41252 = CARTESIAN_POINT ( 'NONE',  ( 9.999999999999998224, 0.000000000000000000, -200.0000000000000000 ) ) ;
#41253 = CARTESIAN_POINT ( 'NONE',  ( 5.405949406249992428, -9.363379034771808662, -46.78125000204838813 ) ) ;
#41254 =( BOUNDED_CURVE ( )  B_SPLINE_CURVE ( 2, ( #18828, #18396, #32222, #25108, #22492, #2236, #25742 ),
 .UNSPECIFIED., .F., .F. ) 
 B_SPLINE_CURVE_WITH_KNOTS ( ( 3, 2, 2, 3 ),
 ( 0.2313432835820896372, 0.2325870646766169947, 0.2338308457711443245, 0.2350746268656717097 ),
 .UNSPECIFIED. ) 
 CURVE ( )  GEOMETRIC_REPRESENTATION_ITEM ( )  RATIONAL_B_SPLINE_CURVE ( ( 0.9999999999999910072, 0.8660254037844477004, 1.000000000000000000, 0.8660254037844387076, 1.000000000000000000, 0.8660254037844327124, 1.000000000000005995 ) ) 
 REPRESENTATION_ITEM ( '' )  );
#41255 = EDGE_CURVE ( 'NONE', #24567, #17213, #25895, .T. ) ;
#41256 = CARTESIAN_POINT ( 'NONE',  ( -9.999999999999998224, 1.224646799147353059E-15, -23.74999999999996447 ) ) ;
#41257 = CARTESIAN_POINT ( 'NONE',  ( 10.81189881249999551, -6.242252689847874514, -142.6562500020484094 ) ) ;
#41258 = ADVANCED_FACE ( 'NONE', ( #22808 ), #38788, .T. ) ;
#41259 = CARTESIAN_POINT ( 'NONE',  ( 10.81189881249999907, 6.242252689847868297, -125.7187500020483810 ) ) ;
#41260 = CARTESIAN_POINT ( 'NONE',  ( -9.999999999999998224, 1.224646799147353059E-15, -59.74999999999997158 ) ) ;
#41261 = VECTOR ( 'NONE', #33086, 1000.000000000000000 ) ;
#41262 = PERSON ( 'NAUO-PER1', 'UNSPECIFIED', 'UNSPECIFIED', ('UNSPECIFIED'), ('UNSPECIFIED'), ('UNSPECIFIED') ) ;
#41263 = CARTESIAN_POINT ( 'NONE',  ( 4.999999999999992006, -8.660254037844389075, -120.7500000000000000 ) ) ;
#41264 = ORIENTED_EDGE ( 'NONE', *, *, #3396, .F. ) ;
#41265 = VECTOR ( 'NONE', #38339, 1000.000000000000000 ) ;
#41266 = ORIENTED_EDGE ( 'NONE', *, *, #42334, .F. ) ;
#41267 = ORIENTED_EDGE ( 'NONE', *, *, #10010, .F. ) ;
#41268 = ADVANCED_FACE ( 'NONE', ( #16088 ), #32113, .T. ) ;
#41269 = CARTESIAN_POINT ( 'NONE',  ( -9.999999999999479527, -5.773502691896549521, -145.5000000040967905 ) ) ;
#41270 = CARTESIAN_POINT ( 'NONE',  ( 10.81189881249999729, 0.000000000000000000, -181.3437500020483810 ) ) ;
#41271 = VECTOR ( 'NONE', #9506, 1000.000000000000000 ) ;
#41272 = CARTESIAN_POINT ( 'NONE',  ( -10.81189881249999729, 1.324075727343319199E-15, -42.59375000204837391 ) ) ;
#41273 = CARTESIAN_POINT ( 'NONE',  ( 5.000000000000000000, 8.660254037844385522, -110.1250000040967763 ) ) ;
#41274 = CARTESIAN_POINT ( 'NONE',  ( 5.405949406249999534, 9.363379034771803333, -173.5937500020484094 ) ) ;
#41275 = CARTESIAN_POINT ( 'NONE',  ( -10.81189881249999907, -6.242252689847864744, -153.4687500020484094 ) ) ;
#41276 = CARTESIAN_POINT ( 'NONE',  ( -9.999999999999998224, 1.224646799147353059E-15, -200.0000000000000000 ) ) ;
#41277 = CARTESIAN_POINT ( 'NONE',  ( 5.405949406249992428, -9.363379034771808662, -132.0937500020483810 ) ) ;
#41278 = CARTESIAN_POINT ( 'NONE',  ( -5.405949406249996869, 9.363379034771805109, -139.0312500020484094 ) ) ;
#41279 = CARTESIAN_POINT ( 'NONE',  ( 5.405949406249992428, -9.363379034771808662, -157.5937500020483810 ) ) ;
#41280 = CARTESIAN_POINT ( 'NONE',  ( -5.000000000000003553, -8.660254037844383745, -152.5000000000000000 ) ) ;
#41281 = CARTESIAN_POINT ( 'NONE',  ( 7.070501591499376803E-16, 11.54700538379251284, -33.50000000409676204 ) ) ;
#41282 = CARTESIAN_POINT ( 'NONE',  ( -10.00000000000000000, -5.773502691896251982, -173.6249999999999716 ) ) ;
#41283 = CARTESIAN_POINT ( 'NONE',  ( 10.81189881249999551, -6.242252689847874514, -82.46875000204836681 ) ) ;
#41284 = CARTESIAN_POINT ( 'NONE',  ( -2.121150477449813534E-15, -11.54700538379251284, -135.8750000000000000 ) ) ;
#41285 = CARTESIAN_POINT ( 'NONE',  ( 10.81189881249999907, 6.242252689847868297, -59.90625000204838813 ) ) ;
#41286 = CARTESIAN_POINT ( 'NONE',  ( 5.000000000000000000, 8.660254037844385522, -133.7499999999999716 ) ) ;
#41287 = CARTESIAN_POINT ( 'NONE',  ( -5.405949406249996869, 9.363379034771805109, -167.3437500020484094 ) ) ;
#41288 = CARTESIAN_POINT ( 'NONE',  ( -10.81189881249999729, 1.324075727343319199E-15, -114.7812500020483952 ) ) ;
#41289 = CARTESIAN_POINT ( 'NONE',  ( -5.405949406249996869, 9.363379034771805109, -154.0312500020484094 ) ) ;
#41290 = CARTESIAN_POINT ( 'NONE',  ( 9.999999999998456346, 5.773502691897149042, -15.75000000409673540 ) ) ;
#41291 = CARTESIAN_POINT ( 'NONE',  ( -5.405949406250003975, -9.363379034771801557, -48.53125000204838813 ) ) ;
#41292 = CARTESIAN_POINT ( 'NONE',  ( -4.999999999999996447, 8.660254037844387298, -120.3750000040967905 ) ) ;
#41293 = CARTESIAN_POINT ( 'NONE',  ( 7.070501591499377789E-16, 11.54700538379251284, -97.62499999999997158 ) ) ;
#41294 = ORIENTED_EDGE ( 'NONE', *, *, #375, .F. ) ;
#41295 = CARTESIAN_POINT ( 'NONE',  ( 10.81189881249999551, -6.242252689847874514, -124.6562500020483952 ) ) ;
#41296 = CARTESIAN_POINT ( 'NONE',  ( 9.999999999999996447, -5.773502691896262640, -151.0000000040967905 ) ) ;
#41297 = CARTESIAN_POINT ( 'NONE',  ( -9.999999999999872102, -5.773502691896326589, -167.6250000000000000 ) ) ;
#41298 = VECTOR ( 'NONE', #5941, 1000.000000000000000 ) ;
#41299 = CARTESIAN_POINT ( 'NONE',  ( 5.405949406249992428, -9.363379034771808662, -177.2812500020484094 ) ) ;
#41300 = ORIENTED_EDGE ( 'NONE', *, *, #40673, .F. ) ;
#41301 = CARTESIAN_POINT ( 'NONE',  ( -10.81189881249999729, 6.242252689847871849, -176.2187500020483810 ) ) ;
#41302 = CARTESIAN_POINT ( 'NONE',  ( -2.121150477449813534E-15, -11.54700538379251284, -58.25000000409676915 ) ) ;
#41303 = CARTESIAN_POINT ( 'NONE',  ( 4.999999999999992006, -8.660254037844389075, -165.7500000000000000 ) ) ;
#41304 = CARTESIAN_POINT ( 'NONE',  ( 5.000000000000000000, -20.00000000000000000, -235.0000000000000000 ) ) ;
#41305 = CARTESIAN_POINT ( 'NONE',  ( 5.405949406249992428, -9.363379034771808662, -67.78125000204838102 ) ) ;
#41306 = CARTESIAN_POINT ( 'NONE',  ( 4.999999999999992006, -8.660254037844389075, -44.62500000409677625 ) ) ;
#41307 = CARTESIAN_POINT ( 'NONE',  ( -10.81189881249999729, 6.242252689847871849, -3.718750002048354819 ) ) ;
#41308 = CARTESIAN_POINT ( 'NONE',  ( 9.999999999999998224, 0.000000000000000000, -134.3750000040967905 ) ) ;
#41309 = CARTESIAN_POINT ( 'NONE',  ( -10.81189881249999907, -6.242252689847864744, -173.1562500020484094 ) ) ;
#41310 = CARTESIAN_POINT ( 'NONE',  ( 9.999999999999998224, 0.000000000000000000, -105.8750000040967763 ) ) ;
#41311 = CYLINDRICAL_SURFACE ( 'NONE', #13034, 20.00000000000000355 ) ;
#41312 = VERTEX_POINT ( 'NONE', #35136 ) ;
#41313 = CARTESIAN_POINT ( 'NONE',  ( 9.999999999999998224, 0.000000000000000000, -84.87500000409677625 ) ) ;
#41314 = DIRECTION ( 'NONE',  ( 0.8660254037844387076, -0.4999999999999998335, 0.000000000000000000 ) ) ;
#41315 = CYLINDRICAL_SURFACE ( 'NONE', #13770, 9.999999999999998224 ) ;
#41316 = EDGE_CURVE ( 'NONE', #40345, #4873, #18704, .T. ) ;
#41318 = VERTEX_POINT ( 'NONE', #18713 ) ;
#41317 = CARTESIAN_POINT ( 'NONE',  ( 10.81189881249999551, -6.242252689847874514, -75.15625000204838102 ) ) ;
#41319 = DIRECTION ( 'NONE',  ( 0.000000000000000000, 0.000000000000000000, 1.000000000000000000 ) ) ;
#41321 = EDGE_LOOP ( 'NONE', ( #6255, #16840, #22367, #8751 ) ) ;
#41320 = DIRECTION ( 'NONE',  ( -0.7559289460184527298, -1.381779857339538216E-16, -0.6546536707079791961 ) ) ;
#41322 = ORIENTED_EDGE ( 'NONE', *, *, #5930, .T. ) ;
#41323 = CARTESIAN_POINT ( 'NONE',  ( -5.405949406250003975, -9.363379034771801557, -36.34375000204836681 ) ) ;
#41324 = CARTESIAN_POINT ( 'NONE',  ( 4.999999999999992006, -8.660254037844389075, -186.7500000000000000 ) ) ;
#41325 = CARTESIAN_POINT ( 'NONE',  ( -10.81189881249999729, 6.242252689847871849, -6.906250002048365033 ) ) ;
#41327 = VERTEX_POINT ( 'NONE', #32735 ) ;
#41326 = CARTESIAN_POINT ( 'NONE',  ( 5.405949406249999534, 9.363379034771803333, -67.09375000204836681 ) ) ;
#41328 = CARTESIAN_POINT ( 'NONE',  ( -10.00000000000076916, 5.773502691895813221, -112.3749999999999858 ) ) ;
#41329 = CARTESIAN_POINT ( 'NONE',  ( -2.121150477449813534E-15, -11.54700538379251284, -38.37499999999996447 ) ) ;
#41330 = CARTESIAN_POINT ( 'NONE',  ( -10.81189881249999729, 1.324075727343319199E-15, -197.0937500020484094 ) ) ;
#41331 = CARTESIAN_POINT ( 'NONE',  ( -5.405949406249996869, 9.363379034771805109, -177.8437500020483810 ) ) ;
#41332 = CARTESIAN_POINT ( 'NONE',  ( -10.81189881249999729, 6.242252689847871849, -159.7187500020483526 ) ) ;
#41333 = EDGE_CURVE ( 'NONE', #38572, #34451, #38635, .T. ) ;
#41334 = CARTESIAN_POINT ( 'NONE',  ( 7.070501591499376803E-16, 11.54700538379251284, -43.62499999999997158 ) ) ;
#41335 = LINE ( 'NONE', #20631, #32937 ) ;
#41336 = CARTESIAN_POINT ( 'NONE',  ( -2.121150477449813534E-15, -11.54700538379251284, -101.7500000040967763 ) ) ;
#41337 = CARTESIAN_POINT ( 'NONE',  ( -10.00000000000000000, -5.773502691896251982, -196.1250000000000568 ) ) ;
#41338 = CARTESIAN_POINT ( 'NONE',  ( 10.81189881249999729, 0.000000000000000000, -103.3437500020483668 ) ) ;
#41339 = CARTESIAN_POINT ( 'NONE',  ( -9.999999999999998224, 0.000000000000000000, -99.99999999999998579 ) ) ;
#41340 = CARTESIAN_POINT ( 'NONE',  ( 5.405949406249992428, -9.363379034771808662, -81.28125000204839523 ) ) ;
#41341 = CARTESIAN_POINT ( 'NONE',  ( 5.405949406249992428, -9.363379034771808662, -91.59375000204838102 ) ) ;
#41342 =( BOUNDED_CURVE ( )  B_SPLINE_CURVE ( 2, ( #21313, #8594, #15037, #20510, #10368, #41148, #37939 ),
 .UNSPECIFIED., .F., .F. ) 
 B_SPLINE_CURVE_WITH_KNOTS ( ( 3, 2, 2, 3 ),
 ( 0.2313432835820896372, 0.2325870646766169947, 0.2338308457711443245, 0.2350746268656717097 ),
 .UNSPECIFIED. ) 
 CURVE ( )  GEOMETRIC_REPRESENTATION_ITEM ( )  RATIONAL_B_SPLINE_CURVE ( ( 0.9999999999999910072, 0.8660254037844477004, 1.000000000000000000, 0.8660254037844387076, 1.000000000000000000, 0.8660254037844327124, 1.000000000000005995 ) ) 
 REPRESENTATION_ITEM ( '' )  );
#41343 = CARTESIAN_POINT ( 'NONE',  ( 5.405949406249992428, -9.363379034771808662, -67.78125000204838102 ) ) ;
#41344 = CARTESIAN_POINT ( 'NONE',  ( 7.070501591499377789E-16, 11.54700538379251284, -152.0000000040967905 ) ) ;
#41345 = CARTESIAN_POINT ( 'NONE',  ( 4.999999999999992006, -8.660254037844389075, -125.2500000000000000 ) ) ;
#41346 = CARTESIAN_POINT ( 'NONE',  ( -10.81189881249999729, -6.242252689847864744, -150.6562500020484094 ) ) ;
#41347 = CARTESIAN_POINT ( 'NONE',  ( -2.293366432827344421E-15, -12.48450537969573659, -163.9062500020483810 ) ) ;
#41348 = CYLINDRICAL_SURFACE ( 'NONE', #28921, 9.999999999999998224 ) ;
#41349 = CARTESIAN_POINT ( 'NONE',  ( -5.000000000000003553, -8.660254037844383745, -182.5000000000000000 ) ) ;
#41350 = CARTESIAN_POINT ( 'NONE',  ( 5.405949406249992428, -9.363379034771808662, -99.09375000204838102 ) ) ;
#41351 = ORIENTED_EDGE ( 'NONE', *, *, #6560, .F. ) ;
#41352 = CARTESIAN_POINT ( 'NONE',  ( -10.00000000000000000, -5.773502691896251982, -67.12500000000000000 ) ) ;
#41353 = CARTESIAN_POINT ( 'NONE',  ( 10.81189881249999729, 0.000000000000000000, -197.8437500020484094 ) ) ;
#41354 = CARTESIAN_POINT ( 'NONE',  ( -10.00000000000000000, -5.773502691896251982, -85.50000000409677625 ) ) ;
#41355 = CARTESIAN_POINT ( 'NONE',  ( 9.999999999999994671, -5.773502691896262640, -133.0000000040967905 ) ) ;
#41356 = CARTESIAN_POINT ( 'NONE',  ( -9.999999999999998224, 1.224646799147353059E-15, -7.625000004096743389 ) ) ;
#41357 = CARTESIAN_POINT ( 'NONE',  ( -2.293366432827344421E-15, -12.48450537969573659, -88.90625000204838102 ) ) ;
#41358 = CARTESIAN_POINT ( 'NONE',  ( 5.405949406249992428, -9.363379034771808662, -78.28125000204838102 ) ) ;
#41359 = CARTESIAN_POINT ( 'NONE',  ( -10.00000000000000000, -5.773502691896251982, -64.50000000409677625 ) ) ;
#41360 = DIRECTION ( 'NONE',  ( -0.000000000000000000, -0.000000000000000000, 1.000000000000000000 ) ) ;
#41361 = CARTESIAN_POINT ( 'NONE',  ( -10.81189881249999729, 1.324075727343319199E-15, -26.09375000204835970 ) ) ;
#41362 = CARTESIAN_POINT ( 'NONE',  ( 7.070501591499376803E-16, 11.54700538379251284, -100.6250000000000000 ) ) ;
#41363 = CARTESIAN_POINT ( 'NONE',  ( 10.81189881249999907, 6.242252689847868297, -190.4062500020484094 ) ) ;
#41364 = VECTOR ( 'NONE', #39836, 1000.000000000000000 ) ;
#41365 = CARTESIAN_POINT ( 'NONE',  ( -5.405949406250003975, -9.363379034771801557, -23.03125000204836326 ) ) ;
#41366 = CARTESIAN_POINT ( 'NONE',  ( 10.81189881249999729, 6.242252689847867408, -5.718750002048342829 ) ) ;
#41367 = CARTESIAN_POINT ( 'NONE',  ( -9.999999999999998224, 1.224646799147353059E-15, -177.1250000040968189 ) ) ;
#41368 = CARTESIAN_POINT ( 'NONE',  ( -5.405949406249996869, 9.363379034771805109, -141.8437500020483810 ) ) ;
#41369 = CARTESIAN_POINT ( 'NONE',  ( 9.999999999999998224, 0.000000000000000000, -161.3750000040967905 ) ) ;
#41370 = EDGE_CURVE ( 'NONE', #30730, #31040, #30309, .T. ) ;
#41371 = CARTESIAN_POINT ( 'NONE',  ( 4.999999999999992006, -8.660254037844389075, -180.7500000000000284 ) ) ;
#41372 = CARTESIAN_POINT ( 'NONE',  ( -9.999999999998969713, -5.773502691896847949, -36.00000000409673362 ) ) ;
#41374 = ORIENTED_EDGE ( 'NONE', *, *, #24570, .T. ) ;
#41373 = CARTESIAN_POINT ( 'NONE',  ( 10.81189881249999907, 6.242252689847868297, -104.9062500020483952 ) ) ;
#41375 = CARTESIAN_POINT ( 'NONE',  ( 9.999999999999998224, 0.000000000000000000, -195.5000000000000000 ) ) ;
#41376 = EDGE_LOOP ( 'NONE', ( #743, #15767, #35393, #3122 ) ) ;
#41377 = VERTEX_POINT ( 'NONE', #28872 ) ;
#41378 = CARTESIAN_POINT ( 'NONE',  ( 10.81189881249999907, 6.242252689847868297, -34.40625000204836681 ) ) ;
#41379 = CALENDAR_DATE ( 2026, 28, 9 ) ;
#41380 = CARTESIAN_POINT ( 'NONE',  ( -2.293366432827344421E-15, -12.48450537969573659, -85.71875000204838102 ) ) ;
#41381 = DIRECTION ( 'NONE',  ( -0.000000000000000000, -0.000000000000000000, -1.000000000000000000 ) ) ;
#41382 = ADVANCED_FACE ( 'NONE', ( #31906 ), #22593, .T. ) ;
#41383 = CARTESIAN_POINT ( 'NONE',  ( -10.00000000000076916, 5.773502691895813221, -125.8749999999999858 ) ) ;
#41384 =( BOUNDED_CURVE ( )  B_SPLINE_CURVE ( 2, ( #8383, #5347, #25422, #38360, #18931, #21746, #21533 ),
 .UNSPECIFIED., .F., .F. ) 
 B_SPLINE_CURVE_WITH_KNOTS ( ( 3, 2, 2, 3 ),
 ( 0.7425373134328361324, 0.7437810945273634067, 0.7450248756218907920, 0.7462686567164180662 ),
 .UNSPECIFIED. ) 
 CURVE ( )  GEOMETRIC_REPRESENTATION_ITEM ( )  RATIONAL_B_SPLINE_CURVE ( ( 0.9999999999999641398, 0.8660254037844745678, 1.000000000000000000, 0.8660254037844387076, 1.000000000000000000, 0.8660254037844267172, 1.000000000000011990 ) ) 
 REPRESENTATION_ITEM ( '' )  );
#41385 = CARTESIAN_POINT ( 'NONE',  ( 9.999999999999998224, 0.000000000000000000, -110.3750000040967763 ) ) ;
#41386 = CARTESIAN_POINT ( 'NONE',  ( -10.81189881249999729, 1.324075727343319199E-15, -162.7812500020484094 ) ) ;
#41387 = CARTESIAN_POINT ( 'NONE',  ( -2.121150477449813534E-15, -11.54700538379251284, -198.8750000000000284 ) ) ;
#41388 = AXIS2_PLACEMENT_3D ( 'NONE', #13701, #7257, #13287 ) ;
#41389 = AXIS2_PLACEMENT_3D ( 'NONE', #18393, #31581, #22069 ) ;
#41390 = CARTESIAN_POINT ( 'NONE',  ( 7.644554776091147741E-16, 12.48450537969573659, -114.9687500020483668 ) ) ;
#41391 = CARTESIAN_POINT ( 'NONE',  ( 10.81189881249999729, 0.000000000000000000, -86.84375000204836681 ) ) ;
#41392 = CARTESIAN_POINT ( 'NONE',  ( -5.405949406250003975, -9.363379034771801557, -3.531250002048374803 ) ) ;
#41393 = CARTESIAN_POINT ( 'NONE',  ( -5.405949406249996869, 9.363379034771805109, -192.8437500020484094 ) ) ;
#41394 = CARTESIAN_POINT ( 'NONE',  ( -10.81189881249999907, -6.242252689847864744, -90.65625000204836681 ) ) ;
#41395 = CARTESIAN_POINT ( 'NONE',  ( -4.999999999999996447, 8.660254037844387298, -174.3750000040968189 ) ) ;
#41396 = CARTESIAN_POINT ( 'NONE',  ( -10.81189881249999729, 6.242252689847871849, -168.9062500020484094 ) ) ;
#41397 =( BOUNDED_CURVE ( )  B_SPLINE_CURVE ( 2, ( #1817, #30533, #41053, #40414, #14943, #24270, #27921 ),
 .UNSPECIFIED., .F., .F. ) 
 B_SPLINE_CURVE_WITH_KNOTS ( ( 3, 2, 2, 3 ),
 ( 0.3768656716417911334, 0.3781094527363185187, 0.3793532338308459040, 0.3805970149253732338 ),
 .UNSPECIFIED. ) 
 CURVE ( )  GEOMETRIC_REPRESENTATION_ITEM ( )  RATIONAL_B_SPLINE_CURVE ( ( 0.9999999999999880096, 0.8660254037844506980, 1.000000000000000000, 0.8660254037844387076, 1.000000000000000000, 0.8660254037844267172, 1.000000000000011990 ) ) 
 REPRESENTATION_ITEM ( '' )  );
#41398 = CARTESIAN_POINT ( 'NONE',  ( 9.999999999999998224, 0.000000000000000000, -0.8750000040967653714 ) ) ;
#41399 = CARTESIAN_POINT ( 'NONE',  ( -2.293366432827344421E-15, -12.48450537969573659, -174.4062500020484379 ) ) ;
#41400 = CARTESIAN_POINT ( 'NONE',  ( 5.405949406249999534, 9.363379034771803333, -190.2812500020484094 ) ) ;
#41401 = CARTESIAN_POINT ( 'NONE',  ( -10.81189881249999729, 6.242252689847871849, -42.71875000204835970 ) ) ;
#41402 = CARTESIAN_POINT ( 'NONE',  ( 9.999999999999996447, -5.773502691896262640, -161.5000000040968189 ) ) ;
#41403 = CARTESIAN_POINT ( 'NONE',  ( 10.81189881249999551, -6.242252689847874514, -3.156250002048346381 ) ) ;
#41404 = CARTESIAN_POINT ( 'NONE',  ( -5.405949406250003975, -9.363379034771801557, -15.34375000204835082 ) ) ;
#41405 = CARTESIAN_POINT ( 'NONE',  ( -9.999999999999742428, -5.773502691896402084, -159.0000000040967905 ) ) ;
#41406 = CARTESIAN_POINT ( 'NONE',  ( 10.81189881249999551, -6.242252689847874514, -125.9687500020483810 ) ) ;
#41407 = CARTESIAN_POINT ( 'NONE',  ( -4.999999999999996447, 8.660254037844387298, -86.99999999999998579 ) ) ;
#41408 = CARTESIAN_POINT ( 'NONE',  ( 10.81189881249999551, -6.242252689847874514, -24.15625000204837747 ) ) ;
#41409 = CARTESIAN_POINT ( 'NONE',  ( -9.999999999999998224, 5.773502691896259087, -105.2500000040967763 ) ) ;
#41410 = CARTESIAN_POINT ( 'NONE',  ( 9.999999999999998224, 0.000000000000000000, -14.37500000409674961 ) ) ;
#41411 = CARTESIAN_POINT ( 'NONE',  ( 9.999999999999996447, -5.773502691896262640, -54.62499999999997868 ) ) ;
#41412 = CARTESIAN_POINT ( 'NONE',  ( -10.81189881249999729, 1.324075727343319199E-15, -117.7812500020483952 ) ) ;
#41413 = CARTESIAN_POINT ( 'NONE',  ( -10.81189881249999729, -6.242252689847864744, -102.6562500020483952 ) ) ;
#41414 = ORIENTED_EDGE ( 'NONE', *, *, #30941, .T. ) ;
#41415 = CARTESIAN_POINT ( 'NONE',  ( -5.000000000000003553, -8.660254037844383745, -91.37500000409677625 ) ) ;
#41416 = CARTESIAN_POINT ( 'NONE',  ( 4.999999999999992006, -8.660254037844389075, -101.2499999999999858 ) ) ;
#41417 = CARTESIAN_POINT ( 'NONE',  ( 10.81189881249999729, 0.000000000000000000, -159.0312500020484094 ) ) ;
#41418 = CARTESIAN_POINT ( 'NONE',  ( 7.644554776091147741E-16, 12.48450537969573659, -50.46875000204836681 ) ) ;
#41419 = VERTEX_POINT ( 'NONE', #15671 ) ;
#41420 = CARTESIAN_POINT ( 'NONE',  ( -5.000000000000003553, -8.660254037844383745, -23.49999999999996447 ) ) ;
#41421 = CARTESIAN_POINT ( 'NONE',  ( -10.81189881249999729, 6.242252689847871849, -30.90625000204834905 ) ) ;
#41422 = CARTESIAN_POINT ( 'NONE',  ( -9.999999999999998224, 5.773502691896259087, -158.8749999999999716 ) ) ;
#41423 = CARTESIAN_POINT ( 'NONE',  ( -10.00000000000000000, -5.773502691896251982, -18.00000000409676559 ) ) ;
#41424 = VECTOR ( 'NONE', #20508, 1000.000000000000000 ) ;
#41425 =( GEOMETRIC_REPRESENTATION_CONTEXT ( 3 ) GLOBAL_UNCERTAINTY_ASSIGNED_CONTEXT ( ( #3253 ) ) GLOBAL_UNIT_ASSIGNED_CONTEXT ( ( #41955, #104, #3543 ) ) REPRESENTATION_CONTEXT ( 'NONE', 'WORKASPACE' ) );
#41426 = CARTESIAN_POINT ( 'NONE',  ( -2.121150477449813534E-15, -11.54700538379251284, -23.37499999999998224 ) ) ;
#41427 = CARTESIAN_POINT ( 'NONE',  ( 10.81189881249999729, 0.000000000000000000, -132.0312500020484094 ) ) ;
#41428 = CARTESIAN_POINT ( 'NONE',  ( 9.999999999999998224, 0.000000000000000000, -45.49999999999998579 ) ) ;
#41429 = CARTESIAN_POINT ( 'NONE',  ( -9.999999999999998224, 1.224646799147353059E-15, -157.2500000000000000 ) ) ;
#41430 = EDGE_LOOP ( 'NONE', ( #24357, #12084, #36070, #583 ) ) ;
#41431 = CARTESIAN_POINT ( 'NONE',  ( -5.405949406249996869, 9.363379034771805109, -58.03125000204836681 ) ) ;
#41432 = PERSON_AND_ORGANIZATION ( #11915, #17965 ) ;
#41434 = EDGE_LOOP ( 'NONE', ( #31757, #791, #34074, #29641 ) ) ;
#41433 = ORIENTED_EDGE ( 'NONE', *, *, #33874, .T. ) ;
#41435 = CARTESIAN_POINT ( 'NONE',  ( -5.000000000000003553, -8.660254037844383745, -121.0000000000000000 ) ) ;
#41436 = DIRECTION ( 'NONE',  ( -0.000000000000000000, -0.000000000000000000, 1.000000000000000000 ) ) ;
#41437 = CARTESIAN_POINT ( 'NONE',  ( -2.293366432827344421E-15, -12.48450537969573659, -157.7187500020484094 ) ) ;
#41438 = CARTESIAN_POINT ( 'NONE',  ( 5.405949406249999534, 9.363379034771803333, -185.7812500020484094 ) ) ;
#41439 = CARTESIAN_POINT ( 'NONE',  ( 10.81189881249999907, 6.242252689847868297, -8.718750002048356151 ) ) ;
#41440 = EDGE_CURVE ( 'NONE', #10196, #18513, #40740, .T. ) ;
#41441 = CARTESIAN_POINT ( 'NONE',  ( -10.81189881249999729, 6.242252689847871849, -137.2187500020483810 ) ) ;
#41442 = EDGE_CURVE ( 'NONE', #16199, #19338, #5411, .T. ) ;
#41443 = CARTESIAN_POINT ( 'NONE',  ( -5.405949406249996869, 9.363379034771805109, -95.53125000204838102 ) ) ;
#41444 = CARTESIAN_POINT ( 'NONE',  ( -5.405949406249996869, 9.363379034771805109, -111.8437500020483810 ) ) ;
#41445 = CARTESIAN_POINT ( 'NONE',  ( 7.070501591499376803E-16, 11.54700538379251284, -187.6250000000000000 ) ) ;
#41446 = CARTESIAN_POINT ( 'NONE',  ( -2.293366432827344421E-15, -12.48450537969573659, -118.9062500020483952 ) ) ;
#41447 = CARTESIAN_POINT ( 'NONE',  ( -2.293366432827344421E-15, -12.48450537969573659, -0.2187500020483489072 ) ) ;
#41448 = CARTESIAN_POINT ( 'NONE',  ( -10.81189881249999729, 6.242252689847871849, -125.2187500020483810 ) ) ;
#41449 = VECTOR ( 'NONE', #29080, 1000.000000000000000 ) ;
#41450 = CARTESIAN_POINT ( 'NONE',  ( -10.81189881249999729, -6.242252689847864744, -194.1562500020484094 ) ) ;
#41451 = CARTESIAN_POINT ( 'NONE',  ( 7.070501591499376803E-16, 11.54700538379251284, -165.5000000040967905 ) ) ;
#41452 = CARTESIAN_POINT ( 'NONE',  ( 5.000000000000000000, 8.660254037844385522, -148.7500000000000000 ) ) ;
#41453 = CARTESIAN_POINT ( 'NONE',  ( 4.999999999999992006, -8.660254037844389075, -12.74999999999995559 ) ) ;
#41454 = LOCAL_TIME ( 11, 57, 6.000000000000000000, #32597 ) ;
#41455 = CARTESIAN_POINT ( 'NONE',  ( -2.293366432827344421E-15, -12.48450537969573659, -64.71875000204838102 ) ) ;
#41456 = CARTESIAN_POINT ( 'NONE',  ( -10.81189881249999907, -6.242252689847864744, -57.46875000204835970 ) ) ;
#41457 = CARTESIAN_POINT ( 'NONE',  ( -9.999999999999998224, 5.773502691896259087, -186.2500000040967905 ) ) ;
#41458 = CARTESIAN_POINT ( 'NONE',  ( 5.405949406249992428, -9.363379034771808662, -30.28125000204837036 ) ) ;
#41459 = CARTESIAN_POINT ( 'NONE',  ( 10.81189881249999551, -6.242252689847874514, -37.46875000204835970 ) ) ;
#41460 = CARTESIAN_POINT ( 'NONE',  ( -9.999999999999998224, 1.224646799147353059E-15, -52.62500000409675494 ) ) ;
#41461 = CARTESIAN_POINT ( 'NONE',  ( -5.405949406249996869, 9.363379034771805109, -143.3437500020483810 ) ) ;
#41462 = CARTESIAN_POINT ( 'NONE',  ( 9.999999999999998224, 0.000000000000000000, -120.5000000000000000 ) ) ;
#41463 = CARTESIAN_POINT ( 'NONE',  ( -9.999999999999998224, 1.224646799147353059E-15, -41.74999999999997868 ) ) ;
#41464 = CARTESIAN_POINT ( 'NONE',  ( 9.999999999999998224, 0.000000000000000000, -72.49999999999998579 ) ) ;
#41465 = CARTESIAN_POINT ( 'NONE',  ( 7.644554776091147741E-16, 12.48450537969573659, -137.6562500020483810 ) ) ;
#41466 = CARTESIAN_POINT ( 'NONE',  ( 5.405949406249992428, -9.363379034771808662, -6.281250002048377468 ) ) ;
#41467 = ORIENTED_EDGE ( 'NONE', *, *, #24143, .T. ) ;
#41468 = CARTESIAN_POINT ( 'NONE',  ( -5.405949406249996869, 9.363379034771805109, -106.0312500020483810 ) ) ;
#41469 = CARTESIAN_POINT ( 'NONE',  ( -9.999999999999998224, 1.224646799147353059E-15, -114.1250000040967763 ) ) ;
#41470 = CARTESIAN_POINT ( 'NONE',  ( -2.121150477449813534E-15, -11.54700538379251284, -140.3750000000000000 ) ) ;
#41471 = CARTESIAN_POINT ( 'NONE',  ( 10.81189881249999551, -6.242252689847874514, -70.46875000204839523 ) ) ;
#41472 = AXIS2_PLACEMENT_3D ( 'NONE', #23087, #36248, #23518 ) ;
#41473 = CARTESIAN_POINT ( 'NONE',  ( -5.000000000000003553, -8.660254037844383745, -25.37500000409675849 ) ) ;
#41474 = PRODUCT_DEFINITION_SHAPE ( 'NONE', 'NONE',  #42691 ) ;
#41475 =( BOUNDED_CURVE ( )  B_SPLINE_CURVE ( 2, ( #27464, #10826, #40599, #41024, #33524, #3947, #11042 ),
 .UNSPECIFIED., .F., .F. ) 
 B_SPLINE_CURVE_WITH_KNOTS ( ( 3, 2, 2, 3 ),
 ( 0.05597014925373139382, 0.05721393034825875828, 0.05845771144278612275, 0.05970149253731348721 ),
 .UNSPECIFIED. ) 
 CURVE ( )  GEOMETRIC_REPRESENTATION_ITEM ( )  RATIONAL_B_SPLINE_CURVE ( ( 0.9999999999999947820, 0.8660254037844439257, 1.000000000000000000, 0.8660254037844387076, 1.000000000000000000, 0.8660254037844327124, 1.000000000000005995 ) ) 
 REPRESENTATION_ITEM ( '' )  );
#41476 = FACE_OUTER_BOUND ( 'NONE', #17637, .T. ) ;
#41477 = CARTESIAN_POINT ( 'NONE',  ( -10.81189881249999907, -6.242252689847864744, -47.15625000204837391 ) ) ;
#41478 = CARTESIAN_POINT ( 'NONE',  ( 9.999999999999998224, 0.000000000000000000, -200.0000000000000000 ) ) ;
#41479 = CARTESIAN_POINT ( 'NONE',  ( 5.405949406249992428, -9.363379034771808662, -148.7812500020483810 ) ) ;
#41480 = CARTESIAN_POINT ( 'NONE',  ( -10.81189881249999729, 6.242252689847871849, -128.2187500020483810 ) ) ;
#41481 = CARTESIAN_POINT ( 'NONE',  ( 7.070501591499376803E-16, 11.54700538379251284, -51.12499999999998579 ) ) ;
#41482 = CARTESIAN_POINT ( 'NONE',  ( 10.00000000000102318, -5.773502691895667560, -57.62499999999995737 ) ) ;
#41483 = ORIENTED_EDGE ( 'NONE', *, *, #356, .F. ) ;
#41484 = VECTOR ( 'NONE', #8607, 1000.000000000000000 ) ;
#41485 = VERTEX_POINT ( 'NONE', #31322 ) ;
#41486 = EDGE_LOOP ( 'NONE', ( #532, #25822, #13324, #1158 ) ) ;
#41487 = CARTESIAN_POINT ( 'NONE',  ( -9.999999999998456346, -5.773502691897145489, -7.500000004096707862 ) ) ;
#41488 = CARTESIAN_POINT ( 'NONE',  ( 10.81189881249999907, 6.242252689847868297, -179.7187500020484094 ) ) ;
#41489 = AXIS2_PLACEMENT_3D ( 'NONE', #41204, #8220, #4980 ) ;
#41490 = CARTESIAN_POINT ( 'NONE',  ( 5.405949406249992428, -9.363379034771808662, -31.59375000204836681 ) ) ;
#41491 = CARTESIAN_POINT ( 'NONE',  ( 10.00000000000102318, -5.773502691895667560, -41.12499999999993605 ) ) ;
#41492 = ADVANCED_FACE ( 'NONE', ( #1964 ), #7798, .T. ) ;
#41493 = CARTESIAN_POINT ( 'NONE',  ( 10.81189881249999729, 0.000000000000000000, -160.3437500020484094 ) ) ;
#41494 = CARTESIAN_POINT ( 'NONE',  ( 5.405949406249999534, 9.363379034771803333, -155.5937500020483810 ) ) ;
#41495 = DIRECTION ( 'NONE',  ( -0.000000000000000000, -0.000000000000000000, 1.000000000000000000 ) ) ;
#41496 = CARTESIAN_POINT ( 'NONE',  ( 7.644554776091147741E-16, 12.48450537969573659, -134.4687500020483810 ) ) ;
#41497 = CARTESIAN_POINT ( 'NONE',  ( 5.405949406249999534, 9.363379034771803333, -142.2812500020483810 ) ) ;
#41499 = EDGE_CURVE ( 'NONE', #12699, #15995, #30055, .T. ) ;
#41498 = CARTESIAN_POINT ( 'NONE',  ( -2.293366432827344421E-15, -12.48450537969573659, -148.7187500020484094 ) ) ;
#41500 = CARTESIAN_POINT ( 'NONE',  ( 11.54700538379253416, -19.99999999999999289, 45.00000000000009237 ) ) ;
#41501 = LINE ( 'NONE', #28996, #6148 ) ;
#41502 = CARTESIAN_POINT ( 'NONE',  ( -4.999999999999996447, 8.660254037844387298, -168.0000000000000000 ) ) ;
#41503 = EDGE_CURVE ( 'NONE', #3056, #6810, #34477, .T. ) ;
#41504 = CARTESIAN_POINT ( 'NONE',  ( 5.405949406249992428, -9.363379034771808662, -81.09375000204838102 ) ) ;
#41505 = CARTESIAN_POINT ( 'NONE',  ( -5.482716661060788255, 9.345839531454744886, -99.99999999999997158 ) ) ;
#41506 = CARTESIAN_POINT ( 'NONE',  ( 7.644554776091147741E-16, 12.48450537969573659, -59.65625000204838813 ) ) ;
#41507 = CARTESIAN_POINT ( 'NONE',  ( 7.070501591499376803E-16, 11.54700538379251284, -133.6250000000000000 ) ) ;
#41508 = CARTESIAN_POINT ( 'NONE',  ( 10.81189881249999907, 6.242252689847868297, -170.7187500020483810 ) ) ;
#41509 = CARTESIAN_POINT ( 'NONE',  ( -5.405949406250003975, -9.363379034771801557, -116.0312500020483952 ) ) ;
#41510 = CARTESIAN_POINT ( 'NONE',  ( 10.81189881249999729, 6.242252689847867408, -143.9062500020484094 ) ) ;
#41511 = CC_DESIGN_PERSON_AND_ORGANIZATION_ASSIGNMENT ( #32798, #22026, ( #3281 ) ) ;
#41512 = CARTESIAN_POINT ( 'NONE',  ( -9.999999999998456346, -5.773502691897145489, -29.62499999999991829 ) ) ;
#41513 = CARTESIAN_POINT ( 'NONE',  ( 10.81189881249999551, -6.242252689847874514, -43.65625000204836681 ) ) ;
#41514 = CARTESIAN_POINT ( 'NONE',  ( -10.00000000000000000, -5.773502691896251982, -121.5000000040967905 ) ) ;
#41515 = CARTESIAN_POINT ( 'NONE',  ( 4.999999999999992006, -8.660254037844389075, -102.7500000000000000 ) ) ;
#41516 = AXIS2_PLACEMENT_3D ( 'NONE', #4213, #30766, #7666 ) ;
#41517 =( BOUNDED_CURVE ( )  B_SPLINE_CURVE ( 2, ( #12891, #39236, #16122, #32149, #29532, #29319, #42674 ),
 .UNSPECIFIED., .F., .F. ) 
 B_SPLINE_CURVE_WITH_KNOTS ( ( 3, 2, 2, 3 ),
 ( 0.3582089552238806873, 0.3594527363184080726, 0.3606965174129355134, 0.3619402985074628432 ),
 .UNSPECIFIED. ) 
 CURVE ( )  GEOMETRIC_REPRESENTATION_ITEM ( )  RATIONAL_B_SPLINE_CURVE ( ( 0.9999999999999880096, 0.8660254037844506980, 1.000000000000000000, 0.8660254037844387076, 1.000000000000000000, 0.8660254037844207220, 1.000000000000017986 ) ) 
 REPRESENTATION_ITEM ( '' )  );
#41518 = ORIENTED_EDGE ( 'NONE', *, *, #17831, .F. ) ;
#41519 = CARTESIAN_POINT ( 'NONE',  ( -10.81189881249999729, 1.324075727343319199E-15, -126.7812500020483668 ) ) ;
#41520 = CARTESIAN_POINT ( 'NONE',  ( 9.999999999999998224, 0.000000000000000000, -141.8750000040967905 ) ) ;
#41521 = CARTESIAN_POINT ( 'NONE',  ( 7.070501591499376803E-16, 11.54700538379251284, -68.00000000409679046 ) ) ;
#41522 = CARTESIAN_POINT ( 'NONE',  ( 5.405949406249999534, 9.363379034771803333, -178.2812500020484094 ) ) ;
#41523 = EDGE_LOOP ( 'NONE', ( #31586, #12420, #29992, #5566 ) ) ;
#41524 = CARTESIAN_POINT ( 'NONE',  ( 10.81189881249999551, -6.242252689847874514, -173.9687500020484094 ) ) ;
#41525 = CARTESIAN_POINT ( 'NONE',  ( 9.999999999999998224, 0.000000000000000000, -50.37500000409675494 ) ) ;
#41526 = CARTESIAN_POINT ( 'NONE',  ( -9.999999999999998224, 1.224646799147353059E-15, -145.2500000000000000 ) ) ;
#41527 = FACE_OUTER_BOUND ( 'NONE', #36185, .T. ) ;
#41528 = CARTESIAN_POINT ( 'NONE',  ( -5.405949406249996869, 9.363379034771805109, -68.53125000204838102 ) ) ;
#41529 = CARTESIAN_POINT ( 'NONE',  ( -10.00000000000000000, -5.773502691896251982, -46.50000000409676204 ) ) ;
#41530 = CARTESIAN_POINT ( 'NONE',  ( 9.999999999999998224, 0.000000000000000000, -84.49999999999997158 ) ) ;
#41531 = CARTESIAN_POINT ( 'NONE',  ( -10.81189881249999729, 1.324075727343319199E-15, -170.2812500020484094 ) ) ;
#41532 = EDGE_CURVE ( 'NONE', #18570, #8575, #36094, .T. ) ;
#41533 = VECTOR ( 'NONE', #40, 1000.000000000000000 ) ;
#41534 = CARTESIAN_POINT ( 'NONE',  ( -10.00000000000031797, 5.773502691896072569, -183.2500000040967905 ) ) ;
#41535 = CARTESIAN_POINT ( 'NONE',  ( -2.121150477449813534E-15, -11.54700538379251284, -34.25000000409674783 ) ) ;
#41536 = EDGE_LOOP ( 'NONE', ( #15261, #15046, #2915, #9104 ) ) ;
#41537 = CYLINDRICAL_SURFACE ( 'NONE', #22891, 9.999999999999998224 ) ;
#41538 = CARTESIAN_POINT ( 'NONE',  ( 9.999999999999998224, 0.000000000000000000, -111.4999999999999858 ) ) ;
#41539 = DIRECTION ( 'NONE',  ( 0.000000000000000000, 0.000000000000000000, -1.000000000000000000 ) ) ;
#41541 = ORIENTED_EDGE ( 'NONE', *, *, #5126, .F. ) ;
#41540 = CARTESIAN_POINT ( 'NONE',  ( 5.405949406249999534, 9.363379034771803333, -76.28125000204838102 ) ) ;
#41543 = ORIENTED_EDGE ( 'NONE', *, *, #36546, .F. ) ;
#41542 = CARTESIAN_POINT ( 'NONE',  ( 4.999999999999992006, -8.660254037844389075, -143.2500000000000000 ) ) ;
#41544 = VERTEX_POINT ( 'NONE', #41428 ) ;
#41545 = CARTESIAN_POINT ( 'NONE',  ( 10.81189881249999729, 0.000000000000000000, -26.84375000204835970 ) ) ;
#41546 = CARTESIAN_POINT ( 'NONE',  ( 10.00000000000031619, -5.773502691896077010, -186.6250000000000284 ) ) ;
#41547 = CARTESIAN_POINT ( 'NONE',  ( 5.405949406249999534, 9.363379034771803333, -4.281250002048375691 ) ) ;
#41549 = ORIENTED_EDGE ( 'NONE', *, *, #21998, .T. ) ;
#41548 = CARTESIAN_POINT ( 'NONE',  ( -10.81189881249999729, 6.242252689847871849, -57.71875000204836681 ) ) ;
#41550 = CARTESIAN_POINT ( 'NONE',  ( -9.999999999999998224, 1.224646799147353059E-15, -123.1250000040967905 ) ) ;
#41551 = CARTESIAN_POINT ( 'NONE',  ( -10.00000000000000000, -5.773502691896251982, -34.12499999999996447 ) ) ;
#41552 = CARTESIAN_POINT ( 'NONE',  ( 7.644554776091147741E-16, 12.48450537969573659, -194.4687500020484094 ) ) ;
#41553 = CARTESIAN_POINT ( 'NONE',  ( 5.405949406249999534, 9.363379034771803333, -179.5937500020484094 ) ) ;
#41554 = CARTESIAN_POINT ( 'NONE',  ( -10.81189881249999907, -6.242252689847864744, -159.4687500020484094 ) ) ;
#41555 = DIRECTION ( 'NONE',  ( -0.000000000000000000, -0.000000000000000000, 1.000000000000000000 ) ) ;
#41556 = DIRECTION ( 'NONE',  ( 0.000000000000000000, 0.000000000000000000, -1.000000000000000000 ) ) ;
#41557 = CARTESIAN_POINT ( 'NONE',  ( 7.070501591499377789E-16, 11.54700538379251284, -198.1250000000000000 ) ) ;
#41558 = CARTESIAN_POINT ( 'NONE',  ( 10.81189881249999907, 6.242252689847868297, -106.2187500020483668 ) ) ;
#41559 = FACE_OUTER_BOUND ( 'NONE', #18614, .T. ) ;
#41560 = CARTESIAN_POINT ( 'NONE',  ( -5.405949406250003975, -9.363379034771801557, -84.53125000204838102 ) ) ;
#41561 = CARTESIAN_POINT ( 'NONE',  ( -10.81189881249999729, 6.242252689847871849, -89.21875000204838102 ) ) ;
#41562 = CARTESIAN_POINT ( 'NONE',  ( -10.81189881249999729, 6.242252689847871849, -71.40625000204839523 ) ) ;
#41563 = CARTESIAN_POINT ( 'NONE',  ( 4.999999999999992006, -8.660254037844389075, -146.6250000040967905 ) ) ;
#41564 = CARTESIAN_POINT ( 'NONE',  ( -9.999999999999998224, 5.773502691896259087, -121.3750000000000000 ) ) ;
#41565 = ORIENTED_EDGE ( 'NONE', *, *, #34023, .T. ) ;
#41566 = CARTESIAN_POINT ( 'NONE',  ( -10.81189881249999729, 1.324075727343319199E-15, -153.7812500020484094 ) ) ;
#41567 = CARTESIAN_POINT ( 'NONE',  ( -10.81189881249999729, 6.242252689847871849, -165.9062500020483810 ) ) ;
#41568 = EDGE_CURVE ( 'NONE', #41596, #36111, #20254, .T. ) ;
#41569 = CARTESIAN_POINT ( 'NONE',  ( 9.999999999999998224, 0.000000000000000000, -39.49999999999997868 ) ) ;
#41570 = DIRECTION ( 'NONE',  ( -0.000000000000000000, -0.000000000000000000, 1.000000000000000000 ) ) ;
#41571 = CARTESIAN_POINT ( 'NONE',  ( 5.405949406249999534, 9.363379034771803333, -98.59375000204838102 ) ) ;
#41572 = ORIENTED_EDGE ( 'NONE', *, *, #21729, .T. ) ;
#41573 = CARTESIAN_POINT ( 'NONE',  ( -9.999999999999998224, 1.224646799147353059E-15, -68.74999999999997158 ) ) ;
#41574 = CARTESIAN_POINT ( 'NONE',  ( -5.405949406250003975, -9.363379034771801557, -196.8437500020484094 ) ) ;
#41575 = CARTESIAN_POINT ( 'NONE',  ( -4.999999999999996447, 8.660254037844387298, -72.37500000409677625 ) ) ;
#41576 = CARTESIAN_POINT ( 'NONE',  ( 8.048493842490250572, -7.181085626304623659, -179.9999999999999716 ) ) ;
#41577 = CARTESIAN_POINT ( 'NONE',  ( -9.999999999999479527, -5.773502691896549521, -124.1249999999999858 ) ) ;
#41578 = CARTESIAN_POINT ( 'NONE',  ( -2.293366432827344421E-15, -12.48450537969573659, -94.90625000204838102 ) ) ;
#41579 = CARTESIAN_POINT ( 'NONE',  ( 5.405949406249999534, 9.363379034771803333, -77.78125000204838102 ) ) ;
#41580 = CARTESIAN_POINT ( 'NONE',  ( 4.999999999999992006, -8.660254037844389075, -68.62500000409677625 ) ) ;
#41581 = CARTESIAN_POINT ( 'NONE',  ( -9.999999999999998224, 1.224646799147353059E-15, -200.0000000000000000 ) ) ;
#41582 = CARTESIAN_POINT ( 'NONE',  ( -5.405949406250003975, -9.363379034771801557, -25.84375000204835970 ) ) ;
#41583 = ORIENTED_EDGE ( 'NONE', *, *, #27828, .F. ) ;
#41584 = CARTESIAN_POINT ( 'NONE',  ( -5.405949406250003975, -9.363379034771801557, -195.5312500020484094 ) ) ;
#41585 = CARTESIAN_POINT ( 'NONE',  ( -5.405949406249996869, 9.363379034771805109, -19.03125000204835970 ) ) ;
#41586 = CARTESIAN_POINT ( 'NONE',  ( -5.405949406249996869, 9.363379034771805109, -6.843750002048371250 ) ) ;
#41587 = CARTESIAN_POINT ( 'NONE',  ( 5.000000000000000000, 8.660254037844385522, -137.1250000040967620 ) ) ;
#41588 = CARTESIAN_POINT ( 'NONE',  ( 7.644554776091147741E-16, 12.48450537969573659, -144.9687500020483810 ) ) ;
#41589 = CARTESIAN_POINT ( 'NONE',  ( 4.999999999999992006, -8.660254037844389075, 0.3749999959032357388 ) ) ;
#41590 = CARTESIAN_POINT ( 'NONE',  ( -5.000000000000003553, -8.660254037844383745, -173.5000000000000284 ) ) ;
#41591 = CARTESIAN_POINT ( 'NONE',  ( -9.999999999999998224, 1.224646799147353059E-15, -170.7500000000000000 ) ) ;
#41592 = CARTESIAN_POINT ( 'NONE',  ( -4.999999999999996447, 8.660254037844387298, -175.8750000040967905 ) ) ;
#41594 = ORIENTED_EDGE ( 'NONE', *, *, #32029, .F. ) ;
#41593 = CARTESIAN_POINT ( 'NONE',  ( -5.405949406250003975, -9.363379034771801557, -99.53125000204839523 ) ) ;
#41595 = CARTESIAN_POINT ( 'NONE',  ( 4.999999999999992006, -8.660254037844389075, -164.2500000000000000 ) ) ;
#41596 = VERTEX_POINT ( 'NONE', #41848 ) ;
#41597 = VERTEX_POINT ( 'NONE', #22868 ) ;
#41598 = CARTESIAN_POINT ( 'NONE',  ( 5.405949406249999534, 9.363379034771803333, -32.78125000204837391 ) ) ;
#41599 = CARTESIAN_POINT ( 'NONE',  ( 5.405949406249999534, 9.363379034771803333, -79.09375000204838102 ) ) ;
#41600 = CARTESIAN_POINT ( 'NONE',  ( -10.00000000000000000, -5.773502691896252870, -173.6249999999999716 ) ) ;
#41601 = CARTESIAN_POINT ( 'NONE',  ( 9.999999999999742428, 5.773502691896404748, -126.3749999999999858 ) ) ;
#41602 =( BOUNDED_CURVE ( )  B_SPLINE_CURVE ( 2, ( #9009, #41794, #32535, #19141, #29284, #12232, #25423 ),
 .UNSPECIFIED., .F., .F. ) 
 B_SPLINE_CURVE_WITH_KNOTS ( ( 3, 2, 2, 3 ),
 ( 0.1940298507462686894, 0.1952736318407960470, 0.1965174129353234322, 0.1977611940298507898 ),
 .UNSPECIFIED. ) 
 CURVE ( )  GEOMETRIC_REPRESENTATION_ITEM ( )  RATIONAL_B_SPLINE_CURVE ( ( 0.9999999999999970024, 0.8660254037844417052, 1.000000000000000000, 0.8660254037844387076, 1.000000000000000000, 0.8660254037844327124, 1.000000000000005995 ) ) 
 REPRESENTATION_ITEM ( '' )  );
#41603 = DIRECTION ( 'NONE',  ( 0.000000000000000000, 1.000000000000000000, 0.000000000000000000 ) ) ;
#41604 = CARTESIAN_POINT ( 'NONE',  ( 10.81189881249999729, 0.000000000000000000, -168.0312500020484094 ) ) ;
#41605 = CARTESIAN_POINT ( 'NONE',  ( -10.00000000000000000, -5.773502691896251982, -10.50000000409676204 ) ) ;
#41606 = CARTESIAN_POINT ( 'NONE',  ( 9.999999999999998224, 0.000000000000000000, -36.87500000409676915 ) ) ;
#41607 = CARTESIAN_POINT ( 'NONE',  ( 5.405949406249992428, -9.363379034771808662, -118.5937500020483810 ) ) ;
#41608 = CARTESIAN_POINT ( 'NONE',  ( -10.81189881249999729, 1.324075727343319199E-15, -84.59375000204836681 ) ) ;
#41609 = CARTESIAN_POINT ( 'NONE',  ( 10.81189881249999907, 6.242252689847868297, -194.7187500020484094 ) ) ;
#41610 = CARTESIAN_POINT ( 'NONE',  ( -2.293366432827344421E-15, -12.48450537969573659, -91.90625000204838102 ) ) ;
#41611 = CARTESIAN_POINT ( 'NONE',  ( -9.999999999999998224, 5.773502691896259087, -168.2500000040967905 ) ) ;
#41612 = CARTESIAN_POINT ( 'NONE',  ( -5.405949406250003975, -9.363379034771801557, -171.5312500020484094 ) ) ;
#41613 = CARTESIAN_POINT ( 'NONE',  ( -2.121150477449813534E-15, -11.54700538379251284, -28.25000000409675138 ) ) ;
#41614 = CARTESIAN_POINT ( 'NONE',  ( -5.405949406250003975, -9.363379034771801557, -174.5312500020484094 ) ) ;
#41615 = CARTESIAN_POINT ( 'NONE',  ( 10.81189881249999729, 0.000000000000000000, -187.5312500020484094 ) ) ;
#41616 = CARTESIAN_POINT ( 'NONE',  ( 10.81189881249999551, -6.242252689847874514, -41.96875000204834549 ) ) ;
#41617 = CARTESIAN_POINT ( 'NONE',  ( -2.121150477449813534E-15, -11.54700538379251284, -160.2500000040967620 ) ) ;
#41618 = CARTESIAN_POINT ( 'NONE',  ( -2.293366432827344421E-15, -12.48450537969573659, -3.406250002048348158 ) ) ;
#41619 = CARTESIAN_POINT ( 'NONE',  ( -5.405949406250003975, -9.363379034771801557, -13.84375000204834905 ) ) ;
#41620 = CARTESIAN_POINT ( 'NONE',  ( 4.999999999999992006, -8.660254037844389075, -158.6250000040967905 ) ) ;
#41621 = CARTESIAN_POINT ( 'NONE',  ( 5.405949406249999534, 9.363379034771803333, -125.5937500020483668 ) ) ;
#41622 = CARTESIAN_POINT ( 'NONE',  ( -5.000000000000003553, -8.660254037844383745, -87.99999999999998579 ) ) ;
#41623 = CARTESIAN_POINT ( 'NONE',  ( -2.293366432827344421E-15, -12.48450537969573659, -24.40625000204838102 ) ) ;
#41624 = CARTESIAN_POINT ( 'NONE',  ( 5.000000000000000000, 8.660254037844385522, -105.6250000040967763 ) ) ;
#41625 = CARTESIAN_POINT ( 'NONE',  ( 0.000000000000000000, 0.000000000000000000, -200.0000000000000000 ) ) ;
#41626 = CARTESIAN_POINT ( 'NONE',  ( -2.293366432827344421E-15, -12.48450537969573659, -114.4062500020483952 ) ) ;
#41627 = CARTESIAN_POINT ( 'NONE',  ( -10.81189881249999729, 1.324075727343319199E-15, -102.7812500020483952 ) ) ;
#41628 = VERTEX_POINT ( 'NONE', #28723 ) ;
#41629 = CARTESIAN_POINT ( 'NONE',  ( 10.00000000000000000, 5.773502691896255534, -92.25000000409679046 ) ) ;
#41630 = FACE_OUTER_BOUND ( 'NONE', #39872, .T. ) ;
#41631 = CARTESIAN_POINT ( 'NONE',  ( 10.81189881249999907, 6.242252689847868297, -154.4062500020484094 ) ) ;
#41632 = CARTESIAN_POINT ( 'NONE',  ( -10.81189881249999729, 1.324075727343319199E-15, -53.09375000204835970 ) ) ;
#41633 = EDGE_LOOP ( 'NONE', ( #10003, #27295, #26472, #4930 ) ) ;
#41634 = CARTESIAN_POINT ( 'NONE',  ( 9.999999999999998224, 0.000000000000000000, -16.99999999999996092 ) ) ;
#41635 = CARTESIAN_POINT ( 'NONE',  ( -5.405949406249996869, 9.363379034771805109, -31.03125000204837036 ) ) ;
#41636 = CARTESIAN_POINT ( 'NONE',  ( 10.00000000000000000, 5.773502691896255534, -154.8750000000000000 ) ) ;
#41637 = CARTESIAN_POINT ( 'NONE',  ( -4.999999999999996447, 8.660254037844387298, -18.37500000409675494 ) ) ;
#41638 = EDGE_CURVE ( 'NONE', #30453, #29986, #6603, .T. ) ;
#41639 = CARTESIAN_POINT ( 'NONE',  ( -9.999999999999998224, 1.224646799147353059E-15, -196.2500000000000000 ) ) ;
#41640 = CARTESIAN_POINT ( 'NONE',  ( -5.405949406250003975, -9.363379034771801557, -125.0312500020483952 ) ) ;
#41641 = CARTESIAN_POINT ( 'NONE',  ( -5.000000000000003553, -8.660254037844383745, -21.99999999999996447 ) ) ;
#41642 = CARTESIAN_POINT ( 'NONE',  ( 9.999999999999998224, 0.000000000000000000, -143.3750000040967905 ) ) ;
#41643 = ORIENTED_EDGE ( 'NONE', *, *, #26060, .T. ) ;
#41644 =( BOUNDED_CURVE ( )  B_SPLINE_CURVE ( 2, ( #10568, #39508, #30456, #40140, #883, #16611, #9938 ),
 .UNSPECIFIED., .F., .F. ) 
 B_SPLINE_CURVE_WITH_KNOTS ( ( 3, 2, 2, 3 ),
 ( 0.9589552238805971740, 0.9601990049751244483, 0.9614427860696519446, 0.9626865671641793298 ),
 .UNSPECIFIED. ) 
 CURVE ( )  GEOMETRIC_REPRESENTATION_ITEM ( )  RATIONAL_B_SPLINE_CURVE ( ( 0.9999999999999880096, 0.8660254037844506980, 1.000000000000000000, 0.8660254037844387076, 1.000000000000000000, 0.8660254037844148378, 1.000000000000023981 ) ) 
 REPRESENTATION_ITEM ( '' )  );
#41645 = CARTESIAN_POINT ( 'NONE',  ( 10.81189881249999551, -6.242252689847874514, -55.65625000204836681 ) ) ;
#41646 = APPLICATION_PROTOCOL_DEFINITION ( 'international standard', 'config_control_design', 1994, #11857 ) ;
#41647 = CARTESIAN_POINT ( 'NONE',  ( 5.405949406249992428, -9.363379034771808662, -114.0937500020483810 ) ) ;
#41649 = ORIENTED_EDGE ( 'NONE', *, *, #11440, .F. ) ;
#41648 = ORIENTED_EDGE ( 'NONE', *, *, #5631, .F. ) ;
#41650 = CARTESIAN_POINT ( 'NONE',  ( 0.000000000000000000, 0.000000000000000000, -99.99999999999998579 ) ) ;
#41651 = CARTESIAN_POINT ( 'NONE',  ( -9.999999999999998224, 1.224646799147353059E-15, -170.7500000000000000 ) ) ;
#41652 = CARTESIAN_POINT ( 'NONE',  ( 10.81189881249999907, 6.242252689847868297, -157.2187500020483810 ) ) ;
#41653 =( BOUNDED_CURVE ( )  B_SPLINE_CURVE ( 2, ( #27007, #30889, #14457, #4555, #24429, #1109, #24210 ),
 .UNSPECIFIED., .F., .F. ) 
 B_SPLINE_CURVE_WITH_KNOTS ( ( 3, 2, 2, 3 ),
 ( 0.2574626865671643117, 0.2587064676616916414, 0.2599502487562190267, 0.2611940298507463565 ),
 .UNSPECIFIED. ) 
 CURVE ( )  GEOMETRIC_REPRESENTATION_ITEM ( )  RATIONAL_B_SPLINE_CURVE ( ( 0.9999999999999880096, 0.8660254037844506980, 1.000000000000000000, 0.8660254037844387076, 1.000000000000000000, 0.8660254037844267172, 1.000000000000011990 ) ) 
 REPRESENTATION_ITEM ( '' )  );
#41654 = CARTESIAN_POINT ( 'NONE',  ( 5.405949406249992428, -9.363379034771808662, -192.2812500020484094 ) ) ;
#41655 = CARTESIAN_POINT ( 'NONE',  ( 10.81189881249999551, -6.242252689847874514, -5.968750002048344605 ) ) ;
#41656 = EDGE_CURVE ( 'NONE', #20021, #22821, #41887, .T. ) ;
#41657 = CARTESIAN_POINT ( 'NONE',  ( -10.81189881249999729, 6.242252689847871849, -143.2187500020483810 ) ) ;
#41658 = CARTESIAN_POINT ( 'NONE',  ( -5.405949406250003975, -9.363379034771801557, -109.8437500020483810 ) ) ;
#41659 = CARTESIAN_POINT ( 'NONE',  ( 9.999999999999998224, 0.000000000000000000, -188.0000000000000000 ) ) ;
#41660 = CARTESIAN_POINT ( 'NONE',  ( 10.81189881249999729, 0.000000000000000000, -115.5312500020483952 ) ) ;
#41661 = CARTESIAN_POINT ( 'NONE',  ( 10.81189881249999907, 6.242252689847868297, -5.718750002048342829 ) ) ;
#41662 = CARTESIAN_POINT ( 'NONE',  ( -2.293366432827344421E-15, -12.48450537969573659, -124.7187500020483952 ) ) ;
#41663 = CARTESIAN_POINT ( 'NONE',  ( -10.81189881249999729, 1.324075727343319199E-15, -197.2812500020484094 ) ) ;
#41664 = DIRECTION ( 'NONE',  ( -1.000000000000000000, 0.000000000000000000, 0.000000000000000000 ) ) ;
#41665 = CARTESIAN_POINT ( 'NONE',  ( 7.070501591499377789E-16, 11.54700538379251284, -144.1250000000000000 ) ) ;
#41666 = CARTESIAN_POINT ( 'NONE',  ( 4.999999999999992006, -8.660254037844389075, -9.749999999999953815 ) ) ;
#41667 = CARTESIAN_POINT ( 'NONE',  ( -10.81189881249999729, 6.242252689847871849, -69.71875000204838102 ) ) ;
#41668 = CARTESIAN_POINT ( 'NONE',  ( 7.644554776091147741E-16, 12.48450537969573659, -56.46875000204837391 ) ) ;
#41669 = CARTESIAN_POINT ( 'NONE',  ( -2.121150477449813534E-15, -11.54700538379251284, -184.2500000040967905 ) ) ;
#41670 = CARTESIAN_POINT ( 'NONE',  ( 5.405949406249999534, 9.363379034771803333, -26.78125000204836681 ) ) ;
#41671 = CARTESIAN_POINT ( 'NONE',  ( 10.81189881249999907, 6.242252689847868297, -37.21875000204835260 ) ) ;
#41672 = CARTESIAN_POINT ( 'NONE',  ( 5.000000000000000000, 8.660254037844385522, -95.12500000409677625 ) ) ;
#41673 = CARTESIAN_POINT ( 'NONE',  ( 10.81189881249999729, 0.000000000000000000, -142.3437500020483810 ) ) ;
#41674 = CARTESIAN_POINT ( 'NONE',  ( 9.999999999999998224, 0.000000000000000000, -115.9999999999999858 ) ) ;
#41675 = CYLINDRICAL_SURFACE ( 'NONE', #38286, 9.999999999999998224 ) ;
#41676 = CARTESIAN_POINT ( 'NONE',  ( 7.070501591499377789E-16, 11.54700538379251284, -78.12500000000000000 ) ) ;
#41677 = CARTESIAN_POINT ( 'NONE',  ( 10.81189881249999551, -6.242252689847874514, -144.1562500020484094 ) ) ;
#41678 = CARTESIAN_POINT ( 'NONE',  ( -10.81189881249999729, -6.242252689847864744, -9.656250002048379244 ) ) ;
#41679 = ORIENTED_EDGE ( 'NONE', *, *, #16436, .T. ) ;
#41680 = CARTESIAN_POINT ( 'NONE',  ( 9.999999999999998224, 0.000000000000000000, -61.99999999999997158 ) ) ;
#41681 = CARTESIAN_POINT ( 'NONE',  ( 9.999999999999998224, 0.000000000000000000, -116.3750000040967905 ) ) ;
#41682 = CARTESIAN_POINT ( 'NONE',  ( -10.00000000000154188, 5.773502691895366468, -8.874999999999937828 ) ) ;
#41683 = CARTESIAN_POINT ( 'NONE',  ( -5.405949406250003975, -9.363379034771801557, -75.34375000204838102 ) ) ;
#41684 = CARTESIAN_POINT ( 'NONE',  ( -9.999999999999998224, 5.773502691896259087, -38.87499999999995737 ) ) ;
#41685 = CARTESIAN_POINT ( 'NONE',  ( 7.070501591499377789E-16, 11.54700538379251284, -23.00000000409677270 ) ) ;
#41686 = CARTESIAN_POINT ( 'NONE',  ( -9.999999999999998224, 1.224646799147353059E-15, -142.2500000000000000 ) ) ;
#41687 = CARTESIAN_POINT ( 'NONE',  ( -5.405949406250003975, -9.363379034771801557, -38.03125000204838102 ) ) ;
#41688 = CARTESIAN_POINT ( 'NONE',  ( -2.121150477449813534E-15, -11.54700538379251284, -99.87500000000000000 ) ) ;
#41689 = CARTESIAN_POINT ( 'NONE',  ( -2.293366432827344421E-15, -12.48450537969573659, -141.4062500020483810 ) ) ;
#41690 = CARTESIAN_POINT ( 'NONE',  ( -5.405949406249996869, 9.363379034771805109, -148.0312500020483810 ) ) ;
#41692 = EDGE_CURVE ( 'NONE', #41040, #13865, #28679, .T. ) ;
#41691 = CARTESIAN_POINT ( 'NONE',  ( -10.00000000000154188, 5.773502691895366468, -59.87499999999995026 ) ) ;
#41693 = CARTESIAN_POINT ( 'NONE',  ( -5.000000000000003553, -8.660254037844383745, -173.8750000040968189 ) ) ;
#41694 = ORIENTED_EDGE ( 'NONE', *, *, #29565, .F. ) ;
#41695 = ORIENTED_EDGE ( 'NONE', *, *, #6508, .T. ) ;
#41696 = ORIENTED_EDGE ( 'NONE', *, *, #40550, .F. ) ;
#41697 = CARTESIAN_POINT ( 'NONE',  ( -9.999999999999998224, 1.224646799147353059E-15, -100.6250000040967905 ) ) ;
#41698 = CARTESIAN_POINT ( 'NONE',  ( 10.81189881249999907, 6.242252689847868297, -178.2187500020483810 ) ) ;
#41699 = CARTESIAN_POINT ( 'NONE',  ( -10.81189881249999907, -6.242252689847864744, -30.46875000204834549 ) ) ;
#41700 = DIRECTION ( 'NONE',  ( 1.000000000000000000, 0.000000000000000000, 0.000000000000000000 ) ) ;
#41701 = CARTESIAN_POINT ( 'NONE',  ( 10.81189881249999729, 6.242252689847867408, -166.2187500020483810 ) ) ;
#41702 = CARTESIAN_POINT ( 'NONE',  ( -5.405949406250003975, -9.363379034771801557, -156.3437500020483810 ) ) ;
#41703 = CARTESIAN_POINT ( 'NONE',  ( -10.81189881249999729, 1.324075727343319199E-15, -137.0937500020483810 ) ) ;
#41704 = VECTOR ( 'NONE', #27197, 1000.000000000000000 ) ;
#41705 = CARTESIAN_POINT ( 'NONE',  ( -10.81189881249999729, 1.324075727343319199E-15, -137.2812500020483810 ) ) ;
#41706 = CARTESIAN_POINT ( 'NONE',  ( 5.405949406249999534, 9.363379034771803333, -148.0937500020483810 ) ) ;
#41707 = CARTESIAN_POINT ( 'NONE',  ( -9.999999999999742428, -5.773502691896402084, -152.6249999999999716 ) ) ;
#41708 = CARTESIAN_POINT ( 'NONE',  ( -9.999999999999998224, 1.224646799147353059E-15, -75.12500000409677625 ) ) ;
#41709 = CARTESIAN_POINT ( 'NONE',  ( -4.999999999999996447, 8.660254037844387298, -169.5000000000000000 ) ) ;
#41710 = CARTESIAN_POINT ( 'NONE',  ( -10.81189881249999729, 1.324075727343319199E-15, -83.09375000204836681 ) ) ;
#41711 = CARTESIAN_POINT ( 'NONE',  ( 5.405949406249992428, -9.363379034771808662, -52.78125000204836681 ) ) ;
#41712 = DIRECTION ( 'NONE',  ( -0.000000000000000000, -0.000000000000000000, 1.000000000000000000 ) ) ;
#41713 = CARTESIAN_POINT ( 'NONE',  ( -10.81189881249999729, 1.324075727343319199E-15, -173.0937500020484094 ) ) ;
#41714 = CARTESIAN_POINT ( 'NONE',  ( 4.999999999999992006, -8.660254037844389075, -134.2499999999999716 ) ) ;
#41715 = VECTOR ( 'NONE', #14451, 1000.000000000000000 ) ;
#41716 = CARTESIAN_POINT ( 'NONE',  ( -10.81189881249999729, -6.242252689847864744, -149.1562500020484094 ) ) ;
#41717 =( BOUNDED_CURVE ( )  B_SPLINE_CURVE ( 2, ( #36050, #16374, #3248, #19424, #16166, #42501, #12929 ),
 .UNSPECIFIED., .F., .F. ) 
 B_SPLINE_CURVE_WITH_KNOTS ( ( 3, 2, 2, 3 ),
 ( 0.06343283582089558059, 0.06467661691542293811, 0.06592039800995032339, 0.06716417910447768091 ),
 .UNSPECIFIED. ) 
 CURVE ( )  GEOMETRIC_REPRESENTATION_ITEM ( )  RATIONAL_B_SPLINE_CURVE ( ( 0.9999999999999940048, 0.8660254037844447028, 1.000000000000000000, 0.8660254037844387076, 1.000000000000000000, 0.8660254037844312691, 1.000000000000007550 ) ) 
 REPRESENTATION_ITEM ( '' )  );
#41718 = DIRECTION ( 'NONE',  ( -0.000000000000000000, -0.000000000000000000, 1.000000000000000000 ) ) ;
#41719 = CARTESIAN_POINT ( 'NONE',  ( -5.405949406249996869, 9.363379034771805109, -38.53125000204838102 ) ) ;
#41720 = CARTESIAN_POINT ( 'NONE',  ( 9.999999999999996447, -5.773502691896262640, -122.5000000040967905 ) ) ;
#41721 = CARTESIAN_POINT ( 'NONE',  ( -9.999999999999998224, 1.224646799147353059E-15, -101.7500000000000000 ) ) ;
#41722 = EDGE_LOOP ( 'NONE', ( #9275, #13758, #6264, #37649 ) ) ;
#41723 = CARTESIAN_POINT ( 'NONE',  ( 10.81189881249999729, 6.242252689847867408, -116.9062500020483952 ) ) ;
#41724 = CARTESIAN_POINT ( 'NONE',  ( 4.999999999999992006, -8.660254037844389075, -140.6250000040967905 ) ) ;
#41725 = CARTESIAN_POINT ( 'NONE',  ( 0.000000000000000000, 0.000000000000000000, -200.0000000000000000 ) ) ;
#41726 = CARTESIAN_POINT ( 'NONE',  ( 7.644554776091147741E-16, 12.48450537969573659, -181.1562500020484094 ) ) ;
#41727 = VERTEX_POINT ( 'NONE', #6256 ) ;
#41728 = CARTESIAN_POINT ( 'NONE',  ( 4.999999999999992006, -8.660254037844389075, -50.62500000409675494 ) ) ;
#41729 = DIRECTION ( 'NONE',  ( -0.000000000000000000, -0.000000000000000000, 1.000000000000000000 ) ) ;
#41730 = CARTESIAN_POINT ( 'NONE',  ( -5.405949406250003975, -9.363379034771801557, -69.53125000204838102 ) ) ;
#41731 = CYLINDRICAL_SURFACE ( 'NONE', #13128, 9.999999999999998224 ) ;
#41732 = CARTESIAN_POINT ( 'NONE',  ( 10.81189881249999729, 0.000000000000000000, -172.5312500020484094 ) ) ;
#41733 = CYLINDRICAL_SURFACE ( 'NONE', #5668, 9.999999999999998224 ) ;
#41735 = EDGE_CURVE ( 'NONE', #11758, #17267, #34730, .T. ) ;
#41734 = LINE ( 'NONE', #2692, #35819 ) ;
#41736 = VERTEX_POINT ( 'NONE', #2390 ) ;
#41737 = CARTESIAN_POINT ( 'NONE',  ( 0.000000000000000000, 20.00000000000000000, -220.0000000000000000 ) ) ;
#41738 = ADVANCED_FACE ( 'NONE', ( #25272 ), #22020, .T. ) ;
#41739 = VECTOR ( 'NONE', #22721, 1000.000000000000000 ) ;
#41740 = EDGE_CURVE ( 'NONE', #9407, #27758, #2180, .T. ) ;
#41741 = VECTOR ( 'NONE', #20298, 1000.000000000000000 ) ;
#41742 = DIRECTION ( 'NONE',  ( 0.000000000000000000, 0.000000000000000000, 1.000000000000000000 ) ) ;
#41744 = ORIENTED_EDGE ( 'NONE', *, *, #42385, .F. ) ;
#41743 = CARTESIAN_POINT ( 'NONE',  ( -10.81189881249999907, -6.242252689847864744, -77.15625000204836681 ) ) ;
#41745 = DIRECTION ( 'NONE',  ( 1.000000000000000000, 0.000000000000000000, 0.000000000000000000 ) ) ;
#41747 = EDGE_LOOP ( 'NONE', ( #5630, #2101, #16150, #41799 ) ) ;
#41746 = CARTESIAN_POINT ( 'NONE',  ( -9.999999999999998224, 1.224646799147353059E-15, -53.74999999999996447 ) ) ;
#41748 = ORIENTED_EDGE ( 'NONE', *, *, #30704, .F. ) ;
#41749 = CARTESIAN_POINT ( 'NONE',  ( -10.81189881249999729, 6.242252689847871849, -29.21875000204835615 ) ) ;
#41750 = CARTESIAN_POINT ( 'NONE',  ( -4.999999999999996447, 8.660254037844387298, -73.87500000409677625 ) ) ;
#41751 = CARTESIAN_POINT ( 'NONE',  ( -10.81189881249999729, 1.324075727343319199E-15, -6.781250002048377468 ) ) ;
#41753 = VERTEX_POINT ( 'NONE', #42066 ) ;
#41752 = CARTESIAN_POINT ( 'NONE',  ( 7.644554776091147741E-16, 12.48450537969573659, -57.96875000204836681 ) ) ;
#41754 = CARTESIAN_POINT ( 'NONE',  ( -2.121150477449813534E-15, -11.54700538379251284, -36.87499999999996447 ) ) ;
#41755 = EDGE_CURVE ( 'NONE', #28241, #1967, #13759, .T. ) ;
#41756 = CARTESIAN_POINT ( 'NONE',  ( 7.644554776091147741E-16, 12.48450537969573659, -191.4687500020484094 ) ) ;
#41757 = CARTESIAN_POINT ( 'NONE',  ( -10.81189881249999729, 1.324075727343319199E-15, -179.0937500020484094 ) ) ;
#41758 = CARTESIAN_POINT ( 'NONE',  ( 5.405949406249992428, -9.363379034771808662, -159.0937500020484094 ) ) ;
#41759 =( BOUNDED_CURVE ( )  B_SPLINE_CURVE ( 2, ( #36996, #24488, #10867, #7431, #24058, #20582, #33772 ),
 .UNSPECIFIED., .F., .F. ) 
 B_SPLINE_CURVE_WITH_KNOTS ( ( 3, 2, 2, 3 ),
 ( 0.3694029850746269883, 0.3706467661691543181, 0.3718905472636816478, 0.3731343283582090331 ),
 .UNSPECIFIED. ) 
 CURVE ( )  GEOMETRIC_REPRESENTATION_ITEM ( )  RATIONAL_B_SPLINE_CURVE ( ( 0.9999999999999880096, 0.8660254037844506980, 1.000000000000000000, 0.8660254037844387076, 1.000000000000000000, 0.8660254037844327124, 1.000000000000005995 ) ) 
 REPRESENTATION_ITEM ( '' )  );
#41760 = CARTESIAN_POINT ( 'NONE',  ( -10.81189881249999729, 6.242252689847871849, -171.7187500020483810 ) ) ;
#41761 = CARTESIAN_POINT ( 'NONE',  ( -9.999999999999998224, 1.224646799147353059E-15, -18.12500000409675138 ) ) ;
#41762 = CARTESIAN_POINT ( 'NONE',  ( 4.999999999999992006, -8.660254037844389075, -101.6250000040967905 ) ) ;
#41763 = EDGE_CURVE ( 'NONE', #20093, #30868, #18183, .T. ) ;
#41764 = CARTESIAN_POINT ( 'NONE',  ( 9.999999999999996447, -5.773502691896262640, -198.6250000000000284 ) ) ;
#41765 = CARTESIAN_POINT ( 'NONE',  ( -10.81189881249999729, 1.324075727343319199E-15, -105.5937500020483810 ) ) ;
#41766 = CARTESIAN_POINT ( 'NONE',  ( 5.405949406249999534, 9.363379034771803333, -76.28125000204838102 ) ) ;
#41767 = CARTESIAN_POINT ( 'NONE',  ( -10.81189881249999729, -6.242252689847864744, -91.96875000204838102 ) ) ;
#41768 = EDGE_CURVE ( 'NONE', #28673, #18350, #38418, .T. ) ;
#41769 = CONICAL_SURFACE ( 'NONE', #23894, 42.00000000000004974, 0.7853981633974495002 ) ;
#41770 = CARTESIAN_POINT ( 'NONE',  ( -10.81189881249999729, 1.324075727343319199E-15, -69.78125000204838102 ) ) ;
#41771 = CARTESIAN_POINT ( 'NONE',  ( -2.121150477449813534E-15, -11.54700538379251284, -143.7500000040968189 ) ) ;
#41772 = CARTESIAN_POINT ( 'NONE',  ( 9.999999999999996447, -5.773502691896262640, -123.6250000000000000 ) ) ;
#41773 = CARTESIAN_POINT ( 'NONE',  ( 5.405949406249992428, -9.363379034771808662, -151.7812500020484094 ) ) ;
#41774 = CARTESIAN_POINT ( 'NONE',  ( -5.405949406250003975, -9.363379034771801557, -164.0312500020484094 ) ) ;
#41775 = CARTESIAN_POINT ( 'NONE',  ( -9.999999999999998224, 1.224646799147353059E-15, -175.2500000000000284 ) ) ;
#41776 = CARTESIAN_POINT ( 'NONE',  ( -2.293366432827344421E-15, -12.48450537969573659, -99.21875000204839523 ) ) ;
#41777 = ORIENTED_EDGE ( 'NONE', *, *, #33338, .T. ) ;
#41778 = CARTESIAN_POINT ( 'NONE',  ( -2.121150477449813534E-15, -11.54700538379251284, -62.37499999999997868 ) ) ;
#41779 = CARTESIAN_POINT ( 'NONE',  ( -10.81189881249999729, 1.324075727343319199E-15, -194.0937500020484094 ) ) ;
#41780 = CARTESIAN_POINT ( 'NONE',  ( -10.00000000000000000, -5.773502691896251982, -78.00000000409677625 ) ) ;
#41781 = EDGE_CURVE ( 'NONE', #32484, #14676, #40302, .T. ) ;
#41782 = CARTESIAN_POINT ( 'NONE',  ( -8.460957583164166351, -5.382509563854436685, -180.0000000000000853 ) ) ;
#41783 = CARTESIAN_POINT ( 'NONE',  ( -5.000000000000003553, -8.660254037844383745, -11.87500000409674783 ) ) ;
#41784 = CARTESIAN_POINT ( 'NONE',  ( 5.405949406249992428, -9.363379034771808662, -91.78125000204838102 ) ) ;
#41785 = CARTESIAN_POINT ( 'NONE',  ( -10.81189881249999729, 1.324075727343319199E-15, -65.28125000204838102 ) ) ;
#41786 = CARTESIAN_POINT ( 'NONE',  ( 4.999999999999992006, -8.660254037844389075, -67.12500000409676204 ) ) ;
#41787 = DIRECTION ( 'NONE',  ( -0.000000000000000000, -0.000000000000000000, 1.000000000000000000 ) ) ;
#41788 = CARTESIAN_POINT ( 'NONE',  ( -5.405949406249996869, 9.363379034771805109, -24.84375000204835970 ) ) ;
#41789 = ORIENTED_EDGE ( 'NONE', *, *, #27249, .T. ) ;
#41790 = CARTESIAN_POINT ( 'NONE',  ( 7.644554776091147741E-16, 12.48450537969573659, -191.6562500020484094 ) ) ;
#41791 = CARTESIAN_POINT ( 'NONE',  ( 5.405949406249992428, -9.363379034771808662, -24.28125000204836681 ) ) ;
#41792 = CARTESIAN_POINT ( 'NONE',  ( 7.644554776091147741E-16, 12.48450537969573659, -6.968750002048348158 ) ) ;
#41793 = CARTESIAN_POINT ( 'NONE',  ( -5.000000000000003553, -8.660254037844383745, -110.8750000040967763 ) ) ;
#41794 = CARTESIAN_POINT ( 'NONE',  ( 9.999999999999872102, 5.773502691896329253, -159.7500000040967905 ) ) ;
#41795 = EDGE_CURVE ( 'NONE', #848, #26104, #42132, .T. ) ;
#41796 = CARTESIAN_POINT ( 'NONE',  ( 5.000000000000000000, 8.660254037844385522, -172.7500000000000284 ) ) ;
#41797 = CARTESIAN_POINT ( 'NONE',  ( -4.999999999999996447, 8.660254037844387298, -1.499999999999973577 ) ) ;
#41799 = ORIENTED_EDGE ( 'NONE', *, *, #27150, .F. ) ;
#41798 = CARTESIAN_POINT ( 'NONE',  ( 5.405949406249999534, 9.363379034771803333, -100.2812500020483952 ) ) ;
#41800 = CARTESIAN_POINT ( 'NONE',  ( 9.999999999999998224, 0.000000000000000000, -116.3750000040967905 ) ) ;
#41801 = ORIENTED_EDGE ( 'NONE', *, *, #5631, .T. ) ;
#41802 = VERTEX_POINT ( 'NONE', #36869 ) ;
#41803 = CARTESIAN_POINT ( 'NONE',  ( -10.81189881249999907, -6.242252689847864744, -32.15625000204835970 ) ) ;
#41804 = CARTESIAN_POINT ( 'NONE',  ( 9.999999999999998224, 0.000000000000000000, -149.0000000000000000 ) ) ;
#41805 = DATE_AND_TIME ( #25225, #33225 ) ;
#41806 = CARTESIAN_POINT ( 'NONE',  ( -10.81189881249999729, 6.242252689847871849, -77.21875000204838102 ) ) ;
#41807 = CYLINDRICAL_SURFACE ( 'NONE', #11849, 9.999999999999998224 ) ;
#41808 = CARTESIAN_POINT ( 'NONE',  ( 7.320067886350967612, 7.614036460224446579, -99.99999999999998579 ) ) ;
#41809 = EDGE_CURVE ( 'NONE', #5939, #8336, #39114, .T. ) ;
#41810 = DIRECTION ( 'NONE',  ( -0.000000000000000000, -0.000000000000000000, 1.000000000000000000 ) ) ;
#41811 = CARTESIAN_POINT ( 'NONE',  ( 5.405949406249992428, -9.363379034771808662, -153.2812500020484094 ) ) ;
#41812 = CARTESIAN_POINT ( 'NONE',  ( 4.999999999999992006, -8.660254037844389075, -11.62500000409674783 ) ) ;
#41813 = CARTESIAN_POINT ( 'NONE',  ( -5.000000000000003553, -8.660254037844383745, -199.0000000000000000 ) ) ;
#41814 = CARTESIAN_POINT ( 'NONE',  ( 5.405949406249992428, -9.363379034771808662, -130.5937500020483810 ) ) ;
#41815 = CARTESIAN_POINT ( 'NONE',  ( 10.81189881249999551, -6.242252689847874514, -112.4687500020483810 ) ) ;
#41816 = CARTESIAN_POINT ( 'NONE',  ( -5.405949406250003975, -9.363379034771801557, -84.34375000204836681 ) ) ;
#41817 = CARTESIAN_POINT ( 'NONE',  ( 10.81189881249999729, 0.000000000000000000, -90.03125000204838102 ) ) ;
#41818 = CARTESIAN_POINT ( 'NONE',  ( 4.999999999999992006, -8.660254037844389075, -173.6250000040968189 ) ) ;
#41819 = CARTESIAN_POINT ( 'NONE',  ( 10.81189881249999729, 6.242252689847867408, -169.4062500020484094 ) ) ;
#41820 = CARTESIAN_POINT ( 'NONE',  ( -9.999999999999998224, 1.224646799147353059E-15, -102.1250000040967905 ) ) ;
#41821 = CARTESIAN_POINT ( 'NONE',  ( 5.405949406249999534, 9.363379034771803333, -175.2812500020484094 ) ) ;
#41822 = CARTESIAN_POINT ( 'NONE',  ( 5.405949406249999534, 9.363379034771803333, -185.7812500020484094 ) ) ;
#41823 = CARTESIAN_POINT ( 'NONE',  ( -5.405949406249996869, 9.363379034771805109, -47.34375000204838102 ) ) ;
#41824 = CARTESIAN_POINT ( 'NONE',  ( 9.999999999999998224, 0.000000000000000000, -162.8750000040967905 ) ) ;
#41825 = CARTESIAN_POINT ( 'NONE',  ( -4.999999999999996447, 8.660254037844387298, -85.87500000409677625 ) ) ;
#41826 = CARTESIAN_POINT ( 'NONE',  ( 5.405949406249999534, 9.363379034771803333, -17.59375000204835260 ) ) ;
#41827 = CARTESIAN_POINT ( 'NONE',  ( -5.000000000000003553, -8.660254037844383745, -157.0000000000000000 ) ) ;
#41828 = CARTESIAN_POINT ( 'NONE',  ( -5.405949406250003975, -9.363379034771801557, -121.8437500020483952 ) ) ;
#41829 = CARTESIAN_POINT ( 'NONE',  ( 7.070501591499377789E-16, 11.54700538379251284, -85.62499999999997158 ) ) ;
#41830 = CARTESIAN_POINT ( 'NONE',  ( -5.405949406249996869, 9.363379034771805109, -17.53125000204835970 ) ) ;
#41831 = CARTESIAN_POINT ( 'NONE',  ( 9.999999999999996447, -5.773502691896262640, -97.00000000409677625 ) ) ;
#41832 = CARTESIAN_POINT ( 'NONE',  ( 9.999999999999998224, 0.000000000000000000, -200.0000000000000000 ) ) ;
#41833 = CARTESIAN_POINT ( 'NONE',  ( -10.81189881249999729, 1.324075727343319199E-15, -113.2812500020483952 ) ) ;
#41834 = CARTESIAN_POINT ( 'NONE',  ( 5.405949406249992428, -9.363379034771808662, -100.7812500020483952 ) ) ;
#41835 = ORIENTED_EDGE ( 'NONE', *, *, #19278, .T. ) ;
#41836 = CARTESIAN_POINT ( 'NONE',  ( -5.000000000000003553, -8.660254037844383745, -92.87500000409677625 ) ) ;
#41837 = LINE ( 'NONE', #36644, #21546 ) ;
#41838 = CARTESIAN_POINT ( 'NONE',  ( 7.644554776091147741E-16, 12.48450537969573659, -158.6562500020484094 ) ) ;
#41839 = CARTESIAN_POINT ( 'NONE',  ( -10.81189881249999729, 6.242252689847871849, -50.21875000204837391 ) ) ;
#41840 = ORIENTED_EDGE ( 'NONE', *, *, #12921, .T. ) ;
#41841 = CARTESIAN_POINT ( 'NONE',  ( -2.121150477449813534E-15, -11.54700538379251284, -18.87499999999997513 ) ) ;
#41842 = CARTESIAN_POINT ( 'NONE',  ( -10.81189881249999729, -6.242252689847864744, -24.65625000204838457 ) ) ;
#41843 = CARTESIAN_POINT ( 'NONE',  ( -2.121150477449813534E-15, -11.54700538379251284, -150.8750000000000284 ) ) ;
#41844 = CARTESIAN_POINT ( 'NONE',  ( -4.999999999999996447, 8.660254037844387298, -22.87500000409675849 ) ) ;
#41845 = DIRECTION ( 'NONE',  ( -0.000000000000000000, -0.000000000000000000, -1.000000000000000000 ) ) ;
#41847 = ORIENTED_EDGE ( 'NONE', *, *, #35860, .F. ) ;
#41846 = CARTESIAN_POINT ( 'NONE',  ( 10.81189881249999907, 6.242252689847868297, -128.9062500020483810 ) ) ;
#41848 = CARTESIAN_POINT ( 'NONE',  ( -5.000020801129981152, 8.660290040615111096, 0.000000000000000000 ) ) ;
#41849 =( BOUNDED_CURVE ( )  B_SPLINE_CURVE ( 2, ( #28659, #5772, #15667, #28868, #42002, #12430, #38783 ),
 .UNSPECIFIED., .F., .F. ) 
 B_SPLINE_CURVE_WITH_KNOTS ( ( 3, 2, 2, 3 ),
 ( 0.7537313432835822669, 0.7549751243781096521, 0.7562189054726369264, 0.7574626865671643117 ),
 .UNSPECIFIED. ) 
 CURVE ( )  GEOMETRIC_REPRESENTATION_ITEM ( )  RATIONAL_B_SPLINE_CURVE ( ( 0.9999999999999761302, 0.8660254037844625774, 1.000000000000000000, 0.8660254037844387076, 1.000000000000000000, 0.8660254037844267172, 1.000000000000011990 ) ) 
 REPRESENTATION_ITEM ( '' )  );
#41850 = ORIENTED_EDGE ( 'NONE', *, *, #40713, .T. ) ;
#41851 = CARTESIAN_POINT ( 'NONE',  ( -10.81189881249999729, 1.324075727343319199E-15, -57.78125000204836681 ) ) ;
#41852 = PERSON_AND_ORGANIZATION ( #11915, #17965 ) ;
#41853 = ADVANCED_FACE ( 'NONE', ( #17212 ), #13966, .T. ) ;
#41854 = CARTESIAN_POINT ( 'NONE',  ( 10.81189881249999729, 0.000000000000000000, -101.8437500020483810 ) ) ;
#41856 = ORIENTED_EDGE ( 'NONE', *, *, #1558, .F. ) ;
#41855 = VERTEX_POINT ( 'NONE', #33649 ) ;
#41857 = CARTESIAN_POINT ( 'NONE',  ( -4.999999999999996447, 8.660254037844387298, -175.5000000000000284 ) ) ;
#41858 = CARTESIAN_POINT ( 'NONE',  ( 10.00000000000000000, 5.773502691896255534, -171.3750000000000000 ) ) ;
#41859 = CARTESIAN_POINT ( 'NONE',  ( -10.81189881249999907, -6.242252689847864744, -160.9687500020484094 ) ) ;
#41860 = CARTESIAN_POINT ( 'NONE',  ( -10.81189881249999729, 1.324075727343319199E-15, -191.2812500020484094 ) ) ;
#41861 = CARTESIAN_POINT ( 'NONE',  ( 5.405949406249992428, -9.363379034771808662, -4.593750002048368586 ) ) ;
#41862 = CARTESIAN_POINT ( 'NONE',  ( 10.81189881249999551, -6.242252689847874514, -143.9687500020484094 ) ) ;
#41863 = CARTESIAN_POINT ( 'NONE',  ( 5.405949406249992428, -9.363379034771808662, -106.5937500020483810 ) ) ;
#41864 = CYLINDRICAL_SURFACE ( 'NONE', #30454, 9.999999999999998224 ) ;
#41865 = CARTESIAN_POINT ( 'NONE',  ( 7.644554776091147741E-16, 12.48450537969573659, -119.6562500020484094 ) ) ;
#41866 = CARTESIAN_POINT ( 'NONE',  ( -9.999999999999998224, 1.224646799147353059E-15, -193.6250000040967905 ) ) ;
#41868 = EDGE_CURVE ( 'NONE', #33849, #28241, #5229, .T. ) ;
#41867 = CARTESIAN_POINT ( 'NONE',  ( 10.81189881249999729, 6.242252689847867408, -125.7187500020483810 ) ) ;
#41869 = CARTESIAN_POINT ( 'NONE',  ( -10.81189881249999729, 6.242252689847871849, -197.4062500020484094 ) ) ;
#41870 = CARTESIAN_POINT ( 'NONE',  ( -4.999999999999996447, 8.660254037844387298, -11.99999999999995559 ) ) ;
#41871 = CARTESIAN_POINT ( 'NONE',  ( 10.00000000000000000, 5.773502691896255534, -138.3750000000000000 ) ) ;
#41872 = CARTESIAN_POINT ( 'NONE',  ( 9.999999999999996447, -5.773502691896262640, -12.62499999999996980 ) ) ;
#41873 = CARTESIAN_POINT ( 'NONE',  ( -2.293366432827344421E-15, -12.48450537969573659, -66.21875000204836681 ) ) ;
#41874 = CARTESIAN_POINT ( 'NONE',  ( 10.81189881249999551, -6.242252689847874514, -53.96875000204838102 ) ) ;
#41875 = CARTESIAN_POINT ( 'NONE',  ( -5.000000000000003553, -8.660254037844383745, -187.3750000040967905 ) ) ;
#41876 = CARTESIAN_POINT ( 'NONE',  ( -5.405949406249996869, 9.363379034771805109, -25.03125000204836681 ) ) ;
#41877 = AXIS2_PLACEMENT_3D ( 'NONE', #33082, #29848, #6958 ) ;
#41878 = CARTESIAN_POINT ( 'NONE',  ( -10.81189881249999907, -6.242252689847864744, -39.46875000204835970 ) ) ;
#41879 = CARTESIAN_POINT ( 'NONE',  ( -2.121150477449813534E-15, -11.54700538379251284, -107.7500000040967763 ) ) ;
#41880 = CARTESIAN_POINT ( 'NONE',  ( 10.81189881249999729, 0.000000000000000000, -146.8437500020483810 ) ) ;
#41881 = CARTESIAN_POINT ( 'NONE',  ( 7.070501591499377789E-16, 11.54700538379251284, -114.1249999999999858 ) ) ;
#41882 = AXIS2_PLACEMENT_3D ( 'NONE', #16205, #3290, #23138 ) ;
#41883 = CARTESIAN_POINT ( 'NONE',  ( -9.999999999999479527, -5.773502691896549521, -102.0000000040967620 ) ) ;
#41884 = CARTESIAN_POINT ( 'NONE',  ( -4.999999999999996447, 8.660254037844387298, -77.99999999999998579 ) ) ;
#41885 = CARTESIAN_POINT ( 'NONE',  ( -5.405949406249996869, 9.363379034771805109, -140.5312500020484094 ) ) ;
#41886 = CARTESIAN_POINT ( 'NONE',  ( 10.81189881249999729, 6.242252689847867408, -8.906250002048373915 ) ) ;
#41887 =( BOUNDED_CURVE ( )  B_SPLINE_CURVE ( 2, ( #28510, #5831, #39259, #38629, #15939, #31961, #9692 ),
 .UNSPECIFIED., .F., .F. ) 
 B_SPLINE_CURVE_WITH_KNOTS ( ( 3, 2, 2, 3 ),
 ( 0.6641791044776121922, 0.6654228855721395774, 0.6666666666666668517, 0.6679104477611942370 ),
 .UNSPECIFIED. ) 
 CURVE ( )  GEOMETRIC_REPRESENTATION_ITEM ( )  RATIONAL_B_SPLINE_CURVE ( ( 0.9999999999999761302, 0.8660254037844625774, 1.000000000000000000, 0.8660254037844387076, 1.000000000000000000, 0.8660254037844148378, 1.000000000000023981 ) ) 
 REPRESENTATION_ITEM ( '' )  );
#41888 = VERTEX_POINT ( 'NONE', #19610 ) ;
#41889 = CARTESIAN_POINT ( 'NONE',  ( -42.00000000000004974, 5.327213576290989989E-15, -219.9999999999999716 ) ) ;
#41890 = CARTESIAN_POINT ( 'NONE',  ( -5.000000000000003553, -8.660254037844383745, -112.3750000040967763 ) ) ;
#41891 = DIRECTION ( 'NONE',  ( -1.000000000000000000, 0.000000000000000000, 0.000000000000000000 ) ) ;
#41892 = CARTESIAN_POINT ( 'NONE',  ( 10.81189881249999729, 0.000000000000000000, -74.84375000204838102 ) ) ;
#41893 = CARTESIAN_POINT ( 'NONE',  ( 9.999999999999996447, -5.773502691896262640, -39.62499999999995737 ) ) ;
#41894 = CARTESIAN_POINT ( 'NONE',  ( 4.999999999999992006, -8.660254037844389075, -28.12500000409676204 ) ) ;
#41895 = CARTESIAN_POINT ( 'NONE',  ( -5.405949406249996869, 9.363379034771805109, -53.53125000204836681 ) ) ;
#41896 = CARTESIAN_POINT ( 'NONE',  ( -9.999999999999227285, -5.773502691896698735, -132.0000000040967620 ) ) ;
#41897 = CARTESIAN_POINT ( 'NONE',  ( -10.81189881249999729, 6.242252689847871849, -33.90625000204835970 ) ) ;
#41898 =( BOUNDED_CURVE ( )  B_SPLINE_CURVE ( 2, ( #27613, #40753, #24173, #24393, #39911, #23530, #20910, #26964, #33885, #17024, #13781, #30223, #662, #12258, #31293, #18098, #21339, #28261, #21987, #31506, #28694, #9038, #25034, #34743, #41174, #34955, #8411, #2150, #34527, #22203, #38176, #5164, #11613, #38598, #1936, #4951, #18316, #28482, #41821, #15062, #1724, #15285, #8620, #14851, #41614, #41399, #21776, #24821, #11833, #31935, #28048, #37966, #25453, #15489, #37748, #5379, #21562, #35164, #18530, #31720, #8192, #35378, #2362, #12048, #25244, #38389, #8830, #5590, #18743, #5803, #18956, #1507, #14641, #27830, #40962, #11405, #24599, #15702, #9669, #12672, #16328, #16117, #2781, #36422, #19794, #22842, #32766, #19377, #9878, #6440, #6857, #35800, #25868, #32143, #6017, #39443, #15909, #2992, #29527, #42669, #29314, #32357, #10086, #39647, #29111, #9459, #23263, #42458, #13093, #2573, #28901, #42247, #42036, #13311, #22626, #6231, #39023, #12465, #32981, #25659, #32565, #38814, #23051, #9241, #3202, #26294, #12886, #19167, #26080, #22411, #6644, #35589, #19583, #36208, #36004, #39231, #3410, #16546, #29744, #190, #26500, #33201, #20224, #1243, #16760, #30805, #7075, #36628, #39860, #3632, #33832, #10716, #34046, #40484, #20862, #4257, #10930, #7713, #37484, #7493, #33414, #14368, #17399, #26708, #40074, #20009, #611, #4468, #7283, #29960, #23910, #26916, #20646, #10294, #27565, #818, #10505, #16975, #40699, #20436, #23480, #37055, #30597, #13522, #3841, #27348, #400, #30173, #1027, #40276, #24124, #13727, #27133, #14149, #23692, #4043, #36839, #33621, #37264, #17187, #17610, #30385, #11143, #13940, #24342, #14589, #8570, #4900, #17829, #27779, #41566, #38127, #12000, #25195, #18047, #1671, #38336, #40914, #15443, #2102, #31243, #31886, #34265, #28213, #14799, #34903, #41773, #18690, #8778, #28430, #11356, #24551, #24772, #37916, #21935, #41346, #5325, #27995, #8143, #18480, #37701, #34478, #21512, #31668, #15232, #34693, #12206, #31025, #8360, #21291, #21720, #11565, #5539, #2316, #5113, #41125, #35115, #28642, #18262, #25399, #31451, #1885, #7927, #21077, #4681, #15014, #11783, #1455, #24984, #19120, #41986, #19746, #13257, #5968, #9821, #12623, #12415, #2941, #6179, #16493, #26029, #22788, #36157, #9408, #38766, #6590, #9615, #32512, #9193, #39181, #38972, #16070, #35539, #22571, #26239, #22363, #15650, #23003, #32927, #32091, #35751, #29691, #19318, #5756, #135, #35949, #38545, #39388, #6391, #42196, #29263, #28850, #25608, #42407, #3360, #32305, #12838, #8986, #2727, #32716, #19532, #15859, #3149, #25817, #16277, #22154, #29475, #29058, #35329, #18909, #42617, #13045, #2525, #4203, #766, #1190, #30120, #7023, #26444, #344, #33780, #40024, #23855, #10662, #10454, #17557, #36369, #557, #33146, #27085, #13678, #24068, #37210, #26869, #13465, #17346, #13892, #10240, #30550, #3575, #7439, #4417, #27297, #30757, #33364, #29905, #6805, #26658, #20175, #39808, #7657, #39596, #36576, #10030, #40228, #17135, #40432, #977, #10876, #37004, #14095, #3785, #30337, #16919, #33996, #20810, #20592, #16708, #23645, #23211, #36791, #19960, #7228, #23428, #20379, #33568, #3992, #34215, #21887, #17777, #38287, #1403, #14533, #37435, #31617, #27512, #31402, #14963, #34638, #21025, #18428, #37650, #5064, #4846, #35066, #8733, #11734, #4631, #34426, #31837, #8090, #30973, #27727, #41071, #34853, #1620, #41519, #5493, #28377, #31190, #40863, #21454, #24718, #18643, #1837, #18212, #28161, #7878, #11304, #21670, #11088, #8309, #24498, #41295, #14749, #24933, #21241, #27944, #2050, #17990, #11516, #11949, #25140, #37864, #38077, #8517, #5275, #15181, #14312, #40646, #24291, #3103, #29219, #5921, #9359, #22107, #18866, #22528, #29431, #5714, #35701, #32674, #32046, #39135, #42150, #26191, #28592, #6130, #25567, #42358, #36113, #15604, #6546, #16231, #19273, #2893, #32253, #22741, #32469, #19700, #19072, #38719, #2274, #2475, #9567, #28806, #15814, #12791, #25983, #29010, #15395, #22958, #9778, #41938, #22320, #41723, #12581, #35907, #12161, #25353, #12369, #38500, #39339, #35495, #2680, #9153, #8943, #42572, #35281, #25774, #38927, #6344, #16023, #19487, #12995, #16659, #9983, #17303, #4158, #26402, #30076, #29860, #10616, #23162, #26824, #39552, #33528, #298, #86, #36325, #23804, #6756, #19910, #10408, #30507, #33097, #39977, #20548, #3523, #27042, #517, #14051, #16444, #23600, #13419, #17089, #24024, #934, #36958, #7400, #26614, #3951, #20128, #33737, #7182, #7611, #36532, #39763, #32883, #10197, #40186, #23383, #3741, #30288, #727, #16871, #37164, #13208, #6973, #33316, #13846, #40387, #13632, #27246, #3314, #29642, #36745, #20336, #10830, #40820, #11260, #20982, #41468, #21631, #11903, #27682, #24240, #1142, #37391, #1357, #7834, #21194, #34168, #4588, #14266, #38034, #33954, #37819, #21407, #41029, #27468, #24885, #14487, #11472, #24457, #28330, #2006, #18165, #40603, #37604, #38244, #17727, #30922, #11046, #4797, #41247, #8047, #5232, #15133, #34809, #34381, #17946, #27896, #31144, #25098, #8262, #24673, #34593, #1577, #14706, #28119, #20765, #1790 ),
 .UNSPECIFIED., .F., .F. ) 
 B_SPLINE_CURVE_WITH_KNOTS ( ( 3, 2, 2, 2, 2, 2, 2, 2, 2, 2, 2, 2, 2, 2, 2, 2, 2, 2, 2, 2, 2, 2, 2, 2, 2, 2, 2, 2, 2, 2, 2, 2, 2, 2, 2, 2, 2, 2, 2, 2, 2, 2, 2, 2, 2, 2, 2, 2, 2, 2, 2, 2, 2, 2, 2, 2, 2, 2, 2, 2, 2, 2, 2, 2, 2, 2, 2, 2, 2, 2, 2, 2, 2, 2, 2, 2, 2, 2, 2, 2, 2, 2, 2, 2, 2, 2, 2, 2, 2, 2, 2, 2, 2, 2, 2, 2, 2, 2, 2, 2, 2, 2, 2, 2, 2, 2, 2, 2, 2, 2, 2, 2, 2, 2, 2, 2, 2, 2, 2, 2, 2, 2, 2, 2, 2, 2, 2, 2, 2, 2, 2, 2, 2, 2, 2, 2, 2, 2, 2, 2, 2, 2, 2, 2, 2, 2, 2, 2, 2, 2, 2, 2, 2, 2, 2, 2, 2, 2, 2, 2, 2, 2, 2, 2, 2, 2, 2, 2, 2, 2, 2, 2, 2, 2, 2, 2, 2, 2, 2, 2, 2, 2, 2, 2, 2, 2, 2, 2, 2, 2, 2, 2, 2, 2, 2, 2, 2, 2, 2, 2, 2, 2, 2, 2, 2, 2, 2, 2, 2, 2, 2, 2, 2, 2, 2, 2, 2, 2, 2, 2, 2, 2, 2, 2, 2, 2, 2, 2, 2, 2, 2, 2, 2, 2, 2, 2, 2, 2, 2, 2, 2, 2, 2, 2, 2, 2, 2, 2, 2, 2, 2, 2, 2, 2, 2, 2, 2, 2, 2, 2, 2, 2, 2, 2, 2, 2, 2, 2, 2, 2, 2, 2, 2, 2, 2, 2, 2, 2, 2, 2, 2, 2, 2, 2, 2, 2, 2, 2, 2, 2, 2, 2, 2, 2, 2, 2, 2, 2, 2, 2, 2, 2, 2, 2, 2, 2, 2, 2, 2, 2, 2, 2, 2, 2, 2, 2, 2, 2, 2, 2, 2, 3 ),
 ( 0.09718516234321271374, 0.09825870646766168837, 0.09950248756218905977, 0.1007462686567164173, 0.1019900497512437748, 0.1032338308457711462, 0.1044776119402985037, 0.1057213930348258751, 0.1069651741293532327, 0.1082089552238805902, 0.1094527363184079616, 0.1106965174129353191, 0.1119402985074626905, 0.1131840796019900480, 0.1144278606965174194, 0.1156716417910447769, 0.1169154228855721345, 0.1181592039800995059, 0.1194029850746268634, 0.1206467661691542348, 0.1218905472636815923, 0.1231343283582089498, 0.1243781094527363212, 0.1256218905472636926, 0.1268656716417910502, 0.1281094527363184077, 0.1293532338308457652, 0.1305970149253731227, 0.1318407960199005080, 0.1330845771144278655, 0.1343283582089552231, 0.1355721393034825806, 0.1368159203980099381, 0.1380597014925373234, 0.1393034825870646809, 0.1405472636815920384, 0.1417910447761193959, 0.1430348258706467535, 0.1442786069651741387, 0.1455223880597014963, 0.1467661691542288538, 0.1480099502487562113, 0.1492537313432835688, 0.1504975124378109541, 0.1517412935323383116, 0.1529850746268656692, 0.1542288557213930267, 0.1554726368159203842, 0.1567164179104477695, 0.1579601990049751270, 0.1592039800995024845, 0.1604477611940298420, 0.1616915422885572273, 0.1629353233830845848, 0.1641791044776119424, 0.1654228855721392999, 0.1666666666666666574, 0.1679104477611940427, 0.1691542288557214002, 0.1703980099502487577, 0.1716417910447761153, 0.1728855721393034728, 0.1741293532338308581, 0.1753731343283582156, 0.1766169154228855731, 0.1778606965174129306, 0.1791044776119402882, 0.1803482587064676734, 0.1815920398009950310, 0.1828358208955223885, 0.1840796019900497460, 0.1853233830845771035, 0.1865671641791044888, 0.1878109452736318463, 0.1890547263681591761, 0.1902985074626865614, 0.1915422885572139189, 0.1927860696517413042, 0.1940298507462686617, 0.1952736318407959915, 0.1965174129353233767, 0.1977611940298507343, 0.1990049751243781195, 0.2002487562189054771, 0.2014925373134328623, 0.2027363184079601921, 0.2039800995024875496, 0.2052238805970149349, 0.2064676616915422924, 0.2077114427860696777, 0.2089552238805970075, 0.2101990049751243650, 0.2114427860696517503, 0.2126865671641791078, 0.2139303482587064931, 0.2151741293532338228, 0.2164179104477611804, 0.2176616915422885656, 0.2189054726368159232, 0.2201492537313432807, 0.2213930348258706382, 0.2226368159203980235, 0.2238805970149254088, 0.2251243781094527385, 0.2263681592039801238, 0.2276119402985074536, 0.2288557213930348389, 0.2300995024875622241, 0.2313432835820895539, 0.2325870646766169392, 0.2338308457711442689, 0.2350746268656716542, 0.2363184079601990395, 0.2375621890547263693, 0.2388059701492537545, 0.2400497512437810843, 0.2412935323383084696, 0.2425373134328358549, 0.2437810945273631846, 0.2450248756218905699, 0.2462686567164178997, 0.2475124378109452850, 0.2487562189054726702, 0.2500000000000000000, 0.2512437810945273853, 0.2524875621890547150, 0.2537313432835821003, 0.2549751243781094301, 0.2562189054726368154, 0.2574626865671642006, 0.2587064676616914749, 0.2599502487562189157, 0.2611940298507462455, 0.2624378109452736307, 0.2636815920398010160, 0.2649253731343282903, 0.2661691542288557311, 0.2674129353233830608, 0.2686567164179104461, 0.2699004975124378314, 0.2711442786069651611, 0.2723880597014925464, 0.2736318407960198762, 0.2748756218905472615, 0.2761194029850746468, 0.2773631840796019765, 0.2786069651741293618, 0.2798507462686566361, 0.2810945273631840768, 0.2823383084577114621, 0.2835820895522387919, 0.2848258706467661772, 0.2860696517412934514, 0.2873134328358208922, 0.2885572139303482775, 0.2898009950248756073, 0.2910447761194029925, 0.2922885572139302668, 0.2935323383084577076, 0.2947761194029850929, 0.2960199004975124226, 0.2972636815920398079, 0.2985074626865670822, 0.2997512437810945229, 0.3009950248756219082, 0.3022388059701492380, 0.3034825870646766233, 0.3047263681592038975, 0.3059701492537313383, 0.3072139303482587236, 0.3084577114427860534, 0.3097014925373134386, 0.3109452736318407684, 0.3121890547263681537, 0.3134328358208955390, 0.3146766169154228687, 0.3159203980099502540, 0.3171641791044776393, 0.3184079601990049690, 0.3196517412935323543, 0.3208955223880596841, 0.3221393034825870694, 0.3233830845771144546, 0.3246268656716417844, 0.3258706467661691697, 0.3271144278606964995, 0.3283582089552238847, 0.3296019900497512700, 0.3308457711442785998, 0.3320895522388059851, 0.3333333333333333148, 0.3345771144278607001, 0.3358208955223880854, 0.3370646766169154152, 0.3383084577114428004, 0.3395522388059701302, 0.3407960199004975155, 0.3420398009950249008, 0.3432835820895522305, 0.3445273631840796158, 0.3457711442786069456, 0.3470149253731343308, 0.3482587064676617161, 0.3495024875621890459, 0.3507462686567164312, 0.3519900497512437609, 0.3532338308457711462, 0.3544776119402985315, 0.3557213930348258613, 0.3569651741293532465, 0.3582089552238805763, 0.3594527363184079616, 0.3606965174129353469, 0.3619402985074626766, 0.3631840796019900619, 0.3644278606965173917, 0.3656716417910447769, 0.3669154228855721622, 0.3681592039800994920, 0.3694029850746268773, 0.3706467661691542070, 0.3718905472636815923, 0.3731343283582089776, 0.3743781094527363074, 0.3756218905472636926, 0.3768656716417910224, 0.3781094527363184077, 0.3793532338308457930, 0.3805970149253731227, 0.3818407960199005080, 0.3830845771144278378, 0.3843283582089552231, 0.3855721393034826083, 0.3868159203980099381, 0.3880597014925373234, 0.3893034825870646531, 0.3905472636815920384, 0.3917910447761194237, 0.3930348258706467535, 0.3942786069651741387, 0.3955223880597014685, 0.3967661691542288538, 0.3980099502487562391, 0.3992537313432835688, 0.4004975124378109541, 0.4017412935323382839, 0.4029850746268656692, 0.4042288557213930544, 0.4054726368159203842, 0.4067164179104477695, 0.4079601990049750992, 0.4092039800995024845, 0.4104477611940298698, 0.4116915422885571996, 0.4129353233830845848, 0.4141791044776118591, 0.4154228855721392999, 0.4166666666666666852, 0.4179104477611940704, 0.4191542288557214002, 0.4203980099502487300, 0.4216417910447761708, 0.4228855721393035005, 0.4241293532338308303, 0.4253731343283582156, 0.4266169154228854898, 0.4278606965174129306, 0.4291044776119403159, 0.4303482587064677012, 0.4315920398009950310, 0.4328358208955223607, 0.4340796019900497460, 0.4353233830845771313, 0.4365671641791044610, 0.4378109452736318463, 0.4390547263681592316, 0.4402985074626865614, 0.4415422885572139466, 0.4427860696517413319, 0.4440298507462686617, 0.4452736318407960470, 0.4465174129353233767, 0.4477611940298507620, 0.4490049751243780918, 0.4502487562189054771, 0.4514925373134328623, 0.4527363184079601921, 0.4539800995024875774, 0.4552238805970149627, 0.4564676616915422924, 0.4577114427860696777, 0.4589552238805970075, 0.4601990049751243927, 0.4614427860696517225, 0.4626865671641791078, 0.4639303482587064931, 0.4651741293532338228, 0.4664179104477612081, 0.4676616915422885379, 0.4689054726368159232, 0.4701492537313433084, 0.4713930348258706382, 0.4726368159203980235, 0.4738805970149253532, 0.4751243781094527385, 0.4763681592039801238, 0.4776119402985074536, 0.4788557213930348389, 0.4800995024875621686, 0.4813432835820895539, 0.4825870646766169392, 0.4838308457711442689, 0.4850746268656716542, 0.4863184079601989840, 0.4875621890547263693, 0.4888059701492537545, 0.4900497512437810843, 0.4912935323383084696, 0.4925373134328357994, 0.4937810945273631846, 0.4950248756218905699, 0.4951951125919689112 ),
 .UNSPECIFIED. ) 
 CURVE ( )  GEOMETRIC_REPRESENTATION_ITEM ( )  RATIONAL_B_SPLINE_CURVE ( ( 0.9683452906431517793, 0.8843625769635171663, 1.000000000000000000, 0.8660254037844387076, 1.000000000000000000, 0.8660254037844387076, 1.000000000000000000, 0.8660254037844387076, 1.000000000000000000, 0.8660254037844387076, 1.000000000000000000, 0.8660254037844387076, 1.000000000000000000, 0.8660254037844387076, 1.000000000000000000, 0.8660254037844387076, 1.000000000000000000, 0.8660254037844387076, 1.000000000000000000, 0.8660254037844387076, 1.000000000000000000, 0.8660254037844387076, 1.000000000000000000, 0.8660254037844387076, 1.000000000000000000, 0.8660254037844387076, 1.000000000000000000, 0.8660254037844387076, 1.000000000000000000, 0.8660254037844387076, 1.000000000000000000, 0.8660254037844387076, 1.000000000000000000, 0.8660254037844387076, 1.000000000000000000, 0.8660254037844387076, 1.000000000000000000, 0.8660254037844387076, 1.000000000000000000, 0.8660254037844387076, 1.000000000000000000, 0.8660254037844387076, 1.000000000000000000, 0.8660254037844387076, 1.000000000000000000, 0.8660254037844387076, 1.000000000000000000, 0.8660254037844387076, 1.000000000000000000, 0.8660254037844387076, 1.000000000000000000, 0.8660254037844387076, 1.000000000000000000, 0.8660254037844387076, 1.000000000000000000, 0.8660254037844387076, 1.000000000000000000, 0.8660254037844387076, 1.000000000000000000, 0.8660254037844387076, 1.000000000000000000, 0.8660254037844387076, 1.000000000000000000, 0.8660254037844387076, 1.000000000000000000, 0.8660254037844387076, 1.000000000000000000, 0.8660254037844387076, 1.000000000000000000, 0.8660254037844387076, 1.000000000000000000, 0.8660254037844387076, 1.000000000000000000, 0.8660254037844387076, 1.000000000000000000, 0.8660254037844387076, 1.000000000000000000, 0.8660254037844387076, 1.000000000000000000, 0.8660254037844387076, 1.000000000000000000, 0.8660254037844387076, 1.000000000000000000, 0.8660254037844387076, 1.000000000000000000, 0.8660254037844387076, 1.000000000000000000, 0.8660254037844387076, 1.000000000000000000, 0.8660254037844387076, 1.000000000000000000, 0.8660254037844387076, 1.000000000000000000, 0.8660254037844387076, 1.000000000000000000, 0.8660254037844387076, 1.000000000000000000, 0.8660254037844387076, 1.000000000000000000, 0.8660254037844387076, 1.000000000000000000, 0.8660254037844387076, 1.000000000000000000, 0.8660254037844387076, 1.000000000000000000, 0.8660254037844387076, 1.000000000000000000, 0.8660254037844387076, 1.000000000000000000, 0.8660254037844387076, 1.000000000000000000, 0.8660254037844387076, 1.000000000000000000, 0.8660254037844387076, 1.000000000000000000, 0.8660254037844387076, 1.000000000000000000, 0.8660254037844387076, 1.000000000000000000, 0.8660254037844387076, 1.000000000000000000, 0.8660254037844387076, 1.000000000000000000, 0.8660254037844387076, 1.000000000000000000, 0.8660254037844387076, 1.000000000000000000, 0.8660254037844387076, 1.000000000000000000, 0.8660254037844387076, 1.000000000000000000, 0.8660254037844387076, 1.000000000000000000, 0.8660254037844387076, 1.000000000000000000, 0.8660254037844387076, 1.000000000000000000, 0.8660254037844387076, 1.000000000000000000, 0.8660254037844387076, 1.000000000000000000, 0.8660254037844387076, 1.000000000000000000, 0.8660254037844387076, 1.000000000000000000, 0.8660254037844387076, 1.000000000000000000, 0.8660254037844387076, 1.000000000000000000, 0.8660254037844387076, 1.000000000000000000, 0.8660254037844387076, 1.000000000000000000, 0.8660254037844387076, 1.000000000000000000, 0.8660254037844387076, 1.000000000000000000, 0.8660254037844387076, 1.000000000000000000, 0.8660254037844387076, 1.000000000000000000, 0.8660254037844387076, 1.000000000000000000, 0.8660254037844387076, 1.000000000000000000, 0.8660254037844387076, 1.000000000000000000, 0.8660254037844387076, 1.000000000000000000, 0.8660254037844387076, 1.000000000000000000, 0.8660254037844387076, 1.000000000000000000, 0.8660254037844387076, 1.000000000000000000, 0.8660254037844387076, 1.000000000000000000, 0.8660254037844387076, 1.000000000000000000, 0.8660254037844387076, 1.000000000000000000, 0.8660254037844387076, 1.000000000000000000, 0.8660254037844387076, 1.000000000000000000, 0.8660254037844387076, 1.000000000000000000, 0.8660254037844387076, 1.000000000000000000, 0.8660254037844387076, 1.000000000000000000, 0.8660254037844387076, 1.000000000000000000, 0.8660254037844387076, 1.000000000000000000, 0.8660254037844387076, 1.000000000000000000, 0.8660254037844387076, 1.000000000000000000, 0.8660254037844387076, 1.000000000000000000, 0.8660254037844387076, 1.000000000000000000, 0.8660254037844387076, 1.000000000000000000, 0.8660254037844387076, 1.000000000000000000, 0.8660254037844387076, 1.000000000000000000, 0.8660254037844387076, 1.000000000000000000, 0.8660254037844387076, 1.000000000000000000, 0.8660254037844387076, 1.000000000000000000, 0.8660254037844387076, 1.000000000000000000, 0.8660254037844387076, 1.000000000000000000, 0.8660254037844387076, 1.000000000000000000, 0.8660254037844387076, 1.000000000000000000, 0.8660254037844387076, 1.000000000000000000, 0.8660254037844387076, 1.000000000000000000, 0.8660254037844387076, 1.000000000000000000, 0.8660254037844387076, 1.000000000000000000, 0.8660254037844387076, 1.000000000000000000, 0.8660254037844387076, 1.000000000000000000, 0.8660254037844387076, 1.000000000000000000, 0.8660254037844387076, 1.000000000000000000, 0.8660254037844387076, 1.000000000000000000, 0.8660254037844387076, 1.000000000000000000, 0.8660254037844387076, 1.000000000000000000, 0.8660254037844387076, 1.000000000000000000, 0.8660254037844387076, 1.000000000000000000, 0.8660254037844387076, 1.000000000000000000, 0.8660254037844387076, 1.000000000000000000, 0.8660254037844387076, 1.000000000000000000, 0.8660254037844387076, 1.000000000000000000, 0.8660254037844387076, 1.000000000000000000, 0.8660254037844387076, 1.000000000000000000, 0.8660254037844387076, 1.000000000000000000, 0.8660254037844387076, 1.000000000000000000, 0.8660254037844387076, 1.000000000000000000, 0.8660254037844387076, 1.000000000000000000, 0.8660254037844387076, 1.000000000000000000, 0.8660254037844387076, 1.000000000000000000, 0.8660254037844387076, 1.000000000000000000, 0.8660254037844387076, 1.000000000000000000, 0.8660254037844387076, 1.000000000000000000, 0.8660254037844387076, 1.000000000000000000, 0.8660254037844387076, 1.000000000000000000, 0.8660254037844387076, 1.000000000000000000, 0.8660254037844387076, 1.000000000000000000, 0.8660254037844387076, 1.000000000000000000, 0.8660254037844387076, 1.000000000000000000, 0.8660254037844387076, 1.000000000000000000, 0.8660254037844387076, 1.000000000000000000, 0.8660254037844387076, 1.000000000000000000, 0.8660254037844387076, 1.000000000000000000, 0.8660254037844387076, 1.000000000000000000, 0.8660254037844387076, 1.000000000000000000, 0.8660254037844387076, 1.000000000000000000, 0.8660254037844387076, 1.000000000000000000, 0.8660254037844387076, 1.000000000000000000, 0.8660254037844387076, 1.000000000000000000, 0.8660254037844387076, 1.000000000000000000, 0.8660254037844387076, 1.000000000000000000, 0.8660254037844387076, 1.000000000000000000, 0.8660254037844387076, 1.000000000000000000, 0.8660254037844387076, 1.000000000000000000, 0.8660254037844387076, 1.000000000000000000, 0.8660254037844387076, 1.000000000000000000, 0.8660254037844387076, 1.000000000000000000, 0.8660254037844387076, 1.000000000000000000, 0.8660254037844387076, 1.000000000000000000, 0.8660254037844387076, 1.000000000000000000, 0.8660254037844387076, 1.000000000000000000, 0.8660254037844387076, 1.000000000000000000, 0.8660254037844387076, 1.000000000000000000, 0.8660254037844387076, 1.000000000000000000, 0.8660254037844387076, 1.000000000000000000, 0.8660254037844387076, 1.000000000000000000, 0.8660254037844387076, 1.000000000000000000, 0.8660254037844387076, 1.000000000000000000, 0.8660254037844387076, 1.000000000000000000, 0.8660254037844387076, 1.000000000000000000, 0.8660254037844387076, 1.000000000000000000, 0.8660254037844387076, 1.000000000000000000, 0.8660254037844387076, 1.000000000000000000, 0.8660254037844387076, 1.000000000000000000, 0.8660254037844387076, 1.000000000000000000, 0.8660254037844387076, 1.000000000000000000, 0.8660254037844387076, 1.000000000000000000, 0.8660254037844387076, 1.000000000000000000, 0.8660254037844387076, 1.000000000000000000, 0.8660254037844387076, 1.000000000000000000, 0.8660254037844387076, 1.000000000000000000, 0.8660254037844387076, 1.000000000000000000, 0.8660254037844387076, 1.000000000000000000, 0.8660254037844387076, 1.000000000000000000, 0.8660254037844387076, 1.000000000000000000, 0.8660254037844387076, 1.000000000000000000, 0.8660254037844387076, 1.000000000000000000, 0.8660254037844387076, 1.000000000000000000, 0.8660254037844387076, 1.000000000000000000, 0.8660254037844387076, 1.000000000000000000, 0.8660254037844387076, 1.000000000000000000, 0.8660254037844387076, 1.000000000000000000, 0.8660254037844387076, 1.000000000000000000, 0.8660254037844387076, 1.000000000000000000, 0.8660254037844387076, 1.000000000000000000, 0.8660254037844387076, 1.000000000000000000, 0.8660254037844387076, 1.000000000000000000, 0.8660254037844387076, 1.000000000000000000, 0.8660254037844387076, 1.000000000000000000, 0.8660254037844387076, 1.000000000000000000, 0.8660254037844387076, 1.000000000000000000, 0.8660254037844387076, 1.000000000000000000, 0.8660254037844387076, 1.000000000000000000, 0.8660254037844387076, 1.000000000000000000, 0.8660254037844387076, 1.000000000000000000, 0.8660254037844387076, 1.000000000000000000, 0.8660254037844387076, 1.000000000000000000, 0.8660254037844387076, 1.000000000000000000, 0.8660254037844387076, 1.000000000000000000, 0.8660254037844387076, 1.000000000000000000, 0.8660254037844387076, 1.000000000000000000, 0.8660254037844387076, 1.000000000000000000, 0.8660254037844387076, 1.000000000000000000, 0.8660254037844387076, 1.000000000000000000, 0.8660254037844387076, 1.000000000000000000, 0.8660254037844387076, 1.000000000000000000, 0.8660254037844387076, 1.000000000000000000, 0.8660254037844387076, 1.000000000000000000, 0.8660254037844387076, 1.000000000000000000, 0.8660254037844387076, 1.000000000000000000, 0.8660254037844387076, 1.000000000000000000, 0.8660254037844387076, 1.000000000000000000, 0.8660254037844387076, 1.000000000000000000, 0.8660254037844387076, 1.000000000000000000, 0.8660254037844387076, 1.000000000000000000, 0.8660254037844387076, 1.000000000000000000, 0.8660254037844387076, 1.000000000000000000, 0.8660254037844387076, 1.000000000000000000, 0.8660254037844387076, 1.000000000000000000, 0.8660254037844387076, 1.000000000000000000, 0.8660254037844387076, 1.000000000000000000, 0.8660254037844387076, 1.000000000000000000, 0.8660254037844387076, 1.000000000000000000, 0.8660254037844387076, 1.000000000000000000, 0.8660254037844387076, 1.000000000000000000, 0.8660254037844387076, 1.000000000000000000, 0.8660254037844387076, 1.000000000000000000, 0.8660254037844387076, 1.000000000000000000, 0.8660254037844387076, 1.000000000000000000, 0.8660254037844387076, 1.000000000000000000, 0.8660254037844387076, 1.000000000000000000, 0.8660254037844387076, 1.000000000000000000, 0.8660254037844387076, 1.000000000000000000, 0.8660254037844387076, 1.000000000000000000, 0.8660254037844387076, 1.000000000000000000, 0.8660254037844387076, 1.000000000000000000, 0.8660254037844387076, 1.000000000000000000, 0.8660254037844387076, 1.000000000000000000, 0.8660254037844387076, 1.000000000000000000, 0.8660254037844387076, 1.000000000000000000, 0.8660254037844387076, 1.000000000000000000, 0.8660254037844387076, 1.000000000000000000, 0.8660254037844387076, 1.000000000000000000, 0.8660254037844387076, 1.000000000000000000, 0.8660254037844387076, 1.000000000000000000, 0.8660254037844387076, 1.000000000000000000, 0.8660254037844387076, 1.000000000000000000, 0.8660254037844387076, 1.000000000000000000, 0.8660254037844387076, 1.000000000000000000, 0.8660254037844387076, 1.000000000000000000, 0.8660254037844387076, 1.000000000000000000, 0.8660254037844387076, 1.000000000000000000, 0.8660254037844387076, 1.000000000000000000, 0.8660254037844387076, 1.000000000000000000, 0.8660254037844387076, 1.000000000000000000, 0.8660254037844387076, 1.000000000000000000, 0.8660254037844387076, 1.000000000000000000, 0.8660254037844387076, 1.000000000000000000, 0.8660254037844387076, 1.000000000000000000, 0.8660254037844387076, 1.000000000000000000, 0.8660254037844387076, 1.000000000000000000, 0.8660254037844387076, 1.000000000000000000, 0.8660254037844387076, 1.000000000000000000, 0.8660254037844387076, 1.000000000000000000, 0.8660254037844387076, 1.000000000000000000, 0.8660254037844387076, 1.000000000000000000, 0.8660254037844387076, 1.000000000000000000, 0.8660254037844387076, 1.000000000000000000, 0.8660254037844387076, 1.000000000000000000, 0.8660254037844387076, 1.000000000000000000, 0.8660254037844387076, 1.000000000000000000, 0.8660254037844387076, 1.000000000000000000, 0.8660254037844387076, 1.000000000000000000, 0.8660254037844387076, 1.000000000000000000, 0.8660254037844387076, 1.000000000000000000, 0.8660254037844387076, 1.000000000000000000, 0.8660254037844387076, 1.000000000000000000, 0.8660254037844387076, 1.000000000000000000, 0.8660254037844387076, 1.000000000000000000, 0.8660254037844387076, 1.000000000000000000, 0.8660254037844387076, 1.000000000000000000, 0.8660254037844387076, 1.000000000000000000, 0.8660254037844387076, 1.000000000000000000, 0.8660254037844387076, 1.000000000000000000, 0.8660254037844387076, 1.000000000000000000, 0.8660254037844387076, 1.000000000000000000, 0.8660254037844387076, 1.000000000000000000, 0.8660254037844387076, 1.000000000000000000, 0.8660254037844387076, 1.000000000000000000, 0.8660254037844387076, 1.000000000000000000, 0.8660254037844387076, 1.000000000000000000, 0.8660254037844387076, 1.000000000000000000, 0.8660254037844387076, 1.000000000000000000, 0.8660254037844387076, 1.000000000000000000, 0.8660254037844387076, 1.000000000000000000, 0.8660254037844387076, 1.000000000000000000, 0.8660254037844387076, 1.000000000000000000, 0.8660254037844387076, 1.000000000000000000, 0.8660254037844387076, 1.000000000000000000, 0.8660254037844387076, 1.000000000000000000, 0.8660254037844387076, 1.000000000000000000, 0.8660254037844387076, 1.000000000000000000, 0.8660254037844387076, 1.000000000000000000, 0.8660254037844387076, 1.000000000000000000, 0.9816628268209255381, 0.9683452906431576634 ) ) 
 REPRESENTATION_ITEM ( '' )  );
#41899 = CARTESIAN_POINT ( 'NONE',  ( 9.999999999998456346, 5.773502691897149042, -24.37499999999995381 ) ) ;
#41900 = CARTESIAN_POINT ( 'NONE',  ( -10.81189881249999907, -6.242252689847864744, -149.1562500020483810 ) ) ;
#41901 = CARTESIAN_POINT ( 'NONE',  ( 10.81189881249999907, 6.242252689847868297, -149.9062500020484094 ) ) ;
#41902 = FACE_OUTER_BOUND ( 'NONE', #41747, .T. ) ;
#41903 = CARTESIAN_POINT ( 'NONE',  ( -2.121150477449813534E-15, -11.54700538379251284, -57.87499999999998579 ) ) ;
#41904 = EDGE_LOOP ( 'NONE', ( #40303, #21363, #30884, #31684 ) ) ;
#41905 = EDGE_CURVE ( 'NONE', #8575, #8431, #14011, .T. ) ;
#41906 =( BOUNDED_CURVE ( )  B_SPLINE_CURVE ( 2, ( #42490, #9911, #26746, #9701, #25903, #26112, #35833 ),
 .UNSPECIFIED., .F., .F. ) 
 B_SPLINE_CURVE_WITH_KNOTS ( ( 3, 2, 2, 3 ),
 ( 0.6044776119402985870, 0.6057213930348259723, 0.6069651741293533576, 0.6082089552238807428 ),
 .UNSPECIFIED. ) 
 CURVE ( )  GEOMETRIC_REPRESENTATION_ITEM ( )  RATIONAL_B_SPLINE_CURVE ( ( 0.9999999999999880096, 0.8660254037844506980, 1.000000000000000000, 0.8660254037844387076, 1.000000000000000000, 0.8660254037844267172, 1.000000000000011990 ) ) 
 REPRESENTATION_ITEM ( '' )  );
#41907 = VERTEX_POINT ( 'NONE', #23936 ) ;
#41908 = ORIENTED_EDGE ( 'NONE', *, *, #6438, .F. ) ;
#41909 = VECTOR ( 'NONE', #41556, 1000.000000000000000 ) ;
#41910 = CARTESIAN_POINT ( 'NONE',  ( -9.999999999999998224, 1.224646799147353059E-15, -200.0000000000000000 ) ) ;
#41911 = CARTESIAN_POINT ( 'NONE',  ( -2.293366432827344421E-15, -12.48450537969573659, -183.2187500020484094 ) ) ;
#41912 = CARTESIAN_POINT ( 'NONE',  ( 10.81189881249999551, -6.242252689847874514, -32.96875000204834549 ) ) ;
#41913 = CARTESIAN_POINT ( 'NONE',  ( 9.999999999999998224, 0.000000000000000000, -167.0000000000000000 ) ) ;
#41914 = CARTESIAN_POINT ( 'NONE',  ( 5.405949406249992428, -9.363379034771808662, -162.0937500020484094 ) ) ;
#41915 = CARTESIAN_POINT ( 'NONE',  ( -5.405949406249996869, 9.363379034771805109, -152.3437500020483810 ) ) ;
#41916 = DIRECTION ( 'NONE',  ( -1.000000000000000000, 0.000000000000000000, 0.000000000000000000 ) ) ;
#41917 = CARTESIAN_POINT ( 'NONE',  ( -10.81189881249999907, -6.242252689847864744, -136.9687500020483810 ) ) ;
#41918 = CARTESIAN_POINT ( 'NONE',  ( -5.405949406249996869, 9.363379034771805109, -137.5312500020484094 ) ) ;
#41919 = CARTESIAN_POINT ( 'NONE',  ( -10.81189881249999729, 1.324075727343319199E-15, -15.59375000204835082 ) ) ;
#41920 = CARTESIAN_POINT ( 'NONE',  ( 10.81189881249999729, 0.000000000000000000, -143.8437500020483810 ) ) ;
#41921 = LINE ( 'NONE', #18412, #35745 ) ;
#41922 = CARTESIAN_POINT ( 'NONE',  ( -4.999999999999996447, 8.660254037844387298, -177.3750000040967905 ) ) ;
#41923 = CARTESIAN_POINT ( 'NONE',  ( -2.121150477449813534E-15, -11.54700538379251284, -173.3750000000000000 ) ) ;
#41924 = CARTESIAN_POINT ( 'NONE',  ( 10.81189881249999729, 0.000000000000000000, -83.84375000204836681 ) ) ;
#41925 = CARTESIAN_POINT ( 'NONE',  ( -9.999999999999227285, -5.773502691896698735, -115.1249999999999574 ) ) ;
#41926 = CARTESIAN_POINT ( 'NONE',  ( 10.81189881249999907, 6.242252689847868297, -50.90625000204838102 ) ) ;
#41927 = CARTESIAN_POINT ( 'NONE',  ( -5.405949406249996869, 9.363379034771805109, -60.84375000204836681 ) ) ;
#41928 = CARTESIAN_POINT ( 'NONE',  ( -9.727846154639308907, -3.402673899969083759, -99.99999999999998579 ) ) ;
#41929 = ADVANCED_FACE ( 'NONE', ( #13120 ), #32790, .F. ) ;
#41930 = CARTESIAN_POINT ( 'NONE',  ( 7.644554776091147741E-16, 12.48450537969573659, -167.4687500020483810 ) ) ;
#41931 = CARTESIAN_POINT ( 'NONE',  ( -4.999999999999996447, 8.660254037844387298, -141.0000000000000000 ) ) ;
#41932 = CARTESIAN_POINT ( 'NONE',  ( 10.81189881249999551, -6.242252689847874514, -142.6562500020484094 ) ) ;
#41933 = FACE_OUTER_BOUND ( 'NONE', #9527, .T. ) ;
#41934 = CARTESIAN_POINT ( 'NONE',  ( 10.81189881249999729, 0.000000000000000000, -39.03125000204838102 ) ) ;
#41935 = CARTESIAN_POINT ( 'NONE',  ( -9.999999999999998224, 5.773502691896259087, -124.7500000040967763 ) ) ;
#41936 = CARTESIAN_POINT ( 'NONE',  ( -9.999999999999998224, 1.224646799147353059E-15, -100.2499999999999858 ) ) ;
#41937 = ORIENTED_EDGE ( 'NONE', *, *, #15907, .F. ) ;
#41938 = CARTESIAN_POINT ( 'NONE',  ( 10.81189881249999551, -6.242252689847874514, -117.1562500020483952 ) ) ;
#41939 = CARTESIAN_POINT ( 'NONE',  ( 10.00000000000000000, 5.773502691896255534, -137.2500000040967905 ) ) ;
#41940 = CARTESIAN_POINT ( 'NONE',  ( -9.999999999999998224, 1.224646799147353059E-15, -22.62500000409675849 ) ) ;
#41941 = CARTESIAN_POINT ( 'NONE',  ( -2.293366432827344421E-15, -12.48450537969573659, -169.9062500020483810 ) ) ;
#41942 = CARTESIAN_POINT ( 'NONE',  ( 5.000000000000000000, 8.660254037844385522, -47.12500000409677625 ) ) ;
#41943 = AXIS2_PLACEMENT_3D ( 'NONE', #15595, #38490, #28797 ) ;
#41944 = CARTESIAN_POINT ( 'NONE',  ( -9.999999999999998224, 1.224646799147353059E-15, -154.6250000040967905 ) ) ;
#41945 = CARTESIAN_POINT ( 'NONE',  ( -5.405949406249996869, 9.363379034771805109, -64.03125000204836681 ) ) ;
#41946 = CARTESIAN_POINT ( 'NONE',  ( -9.999999999999479527, -5.773502691896549521, -148.5000000040967336 ) ) ;
#41947 = CARTESIAN_POINT ( 'NONE',  ( 7.644554776091147741E-16, 12.48450537969573659, -170.6562500020484094 ) ) ;
#41948 = CARTESIAN_POINT ( 'NONE',  ( 10.00000000000076916, -5.773502691895816774, -106.0000000040967763 ) ) ;
#41949 = CARTESIAN_POINT ( 'NONE',  ( -10.00000000000019185, -5.773502691896140071, -178.1249999999999432 ) ) ;
#41950 = ORIENTED_EDGE ( 'NONE', *, *, #18971, .T. ) ;
#41951 = CARTESIAN_POINT ( 'NONE',  ( 0.000000000000000000, 0.000000000000000000, -200.0000000000000000 ) ) ;
#41952 = CARTESIAN_POINT ( 'NONE',  ( 10.00000000000102318, -5.773502691895667560, -71.12499999999995737 ) ) ;
#41954 = VERTEX_POINT ( 'NONE', #39676 ) ;
#41953 = CARTESIAN_POINT ( 'NONE',  ( 5.405949406249999534, 9.363379034771803333, -80.78125000204838102 ) ) ;
#41955 =( LENGTH_UNIT ( ) NAMED_UNIT ( * ) SI_UNIT ( .MILLI., .METRE. ) );
#41957 = ORIENTED_EDGE ( 'NONE', *, *, #8053, .T. ) ;
#41956 = CARTESIAN_POINT ( 'NONE',  ( -9.999999999999479527, -5.773502691896549521, -140.6250000000000000 ) ) ;
#41958 = ORIENTED_EDGE ( 'NONE', *, *, #19707, .F. ) ;
#41959 = CARTESIAN_POINT ( 'NONE',  ( 7.644554776091147741E-16, 12.48450537969573659, -26.46875000204837747 ) ) ;
#41960 = CARTESIAN_POINT ( 'NONE',  ( -2.121150477449813534E-15, -11.54700538379251284, -53.37499999999997868 ) ) ;
#41961 = CARTESIAN_POINT ( 'NONE',  ( -5.405949406250003975, -9.363379034771801557, -2.031250002048373915 ) ) ;
#41963 = EDGE_LOOP ( 'NONE', ( #6035, #23715, #30308, #23174 ) ) ;
#41962 = CARTESIAN_POINT ( 'NONE',  ( -2.293366432827344421E-15, -12.48450537969573659, -52.71875000204837391 ) ) ;
#41964 = CARTESIAN_POINT ( 'NONE',  ( -9.999999999999998224, 1.224646799147353059E-15, -4.249999999999976019 ) ) ;
#41965 = CARTESIAN_POINT ( 'NONE',  ( 9.999999999999996447, -5.773502691896262640, -29.12499999999998579 ) ) ;
#41966 = CARTESIAN_POINT ( 'NONE',  ( 5.405949406249999534, 9.363379034771803333, -187.0937500020483810 ) ) ;
#41967 = CARTESIAN_POINT ( 'NONE',  ( -5.405949406249996869, 9.363379034771805109, -180.8437500020483810 ) ) ;
#41968 =( BOUNDED_CURVE ( )  B_SPLINE_CURVE ( 2, ( #20749, #1126, #11244, #14249, #11030, #4781, #26810 ),
 .UNSPECIFIED., .F., .F. ) 
 B_SPLINE_CURVE_WITH_KNOTS ( ( 3, 2, 2, 3 ),
 ( 0.01119402985074628015, 0.01243781094527364461, 0.01368159203980100908, 0.01492537313432837180 ),
 .UNSPECIFIED. ) 
 CURVE ( )  GEOMETRIC_REPRESENTATION_ITEM ( )  RATIONAL_B_SPLINE_CURVE ( ( 0.9999999999999986677, 0.8660254037844400399, 1.000000000000000000, 0.8660254037844387076, 1.000000000000000000, 0.8660254037844372643, 1.000000000000001554 ) ) 
 REPRESENTATION_ITEM ( '' )  );
#41969 = CARTESIAN_POINT ( 'NONE',  ( 10.81189881249999551, -6.242252689847874514, -158.9687500020484094 ) ) ;
#41970 = CARTESIAN_POINT ( 'NONE',  ( 7.644554776091147741E-16, 12.48450537969573659, -167.4687500020483526 ) ) ;
#41971 = DIRECTION ( 'NONE',  ( -0.000000000000000000, -0.000000000000000000, 1.000000000000000000 ) ) ;
#41972 = DIRECTION ( 'NONE',  ( -0.000000000000000000, -0.000000000000000000, 1.000000000000000000 ) ) ;
#41973 = CARTESIAN_POINT ( 'NONE',  ( -9.999999999999998224, 1.224646799147353059E-15, -196.2500000000000000 ) ) ;
#41974 = VECTOR ( 'NONE', #19622, 1000.000000000000000 ) ;
#41975 = CARTESIAN_POINT ( 'NONE',  ( 7.644554776091147741E-16, 12.48450537969573659, -107.4687500020483668 ) ) ;
#41976 = CARTESIAN_POINT ( 'NONE',  ( 0.000000000000000000, 0.000000000000000000, -217.0000000000000853 ) ) ;
#41977 = CARTESIAN_POINT ( 'NONE',  ( 5.405949406249999534, 9.363379034771803333, -77.78125000204838102 ) ) ;
#41978 = EDGE_CURVE ( 'NONE', #28714, #2188, #10112, .T. ) ;
#41979 = CARTESIAN_POINT ( 'NONE',  ( -2.293366432827344421E-15, -12.48450537969573659, -88.71875000204838102 ) ) ;
#41980 = EDGE_CURVE ( 'NONE', #32014, #23494, #3229, .T. ) ;
#41981 = CARTESIAN_POINT ( 'NONE',  ( 10.81189881249999729, 0.000000000000000000, -57.03125000204836681 ) ) ;
#41982 = CARTESIAN_POINT ( 'NONE',  ( -5.000000000000003553, -8.660254037844383745, -149.8750000040967905 ) ) ;
#41983 = CARTESIAN_POINT ( 'NONE',  ( 7.070501591499377789E-16, 11.54700538379251284, -123.1249999999999858 ) ) ;
#41984 = ORIENTED_EDGE ( 'NONE', *, *, #2158, .F. ) ;
#41985 = AXIS2_PLACEMENT_3D ( 'NONE', #42035, #29313, #19166 ) ;
#41986 = CARTESIAN_POINT ( 'NONE',  ( -10.81189881249999729, 1.324075727343319199E-15, -146.2812500020483810 ) ) ;
#41987 = CARTESIAN_POINT ( 'NONE',  ( -10.81189881249999729, 6.242252689847871849, -153.9062500020483810 ) ) ;
#41988 = CARTESIAN_POINT ( 'NONE',  ( 5.405949406249999534, 9.363379034771803333, -196.2812500020484094 ) ) ;
#41989 = DIRECTION ( 'NONE',  ( -0.000000000000000000, -0.000000000000000000, 1.000000000000000000 ) ) ;
#41990 = CARTESIAN_POINT ( 'NONE',  ( -10.81189881249999729, 1.324075727343319199E-15, -90.59375000204838102 ) ) ;
#41991 = ORIENTED_EDGE ( 'NONE', *, *, #13519, .F. ) ;
#41992 = CARTESIAN_POINT ( 'NONE',  ( 5.000000000000000000, 8.660254037844385522, -66.24999999999997158 ) ) ;
#41993 = CARTESIAN_POINT ( 'NONE',  ( -2.293366432827344421E-15, -12.48450537969573659, -184.7187500020484094 ) ) ;
#41994 = CARTESIAN_POINT ( 'NONE',  ( -9.999999999999998224, 1.224646799147353059E-15, -70.62500000409677625 ) ) ;
#41995 = CARTESIAN_POINT ( 'NONE',  ( 9.999999999999998224, 0.000000000000000000, -116.3750000040967905 ) ) ;
#41996 = CARTESIAN_POINT ( 'NONE',  ( 9.999999999999998224, 0.000000000000000000, -200.0000000000000000 ) ) ;
#41997 = CARTESIAN_POINT ( 'NONE',  ( 5.405949406249992428, -9.363379034771808662, -81.28125000204839523 ) ) ;
#41998 = CARTESIAN_POINT ( 'NONE',  ( 7.644554776091147741E-16, 12.48450537969573659, -64.15625000204838102 ) ) ;
#41999 = CARTESIAN_POINT ( 'NONE',  ( -5.000000000000003553, -8.660254037844383745, -67.37500000409676204 ) ) ;
#42000 = CARTESIAN_POINT ( 'NONE',  ( 0.000000000000000000, 0.000000000000000000, -200.0000000000000000 ) ) ;
#42001 = CARTESIAN_POINT ( 'NONE',  ( -5.405949406249996869, 9.363379034771805109, -21.84375000204835615 ) ) ;
#42002 = CARTESIAN_POINT ( 'NONE',  ( -4.999999999999996447, 8.660254037844387298, -46.87500000409677625 ) ) ;
#42003 = CARTESIAN_POINT ( 'NONE',  ( 10.81189881249999907, 6.242252689847868297, -194.9062500020484379 ) ) ;
#42004 = CARTESIAN_POINT ( 'NONE',  ( 5.405949406249999534, 9.363379034771803333, -23.78125000204836681 ) ) ;
#42005 = CARTESIAN_POINT ( 'NONE',  ( -10.81189881249999729, 1.324075727343319199E-15, -5.093750002048369474 ) ) ;
#42006 = DIRECTION ( 'NONE',  ( 1.000000000000000000, 0.000000000000000000, 0.000000000000000000 ) ) ;
#42007 = CARTESIAN_POINT ( 'NONE',  ( 9.999999999999998224, 0.000000000000000000, -36.87500000409676915 ) ) ;
#42008 = CARTESIAN_POINT ( 'NONE',  ( -9.999999999999998224, 1.224646799147353059E-15, -39.12500000409676915 ) ) ;
#42009 = CARTESIAN_POINT ( 'NONE',  ( -4.999999999999996447, 8.660254037844387298, -175.5000000000000284 ) ) ;
#42010 = DIRECTION ( 'NONE',  ( -0.000000000000000000, -0.000000000000000000, 1.000000000000000000 ) ) ;
#42012 = ORIENTED_EDGE ( 'NONE', *, *, #19620, .T. ) ;
#42011 = CARTESIAN_POINT ( 'NONE',  ( -5.405949406250003975, -9.363379034771801557, -101.0312500020483952 ) ) ;
#42013 = DIRECTION ( 'NONE',  ( -0.000000000000000000, -0.000000000000000000, 1.000000000000000000 ) ) ;
#42014 = ADVANCED_FACE ( 'NONE', ( #36450 ), #9903, .T. ) ;
#42015 = ORIENTED_EDGE ( 'NONE', *, *, #25929, .T. ) ;
#42016 = ORIENTED_EDGE ( 'NONE', *, *, #22928, .F. ) ;
#42017 =( BOUNDED_CURVE ( )  B_SPLINE_CURVE ( 2, ( #27711, #31175, #24052, #5049, #37193, #21438, #40417 ),
 .UNSPECIFIED., .F., .F. ) 
 B_SPLINE_CURVE_WITH_KNOTS ( ( 3, 2, 2, 3 ),
 ( 0.2201492537313433639, 0.2213930348258707215, 0.2226368159203980790, 0.2238805970149254365 ),
 .UNSPECIFIED. ) 
 CURVE ( )  GEOMETRIC_REPRESENTATION_ITEM ( )  RATIONAL_B_SPLINE_CURVE ( ( 0.9999999999999910072, 0.8660254037844477004, 1.000000000000000000, 0.8660254037844387076, 1.000000000000000000, 0.8660254037844327124, 1.000000000000005995 ) ) 
 REPRESENTATION_ITEM ( '' )  );
#42018 = CARTESIAN_POINT ( 'NONE',  ( -5.405949406249996869, 9.363379034771805109, -26.53125000204836681 ) ) ;
#42019 = CALENDAR_DATE ( 2026, 28, 9 ) ;
#42020 = CARTESIAN_POINT ( 'NONE',  ( -5.405949406249996869, 9.363379034771805109, -80.34375000204838102 ) ) ;
#42021 = CARTESIAN_POINT ( 'NONE',  ( 0.000000000000000000, 0.000000000000000000, -203.0000000000000000 ) ) ;
#42022 = FACE_OUTER_BOUND ( 'NONE', #7799, .T. ) ;
#42023 = CARTESIAN_POINT ( 'NONE',  ( -1.040834085586084257E-14, 125.0000000000000000, 22.49999999999999289 ) ) ;
#42024 = LINE ( 'NONE', #25647, #22577 ) ;
#42025 = CARTESIAN_POINT ( 'NONE',  ( 10.81189881249999907, 6.242252689847868297, -155.9062500020484094 ) ) ;
#42026 = CARTESIAN_POINT ( 'NONE',  ( -4.999999999999996447, 8.660254037844387298, -7.875000004096744277 ) ) ;
#42027 = DIRECTION ( 'NONE',  ( -0.000000000000000000, -0.000000000000000000, -1.000000000000000000 ) ) ;
#42028 = CARTESIAN_POINT ( 'NONE',  ( -2.293366432827344421E-15, -12.48450537969573659, -130.7187500020483810 ) ) ;
#42029 = EDGE_CURVE ( 'NONE', #35877, #900, #40483, .T. ) ;
#42030 = CARTESIAN_POINT ( 'NONE',  ( 10.81189881249999729, 0.000000000000000000, -118.3437500020483810 ) ) ;
#42031 = CARTESIAN_POINT ( 'NONE',  ( 10.81189881249999551, -6.242252689847874514, -79.46875000204838102 ) ) ;
#42032 = CARTESIAN_POINT ( 'NONE',  ( -2.293366432827344421E-15, -12.48450537969573659, -87.40625000204838102 ) ) ;
#42033 = CARTESIAN_POINT ( 'NONE',  ( -9.999999999999998224, 1.224646799147353059E-15, -169.6250000040967905 ) ) ;
#42034 = ADVANCED_FACE ( 'NONE', ( #27808 ), #30623, .T. ) ;
#42035 = CARTESIAN_POINT ( 'NONE',  ( 0.000000000000000000, 0.000000000000000000, -200.0000000000000000 ) ) ;
#42036 = CARTESIAN_POINT ( 'NONE',  ( -5.405949406249996869, 9.363379034771805109, -166.0312500020484094 ) ) ;
#42037 = CARTESIAN_POINT ( 'NONE',  ( 5.405949406249999534, 9.363379034771803333, -182.7812500020484094 ) ) ;
#42038 = CARTESIAN_POINT ( 'NONE',  ( -5.405949406249996869, 9.363379034771805109, -45.84375000204838102 ) ) ;
#42039 = AXIS2_PLACEMENT_3D ( 'NONE', #3431, #33434, #30825 ) ;
#42040 = EDGE_CURVE ( 'NONE', #27003, #14981, #8002, .T. ) ;
#42041 = CARTESIAN_POINT ( 'NONE',  ( 7.070501591499377789E-16, 11.54700538379251284, -164.0000000040967905 ) ) ;
#42042 = CARTESIAN_POINT ( 'NONE',  ( -10.81189881249999729, 6.242252689847871849, -5.406250002048357928 ) ) ;
#42043 = CARTESIAN_POINT ( 'NONE',  ( 5.405949406249999534, 9.363379034771803333, -16.09375000204835260 ) ) ;
#42044 = CARTESIAN_POINT ( 'NONE',  ( 4.999999999999992006, -8.660254037844389075, -126.7499999999999716 ) ) ;
#42045 = CARTESIAN_POINT ( 'NONE',  ( 5.405949406249992428, -9.363379034771808662, -112.5937500020483810 ) ) ;
#42046 = CARTESIAN_POINT ( 'NONE',  ( 9.999999999999998224, 0.000000000000000000, -88.99999999999998579 ) ) ;
#42047 = CARTESIAN_POINT ( 'NONE',  ( 10.81189881249999907, 6.242252689847868297, -17.90625000204837391 ) ) ;
#42048 = CARTESIAN_POINT ( 'NONE',  ( -5.000000000000003553, -8.660254037844383745, -97.37500000409677625 ) ) ;
#42049 = CARTESIAN_POINT ( 'NONE',  ( 5.500000000000000888, -20.00000000000000000, -232.0000000000000000 ) ) ;
#42050 = CARTESIAN_POINT ( 'NONE',  ( 10.81189881249999551, -6.242252689847874514, -117.1562500020483810 ) ) ;
#42051 = CARTESIAN_POINT ( 'NONE',  ( -2.293366432827344421E-15, -12.48450537969573659, -94.90625000204838102 ) ) ;
#42052 = ORIENTED_EDGE ( 'NONE', *, *, #2395, .T. ) ;
#42053 = CARTESIAN_POINT ( 'NONE',  ( -4.999999999999996447, 8.660254037844387298, -91.87500000409677625 ) ) ;
#42054 = CARTESIAN_POINT ( 'NONE',  ( -9.999999999999742428, -5.773502691896402084, -101.6249999999999716 ) ) ;
#42055 = CARTESIAN_POINT ( 'NONE',  ( 5.405949406249999534, 9.363379034771803333, -47.59375000204838102 ) ) ;
#42056 = ORIENTED_EDGE ( 'NONE', *, *, #29392, .T. ) ;
#42057 = CARTESIAN_POINT ( 'NONE',  ( 5.000000000000000000, 8.660254037844385522, -21.24999999999996447 ) ) ;
#42058 = CARTESIAN_POINT ( 'NONE',  ( -5.405949406249996869, 9.363379034771805109, -23.53125000204836681 ) ) ;
#42059 = CARTESIAN_POINT ( 'NONE',  ( -4.999999999999996447, 8.660254037844387298, -150.0000000000000000 ) ) ;
#42060 = ADVANCED_FACE ( 'NONE', ( #31272 ), #13095, .T. ) ;
#42061 = CARTESIAN_POINT ( 'NONE',  ( -10.00000000000000000, -5.773502691896251982, -21.00000000409677270 ) ) ;
#42062 = EDGE_CURVE ( 'NONE', #17414, #42281, #570, .T. ) ;
#42063 = CARTESIAN_POINT ( 'NONE',  ( 9.999999999999996447, -5.773502691896262640, -197.1250000000000284 ) ) ;
#42065 = ORIENTED_EDGE ( 'NONE', *, *, #13398, .F. ) ;
#42064 = CARTESIAN_POINT ( 'NONE',  ( -5.405949406249996869, 9.363379034771805109, -124.0312500020483952 ) ) ;
#42066 = CARTESIAN_POINT ( 'NONE',  ( -9.999999999999998224, 1.224646799147353059E-15, -158.7500000000000000 ) ) ;
#42067 = ORIENTED_EDGE ( 'NONE', *, *, #9956, .T. ) ;
#42068 = CARTESIAN_POINT ( 'NONE',  ( -5.405949406249996869, 9.363379034771805109, -50.53125000204835970 ) ) ;
#42069 = APPROVAL_STATUS ( 'not_yet_approved' ) ;
#42070 = AXIS2_PLACEMENT_3D ( 'NONE', #3385, #17160, #9852 ) ;
#42071 = CARTESIAN_POINT ( 'NONE',  ( -10.81189881249999729, 1.324075727343319199E-15, -107.0937500020483810 ) ) ;
#42073 = EDGE_LOOP ( 'NONE', ( #22599, #42571, #32123, #7259 ) ) ;
#42072 = VERTEX_POINT ( 'NONE', #14619 ) ;
#42074 = CARTESIAN_POINT ( 'NONE',  ( -9.999999999999868550, 5.773502691896333694, -175.3750000000000000 ) ) ;
#42075 = CARTESIAN_POINT ( 'NONE',  ( -9.999999999999998224, 1.224646799147353059E-15, -112.6250000040967763 ) ) ;
#42076 = CARTESIAN_POINT ( 'NONE',  ( 7.644554776091147741E-16, 12.48450537969573659, -150.9687500020483810 ) ) ;
#42077 = CARTESIAN_POINT ( 'NONE',  ( 10.81189881249999729, 0.000000000000000000, -183.0312500020484094 ) ) ;
#42078 = CARTESIAN_POINT ( 'NONE',  ( -10.81189881249999907, -6.242252689847864744, -3.468750002048364145 ) ) ;
#42079 = CARTESIAN_POINT ( 'NONE',  ( 0.000000000000000000, 0.000000000000000000, -176.9999999999999432 ) ) ;
#42080 = CARTESIAN_POINT ( 'NONE',  ( -10.81189881249999729, 1.324075727343319199E-15, -138.5937500020483810 ) ) ;
#42081 = CARTESIAN_POINT ( 'NONE',  ( -10.81189881249999729, 1.324075727343319199E-15, -101.0937500020483810 ) ) ;
#42082 = CARTESIAN_POINT ( 'NONE',  ( -9.999999999999479527, -5.773502691896549521, -148.1249999999999716 ) ) ;
#42083 = CARTESIAN_POINT ( 'NONE',  ( -2.293366432827344421E-15, -12.48450537969573659, -111.4062500020483952 ) ) ;
#42084 = CARTESIAN_POINT ( 'NONE',  ( -9.999999999999998224, 1.224646799147353059E-15, -190.6250000040967905 ) ) ;
#42085 = CARTESIAN_POINT ( 'NONE',  ( 10.81189881249999729, 6.242252689847867408, -119.7187500020483810 ) ) ;
#42086 = CARTESIAN_POINT ( 'NONE',  ( -2.293366432827344421E-15, -12.48450537969573659, -195.4062500020484094 ) ) ;
#42087 = CARTESIAN_POINT ( 'NONE',  ( -23.09401076758503280, 0.000000000000000000, 49.99999999999998579 ) ) ;
#42088 = CARTESIAN_POINT ( 'NONE',  ( -5.000000000000003553, -8.660254037844383745, -139.0000000000000000 ) ) ;
#42089 = CARTESIAN_POINT ( 'NONE',  ( -10.00000000000000000, -5.773502691896251982, -10.12499999999996803 ) ) ;
#42090 = CARTESIAN_POINT ( 'NONE',  ( 5.405949406249992428, -9.363379034771808662, -70.59375000204836681 ) ) ;
#42091 = CARTESIAN_POINT ( 'NONE',  ( 10.81189881249999729, 0.000000000000000000, -50.84375000204835260 ) ) ;
#42092 = CARTESIAN_POINT ( 'NONE',  ( -10.00000000000000000, -5.773502691896251982, -190.5000000040967905 ) ) ;
#42093 = CARTESIAN_POINT ( 'NONE',  ( 7.644554776091147741E-16, 12.48450537969573659, -25.15625000204838457 ) ) ;
#42094 = CARTESIAN_POINT ( 'NONE',  ( -10.81189881249999729, 6.242252689847871849, -35.21875000204835260 ) ) ;
#42095 = CARTESIAN_POINT ( 'NONE',  ( -2.293366432827344421E-15, -12.48450537969573659, -145.7187500020484094 ) ) ;
#42096 = CARTESIAN_POINT ( 'NONE',  ( -4.999999999999996447, 8.660254037844387298, -113.9999999999999858 ) ) ;
#42097 = CARTESIAN_POINT ( 'NONE',  ( 9.999999999999998224, 0.000000000000000000, -42.49999999999998579 ) ) ;
#42098 = CARTESIAN_POINT ( 'NONE',  ( 4.999999999999992006, -8.660254037844389075, -65.24999999999997158 ) ) ;
#42099 = CARTESIAN_POINT ( 'NONE',  ( 5.405949406249992428, -9.363379034771808662, -138.2812500020483810 ) ) ;
#42100 = CARTESIAN_POINT ( 'NONE',  ( 5.405949406249992428, -9.363379034771808662, -118.7812500020483952 ) ) ;
#42101 = VERTEX_POINT ( 'NONE', #20674 ) ;
#42102 = CARTESIAN_POINT ( 'NONE',  ( -2.121150477449813534E-15, -11.54700538379251284, -176.3750000000000000 ) ) ;
#42103 = CARTESIAN_POINT ( 'NONE',  ( -2.121150477449813534E-15, -11.54700538379251284, -115.2500000040967763 ) ) ;
#42104 = CARTESIAN_POINT ( 'NONE',  ( -9.999999999999227285, -5.773502691896698735, -128.6249999999999716 ) ) ;
#42105 = CARTESIAN_POINT ( 'NONE',  ( 5.405949406249992428, -9.363379034771808662, -72.09375000204836681 ) ) ;
#42106 = CARTESIAN_POINT ( 'NONE',  ( -9.999999999999998224, 1.224646799147353059E-15, -40.24999999999997868 ) ) ;
#42107 = AXIS2_PLACEMENT_3D ( 'NONE', #8542, #21694, #25789 ) ;
#42108 = EDGE_CURVE ( 'NONE', #10196, #23394, #34721, .T. ) ;
#42109 = CARTESIAN_POINT ( 'NONE',  ( 9.999999999999998224, 0.000000000000000000, -27.87500000409676204 ) ) ;
#42110 = CARTESIAN_POINT ( 'NONE',  ( -2.293366432827344421E-15, -12.48450537969573659, -49.90625000204837391 ) ) ;
#42111 = CARTESIAN_POINT ( 'NONE',  ( -5.000000000000003553, -8.660254037844383745, -142.0000000000000000 ) ) ;
#42112 = CARTESIAN_POINT ( 'NONE',  ( -2.293366432827344421E-15, -12.48450537969573659, -39.40625000204836681 ) ) ;
#42113 = CARTESIAN_POINT ( 'NONE',  ( -9.999999999999996447, 5.773502691896259975, -166.3750000000000000 ) ) ;
#42114 = CARTESIAN_POINT ( 'NONE',  ( 10.81189881249999729, 0.000000000000000000, -138.0312500020484094 ) ) ;
#42115 = CARTESIAN_POINT ( 'NONE',  ( 10.81189881249999551, -6.242252689847874514, -148.6562500020484094 ) ) ;
#42116 = CARTESIAN_POINT ( 'NONE',  ( -5.000000000000003553, -8.660254037844383745, -164.8750000040967905 ) ) ;
#42117 = PLANE ( 'NONE',  #14158 ) ;
#42118 = VERTEX_POINT ( 'NONE', #14176 ) ;
#42119 = ORIENTED_EDGE ( 'NONE', *, *, #19360, .F. ) ;
#42120 = ORIENTED_EDGE ( 'NONE', *, *, #25999, .T. ) ;
#42121 = AXIS2_PLACEMENT_3D ( 'NONE', #14925, #34173, #30926 ) ;
#42122 = LINE ( 'NONE', #41910, #14558 ) ;
#42123 = CARTESIAN_POINT ( 'NONE',  ( 5.405949406249999534, 9.363379034771803333, -181.0937500020483810 ) ) ;
#42124 = LOCAL_TIME ( 11, 57, 6.000000000000000000, #8176 ) ;
#42125 = CARTESIAN_POINT ( 'NONE',  ( -10.81189881249999907, -6.242252689847864744, -27.46875000204838457 ) ) ;
#42126 = CARTESIAN_POINT ( 'NONE',  ( 9.999999999999998224, 0.000000000000000000, -21.49999999999996447 ) ) ;
#42127 = CARTESIAN_POINT ( 'NONE',  ( 10.81189881249999729, 0.000000000000000000, -164.8437500020484094 ) ) ;
#42128 = CARTESIAN_POINT ( 'NONE',  ( 5.405949406249992428, -9.363379034771808662, -148.5937500020483810 ) ) ;
#42129 = CARTESIAN_POINT ( 'NONE',  ( -5.000000000000003553, -8.660254037844383745, -176.5000000000000000 ) ) ;
#42130 = CARTESIAN_POINT ( 'NONE',  ( 10.81189881249999907, 6.242252689847868297, -130.2187500020483810 ) ) ;
#42131 = CARTESIAN_POINT ( 'NONE',  ( -10.81189881249999729, 6.242252689847871849, -140.4062500020484094 ) ) ;
#42133 = CARTESIAN_POINT ( 'NONE',  ( 10.81189881249999729, 0.000000000000000000, -20.84375000204835615 ) ) ;
#42132 =( BOUNDED_CURVE ( )  B_SPLINE_CURVE ( 2, ( #23079, #33441, #16785, #7310, #23716, #26735, #36237 ),
 .UNSPECIFIED., .F., .F. ) 
 B_SPLINE_CURVE_WITH_KNOTS ( ( 3, 2, 2, 3 ),
 ( 0.8731343283582092551, 0.8743781094527366404, 0.8756218905472639147, 0.8768656716417913000 ),
 .UNSPECIFIED. ) 
 CURVE ( )  GEOMETRIC_REPRESENTATION_ITEM ( )  RATIONAL_B_SPLINE_CURVE ( ( 0.9999999999999641398, 0.8660254037844745678, 1.000000000000000000, 0.8660254037844387076, 1.000000000000000000, 0.8660254037844148378, 1.000000000000023981 ) ) 
 REPRESENTATION_ITEM ( '' )  );
#42134 = CARTESIAN_POINT ( 'NONE',  ( -5.405949406249996869, 9.363379034771805109, -143.3437500020483810 ) ) ;
#42135 = CYLINDRICAL_SURFACE ( 'NONE', #4706, 9.999999999999998224 ) ;
#42136 = CARTESIAN_POINT ( 'NONE',  ( 9.999999999998969713, 5.773502691896851502, -70.87499999999997158 ) ) ;
#42137 = CARTESIAN_POINT ( 'NONE',  ( 9.999999999999996447, -5.773502691896262640, -161.1250000000000284 ) ) ;
#42138 = AXIS2_PLACEMENT_3D ( 'NONE', #10681, #14333, #40245 ) ;
#42139 = CARTESIAN_POINT ( 'NONE',  ( -2.293366432827344421E-15, -12.48450537969573659, -79.71875000204838102 ) ) ;
#42140 = CARTESIAN_POINT ( 'NONE',  ( -10.81189881249999729, 1.324075727343319199E-15, -48.78125000204838813 ) ) ;
#42141 = CARTESIAN_POINT ( 'NONE',  ( 10.81189881249999729, 0.000000000000000000, -64.34375000204836681 ) ) ;
#42142 = CARTESIAN_POINT ( 'NONE',  ( -10.00000000000102496, 5.773502691895664007, -56.87499999999995026 ) ) ;
#42143 = CARTESIAN_POINT ( 'NONE',  ( -5.405949406250003975, -9.363379034771801557, -168.3437500020484094 ) ) ;
#42144 = CARTESIAN_POINT ( 'NONE',  ( -10.00000000000000000, -5.773502691896251982, -140.6249999999999716 ) ) ;
#42145 = CARTESIAN_POINT ( 'NONE',  ( 5.405949406249999534, 9.363379034771803333, -145.2812500020483810 ) ) ;
#42146 = DIRECTION ( 'NONE',  ( -0.000000000000000000, -0.000000000000000000, 1.000000000000000000 ) ) ;
#42147 = CARTESIAN_POINT ( 'NONE',  ( -4.999999999999996447, 8.660254037844387298, -118.8750000040967905 ) ) ;
#42148 = CARTESIAN_POINT ( 'NONE',  ( -10.00000000000000000, -5.773502691896251982, -94.12499999999998579 ) ) ;
#42149 = ORIENTED_EDGE ( 'NONE', *, *, #33874, .F. ) ;
#42150 = CARTESIAN_POINT ( 'NONE',  ( -10.81189881249999729, 1.324075727343319199E-15, -120.7812500020483952 ) ) ;
#42151 = CARTESIAN_POINT ( 'NONE',  ( -9.999999999999998224, 1.224646799147353059E-15, -142.6250000040967905 ) ) ;
#42152 = CARTESIAN_POINT ( 'NONE',  ( -9.999999999999998224, 1.224646799147353059E-15, -49.24999999999998579 ) ) ;
#42153 = CARTESIAN_POINT ( 'NONE',  ( 10.81189881249999729, 0.000000000000000000, -171.0312500020484094 ) ) ;
#42154 = CARTESIAN_POINT ( 'NONE',  ( 4.999999999999992006, -8.660254037844389075, -49.12500000409678336 ) ) ;
#42155 = CARTESIAN_POINT ( 'NONE',  ( 9.999999999999998224, 0.000000000000000000, -30.49999999999997158 ) ) ;
#42156 = CARTESIAN_POINT ( 'NONE',  ( 10.81189881249999907, 6.242252689847868297, -59.90625000204838102 ) ) ;
#42157 = CARTESIAN_POINT ( 'NONE',  ( -9.999999999999998224, 1.224646799147353059E-15, -148.6250000040967905 ) ) ;
#42158 = CARTESIAN_POINT ( 'NONE',  ( 10.81189881249999729, 0.000000000000000000, -166.5312500020484094 ) ) ;
#42159 = APPLICATION_CONTEXT ( 'configuration controlled 3d designs of mechanical parts and assemblies' ) ;
#42160 = LINE ( 'NONE', #12591, #35298 ) ;
#42161 = CARTESIAN_POINT ( 'NONE',  ( 0.000000000000000000, 0.000000000000000000, -200.0000000000000000 ) ) ;
#42162 = ORIENTED_EDGE ( 'NONE', *, *, #28084, .F. ) ;
#42163 = DIRECTION ( 'NONE',  ( -1.000000000000000000, 0.000000000000000000, -0.000000000000000000 ) ) ;
#42164 = CARTESIAN_POINT ( 'NONE',  ( -9.999999999999479527, -5.773502691896549521, -71.62499999999998579 ) ) ;
#42165 = VECTOR ( 'NONE', #32479, 1000.000000000000000 ) ;
#42167 = VERTEX_POINT ( 'NONE', #5145 ) ;
#42166 = CARTESIAN_POINT ( 'NONE',  ( 7.644554776091147741E-16, 12.48450537969573659, -79.15625000204838102 ) ) ;
#42168 =( NAMED_UNIT ( * ) SI_UNIT ( $, .STERADIAN. ) SOLID_ANGLE_UNIT ( ) );
#42170 = ORIENTED_EDGE ( 'NONE', *, *, #37881, .F. ) ;
#42169 = LINE ( 'NONE', #28404, #692 ) ;
#42171 = ORIENTED_EDGE ( 'NONE', *, *, #42504, .T. ) ;
#42172 = CARTESIAN_POINT ( 'NONE',  ( -2.293366432827344421E-15, -12.48450537969573659, -31.71875000204835260 ) ) ;
#42173 = CYLINDRICAL_SURFACE ( 'NONE', #429, 9.999999999999998224 ) ;
#42174 = CARTESIAN_POINT ( 'NONE',  ( 10.81189881249999907, 6.242252689847868297, -5.906250002048359704 ) ) ;
#42176 = ORIENTED_EDGE ( 'NONE', *, *, #32327, .T. ) ;
#42175 = CARTESIAN_POINT ( 'NONE',  ( 10.81189881249999907, 6.242252689847868297, -52.21875000204837391 ) ) ;
#42177 = CARTESIAN_POINT ( 'NONE',  ( -9.999999999999998224, 1.224646799147353059E-15, -71.74999999999998579 ) ) ;
#42178 = CARTESIAN_POINT ( 'NONE',  ( -5.000000000000003553, -8.660254037844383745, -26.49999999999996803 ) ) ;
#42179 = CARTESIAN_POINT ( 'NONE',  ( -5.405949406250003975, -9.363379034771801557, -186.3437500020483810 ) ) ;
#42180 = CARTESIAN_POINT ( 'NONE',  ( -2.293366432827344421E-15, -12.48450537969573659, -174.2187500020484094 ) ) ;
#42181 = CARTESIAN_POINT ( 'NONE',  ( -5.405949406250003975, -9.363379034771801557, -157.8437500020483810 ) ) ;
#42182 = AXIS2_PLACEMENT_3D ( 'NONE', #21493, #8122, #24322 ) ;
#42183 = CARTESIAN_POINT ( 'NONE',  ( -10.81189881249999729, -6.242252689847864744, -171.4687500020483526 ) ) ;
#42184 = DIRECTION ( 'NONE',  ( -0.000000000000000000, -0.000000000000000000, -1.000000000000000000 ) ) ;
#42185 = CARTESIAN_POINT ( 'NONE',  ( -9.999999999999998224, 1.224646799147353059E-15, -200.0000000000000000 ) ) ;
#42186 = CARTESIAN_POINT ( 'NONE',  ( -10.00000000000000000, -5.773502691896251982, -190.1250000000000284 ) ) ;
#42187 = CARTESIAN_POINT ( 'NONE',  ( -10.81189881249999729, 6.242252689847871849, -107.2187500020483810 ) ) ;
#42188 = LINE ( 'NONE', #9813, #33450 ) ;
#42189 = CARTESIAN_POINT ( 'NONE',  ( -5.405949406249996869, 9.363379034771805109, -71.53125000204838102 ) ) ;
#42190 = CARTESIAN_POINT ( 'NONE',  ( -9.999999999999227285, -5.773502691896698735, -132.0000000040967620 ) ) ;
#42191 = CARTESIAN_POINT ( 'NONE',  ( 10.81189881249999729, 0.000000000000000000, -83.84375000204836681 ) ) ;
#42192 = CARTESIAN_POINT ( 'NONE',  ( -10.81189881249999729, 1.324075727343319199E-15, -60.78125000204836681 ) ) ;
#42193 = CARTESIAN_POINT ( 'NONE',  ( 10.00000000000000000, 5.773502691896255534, -144.7500000040967905 ) ) ;
#42194 = CARTESIAN_POINT ( 'NONE',  ( 7.070501591499377789E-16, 11.54700538379251284, -121.6249999999999858 ) ) ;
#42195 = ORIENTED_EDGE ( 'NONE', *, *, #7580, .F. ) ;
#42196 = CARTESIAN_POINT ( 'NONE',  ( -2.293366432827344421E-15, -12.48450537969573659, -141.4062500020484094 ) ) ;
#42197 = CARTESIAN_POINT ( 'NONE',  ( -10.81189881249999907, -6.242252689847864744, -158.1562500020484094 ) ) ;
#42198 = AXIS2_PLACEMENT_3D ( 'NONE', #25985, #8945, #12583 ) ;
#42199 = CARTESIAN_POINT ( 'NONE',  ( 10.81189881249999729, 0.000000000000000000, -198.0312500020484094 ) ) ;
#42200 = CARTESIAN_POINT ( 'NONE',  ( -2.121150477449813534E-15, -11.54700538379251284, -179.3750000000000000 ) ) ;
#42201 = CARTESIAN_POINT ( 'NONE',  ( 5.405949406249999534, 9.363379034771803333, -91.09375000204838102 ) ) ;
#42202 = ORIENTED_EDGE ( 'NONE', *, *, #18426, .T. ) ;
#42203 = CARTESIAN_POINT ( 'NONE',  ( -5.000000000000003553, -8.660254037844383745, -66.99999999999997158 ) ) ;
#42204 = CARTESIAN_POINT ( 'NONE',  ( -5.405949406250003975, -9.363379034771801557, -190.8437500020484094 ) ) ;
#42205 = CARTESIAN_POINT ( 'NONE',  ( 9.999999999999998224, 0.000000000000000000, -74.37500000409677625 ) ) ;
#42206 = FACE_OUTER_BOUND ( 'NONE', #28461, .T. ) ;
#42207 = CARTESIAN_POINT ( 'NONE',  ( -9.999999999999998224, 1.224646799147353059E-15, -12.12500000409674783 ) ) ;
#42208 = CARTESIAN_POINT ( 'NONE',  ( -2.293366432827344421E-15, -12.48450537969573659, -85.90625000204839523 ) ) ;
#42209 = CARTESIAN_POINT ( 'NONE',  ( -10.81189881249999729, 1.324075727343319199E-15, -63.78125000204837391 ) ) ;
#42210 = CARTESIAN_POINT ( 'NONE',  ( 5.000000000000000000, 8.660254037844385522, -63.62500000409676204 ) ) ;
#42211 = CARTESIAN_POINT ( 'NONE',  ( 5.405949406249999534, 9.363379034771803333, -17.59375000204835260 ) ) ;
#42212 = ORIENTED_EDGE ( 'NONE', *, *, #12691, .T. ) ;
#42213 = CARTESIAN_POINT ( 'NONE',  ( -10.81189881249999729, 1.324075727343319199E-15, -194.2812500020484094 ) ) ;
#42214 = CARTESIAN_POINT ( 'NONE',  ( 7.644554776091147741E-16, 12.48450537969573659, -13.15625000204836859 ) ) ;
#42215 = CARTESIAN_POINT ( 'NONE',  ( -10.81189881249999729, -6.242252689847864744, -3.468750002048364145 ) ) ;
#42216 = CARTESIAN_POINT ( 'NONE',  ( -9.999999999999227285, -5.773502691896698735, -111.0000000040967620 ) ) ;
#42217 = CARTESIAN_POINT ( 'NONE',  ( 9.999999999999998224, 0.000000000000000000, -114.8750000040967905 ) ) ;
#42218 = CARTESIAN_POINT ( 'NONE',  ( -10.00000000000000000, -5.773502691896252870, -173.6249999999999716 ) ) ;
#42219 = CARTESIAN_POINT ( 'NONE',  ( 10.00000000000000000, 5.773502691896255534, -172.8750000000000000 ) ) ;
#42220 = CARTESIAN_POINT ( 'NONE',  ( -9.999999999999998224, 1.224646799147353059E-15, -169.6250000040967905 ) ) ;
#42222 = EDGE_LOOP ( 'NONE', ( #19718, #14991, #35356, #20673 ) ) ;
#42221 = CARTESIAN_POINT ( 'NONE',  ( 10.81189881249999551, -6.242252689847874514, -99.15625000204838102 ) ) ;
#42223 = CARTESIAN_POINT ( 'NONE',  ( -10.00000000000051337, 5.773502691895962435, -115.7500000040967905 ) ) ;
#42224 = EDGE_CURVE ( 'NONE', #4287, #13498, #7740, .T. ) ;
#42225 = ORIENTED_EDGE ( 'NONE', *, *, #1000, .F. ) ;
#42226 =( BOUNDED_CURVE ( )  B_SPLINE_CURVE ( 2, ( #41642, #25273, #22022, #5622, #18774, #11436, #24634 ),
 .UNSPECIFIED., .F., .F. ) 
 B_SPLINE_CURVE_WITH_KNOTS ( ( 3, 2, 2, 3 ),
 ( 0.2761194029850747578, 0.2773631840796020875, 0.2786069651741294728, 0.2798507462686568026 ),
 .UNSPECIFIED. ) 
 CURVE ( )  GEOMETRIC_REPRESENTATION_ITEM ( )  RATIONAL_B_SPLINE_CURVE ( ( 0.9999999999999880096, 0.8660254037844506980, 1.000000000000000000, 0.8660254037844387076, 1.000000000000000000, 0.8660254037844267172, 1.000000000000011990 ) ) 
 REPRESENTATION_ITEM ( '' )  );
#42227 = EDGE_CURVE ( 'NONE', #39036, #20043, #21104, .T. ) ;
#42228 = ORIENTED_EDGE ( 'NONE', *, *, #41255, .T. ) ;
#42229 = CARTESIAN_POINT ( 'NONE',  ( 10.81189881249999729, 0.000000000000000000, -35.84375000204836681 ) ) ;
#42230 = CARTESIAN_POINT ( 'NONE',  ( 5.405949406249999534, 9.363379034771803333, -29.78125000204837036 ) ) ;
#42231 = ITEM_DEFINED_TRANSFORMATION ( 'NONE', 'NONE', #11063,  #39998 ) ;
#42232 = CARTESIAN_POINT ( 'NONE',  ( 10.81189881249999907, 6.242252689847868297, -76.21875000204836681 ) ) ;
#42233 = LINE ( 'NONE', #19362, #4991 ) ;
#42234 = CARTESIAN_POINT ( 'NONE',  ( 7.608343550068628502, 7.301534541193676731, -99.99999999999997158 ) ) ;
#42235 = CARTESIAN_POINT ( 'NONE',  ( -9.999999999999998224, 1.224646799147353059E-15, -69.12500000409677625 ) ) ;
#42236 = CARTESIAN_POINT ( 'NONE',  ( 45.00000000000000711, 5.510910596163090344E-15, -203.0000000000000000 ) ) ;
#42237 = CARTESIAN_POINT ( 'NONE',  ( 7.644554776091147741E-16, 12.48450537969573659, -160.1562500020484094 ) ) ;
#42238 = CARTESIAN_POINT ( 'NONE',  ( -9.999999999999998224, 1.224646799147353059E-15, -13.62500000409674961 ) ) ;
#42239 = CYLINDRICAL_SURFACE ( 'NONE', #38444, 9.999999999999998224 ) ;
#42240 = CARTESIAN_POINT ( 'NONE',  ( -10.81189881249999729, 6.242252689847871849, -132.7187500020483810 ) ) ;
#42241 = CARTESIAN_POINT ( 'NONE',  ( -5.405949406249996869, 9.363379034771805109, -98.53125000204839523 ) ) ;
#42242 = CARTESIAN_POINT ( 'NONE',  ( 10.81189881249999729, 0.000000000000000000, -104.8437500020483810 ) ) ;
#42243 = CARTESIAN_POINT ( 'NONE',  ( -5.405949406250003975, -9.363379034771801557, -79.84375000204838102 ) ) ;
#42244 = CARTESIAN_POINT ( 'NONE',  ( -5.405949406249996869, 9.363379034771805109, -83.53125000204838102 ) ) ;
#42245 = CARTESIAN_POINT ( 'NONE',  ( -10.00000000000000000, -5.773502691896251982, -168.0000000040967905 ) ) ;
#42246 = CARTESIAN_POINT ( 'NONE',  ( -2.121150477449813534E-15, -11.54700538379251284, -66.87500000000000000 ) ) ;
#42247 = CARTESIAN_POINT ( 'NONE',  ( 7.644554776091147741E-16, 12.48450537969573659, -166.1562500020483810 ) ) ;
#42248 = CARTESIAN_POINT ( 'NONE',  ( -5.405949406249996869, 9.363379034771805109, -184.0312500020484094 ) ) ;
#42249 = CARTESIAN_POINT ( 'NONE',  ( -2.121150477449813534E-15, -11.54700538379251284, -158.7500000040968189 ) ) ;
#42250 = CARTESIAN_POINT ( 'NONE',  ( -10.81189881249999729, 1.324075727343319199E-15, -3.781250002048375247 ) ) ;
#42251 = CARTESIAN_POINT ( 'NONE',  ( -2.293366432827344421E-15, -12.48450537969573659, -3.218750002048353931 ) ) ;
#42252 = CARTESIAN_POINT ( 'NONE',  ( 9.999999999999998224, 0.000000000000000000, -200.0000000000000000 ) ) ;
#42253 = CARTESIAN_POINT ( 'NONE',  ( 10.81189881249999551, -6.242252689847874514, -112.4687500020483810 ) ) ;
#42254 = CARTESIAN_POINT ( 'NONE',  ( 5.000000000000000000, 8.660254037844385522, -90.24999999999998579 ) ) ;
#42255 = CARTESIAN_POINT ( 'NONE',  ( -2.293366432827344421E-15, -12.48450537969573659, -9.406250002048365033 ) ) ;
#42256 = CARTESIAN_POINT ( 'NONE',  ( 10.00000000000000000, 5.773502691896255534, -99.75000000409679046 ) ) ;
#42257 = DIRECTION ( 'NONE',  ( 1.000000000000000000, 0.000000000000000000, 0.000000000000000000 ) ) ;
#42258 = CARTESIAN_POINT ( 'NONE',  ( -10.81189881249999907, -6.242252689847864744, -107.1562500020483952 ) ) ;
#42259 = CARTESIAN_POINT ( 'NONE',  ( 5.405949406249992428, -9.363379034771808662, -90.28125000204838102 ) ) ;
#42260 = ORIENTED_EDGE ( 'NONE', *, *, #4814, .T. ) ;
#42261 = CARTESIAN_POINT ( 'NONE',  ( -10.00000000000000000, -5.773502691896251982, -87.00000000409677625 ) ) ;
#42262 = CARTESIAN_POINT ( 'NONE',  ( 5.000000000000000000, 8.660254037844385522, -4.749999999999976907 ) ) ;
#42263 = CARTESIAN_POINT ( 'NONE',  ( -10.81189881249999907, -6.242252689847864744, -42.46875000204835970 ) ) ;
#42264 = ORIENTED_EDGE ( 'NONE', *, *, #42543, .F. ) ;
#42265 = CARTESIAN_POINT ( 'NONE',  ( 4.999999999999992006, -8.660254037844389075, -20.24999999999996092 ) ) ;
#42266 = CARTESIAN_POINT ( 'NONE',  ( -4.999999999999996447, 8.660254037844387298, -157.5000000000000000 ) ) ;
#42267 = CARTESIAN_POINT ( 'NONE',  ( -9.999999999999998224, 1.224646799147353059E-15, -24.12500000409675849 ) ) ;
#42268 =( BOUNDED_CURVE ( )  B_SPLINE_CURVE ( 2, ( #35152, #28890, #9025, #26068, #29098, #25855, #42235 ),
 .UNSPECIFIED., .F., .F. ) 
 B_SPLINE_CURVE_WITH_KNOTS ( ( 3, 2, 2, 3 ),
 ( 0.6417910447761195902, 0.6430348258706469755, 0.6442786069651742498, 0.6455223880597016350 ),
 .UNSPECIFIED. ) 
 CURVE ( )  GEOMETRIC_REPRESENTATION_ITEM ( )  RATIONAL_B_SPLINE_CURVE ( ( 0.9999999999999761302, 0.8660254037844625774, 1.000000000000000000, 0.8660254037844387076, 1.000000000000000000, 0.8660254037844267172, 1.000000000000011990 ) ) 
 REPRESENTATION_ITEM ( '' )  );
#42269 = CARTESIAN_POINT ( 'NONE',  ( 7.070501591499377789E-16, 11.54700538379251284, -196.6250000000000284 ) ) ;
#42271 = ORIENTED_EDGE ( 'NONE', *, *, #21736, .T. ) ;
#42270 = CARTESIAN_POINT ( 'NONE',  ( -10.81189881249999729, 6.242252689847871849, -122.4062500020483952 ) ) ;
#42272 = CARTESIAN_POINT ( 'NONE',  ( 4.999999999999992006, -8.660254037844389075, -152.2500000000000000 ) ) ;
#42273 = EDGE_CURVE ( 'NONE', #13682, #20412, #31480, .T. ) ;
#42274 = EDGE_CURVE ( 'NONE', #31861, #13677, #1913, .T. ) ;
#42275 = ORIENTED_EDGE ( 'NONE', *, *, #10365, .F. ) ;
#42276 = ADVANCED_FACE ( 'NONE', ( #4285 ), #31052, .F. ) ;
#42277 = CARTESIAN_POINT ( 'NONE',  ( 10.81189881249999907, 6.242252689847868297, -53.90625000204838102 ) ) ;
#42278 = PERSON_AND_ORGANIZATION ( #11915, #17965 ) ;
#42279 = CARTESIAN_POINT ( 'NONE',  ( -10.81189881249999729, 1.324075727343319199E-15, -104.0937500020483810 ) ) ;
#42281 = VERTEX_POINT ( 'NONE', #7954 ) ;
#42280 = EDGE_LOOP ( 'NONE', ( #25899, #18354, #32779, #3699 ) ) ;
#42282 = DIRECTION ( 'NONE',  ( -0.000000000000000000, -0.000000000000000000, 1.000000000000000000 ) ) ;
#42283 = APPROVAL ( #15097, 'UNSPECIFIED' ) ;
#42284 = CARTESIAN_POINT ( 'NONE',  ( 9.999999999999998224, 0.000000000000000000, -33.49999999999997158 ) ) ;
#42285 = CARTESIAN_POINT ( 'NONE',  ( 5.405949406249999534, 9.363379034771803333, -184.2812500020484094 ) ) ;
#42286 = CARTESIAN_POINT ( 'NONE',  ( 9.999999999999998224, 0.000000000000000000, -176.0000000000000000 ) ) ;
#42287 = CARTESIAN_POINT ( 'NONE',  ( 9.999999999999994671, -5.773502691896262640, -132.6250000000000000 ) ) ;
#42288 = ADVANCED_FACE ( 'NONE', ( #34291 ), #40939, .T. ) ;
#42289 = CARTESIAN_POINT ( 'NONE',  ( 5.405949406249992428, -9.363379034771808662, -138.0937500020483810 ) ) ;
#42290 = CARTESIAN_POINT ( 'NONE',  ( -10.81189881249999729, 6.242252689847871849, -99.71875000204839523 ) ) ;
#42291 = FACE_BOUND ( 'NONE', #20203, .T. ) ;
#42292 = CARTESIAN_POINT ( 'NONE',  ( -10.81189881249999907, -6.242252689847864744, -110.1562500020483952 ) ) ;
#42293 = CARTESIAN_POINT ( 'NONE',  ( 5.000000000000000000, 8.660254037844385522, -192.6250000040967905 ) ) ;
#42294 = CARTESIAN_POINT ( 'NONE',  ( 10.81189881249999551, -6.242252689847874514, -121.4687500020484237 ) ) ;
#42295 = CARTESIAN_POINT ( 'NONE',  ( -10.81189881249999729, -6.242252689847864744, -189.6562500020484379 ) ) ;
#42296 = FACE_OUTER_BOUND ( 'NONE', #23725, .T. ) ;
#42297 = CARTESIAN_POINT ( 'NONE',  ( 9.999999999999998224, 0.000000000000000000, -138.5000000000000000 ) ) ;
#42298 = CARTESIAN_POINT ( 'NONE',  ( -10.00000000000000000, -5.773502691896251982, -5.624999999999963585 ) ) ;
#42299 = EDGE_CURVE ( 'NONE', #21209, #28518, #22612, .T. ) ;
#42300 = CARTESIAN_POINT ( 'NONE',  ( 7.644554776091147741E-16, 12.48450537969573659, -66.96875000204838102 ) ) ;
#42301 = CARTESIAN_POINT ( 'NONE',  ( 7.644554776091147741E-16, 12.48450537969573659, -47.46875000204836681 ) ) ;
#42302 = CARTESIAN_POINT ( 'NONE',  ( 4.999999999999992006, -8.660254037844389075, -181.1250000040967905 ) ) ;
#42303 = CARTESIAN_POINT ( 'NONE',  ( 5.405949406249992428, -9.363379034771808662, -28.78125000204837036 ) ) ;
#42304 = CARTESIAN_POINT ( 'NONE',  ( -10.81189881249999907, -6.242252689847864744, -31.96875000204834905 ) ) ;
#42305 = CARTESIAN_POINT ( 'NONE',  ( -5.000000000000003553, -8.660254037844383745, -107.8750000040967763 ) ) ;
#42306 = CARTESIAN_POINT ( 'NONE',  ( 5.405949406249992428, -9.363379034771808662, -139.5937500020483810 ) ) ;
#42307 = CARTESIAN_POINT ( 'NONE',  ( 9.999999999999998224, 0.000000000000000000, -117.5000000000000000 ) ) ;
#42308 = CARTESIAN_POINT ( 'NONE',  ( 7.070501591499376803E-16, 11.54700538379251284, -163.6250000000000284 ) ) ;
#42309 = CARTESIAN_POINT ( 'NONE',  ( -9.999999999999998224, 1.224646799147353059E-15, -67.24999999999997158 ) ) ;
#42310 = CARTESIAN_POINT ( 'NONE',  ( -10.81189881249999729, 6.242252689847871849, -132.9062500020483810 ) ) ;
#42311 = CARTESIAN_POINT ( 'NONE',  ( -5.405949406250003975, -9.363379034771801557, -119.0312500020483952 ) ) ;
#42312 = ORIENTED_EDGE ( 'NONE', *, *, #645, .T. ) ;
#42313 = CARTESIAN_POINT ( 'NONE',  ( 9.999999999999998224, 0.000000000000000000, -7.999999999999952038 ) ) ;
#42314 = CARTESIAN_POINT ( 'NONE',  ( -4.999999999999996447, 8.660254037844387298, -114.3750000040967763 ) ) ;
#42315 = CARTESIAN_POINT ( 'NONE',  ( 10.00000000000102318, -5.773502691895667560, -86.50000000409674783 ) ) ;
#42316 = CARTESIAN_POINT ( 'NONE',  ( -10.81189881249999729, 6.242252689847871849, -62.21875000204838102 ) ) ;
#42317 = CARTESIAN_POINT ( 'NONE',  ( -2.121150477449813534E-15, -11.54700538379251284, -42.87499999999997868 ) ) ;
#42318 = CARTESIAN_POINT ( 'NONE',  ( -4.999999999999996447, 8.660254037844387298, -18.37500000409675494 ) ) ;
#42319 = CARTESIAN_POINT ( 'NONE',  ( -2.293366432827344421E-15, -12.48450537969573659, -43.90625000204838102 ) ) ;
#42320 = EDGE_CURVE ( 'NONE', #41736, #31697, #2220, .T. ) ;
#42321 = CARTESIAN_POINT ( 'NONE',  ( 9.999999999998456346, 5.773502691897149042, -16.87499999999993250 ) ) ;
#42322 = CARTESIAN_POINT ( 'NONE',  ( -4.999999999999996447, 8.660254037844387298, -46.87500000409677625 ) ) ;
#42323 = CARTESIAN_POINT ( 'NONE',  ( 7.644554776091147741E-16, 12.48450537969573659, -32.65625000204835970 ) ) ;
#42324 = DIRECTION ( 'NONE',  ( -0.000000000000000000, -0.000000000000000000, 1.000000000000000000 ) ) ;
#42325 = CARTESIAN_POINT ( 'NONE',  ( 7.644554776091147741E-16, 12.48450537969573659, -140.6562500020484094 ) ) ;
#42326 = CARTESIAN_POINT ( 'NONE',  ( 5.405949406249999534, 9.363379034771803333, -146.7812500020483810 ) ) ;
#42327 = FACE_OUTER_BOUND ( 'NONE', #37892, .T. ) ;
#42328 = ORIENTED_EDGE ( 'NONE', *, *, #30246, .T. ) ;
#42329 = ORIENTED_EDGE ( 'NONE', *, *, #2100, .T. ) ;
#42330 = ORIENTED_EDGE ( 'NONE', *, *, #20300, .T. ) ;
#42331 = CARTESIAN_POINT ( 'NONE',  ( 9.999999999999998224, 0.000000000000000000, -108.8750000040967763 ) ) ;
#42332 = CARTESIAN_POINT ( 'NONE',  ( -10.81189881249999729, 6.242252689847871849, -176.2187500020483810 ) ) ;
#42334 = EDGE_CURVE ( 'NONE', #28132, #1053, #25844, .T. ) ;
#42333 = CARTESIAN_POINT ( 'NONE',  ( -10.81189881249999729, 6.242252689847871849, -23.21875000204836326 ) ) ;
#42335 = CARTESIAN_POINT ( 'NONE',  ( 10.00000000000025402, -5.773502691896113426, -128.5000000040967905 ) ) ;
#42336 = CARTESIAN_POINT ( 'NONE',  ( 10.81189881249999551, -6.242252689847874514, -167.9687500020483810 ) ) ;
#42337 = CARTESIAN_POINT ( 'NONE',  ( 10.81189881249999907, 6.242252689847868297, -146.7187500020484094 ) ) ;
#42338 = CARTESIAN_POINT ( 'NONE',  ( -9.999999999999998224, 1.224646799147353059E-15, -100.2499999999999858 ) ) ;
#42339 = CARTESIAN_POINT ( 'NONE',  ( 5.405949406249992428, -9.363379034771808662, -127.5937500020483668 ) ) ;
#42340 = CARTESIAN_POINT ( 'NONE',  ( 10.81189881249999907, 6.242252689847868297, -133.4062500020483810 ) ) ;
#42341 = CARTESIAN_POINT ( 'NONE',  ( -5.405949406249996869, 9.363379034771805109, -18.84375000204835260 ) ) ;
#42342 = CARTESIAN_POINT ( 'NONE',  ( -10.81189881249999729, -6.242252689847864744, -145.9687500020484094 ) ) ;
#42343 = CARTESIAN_POINT ( 'NONE',  ( 10.01657826025561704, -4.085534667769917583, -180.0000000000000284 ) ) ;
#42344 = CARTESIAN_POINT ( 'NONE',  ( -10.00000000000154188, 5.773502691895366468, -25.37499999999993605 ) ) ;
#42345 = CARTESIAN_POINT ( 'NONE',  ( 5.000000000000000000, 8.660254037844385522, -165.2500000000000000 ) ) ;
#42346 = CARTESIAN_POINT ( 'NONE',  ( -9.999999999999998224, 1.224646799147353059E-15, -55.62500000409676204 ) ) ;
#42347 = CARTESIAN_POINT ( 'NONE',  ( -5.405949406250003975, -9.363379034771801557, -73.84375000204838102 ) ) ;
#42348 = CARTESIAN_POINT ( 'NONE',  ( -2.293366432827344421E-15, -12.48450537969573659, -48.40625000204837391 ) ) ;
#42349 = CARTESIAN_POINT ( 'NONE',  ( 10.81189881249999907, 6.242252689847868297, -55.21875000204836681 ) ) ;
#42350 = LINE ( 'NONE', #16434, #26793 ) ;
#42351 = CARTESIAN_POINT ( 'NONE',  ( 10.81189881249999907, 6.242252689847868297, -158.7187500020483810 ) ) ;
#42352 = CARTESIAN_POINT ( 'NONE',  ( -9.999999999999998224, 5.773502691896259087, -136.3750000000000000 ) ) ;
#42353 = CARTESIAN_POINT ( 'NONE',  ( 5.405949406249999534, 9.363379034771803333, -146.7812500020483810 ) ) ;
#42354 = DIRECTION ( 'NONE',  ( -0.000000000000000000, -0.000000000000000000, 1.000000000000000000 ) ) ;
#42355 = CARTESIAN_POINT ( 'NONE',  ( 5.000000000000000000, 8.660254037844385522, -111.6250000040967763 ) ) ;
#42356 = CARTESIAN_POINT ( 'NONE',  ( -2.121150477449813534E-15, -11.54700538379251284, -89.37499999999997158 ) ) ;
#42357 = ORIENTED_EDGE ( 'NONE', *, *, #27427, .F. ) ;
#42358 = CARTESIAN_POINT ( 'NONE',  ( 10.81189881249999551, -6.242252689847874514, -120.1562500020483952 ) ) ;
#42359 = CARTESIAN_POINT ( 'NONE',  ( 4.999999999999992006, -8.660254037844389075, -139.1250000040967905 ) ) ;
#42360 = CARTESIAN_POINT ( 'NONE',  ( -9.999999999999479527, -5.773502691896549521, -49.12499999999995737 ) ) ;
#42361 = CARTESIAN_POINT ( 'NONE',  ( 10.81189881249999907, 6.242252689847868297, -175.4062500020484094 ) ) ;
#42362 = CARTESIAN_POINT ( 'NONE',  ( -2.121150477449813534E-15, -11.54700538379251284, -47.75000000409676204 ) ) ;
#42363 = LINE ( 'NONE', #3318, #31125 ) ;
#42364 = CARTESIAN_POINT ( 'NONE',  ( 7.644554776091147741E-16, 12.48450537969573659, -58.15625000204838102 ) ) ;
#42365 = VECTOR ( 'NONE', #34223, 1000.000000000000000 ) ;
#42366 = CARTESIAN_POINT ( 'NONE',  ( 9.999999999999998224, 0.000000000000000000, -76.99999999999998579 ) ) ;
#42367 = CARTESIAN_POINT ( 'NONE',  ( -5.405949406249996869, 9.363379034771805109, -163.0312500020484094 ) ) ;
#42368 = CARTESIAN_POINT ( 'NONE',  ( 5.405949406249999534, 9.363379034771803333, -140.5937500020483810 ) ) ;
#42369 = CARTESIAN_POINT ( 'NONE',  ( 9.999999999999479527, 5.773502691896553074, -100.8749999999999716 ) ) ;
#42370 = CYLINDRICAL_SURFACE ( 'NONE', #22711, 9.999999999999998224 ) ;
#42371 = ORIENTED_EDGE ( 'NONE', *, *, #38942, .F. ) ;
#42372 = CARTESIAN_POINT ( 'NONE',  ( 0.000000000000000000, 0.000000000000000000, -200.0000000000000000 ) ) ;
#42374 = ORIENTED_EDGE ( 'NONE', *, *, #37263, .F. ) ;
#42373 = CARTESIAN_POINT ( 'NONE',  ( 5.405949406249992428, -9.363379034771808662, -72.28125000204838102 ) ) ;
#42375 = APPROVAL_STATUS ( 'not_yet_approved' ) ;
#42377 = VERTEX_POINT ( 'NONE', #31698 ) ;
#42376 = CARTESIAN_POINT ( 'NONE',  ( -10.81189881249999729, 1.324075727343319199E-15, -122.0937500020483952 ) ) ;
#42378 = ORIENTED_EDGE ( 'NONE', *, *, #36968, .F. ) ;
#42379 = AXIS2_PLACEMENT_3D ( 'NONE', #38065, #11075, #31390 ) ;
#42380 =( BOUNDED_CURVE ( )  B_SPLINE_CURVE ( 2, ( #20141, #13643, #26835, #39987, #7192, #34604, #11270 ),
 .UNSPECIFIED., .F., .F. ) 
 B_SPLINE_CURVE_WITH_KNOTS ( ( 3, 2, 2, 3 ),
 ( 0.2388059701492538378, 0.2400497512437811953, 0.2412935323383085806, 0.2425373134328359381 ),
 .UNSPECIFIED. ) 
 CURVE ( )  GEOMETRIC_REPRESENTATION_ITEM ( )  RATIONAL_B_SPLINE_CURVE ( ( 0.9999999999999880096, 0.8660254037844506980, 1.000000000000000000, 0.8660254037844387076, 1.000000000000000000, 0.8660254037844267172, 1.000000000000011990 ) ) 
 REPRESENTATION_ITEM ( '' )  );
#42381 = CARTESIAN_POINT ( 'NONE',  ( 5.405949406249999534, 9.363379034771803333, -32.59375000204836681 ) ) ;
#42382 = FACE_OUTER_BOUND ( 'NONE', #2049, .T. ) ;
#42383 = CARTESIAN_POINT ( 'NONE',  ( 10.81189881249999551, -6.242252689847874514, -0.1562500020483646446 ) ) ;
#42385 = EDGE_CURVE ( 'NONE', #29474, #5068, #11007, .T. ) ;
#42384 = CARTESIAN_POINT ( 'NONE',  ( -10.81189881249999729, 6.242252689847871849, -56.21875000204837391 ) ) ;
#42386 = DIRECTION ( 'NONE',  ( 0.000000000000000000, 0.000000000000000000, -1.000000000000000000 ) ) ;
#42387 = CARTESIAN_POINT ( 'NONE',  ( -10.00000000000000000, -5.773502691896251982, -31.12499999999995737 ) ) ;
#42388 = CARTESIAN_POINT ( 'NONE',  ( 5.405949406249999534, 9.363379034771803333, -185.5937500020483810 ) ) ;
#42389 = CARTESIAN_POINT ( 'NONE',  ( -10.81189881249999729, 1.324075727343319199E-15, -170.0937500020484094 ) ) ;
#42390 = CARTESIAN_POINT ( 'NONE',  ( -10.81189881249999729, 6.242252689847871849, -147.7187500020484094 ) ) ;
#42391 = CARTESIAN_POINT ( 'NONE',  ( -5.405949406250003975, -9.363379034771801557, -172.8437500020484094 ) ) ;
#42392 = CARTESIAN_POINT ( 'NONE',  ( -10.00000000000051337, 5.773502691895962435, -123.2500000040967763 ) ) ;
#42393 = VECTOR ( 'NONE', #26975, 1000.000000000000000 ) ;
#42394 = CYLINDRICAL_SURFACE ( 'NONE', #39147, 9.999999999999998224 ) ;
#42395 = CARTESIAN_POINT ( 'NONE',  ( -4.999999999999996447, 8.660254037844387298, -190.5000000000000000 ) ) ;
#42396 = CARTESIAN_POINT ( 'NONE',  ( 5.405949406249992428, -9.363379034771808662, -94.59375000204838102 ) ) ;
#42397 = CARTESIAN_POINT ( 'NONE',  ( 9.999999999999998224, 0.000000000000000000, -47.37500000409677625 ) ) ;
#42398 = CARTESIAN_POINT ( 'NONE',  ( -10.81189881249999729, 6.242252689847871849, -74.40625000204836681 ) ) ;
#42399 = CARTESIAN_POINT ( 'NONE',  ( -2.121150477449813534E-15, -11.54700538379251284, -131.7500000040967905 ) ) ;
#42400 = CARTESIAN_POINT ( 'NONE',  ( 10.81189881249999907, 6.242252689847868297, -197.7187500020484094 ) ) ;
#42401 = CARTESIAN_POINT ( 'NONE',  ( 10.81189881249999729, 6.242252689847867408, -85.21875000204836681 ) ) ;
#42402 = CARTESIAN_POINT ( 'NONE',  ( 5.405949406249999534, 9.363379034771803333, -56.78125000204836681 ) ) ;
#42403 = CARTESIAN_POINT ( 'NONE',  ( -2.121150477449813534E-15, -11.54700538379251284, -148.2500000040968189 ) ) ;
#42404 = CARTESIAN_POINT ( 'NONE',  ( 9.999999999999998224, 0.000000000000000000, -117.5000000000000000 ) ) ;
#42405 = EDGE_CURVE ( 'NONE', #14673, #11901, #27019, .T. ) ;
#42406 = ORIENTED_EDGE ( 'NONE', *, *, #12220, .F. ) ;
#42407 = CARTESIAN_POINT ( 'NONE',  ( 10.81189881249999729, 6.242252689847867408, -140.9062500020484094 ) ) ;
#42408 = CARTESIAN_POINT ( 'NONE',  ( 10.81189881249999551, -6.242252689847874514, -153.1562500020484379 ) ) ;
#42409 = CARTESIAN_POINT ( 'NONE',  ( -1.040834085586084257E-14, 145.0000000000000000, 2.499999999999992006 ) ) ;
#42410 = LINE ( 'NONE', #6394, #27515 ) ;
#42411 = CARTESIAN_POINT ( 'NONE',  ( -10.81189881249999729, 1.324075727343319199E-15, -89.09375000204838102 ) ) ;
#42412 = ORIENTED_EDGE ( 'NONE', *, *, #42224, .T. ) ;
#42413 = CARTESIAN_POINT ( 'NONE',  ( -9.999999999999998224, 1.224646799147353059E-15, -61.24999999999997158 ) ) ;
#42414 = CARTESIAN_POINT ( 'NONE',  ( 5.405949406249992428, -9.363379034771808662, -189.0937500020483810 ) ) ;
#42415 = CARTESIAN_POINT ( 'NONE',  ( -2.121150477449813534E-15, -11.54700538379251284, -71.75000000409674783 ) ) ;
#42416 = CARTESIAN_POINT ( 'NONE',  ( 9.999999999999998224, 1.224646799147353059E-15, -99.99999999999998579 ) ) ;
#42417 = CARTESIAN_POINT ( 'NONE',  ( 9.999999999999998224, 0.000000000000000000, -12.87500000409674783 ) ) ;
#42418 = CARTESIAN_POINT ( 'NONE',  ( -10.81189881249999729, 1.324075727343319199E-15, -86.28125000204838102 ) ) ;
#42419 = CARTESIAN_POINT ( 'NONE',  ( 5.405949406249992428, -9.363379034771808662, -70.78125000204838102 ) ) ;
#42420 = VECTOR ( 'NONE', #30996, 1000.000000000000000 ) ;
#42421 = CARTESIAN_POINT ( 'NONE',  ( 7.070501591499377789E-16, 11.54700538379251284, -63.50000000409677625 ) ) ;
#42422 = CARTESIAN_POINT ( 'NONE',  ( -10.81189881249999729, 1.324075727343319199E-15, -21.59375000204835615 ) ) ;
#42423 = CARTESIAN_POINT ( 'NONE',  ( 0.000000000000000000, 0.000000000000000000, -200.0000000000000000 ) ) ;
#42424 = CARTESIAN_POINT ( 'NONE',  ( 5.405949406249992428, -9.363379034771808662, -181.7812500020483810 ) ) ;
#42425 = CARTESIAN_POINT ( 'NONE',  ( 7.644554776091147741E-16, 12.48450537969573659, -10.15625000204836681 ) ) ;
#42426 = FACE_OUTER_BOUND ( 'NONE', #37129, .T. ) ;
#42427 = CARTESIAN_POINT ( 'NONE',  ( -1.040834085586084257E-14, 139.9999999999999716, 22.49999999999999289 ) ) ;
#42428 = CARTESIAN_POINT ( 'NONE',  ( -9.999999999999998224, 1.224646799147353059E-15, -28.62500000409676204 ) ) ;
#42429 = CARTESIAN_POINT ( 'NONE',  ( -9.999999999999998224, 1.224646799147353059E-15, -200.0000000000000000 ) ) ;
#42430 = CARTESIAN_POINT ( 'NONE',  ( 9.999999999999998224, 0.000000000000000000, -176.0000000000000000 ) ) ;
#42431 = CARTESIAN_POINT ( 'NONE',  ( -9.999999999999996447, 5.773502691896259975, -166.3750000000000000 ) ) ;
#42433 = ORIENTED_EDGE ( 'NONE', *, *, #19089, .F. ) ;
#42432 = CARTESIAN_POINT ( 'NONE',  ( -5.405949406250003975, -9.363379034771801557, -96.53125000204839523 ) ) ;
#42434 = EDGE_CURVE ( 'NONE', #40786, #17582, #3589, .T. ) ;
#42435 = CARTESIAN_POINT ( 'NONE',  ( 9.999999999999742428, 5.773502691896404748, -116.2500000040967620 ) ) ;
#42436 = ORIENTED_EDGE ( 'NONE', *, *, #2377, .T. ) ;
#42437 = VERTEX_POINT ( 'NONE', #12236 ) ;
#42438 = ADVANCED_FACE ( 'NONE', ( #19145 ), #25429, .T. ) ;
#42439 = CARTESIAN_POINT ( 'NONE',  ( -10.81189881249999729, 6.242252689847871849, -35.21875000204835260 ) ) ;
#42440 = CARTESIAN_POINT ( 'NONE',  ( 7.644554776091147741E-16, 12.48450537969573659, -32.65625000204835970 ) ) ;
#42441 = PERSON_AND_ORGANIZATION_ROLE ( 'classification_officer' ) ;
#42442 = CARTESIAN_POINT ( 'NONE',  ( -2.293366432827344421E-15, -12.48450537969573659, -82.71875000204838102 ) ) ;
#42443 = FACE_OUTER_BOUND ( 'NONE', #4390, .T. ) ;
#42444 = CARTESIAN_POINT ( 'NONE',  ( 5.405949406249999534, 9.363379034771803333, -193.0937500020484094 ) ) ;
#42445 = VECTOR ( 'NONE', #12087, 1000.000000000000000 ) ;
#42446 = DIRECTION ( 'NONE',  ( -1.734723475976807094E-16, -1.000000000000000000, -0.000000000000000000 ) ) ;
#42447 = CARTESIAN_POINT ( 'NONE',  ( -9.999999999999479527, -5.773502691896549521, -144.0000000040967620 ) ) ;
#42448 = CARTESIAN_POINT ( 'NONE',  ( 10.81189881249999907, 6.242252689847868297, -160.4062500020484094 ) ) ;
#42449 = CARTESIAN_POINT ( 'NONE',  ( -10.00000000000000000, -5.773502691896251982, -12.00000000409676915 ) ) ;
#42450 = CARTESIAN_POINT ( 'NONE',  ( 9.999999999999998224, 0.000000000000000000, -79.99999999999998579 ) ) ;
#42451 = CARTESIAN_POINT ( 'NONE',  ( 10.81189881249999551, -6.242252689847874514, -130.4687500020483810 ) ) ;
#42452 = CARTESIAN_POINT ( 'NONE',  ( -10.81189881249999907, -6.242252689847864744, -99.65625000204839523 ) ) ;
#42453 = CARTESIAN_POINT ( 'NONE',  ( -5.405949406249996869, 9.363379034771805109, -105.8437500020483810 ) ) ;
#42454 = CARTESIAN_POINT ( 'NONE',  ( -2.293366432827344421E-15, -12.48450537969573659, -81.21875000204838102 ) ) ;
#42455 = CARTESIAN_POINT ( 'NONE',  ( 5.405949406249992428, -9.363379034771808662, -85.78125000204838102 ) ) ;
#42456 = CARTESIAN_POINT ( 'NONE',  ( 9.999999999999998224, 0.000000000000000000, -173.3750000040968189 ) ) ;
#42457 = CARTESIAN_POINT ( 'NONE',  ( -9.999999999999998224, 1.224646799147353059E-15, -45.12500000409677625 ) ) ;
#42458 = CARTESIAN_POINT ( 'NONE',  ( 10.81189881249999551, -6.242252689847874514, -166.6562500020484094 ) ) ;
#42459 = CARTESIAN_POINT ( 'NONE',  ( 5.405949406249992428, -9.363379034771808662, -183.2812500020484094 ) ) ;
#42460 = CARTESIAN_POINT ( 'NONE',  ( -10.00000000000000000, -5.773502691896251982, -154.5000000040967905 ) ) ;
#42461 = DIRECTION ( 'NONE',  ( -0.000000000000000000, -0.000000000000000000, -1.000000000000000000 ) ) ;
#42462 = CARTESIAN_POINT ( 'NONE',  ( 5.405949406249992428, -9.363379034771808662, -6.093750002048370362 ) ) ;
#42463 = CARTESIAN_POINT ( 'NONE',  ( -5.405949406249996869, 9.363379034771805109, -116.3437500020483810 ) ) ;
#42464 = ADVANCED_FACE ( 'NONE', ( #9015 ), #12028, .T. ) ;
#42465 = CARTESIAN_POINT ( 'NONE',  ( -10.00000000000000000, -5.773502691896251982, -82.12499999999998579 ) ) ;
#42466 = CARTESIAN_POINT ( 'NONE',  ( 10.81189881249999729, 0.000000000000000000, -16.53125000204835970 ) ) ;
#42467 = CARTESIAN_POINT ( 'NONE',  ( -2.121150477449813534E-15, -11.54700538379251284, -98.75000000409677625 ) ) ;
#42468 = CARTESIAN_POINT ( 'NONE',  ( 5.500000000000003553, 20.00000000000000000, -232.0000000000000000 ) ) ;
#42469 = CARTESIAN_POINT ( 'NONE',  ( -10.81189881249999907, -6.242252689847864744, -110.1562500020483952 ) ) ;
#42470 = CARTESIAN_POINT ( 'NONE',  ( 10.81189881249999551, -6.242252689847874514, -91.65625000204838102 ) ) ;
#42471 = ORIENTED_EDGE ( 'NONE', *, *, #7221, .F. ) ;
#42472 = CARTESIAN_POINT ( 'NONE',  ( 9.999999999999996447, -5.773502691896262640, -88.00000000409677625 ) ) ;
#42473 = CARTESIAN_POINT ( 'NONE',  ( 5.405949406249999534, 9.363379034771803333, -38.59375000204837391 ) ) ;
#42474 = ORIENTED_EDGE ( 'NONE', *, *, #3634, .T. ) ;
#42475 = CARTESIAN_POINT ( 'NONE',  ( -9.999999999999998224, 5.773502691896259087, -14.87499999999997335 ) ) ;
#42476 = CARTESIAN_POINT ( 'NONE',  ( 7.070501591499377789E-16, 11.54700538379251284, -151.6250000000000000 ) ) ;
#42477 =( BOUNDED_CURVE ( )  B_SPLINE_CURVE ( 2, ( #19246, #22709, #36080, #35876, #32644, #3071, #16197 ),
 .UNSPECIFIED., .F., .F. ) 
 B_SPLINE_CURVE_WITH_KNOTS ( ( 3, 2, 2, 3 ),
 ( 0.2388059701492538378, 0.2400497512437811953, 0.2412935323383085806, 0.2425373134328359381 ),
 .UNSPECIFIED. ) 
 CURVE ( )  GEOMETRIC_REPRESENTATION_ITEM ( )  RATIONAL_B_SPLINE_CURVE ( ( 0.9999999999999880096, 0.8660254037844506980, 1.000000000000000000, 0.8660254037844387076, 1.000000000000000000, 0.8660254037844267172, 1.000000000000011990 ) ) 
 REPRESENTATION_ITEM ( '' )  );
#42478 = CARTESIAN_POINT ( 'NONE',  ( 7.070501591499377789E-16, 11.54700538379251284, -9.500000004096758488 ) ) ;
#42479 = VECTOR ( 'NONE', #24335, 1000.000000000000000 ) ;
#42480 = CARTESIAN_POINT ( 'NONE',  ( -9.999999999999742428, -5.773502691896402084, -120.0000000040967905 ) ) ;
#42482 = VERTEX_POINT ( 'NONE', #2552 ) ;
#42481 = CARTESIAN_POINT ( 'NONE',  ( -5.405949406250003975, -9.363379034771801557, -120.5312500020483952 ) ) ;
#42483 = CARTESIAN_POINT ( 'NONE',  ( -9.999999999999998224, 1.224646799147353059E-15, -117.1250000040967905 ) ) ;
#42484 = ORIENTED_EDGE ( 'NONE', *, *, #31256, .T. ) ;
#42485 = CARTESIAN_POINT ( 'NONE',  ( 10.81189881249999551, -6.242252689847874514, -52.65625000204837391 ) ) ;
#42486 = COORDINATED_UNIVERSAL_TIME_OFFSET ( 6, 0, .AHEAD. ) ;
#42487 = CARTESIAN_POINT ( 'NONE',  ( -5.405949406249996869, 9.363379034771805109, -99.84375000204838102 ) ) ;
#42488 = ORIENTED_EDGE ( 'NONE', *, *, #25736, .F. ) ;
#42489 = CARTESIAN_POINT ( 'NONE',  ( 7.070501591499376803E-16, 11.54700538379251284, -175.6250000000000000 ) ) ;
#42490 = CARTESIAN_POINT ( 'NONE',  ( 9.999999999999998224, 0.000000000000000000, -78.49999999999998579 ) ) ;
#42491 = CARTESIAN_POINT ( 'NONE',  ( 5.405949406249999534, 9.363379034771803333, -176.7812500020484094 ) ) ;
#42492 = CARTESIAN_POINT ( 'NONE',  ( -10.81189881249999907, -6.242252689847864744, -0.4687500020483501006 ) ) ;
#42493 = FACE_OUTER_BOUND ( 'NONE', #27696, .T. ) ;
#42494 = CARTESIAN_POINT ( 'NONE',  ( 10.81189881249999729, 0.000000000000000000, -133.3437500020484094 ) ) ;
#42495 = CARTESIAN_POINT ( 'NONE',  ( -10.81189881249999907, -6.242252689847864744, -103.9687500020483668 ) ) ;
#42496 = CARTESIAN_POINT ( 'NONE',  ( 10.00000000000051159, -5.773502691895965988, -143.1250000000000000 ) ) ;
#42497 = CARTESIAN_POINT ( 'NONE',  ( 10.81189881249999907, 6.242252689847868297, -110.9062500020483952 ) ) ;
#42498 = CARTESIAN_POINT ( 'NONE',  ( 10.00000000000000000, 5.773502691896255534, -197.2500000040968189 ) ) ;
#42499 = CARTESIAN_POINT ( 'NONE',  ( -5.405949406250003975, -9.363379034771801557, -117.3437500020483810 ) ) ;
#42500 = CARTESIAN_POINT ( 'NONE',  ( -5.405949406250003975, -9.363379034771801557, -185.0312500020484094 ) ) ;
#42501 = CARTESIAN_POINT ( 'NONE',  ( 10.00000000000031619, -5.773502691896077010, -185.5000000040967905 ) ) ;
#42502 = CARTESIAN_POINT ( 'NONE',  ( 7.070501591499377789E-16, 11.54700538379251284, -139.6250000000000000 ) ) ;
#42503 = CARTESIAN_POINT ( 'NONE',  ( 4.999999999999992006, -8.660254037844389075, -3.749999999999975575 ) ) ;
#42504 = EDGE_CURVE ( 'NONE', #34637, #36657, #33076, .T. ) ;
#42505 = CARTESIAN_POINT ( 'NONE',  ( -10.81189881249999729, -6.242252689847864744, -61.96875000204838813 ) ) ;
#42506 = CARTESIAN_POINT ( 'NONE',  ( 7.644554776091147741E-16, 12.48450537969573659, -48.96875000204835970 ) ) ;
#42507 = DESIGN_CONTEXT ( 'detailed design', #844, 'design' ) ;
#42508 = CARTESIAN_POINT ( 'NONE',  ( -9.999999999999998224, 1.224646799147353059E-15, -183.1250000040967905 ) ) ;
#42509 = CARTESIAN_POINT ( 'NONE',  ( -2.293366432827344421E-15, -12.48450537969573659, -15.40625000204837391 ) ) ;
#42510 = CARTESIAN_POINT ( 'NONE',  ( 10.81189881249999729, 0.000000000000000000, -26.84375000204835970 ) ) ;
#42511 = CARTESIAN_POINT ( 'NONE',  ( -5.000000000000003553, -8.660254037844383745, -105.9999999999999858 ) ) ;
#42512 = CARTESIAN_POINT ( 'NONE',  ( 7.644554776091147741E-16, 12.48450537969573659, -141.9687500020483810 ) ) ;
#42513 = EDGE_CURVE ( 'NONE', #41090, #28241, #9435, .T. ) ;
#42514 = CARTESIAN_POINT ( 'NONE',  ( 9.999999999999996447, -5.773502691896262640, -111.6249999999999858 ) ) ;
#42515 = CARTESIAN_POINT ( 'NONE',  ( 10.00000000000051159, -5.773502691895965988, -147.6249999999999716 ) ) ;
#42516 = EDGE_CURVE ( 'NONE', #15509, #31308, #15411, .T. ) ;
#42517 = CARTESIAN_POINT ( 'NONE',  ( -9.999999999999998224, 5.773502691896259087, -64.37499999999998579 ) ) ;
#42518 = CARTESIAN_POINT ( 'NONE',  ( 10.81189881249999551, -6.242252689847874514, -132.1562500020484094 ) ) ;
#42519 = CARTESIAN_POINT ( 'NONE',  ( -10.81189881249999729, 1.324075727343319199E-15, -114.7812500020483952 ) ) ;
#42520 = ORIENTED_EDGE ( 'NONE', *, *, #2395, .F. ) ;
#42521 =( BOUNDED_CURVE ( )  B_SPLINE_CURVE ( 2, ( #7464, #37025, #37229, #4437, #36812, #4012, #10473 ),
 .UNSPECIFIED., .F., .F. ) 
 B_SPLINE_CURVE_WITH_KNOTS ( ( 3, 2, 2, 3 ),
 ( 0.5485074626865672487, 0.5497512437810946340, 0.5509950248756221303, 0.5522388059701495155 ),
 .UNSPECIFIED. ) 
 CURVE ( )  GEOMETRIC_REPRESENTATION_ITEM ( )  RATIONAL_B_SPLINE_CURVE ( ( 0.9999999999999880096, 0.8660254037844506980, 1.000000000000000000, 0.8660254037844387076, 1.000000000000000000, 0.8660254037844148378, 1.000000000000023981 ) ) 
 REPRESENTATION_ITEM ( '' )  );
#42522 = CARTESIAN_POINT ( 'NONE',  ( -9.999999999999998224, 1.224646799147353059E-15, -196.6250000040967905 ) ) ;
#42523 = CARTESIAN_POINT ( 'NONE',  ( -2.121150477449813534E-15, -11.54700538379251284, -106.2500000040967763 ) ) ;
#42524 = CARTESIAN_POINT ( 'NONE',  ( 0.000000000000000000, 0.000000000000000000, -200.0000000000000000 ) ) ;
#42525 = CARTESIAN_POINT ( 'NONE',  ( 10.81189881249999729, 0.000000000000000000, -68.84375000204836681 ) ) ;
#42526 = EDGE_LOOP ( 'NONE', ( #38212, #17302, #4494, #21598 ) ) ;
#42527 = CARTESIAN_POINT ( 'NONE',  ( 10.00000000000000000, 5.773502691896255534, -40.87499999999997158 ) ) ;
#42528 = CARTESIAN_POINT ( 'NONE',  ( 9.999999999999998224, 0.000000000000000000, -17.37500000409675138 ) ) ;
#42529 = CARTESIAN_POINT ( 'NONE',  ( 10.81189881249999729, 0.000000000000000000, -45.03125000204838102 ) ) ;
#42530 = CARTESIAN_POINT ( 'NONE',  ( 7.070501591499376803E-16, 11.54700538379251284, -16.62499999999996447 ) ) ;
#42531 = CARTESIAN_POINT ( 'NONE',  ( 5.000000000000000000, 8.660254037844385522, -35.12500000409676915 ) ) ;
#42532 = CARTESIAN_POINT ( 'NONE',  ( 5.405949406249999534, 9.363379034771803333, -38.78125000204838102 ) ) ;
#42533 =( BOUNDED_CURVE ( )  B_SPLINE_CURVE ( 2, ( #35681, #21867, #42129, #2451, #29198, #38908, #12348 ),
 .UNSPECIFIED., .F., .F. ) 
 B_SPLINE_CURVE_WITH_KNOTS ( ( 3, 2, 2, 3 ),
 ( 0.1156716417910447492, 0.1169154228855721483, 0.1181592039800995753, 0.1194029850746269744 ),
 .UNSPECIFIED. ) 
 CURVE ( )  GEOMETRIC_REPRESENTATION_ITEM ( )  RATIONAL_B_SPLINE_CURVE ( ( 1.000000000000003109, 0.8660254037844358210, 1.000000000000000000, 0.8660254037844387076, 1.000000000000000000, 0.8660254037844267172, 1.000000000000011990 ) ) 
 REPRESENTATION_ITEM ( '' )  );
#42534 = DIRECTION ( 'NONE',  ( -0.000000000000000000, -0.000000000000000000, 1.000000000000000000 ) ) ;
#42535 = CARTESIAN_POINT ( 'NONE',  ( 10.81189881249999729, 0.000000000000000000, -136.5312500020484094 ) ) ;
#42536 = CARTESIAN_POINT ( 'NONE',  ( -2.293366432827344421E-15, -12.48450537969573659, -153.4062500020483810 ) ) ;
#42537 = EDGE_CURVE ( 'NONE', #14343, #14344, #19824, .T. ) ;
#42538 = CARTESIAN_POINT ( 'NONE',  ( 9.999999999999998224, 0.000000000000000000, -192.5000000000000000 ) ) ;
#42539 = ORIENTED_EDGE ( 'NONE', *, *, #27350, .F. ) ;
#42540 = ORIENTED_EDGE ( 'NONE', *, *, #10106, .F. ) ;
#42541 = ADVANCED_FACE ( 'NONE', ( #26267 ), #792, .T. ) ;
#42542 = EDGE_LOOP ( 'NONE', ( #22392, #37837, #20927, #7845 ) ) ;
#42543 = EDGE_CURVE ( 'NONE', #7196, #31273, #36181, .T. ) ;
#42544 = LINE ( 'NONE', #23135, #33203 ) ;
#42545 = CARTESIAN_POINT ( 'NONE',  ( -10.81189881249999907, -6.242252689847864744, -175.9687500020483526 ) ) ;
#42546 = CARTESIAN_POINT ( 'NONE',  ( -2.293366432827344421E-15, -12.48450537969573659, -22.71875000204837747 ) ) ;
#42547 = CARTESIAN_POINT ( 'NONE',  ( -9.999999999999998224, 1.224646799147353059E-15, -103.2500000000000000 ) ) ;
#42548 = CARTESIAN_POINT ( 'NONE',  ( -5.405949406249996869, 9.363379034771805109, -155.3437500020483810 ) ) ;
#42549 = CARTESIAN_POINT ( 'NONE',  ( 7.644554776091147741E-16, 12.48450537969573659, -144.9687500020483810 ) ) ;
#42550 = CARTESIAN_POINT ( 'NONE',  ( 9.999999999999998224, 0.000000000000000000, -119.0000000000000000 ) ) ;
#42551 = CARTESIAN_POINT ( 'NONE',  ( 10.81189881249999551, -6.242252689847874514, -125.9687500020483810 ) ) ;
#42552 = CARTESIAN_POINT ( 'NONE',  ( -5.405949406250003975, -9.363379034771801557, -129.5312500020484094 ) ) ;
#42553 = CARTESIAN_POINT ( 'NONE',  ( 10.81189881249999551, -6.242252689847874514, -20.96875000204836681 ) ) ;
#42554 = CARTESIAN_POINT ( 'NONE',  ( 5.405949406249992428, -9.363379034771808662, -135.0937500020483810 ) ) ;
#42555 = CARTESIAN_POINT ( 'NONE',  ( -9.999999999999998224, 1.224646799147353059E-15, -88.62500000409677625 ) ) ;
#42556 = CARTESIAN_POINT ( 'NONE',  ( 5.000000000000000000, 8.660254037844385522, -120.2500000000000000 ) ) ;
#42557 = CARTESIAN_POINT ( 'NONE',  ( 9.999999999999996447, -5.773502691896262640, -159.6250000000000284 ) ) ;
#42558 = CARTESIAN_POINT ( 'NONE',  ( 10.81189881249999729, 0.000000000000000000, -1.531250002048373249 ) ) ;
#42559 = CARTESIAN_POINT ( 'NONE',  ( -10.81189881249999907, -6.242252689847864744, -69.46875000204838102 ) ) ;
#42560 = CARTESIAN_POINT ( 'NONE',  ( -2.293366432827344421E-15, -12.48450537969573659, -52.90625000204837391 ) ) ;
#42561 = CARTESIAN_POINT ( 'NONE',  ( 10.81189881249999729, 0.000000000000000000, -50.84375000204835260 ) ) ;
#42562 = CARTESIAN_POINT ( 'NONE',  ( -4.999999999999996447, 8.660254037844387298, -56.99999999999996447 ) ) ;
#42563 = CARTESIAN_POINT ( 'NONE',  ( 5.405949406249999534, 9.363379034771803333, -164.5937500020484094 ) ) ;
#42564 = EDGE_CURVE ( 'NONE', #21267, #23881, #6855, .T. ) ;
#42565 = CARTESIAN_POINT ( 'NONE',  ( 9.999999999999996447, -5.773502691896262640, -137.1250000000000000 ) ) ;
#42566 = CARTESIAN_POINT ( 'NONE',  ( 10.81189881249999729, 0.000000000000000000, -136.5312500020484094 ) ) ;
#42567 = CARTESIAN_POINT ( 'NONE',  ( -2.121150477449813534E-15, -11.54700538379251284, -150.8750000000000000 ) ) ;
#42568 = CARTESIAN_POINT ( 'NONE',  ( 10.00000000000000000, 5.773502691896255534, -110.2500000040967905 ) ) ;
#42569 = CARTESIAN_POINT ( 'NONE',  ( 4.999999999999992006, -8.660254037844389075, -92.24999999999998579 ) ) ;
#42570 = ADVANCED_FACE ( 'NONE', ( #19772 ), #164, .T. ) ;
#42571 = ORIENTED_EDGE ( 'NONE', *, *, #35671, .T. ) ;
#42572 = CARTESIAN_POINT ( 'NONE',  ( 10.81189881249999729, 6.242252689847867408, -115.4062500020484094 ) ) ;
#42573 = CARTESIAN_POINT ( 'NONE',  ( 10.00000000000000000, 5.773502691896255534, -131.2500000040967905 ) ) ;
#42574 = CARTESIAN_POINT ( 'NONE',  ( 9.999999999999998224, 0.000000000000000000, -21.87500000409675494 ) ) ;
#42575 = EDGE_CURVE ( 'NONE', #10245, #13289, #20408, .T. ) ;
#42576 = CARTESIAN_POINT ( 'NONE',  ( -5.405949406249996869, 9.363379034771805109, -173.5312500020484094 ) ) ;
#42577 = CARTESIAN_POINT ( 'NONE',  ( -9.999999999999998224, 5.773502691896259087, -42.25000000409674783 ) ) ;
#42578 = CARTESIAN_POINT ( 'NONE',  ( 0.000000000000000000, 0.000000000000000000, -200.0000000000000000 ) ) ;
#42579 = CARTESIAN_POINT ( 'NONE',  ( 5.405949406249992428, -9.363379034771808662, -60.28125000204836681 ) ) ;
#42580 = CARTESIAN_POINT ( 'NONE',  ( 7.070501591499376803E-16, 11.54700538379251284, -156.1250000000000000 ) ) ;
#42581 = CARTESIAN_POINT ( 'NONE',  ( -5.405949406249996869, 9.363379034771805109, -164.5312500020484094 ) ) ;
#42582 = CARTESIAN_POINT ( 'NONE',  ( 10.81189881249999729, 0.000000000000000000, -143.8437500020483810 ) ) ;
#42583 = VECTOR ( 'NONE', #13299, 1000.000000000000000 ) ;
#42584 = DIRECTION ( 'NONE',  ( 1.000000000000000000, 0.000000000000000000, 0.000000000000000000 ) ) ;
#42585 = CARTESIAN_POINT ( 'NONE',  ( -4.999999999999996447, 8.660254037844387298, -150.0000000000000000 ) ) ;
#42586 = ORIENTED_EDGE ( 'NONE', *, *, #34175, .T. ) ;
#42587 = CARTESIAN_POINT ( 'NONE',  ( 5.000000000000000000, 8.660254037844385522, -131.1250000040967620 ) ) ;
#42588 = EDGE_CURVE ( 'NONE', #38971, #26946, #37483, .T. ) ;
#42590 = VERTEX_POINT ( 'NONE', #36398 ) ;
#42589 = CARTESIAN_POINT ( 'NONE',  ( -5.405949406250003975, -9.363379034771801557, -69.53125000204838102 ) ) ;
#42591 = APPROVAL_STATUS ( 'not_yet_approved' ) ;
#42593 = ORIENTED_EDGE ( 'NONE', *, *, #40781, .F. ) ;
#42592 = CARTESIAN_POINT ( 'NONE',  ( -2.293366432827344421E-15, -12.48450537969573659, -117.2187500020483952 ) ) ;
#42594 =( BOUNDED_CURVE ( )  B_SPLINE_CURVE ( 2, ( #38664, #5224, #18380, #18809, #12318, #31995, #28543 ),
 .UNSPECIFIED., .F., .F. ) 
 B_SPLINE_CURVE_WITH_KNOTS ( ( 3, 2, 2, 3 ),
 ( 0.2686567164179105571, 0.2699004975124379424, 0.2711442786069652722, 0.2723880597014926574 ),
 .UNSPECIFIED. ) 
 CURVE ( )  GEOMETRIC_REPRESENTATION_ITEM ( )  RATIONAL_B_SPLINE_CURVE ( ( 0.9999999999999880096, 0.8660254037844506980, 1.000000000000000000, 0.8660254037844387076, 1.000000000000000000, 0.8660254037844267172, 1.000000000000011990 ) ) 
 REPRESENTATION_ITEM ( '' )  );
#42595 = ORIENTED_EDGE ( 'NONE', *, *, #41763, .F. ) ;
#42596 = CARTESIAN_POINT ( 'NONE',  ( -10.81189881249999729, 6.242252689847871849, -20.21875000204836326 ) ) ;
#42597 = CARTESIAN_POINT ( 'NONE',  ( 10.81189881249999729, 0.000000000000000000, -0.03125000204837191653 ) ) ;
#42598 = CARTESIAN_POINT ( 'NONE',  ( -5.405949406250003975, -9.363379034771801557, -48.34375000204838102 ) ) ;
#42599 = LINE ( 'NONE', #3340, #24690 ) ;
#42600 = CARTESIAN_POINT ( 'NONE',  ( -9.999999999999998224, 5.773502691896259087, -28.37499999999998224 ) ) ;
#42601 = CARTESIAN_POINT ( 'NONE',  ( -10.81189881249999729, -6.242252689847864744, -184.9687500020484094 ) ) ;
#42602 = CARTESIAN_POINT ( 'NONE',  ( -2.293366432827344421E-15, -12.48450537969573659, -171.2187500020484094 ) ) ;
#42603 = CARTESIAN_POINT ( 'NONE',  ( -10.81189881249999907, -6.242252689847864744, -150.4687500020484094 ) ) ;
#42604 = CARTESIAN_POINT ( 'NONE',  ( -2.293366432827344421E-15, -12.48450537969573659, -172.7187500020483810 ) ) ;
#42605 = CARTESIAN_POINT ( 'NONE',  ( -9.999999999999998224, 1.224646799147353059E-15, -40.62500000409677625 ) ) ;
#42606 = CARTESIAN_POINT ( 'NONE',  ( 4.999999999999992006, -8.660254037844389075, -185.2500000000000000 ) ) ;
#42607 = CARTESIAN_POINT ( 'NONE',  ( 7.644554776091147741E-16, 12.48450537969573659, -96.96875000204838102 ) ) ;
#42608 = DIRECTION ( 'NONE',  ( 1.000000000000000000, 0.000000000000000000, 0.000000000000000000 ) ) ;
#42609 = CARTESIAN_POINT ( 'NONE',  ( -10.81189881249999729, 1.324075727343319199E-15, -74.28125000204838102 ) ) ;
#42610 = CARTESIAN_POINT ( 'NONE',  ( 9.999999999999998224, 0.000000000000000000, -89.37500000409677625 ) ) ;
#42611 = CARTESIAN_POINT ( 'NONE',  ( -5.405949406249996869, 9.363379034771805109, -182.3437500020483810 ) ) ;
#42612 = CARTESIAN_POINT ( 'NONE',  ( -5.405949406250003975, -9.363379034771801557, -162.5312500020484094 ) ) ;
#42613 = CARTESIAN_POINT ( 'NONE',  ( -5.405949406249996869, 9.363379034771805109, -62.53125000204837391 ) ) ;
#42614 = CARTESIAN_POINT ( 'NONE',  ( -9.999999999999998224, 1.224646799147353059E-15, -139.6250000040967905 ) ) ;
#42615 = CARTESIAN_POINT ( 'NONE',  ( -10.00000000000000000, -5.773502691896251982, -115.1249999999999858 ) ) ;
#42616 = EDGE_LOOP ( 'NONE', ( #36285, #5300 ) ) ;
#42617 = CARTESIAN_POINT ( 'NONE',  ( -10.81189881249999729, 1.324075727343319199E-15, -138.7812500020483810 ) ) ;
#42618 = CARTESIAN_POINT ( 'NONE',  ( -5.405949406250003975, -9.363379034771801557, -158.0312500020484094 ) ) ;
#42619 = CARTESIAN_POINT ( 'NONE',  ( -5.405949406249996869, 9.363379034771805109, -199.0312500020484094 ) ) ;
#42620 = CARTESIAN_POINT ( 'NONE',  ( 5.405949406249992428, -9.363379034771808662, -87.09375000204836681 ) ) ;
#42621 = EDGE_LOOP ( 'NONE', ( #38100, #9380, #29985, #5506 ) ) ;
#42622 = CARTESIAN_POINT ( 'NONE',  ( -9.999999999999998224, 1.224646799147353059E-15, -53.74999999999996447 ) ) ;
#42623 = CARTESIAN_POINT ( 'NONE',  ( 7.644554776091147741E-16, 12.48450537969573659, -188.4687500020484094 ) ) ;
#42624 = CARTESIAN_POINT ( 'NONE',  ( 4.999999999999992006, -8.660254037844389075, -67.12500000409676204 ) ) ;
#42625 = CYLINDRICAL_SURFACE ( 'NONE', #7949, 9.999999999999998224 ) ;
#42626 = CARTESIAN_POINT ( 'NONE',  ( -5.000000000000003553, -8.660254037844383745, -124.0000000000000000 ) ) ;
#42627 = CARTESIAN_POINT ( 'NONE',  ( -5.405949406249996869, 9.363379034771805109, -82.03125000204839523 ) ) ;
#42628 = CARTESIAN_POINT ( 'NONE',  ( -5.405949406249996869, 9.363379034771805109, -68.53125000204838102 ) ) ;
#42629 = CARTESIAN_POINT ( 'NONE',  ( -9.999999999999998224, 5.773502691896259087, -57.25000000409677625 ) ) ;
#42630 = CARTESIAN_POINT ( 'NONE',  ( -10.81189881249999729, 1.324075727343319199E-15, -20.09375000204835615 ) ) ;
#42631 = CARTESIAN_POINT ( 'NONE',  ( 9.999999999998969713, 5.773502691896851502, -38.25000000409674072 ) ) ;
#42632 = CARTESIAN_POINT ( 'NONE',  ( 5.405949406249992428, -9.363379034771808662, -187.7812500020484094 ) ) ;
#42633 = EDGE_CURVE ( 'NONE', #12497, #24317, #16787, .T. ) ;
#42634 = CARTESIAN_POINT ( 'NONE',  ( 5.405949406249999534, 9.363379034771803333, -14.78125000204835793 ) ) ;
#42635 = CARTESIAN_POINT ( 'NONE',  ( 7.295574285832478800, -8.272403601877444501, -0.05005682399628019752 ) ) ;
#42636 = CARTESIAN_POINT ( 'NONE',  ( -11.54700538379250396, -20.00000000000000355, 0.000000000000000000 ) ) ;
#42637 = CARTESIAN_POINT ( 'NONE',  ( -9.886419945013566135, -1.735418534722659389, -0.000000000000000000 ) ) ;
#42638 = CARTESIAN_POINT ( 'NONE',  ( 9.999999999999998224, 0.000000000000000000, -122.3750000040967905 ) ) ;
#42639 =( BOUNDED_CURVE ( )  B_SPLINE_CURVE ( 2, ( #5731, #21907, #28825, #35087, #5512, #18663, #28613 ),
 .UNSPECIFIED., .F., .F. ) 
 B_SPLINE_CURVE_WITH_KNOTS ( ( 3, 2, 2, 3 ),
 ( 0.1007462686567163757, 0.1019900497512437887, 0.1032338308457712017, 0.1044776119402986148 ),
 .UNSPECIFIED. ) 
 CURVE ( )  GEOMETRIC_REPRESENTATION_ITEM ( )  RATIONAL_B_SPLINE_CURVE ( ( 1.000000000000004441, 0.8660254037844342667, 1.000000000000000000, 0.8660254037844387076, 1.000000000000000000, 0.8660254037844267172, 1.000000000000011990 ) ) 
 REPRESENTATION_ITEM ( '' )  );
#42640 = CARTESIAN_POINT ( 'NONE',  ( -10.00000000000000000, -5.773502691896251982, -170.6250000000000284 ) ) ;
#42641 = CARTESIAN_POINT ( 'NONE',  ( 7.070501591499376803E-16, 11.54700538379251284, -1.624999999999975575 ) ) ;
#42643 = ORIENTED_EDGE ( 'NONE', *, *, #40051, .F. ) ;
#42642 = CARTESIAN_POINT ( 'NONE',  ( -10.81189881249999907, -6.242252689847864744, -92.15625000204839523 ) ) ;
#42644 = DIRECTION ( 'NONE',  ( -0.000000000000000000, -0.000000000000000000, 1.000000000000000000 ) ) ;
#42646 = ORIENTED_EDGE ( 'NONE', *, *, #4837, .F. ) ;
#42645 = FACE_OUTER_BOUND ( 'NONE', #17314, .T. ) ;
#42647 = ORIENTED_EDGE ( 'NONE', *, *, #41568, .T. ) ;
#42648 = EDGE_CURVE ( 'NONE', #26059, #5330, #21212, .T. ) ;
#42649 = CARTESIAN_POINT ( 'NONE',  ( 5.405949406249992428, -9.363379034771808662, -31.59375000204836681 ) ) ;
#42650 = CARTESIAN_POINT ( 'NONE',  ( -2.293366432827344421E-15, -12.48450537969573659, -21.40625000204837036 ) ) ;
#42651 = APPROVAL_ROLE ( '' ) ;
#42652 = AXIS2_PLACEMENT_3D ( 'NONE', #12208, #25401, #34481 ) ;
#42653 = CARTESIAN_POINT ( 'NONE',  ( 10.81189881249999729, 0.000000000000000000, -67.34375000204836681 ) ) ;
#42654 = CARTESIAN_POINT ( 'NONE',  ( 9.999999999999998224, 0.000000000000000000, -200.0000000000000000 ) ) ;
#42655 = CARTESIAN_POINT ( 'NONE',  ( 5.405949406249999534, 9.363379034771803333, -191.5937500020484094 ) ) ;
#42656 = CARTESIAN_POINT ( 'NONE',  ( 9.999999999999479527, 5.773502691896553074, -72.75000000409673362 ) ) ;
#42657 = AXIS2_PLACEMENT_3D ( 'NONE', #5647, #31984, #31557 ) ;
#42658 = CARTESIAN_POINT ( 'NONE',  ( -9.999999999999998224, 1.224646799147353059E-15, -144.1250000040967905 ) ) ;
#42659 = CARTESIAN_POINT ( 'NONE',  ( 5.405949406249999534, 9.363379034771803333, -160.2812500020484094 ) ) ;
#42660 = CARTESIAN_POINT ( 'NONE',  ( -2.121150477449813534E-15, -11.54700538379251284, -7.250000004096746054 ) ) ;
#42661 = CARTESIAN_POINT ( 'NONE',  ( -5.000000000000003553, -8.660254037844383745, -103.3750000040967763 ) ) ;
#42662 = CARTESIAN_POINT ( 'NONE',  ( -5.405949406250003975, -9.363379034771801557, -118.8437500020483810 ) ) ;
#42663 = CARTESIAN_POINT ( 'NONE',  ( 10.81189881249999907, 6.242252689847868297, -98.90625000204839523 ) ) ;
#42664 = CARTESIAN_POINT ( 'NONE',  ( 7.644554776091147741E-16, 12.48450537969573659, -111.9687500020483668 ) ) ;
#42665 = CARTESIAN_POINT ( 'NONE',  ( 10.81189881249999551, -6.242252689847874514, -74.96875000204838102 ) ) ;
#42666 = CARTESIAN_POINT ( 'NONE',  ( 10.81189881249999551, -6.242252689847874514, -81.15625000204839523 ) ) ;
#42667 = CARTESIAN_POINT ( 'NONE',  ( 9.999999999999996447, -5.773502691896262640, -161.5000000040968189 ) ) ;
#42668 = CYLINDRICAL_SURFACE ( 'NONE', #1341, 9.999999999999998224 ) ;
#42669 = CARTESIAN_POINT ( 'NONE',  ( 7.644554776091147741E-16, 12.48450537969573659, -167.6562500020484094 ) ) ;
#42670 = CARTESIAN_POINT ( 'NONE',  ( -10.81189881249999729, 1.324075727343319199E-15, -183.7812500020484094 ) ) ;
#42671 = CARTESIAN_POINT ( 'NONE',  ( -9.999999999999998224, 5.773502691896259087, -153.2500000040967620 ) ) ;
#42672 = CARTESIAN_POINT ( 'NONE',  ( -5.000000000000003553, -8.660254037844383745, -157.0000000000000000 ) ) ;
#42673 = CARTESIAN_POINT ( 'NONE',  ( 10.81189881249999729, 0.000000000000000000, -8.843750002048345493 ) ) ;
#42674 = CARTESIAN_POINT ( 'NONE',  ( -9.999999999999998224, 1.224646799147353059E-15, -127.2499999999999716 ) ) ;
#42675 = CARTESIAN_POINT ( 'NONE',  ( 10.81189881249999551, -6.242252689847874514, -115.4687500020483810 ) ) ;
#42676 = CARTESIAN_POINT ( 'NONE',  ( 9.999999999999998224, 0.000000000000000000, -84.49999999999997158 ) ) ;
#42677 = CARTESIAN_POINT ( 'NONE',  ( -2.293366432827344421E-15, -12.48450537969573659, -10.90625000204836681 ) ) ;
#42678 = CARTESIAN_POINT ( 'NONE',  ( -9.999999999999998224, 5.773502691896259087, -99.25000000409677625 ) ) ;
#42679 = DIRECTION ( 'NONE',  ( -1.000000000000000000, 0.000000000000000000, 0.000000000000000000 ) ) ;
#42680 = CARTESIAN_POINT ( 'NONE',  ( 10.81189881249999907, 6.242252689847868297, -110.9062500020483952 ) ) ;
#42681 = CARTESIAN_POINT ( 'NONE',  ( -10.81189881249999729, 1.324075727343319199E-15, -90.78125000204838102 ) ) ;
#42682 = EDGE_LOOP ( 'NONE', ( #6804, #22029, #13016, #6364 ) ) ;
#42683 = EDGE_CURVE ( 'NONE', #21484, #34431, #14771, .T. ) ;
#42684 = CARTESIAN_POINT ( 'NONE',  ( -2.121150477449813534E-15, -11.54700538379251284, -80.75000000409677625 ) ) ;
#42685 = CARTESIAN_POINT ( 'NONE',  ( 4.999999999999992006, -8.660254037844389075, -140.6250000040967905 ) ) ;
#42686 = CARTESIAN_POINT ( 'NONE',  ( -10.81189881249999907, -6.242252689847864744, -39.46875000204835970 ) ) ;
#42687 = ORIENTED_EDGE ( 'NONE', *, *, #14286, .F. ) ;
#42688 = CARTESIAN_POINT ( 'NONE',  ( -9.999999999999998224, 1.224646799147353059E-15, -13.24999999999995559 ) ) ;
#42689 = CIRCLE ( 'NONE', #26857, 60.00000000000000711 ) ;
#42690 = ADVANCED_FACE ( 'NONE', ( #5088 ), #37235, .T. ) ;
#42691 = NEXT_ASSEMBLY_USAGE_OCCURRENCE ( 'NAUO1', ' ', ' ', #19626, #20655, $ ) ;
#42692 = NEXT_ASSEMBLY_USAGE_OCCURRENCE ( 'NAUO2', ' ', ' ', #19626, #24384, $ ) ;
#42693 = NEXT_ASSEMBLY_USAGE_OCCURRENCE ( 'NAUO3', ' ', ' ', #19626, #14057, $ ) ;
#42694 = NEXT_ASSEMBLY_USAGE_OCCURRENCE ( 'NAUO4', ' ', ' ', #19626, #3281, $ ) ;
#42695 = NEXT_ASSEMBLY_USAGE_OCCURRENCE ( 'NAUO5', ' ', ' ', #19626, #8303, $ ) ;
#42696 = NEXT_ASSEMBLY_USAGE_OCCURRENCE ( 'NAUO6', ' ', ' ', #19626, #15921, $ ) ;
#42697 = COLOUR_RGB('Deep Blue', 0.09019608, 0.27058824, 0.51372549);
#42698 = FILL_AREA_STYLE_COLOUR('',#42697);
#42699 = FILL_AREA_STYLE('',(#42698));
#42700 = SURFACE_STYLE_FILL_AREA(#42699);
#42701 = SURFACE_SIDE_STYLE('',(#42700));
#42702 = SURFACE_STYLE_USAGE(.BOTH.,#42701);
#42703 = PRESENTATION_STYLE_ASSIGNMENT((#42702));
#42704 = COLOUR_RGB('Light Blue', 0.66274510, 0.83137255, 0.94901961);
#42705 = FILL_AREA_STYLE_COLOUR('',#42704);
#42706 = FILL_AREA_STYLE('',(#42705));
#42707 = SURFACE_STYLE_FILL_AREA(#42706);
#42708 = SURFACE_SIDE_STYLE('',(#42707));
#42709 = SURFACE_STYLE_USAGE(.BOTH.,#42708);
#42710 = PRESENTATION_STYLE_ASSIGNMENT((#42709));
#42711 = COLOUR_RGB('Sky Blue', 0.31764706, 0.68627451, 0.89019608);
#42712 = FILL_AREA_STYLE_COLOUR('',#42711);
#42713 = FILL_AREA_STYLE('',(#42712));
#42714 = SURFACE_STYLE_FILL_AREA(#42713);
#42715 = SURFACE_SIDE_STYLE('',(#42714));
#42716 = SURFACE_STYLE_USAGE(.BOTH.,#42715);
#42717 = PRESENTATION_STYLE_ASSIGNMENT((#42716));
#42718 = COLOUR_RGB('Slate Gray', 0.40784314, 0.44705882, 0.49803922);
#42719 = FILL_AREA_STYLE_COLOUR('',#42718);
#42720 = FILL_AREA_STYLE('',(#42719));
#42721 = SURFACE_STYLE_FILL_AREA(#42720);
#42722 = SURFACE_SIDE_STYLE('',(#42721));
#42723 = SURFACE_STYLE_USAGE(.BOTH.,#42722);
#42724 = PRESENTATION_STYLE_ASSIGNMENT((#42723));
#42725 = COLOUR_RGB('Light Gray', 0.72549020, 0.75294118, 0.79215686);
#42726 = FILL_AREA_STYLE_COLOUR('',#42725);
#42727 = FILL_AREA_STYLE('',(#42726));
#42728 = SURFACE_STYLE_FILL_AREA(#42727);
#42729 = SURFACE_SIDE_STYLE('',(#42728));
#42730 = SURFACE_STYLE_USAGE(.BOTH.,#42729);
#42731 = PRESENTATION_STYLE_ASSIGNMENT((#42730));
#42732 = COLOUR_RGB('Black', 0.08235294, 0.09019608, 0.10196078);
#42733 = FILL_AREA_STYLE_COLOUR('',#42732);
#42734 = FILL_AREA_STYLE('',(#42733));
#42735 = SURFACE_STYLE_FILL_AREA(#42734);
#42736 = SURFACE_SIDE_STYLE('',(#42735));
#42737 = SURFACE_STYLE_USAGE(.BOTH.,#42736);
#42738 = PRESENTATION_STYLE_ASSIGNMENT((#42737));
#42739 = STYLED_ITEM('',(#42731),#29947);
#42740 = MECHANICAL_DESIGN_GEOMETRIC_PRESENTATION_REPRESENTATION('',(#42739),#11785);
#42741 = STYLED_ITEM('',(#42724),#29300);
#42742 = MECHANICAL_DESIGN_GEOMETRIC_PRESENTATION_REPRESENTATION('',(#42741),#28294);
#42743 = STYLED_ITEM('',(#42703),#1204);
#42744 = MECHANICAL_DESIGN_GEOMETRIC_PRESENTATION_REPRESENTATION('',(#42743),#28334);
#42745 = STYLED_ITEM('',(#42717),#28380);
#42746 = MECHANICAL_DESIGN_GEOMETRIC_PRESENTATION_REPRESENTATION('',(#42745),#29026);
#42747 = STYLED_ITEM('',(#42710),#1487);
#42748 = MECHANICAL_DESIGN_GEOMETRIC_PRESENTATION_REPRESENTATION('',(#42747),#13832);
#42749 = STYLED_ITEM('',(#42738),#30024);
#42750 = MECHANICAL_DESIGN_GEOMETRIC_PRESENTATION_REPRESENTATION('',(#42749),#15874);
ENDSEC;
END-ISO-10303-21;
